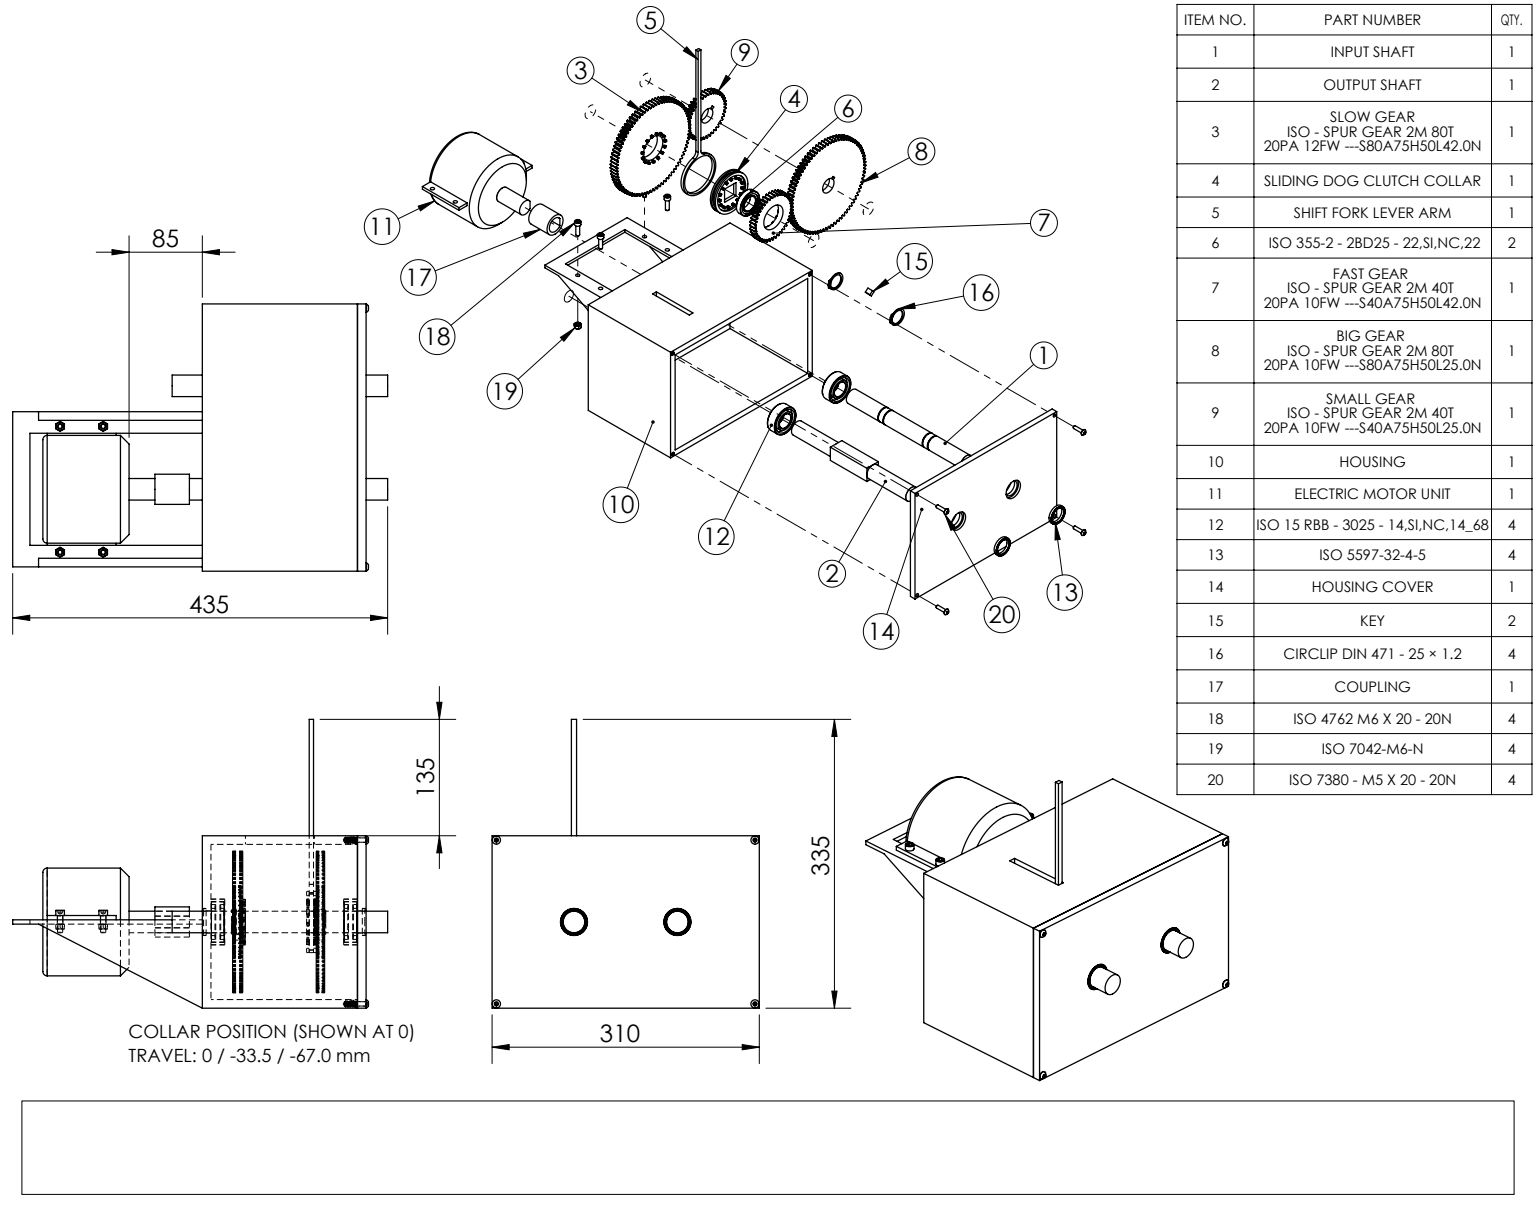
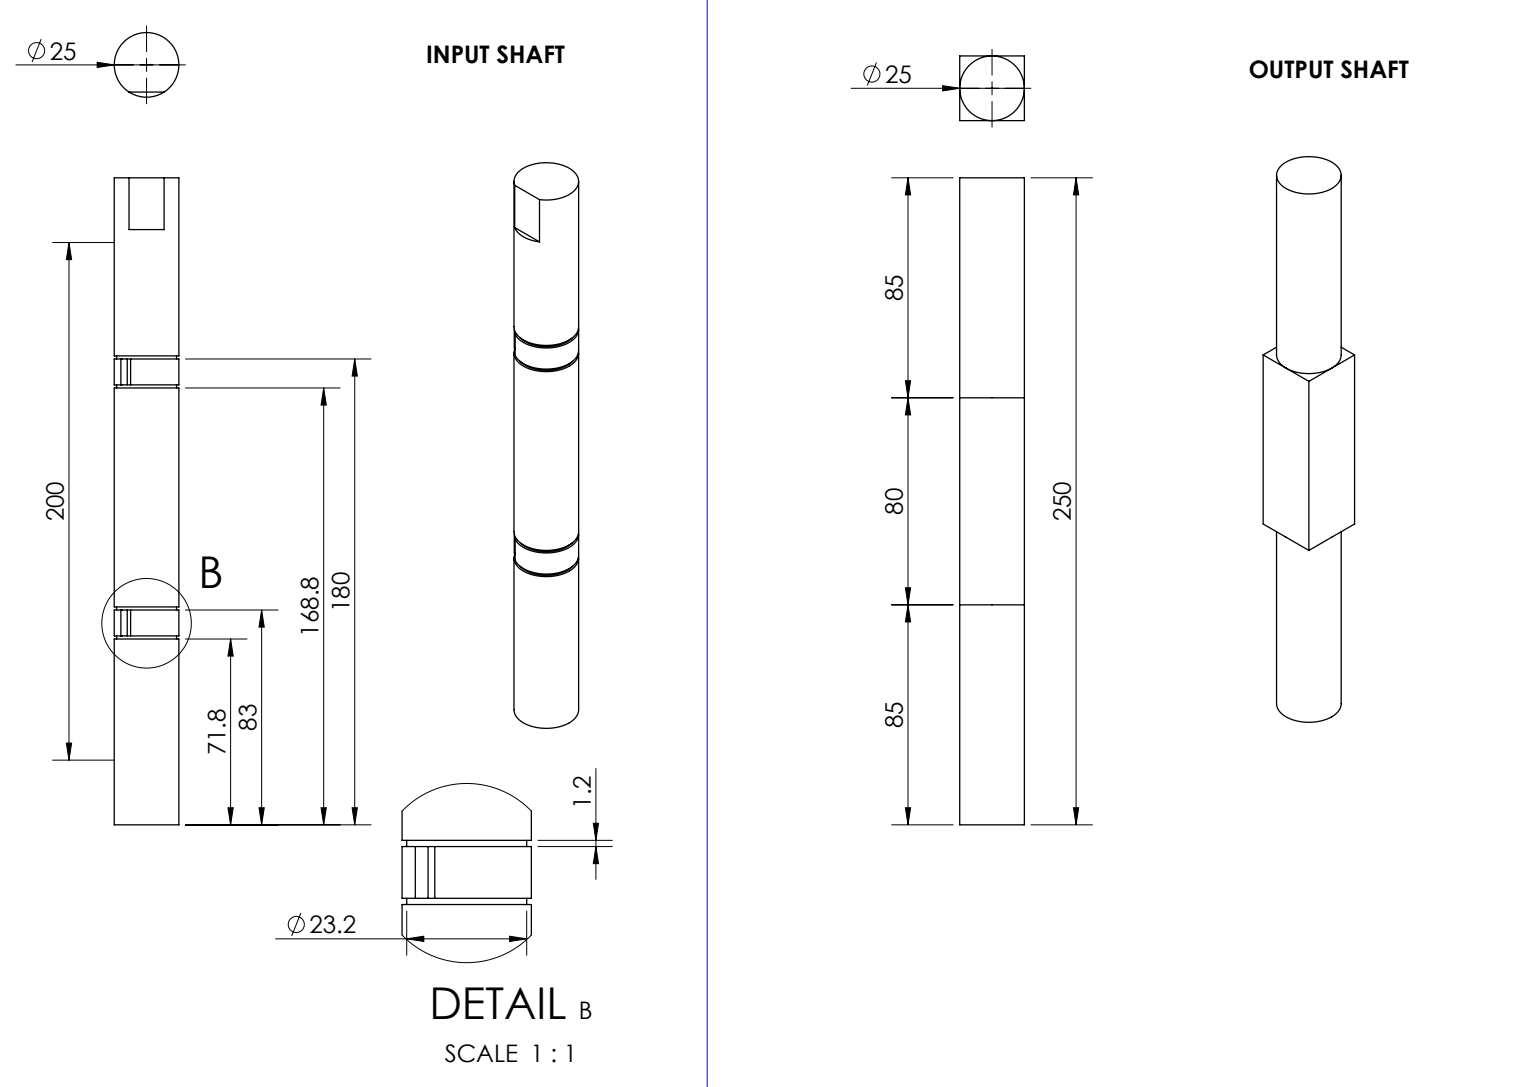
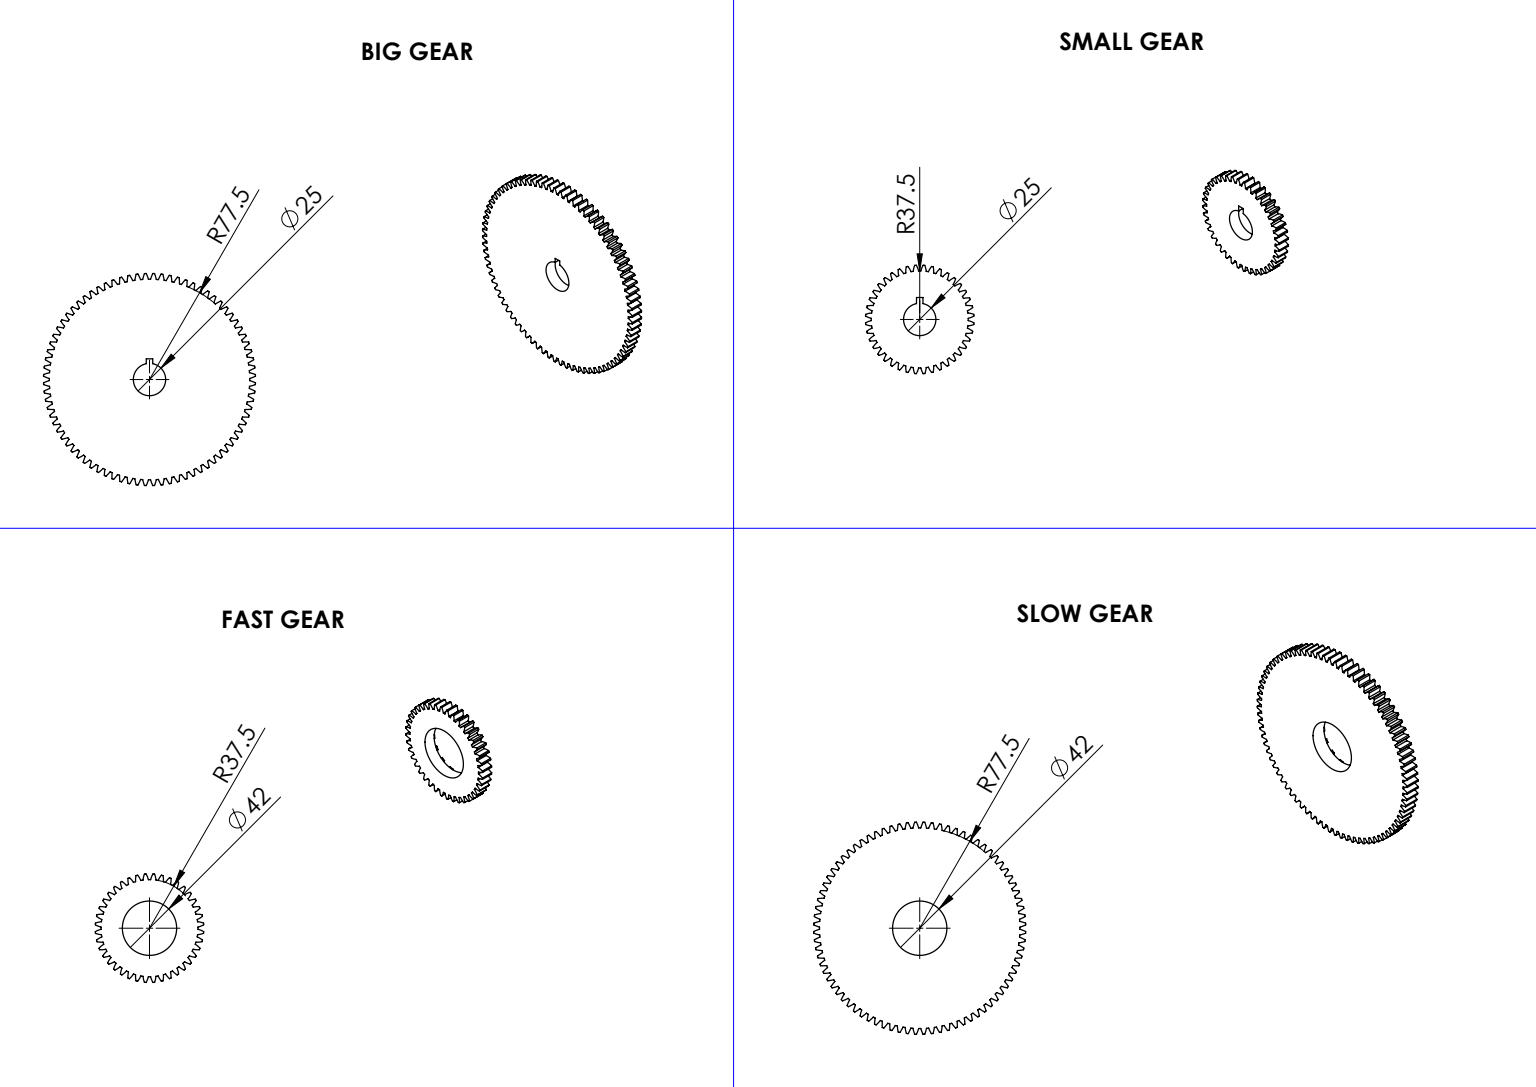
ISO-10303-21;
HEADER;
FILE_DESCRIPTION (('STEP AP214'),
    '1' );
FILE_NAME ('BR-542',
    '2026-10-08T09:53:37',
    ( '' ),
    ( '' ),
    'SwSTEP 2.0',
    'SolidWorks 2026',
    '' );
FILE_SCHEMA (( 'AUTOMOTIVE_DESIGN' ));
ENDSEC;

DATA;
#1 = ORIENTED_EDGE ( 'NONE', *, *, #51679, .F. ) ;
#2 = CARTESIAN_POINT ( 'NONE',  ( -96.15314808468745866, -211.9973110713294489, 75.77864583420047495 ) ) ;
#3 = EDGE_LOOP ( 'NONE', ( #16003, #47116, #6301, #7133 ) ) ;
#4 = DIRECTION ( 'NONE',  ( -1.000000000000000000, -0.000000000000000000, -0.000000000000000000 ) ) ;
#5 = CARTESIAN_POINT ( 'NONE',  ( 10.00000000000000000, 21.53537804866126137, -30.80686688396986028 ) ) ;
#6 = DIRECTION ( 'NONE',  ( -0.000000000000000000, -0.000000000000000000, 1.000000000000000000 ) ) ;
#7 = DIRECTION ( 'NONE',  ( 0.000000000000000000, 0.7071067811865487940, -0.7071067811865462405 ) ) ;
#8 = DIRECTION ( 'NONE',  ( -1.000000000000000000, 0.000000000000000000, 0.000000000000000000 ) ) ;
#9 = CARTESIAN_POINT ( 'NONE',  ( -92.34999999999999432, -209.9999999999999716, 90.00000000000000000 ) ) ;
#10 = CARTESIAN_POINT ( 'NONE',  ( 96.15314808468748708, 91.99731107132950569, 84.98614583420047097 ) ) ;
#11 = CYLINDRICAL_SURFACE ( 'NONE', #11189, 82.00000000000000000 ) ;
#12 = CARTESIAN_POINT ( 'NONE',  ( 20.85212586905262100, -130.9402397935870965, 2.500000000000000000 ) ) ;
#13 = DIRECTION ( 'NONE',  ( 0.000000000000000000, 0.8660254037844421493, 0.4999999999999938938 ) ) ;
#14 = CARTESIAN_POINT ( 'NONE',  ( -5.000000000000000000, 2.488344183252603870, -1.689918788536291405 ) ) ;
#15 = DIRECTION ( 'NONE',  ( 9.814797785686868941E-17, -1.000000000000000000, 0.000000000000000000 ) ) ;
#16 = CARTESIAN_POINT ( 'NONE',  ( 2.255011273957053586, 4.471571325851512846, -0.5083873451168745561 ) ) ;
#17 = DIRECTION ( 'NONE',  ( 0.000000000000000000, 0.8910065241883656784, 0.4539904997395510788 ) ) ;
#18 = CARTESIAN_POINT ( 'NONE',  ( 99.99999999999998579, 90.00000000000000000, -90.00000000000000000 ) ) ;
#19 = AXIS2_PLACEMENT_3D ( 'NONE', #55225, #15366, #9737 ) ;
#20 = CYLINDRICAL_SURFACE ( 'NONE', #64875, 31.99999999999998579 ) ;
#21 = AXIS2_PLACEMENT_3D ( 'NONE', #73803, #50119, #22316 ) ;
#22 = FACE_OUTER_BOUND ( 'NONE', #9056, .T. ) ;
#23 = CARTESIAN_POINT ( 'NONE',  ( -92.69370383062505425, 91.33154071421968467, 89.37822916753378877 ) ) ;
#24 = CARTESIAN_POINT ( 'NONE',  ( 0.000000000000000000, -37.22597642581153821, 10.79786254984320415 ) ) ;
#25 = AXIS2_PLACEMENT_3D ( 'NONE', #2057, #18922, #40477 ) ;
#26 = ADVANCED_FACE ( 'NONE', ( #50299 ), #9718, .T. ) ;
#27 = CARTESIAN_POINT ( 'NONE',  ( -93.07557990970633455, 88.17815826261617929, 75.00000000000001421 ) ) ;
#28 = ORIENTED_EDGE ( 'NONE', *, *, #17747, .T. ) ;
#29 = CARTESIAN_POINT ( 'NONE',  ( -92.35000000000005116, 91.52997821335253548, 77.03541666666666288 ) ) ;
#30 = DIRECTION ( 'NONE',  ( 0.000000000000000000, 0.3090169943749410675, 0.9510565162951556406 ) ) ;
#31 = CARTESIAN_POINT ( 'NONE',  ( 10.00000000000000000, 69.42325613327439271, 34.44570377933623462 ) ) ;
#32 = DIRECTION ( 'NONE',  ( 0.4565542962317865050, 0.000000000000000000, 0.8896955516311735312 ) ) ;
#33 = CIRCLE ( 'NONE', #8406, 42.00000000000000000 ) ;
#34 = DIRECTION ( 'NONE',  ( -8.783410004945701396E-16, -1.065814103640131188E-14, -1.000000000000000000 ) ) ;
#35 = VECTOR ( 'NONE', #29817, 1000.000000000000000 ) ;
#36 = CONICAL_SURFACE ( 'NONE', #30016, 3.000000000000000000, 0.9599310885968762586 ) ;
#37 = CARTESIAN_POINT ( 'NONE',  ( 97.30629616937498838, -208.6684592857803011, 84.45697916753383083 ) ) ;
#38 = ORIENTED_EDGE ( 'NONE', *, *, #69676, .T. ) ;
#39 = EDGE_CURVE ( 'NONE', #49169, #37092, #23562, .T. ) ;
#40 = VECTOR ( 'NONE', #42271, 1000.000000000000000 ) ;
#41 = ORIENTED_EDGE ( 'NONE', *, *, #37857, .F. ) ;
#42 = AXIS2_PLACEMENT_3D ( 'NONE', #21315, #43177, #8581 ) ;
#43 = ADVANCED_FACE ( 'NONE', ( #33760 ), #72489, .F. ) ;
#44 = DIRECTION ( 'NONE',  ( 0.000000000000000000, 0.000000000000000000, -1.000000000000000000 ) ) ;
#45 = VERTEX_POINT ( 'NONE', #4470 ) ;
#46 = DIRECTION ( 'NONE',  ( -1.000000000000000000, 0.000000000000000000, 0.000000000000000000 ) ) ;
#47 = CARTESIAN_POINT ( 'NONE',  ( 96.15314808468750130, -211.9973110713294489, 77.78947916753381264 ) ) ;
#48 = ORIENTED_EDGE ( 'NONE', *, *, #42717, .F. ) ;
#49 = CARTESIAN_POINT ( 'NONE',  ( 95.00000000000000000, -212.6630814284392557, 84.24531250086715772 ) ) ;
#50 = EDGE_CURVE ( 'NONE', #4438, #10838, #58395, .T. ) ;
#51 = EDGE_CURVE ( 'NONE', #68933, #53084, #10085, .T. ) ;
#52 = ORIENTED_EDGE ( 'NONE', *, *, #54649, .T. ) ;
#53 = CARTESIAN_POINT ( 'NONE',  ( -92.35000000000005116, -211.5299782133524786, 88.35958333333334735 ) ) ;
#54 = ORIENTED_EDGE ( 'NONE', *, *, #5365, .T. ) ;
#55 = ORIENTED_EDGE ( 'NONE', *, *, #2305, .T. ) ;
#56 = CARTESIAN_POINT ( 'NONE',  ( -97.30629616937501680, 88.66845928578038638, 75.24947916753383481 ) ) ;
#57 = DIRECTION ( 'NONE',  ( -0.9966891607226785466, -0.08130631524009969413, 0.000000000000000000 ) ) ;
#58 = ORIENTED_EDGE ( 'NONE', *, *, #67325, .F. ) ;
#59 = DIRECTION ( 'NONE',  ( -0.3311129884571295534, -0.9435911131814398445, 0.000000000000000000 ) ) ;
#60 = CARTESIAN_POINT ( 'NONE',  ( 97.64999999999997726, -211.5299782133524502, 87.16895833506762870 ) ) ;
#61 = EDGE_LOOP ( 'NONE', ( #56429, #49717, #59358, #37465 ) ) ;
#62 = DIRECTION ( 'NONE',  ( -1.000000000000000000, 0.000000000000000000, 0.000000000000000000 ) ) ;
#63 = EDGE_LOOP ( 'NONE', ( #58419, #58729, #9713, #39288 ) ) ;
#64 = CARTESIAN_POINT ( 'NONE',  ( -26.29030328629083968, -123.6496510949466341, -5.500000000000000000 ) ) ;
#65 = CIRCLE ( 'NONE', #33475, 42.00000000000000000 ) ;
#66 = EDGE_CURVE ( 'NONE', #32419, #45509, #49931, .T. ) ;
#67 = EDGE_LOOP ( 'NONE', ( #2457, #71707, #71945, #64726 ) ) ;
#68 = CIRCLE ( 'NONE', #60030, 16.00000000000000000 ) ;
#69 = ORIENTED_EDGE ( 'NONE', *, *, #12987, .T. ) ;
#70 = VERTEX_POINT ( 'NONE', #39037 ) ;
#71 = FACE_OUTER_BOUND ( 'NONE', #8361, .T. ) ;
#72 = ITEM_DEFINED_TRANSFORMATION ( 'NONE', 'NONE', #20767,  #43395 ) ;
#73 = CARTESIAN_POINT ( 'NONE',  ( -5.000000000000000000, -2.886751345948134428, -2.080000000000000071 ) ) ;
#74 = ORIENTED_EDGE ( 'NONE', *, *, #31039, .F. ) ;
#75 = VERTEX_POINT ( 'NONE', #9336 ) ;
#76 = AXIS2_PLACEMENT_3D ( 'NONE', #48493, #31191, #42490 ) ;
#77 = ORIENTED_EDGE ( 'NONE', *, *, #22870, .F. ) ;
#78 = CARTESIAN_POINT ( 'NONE',  ( 95.00000000000000000, -213.0599564267049857, 76.18874999999999886 ) ) ;
#79 = CARTESIAN_POINT ( 'NONE',  ( -97.64999999960622290, -209.9999706925929672, 76.74344264316562203 ) ) ;
#80 = CARTESIAN_POINT ( 'NONE',  ( -97.65000000000001990, 90.00000000000004263, 86.82500000000000284 ) ) ;
#81 = EDGE_CURVE ( 'NONE', #13281, #10925, #26630, .T. ) ;
#82 = ORIENTED_EDGE ( 'NONE', *, *, #60544, .T. ) ;
#83 = DIRECTION ( 'NONE',  ( -1.000000000000000000, 0.000000000000000000, 0.000000000000000000 ) ) ;
#84 = ORIENTED_EDGE ( 'NONE', *, *, #17370, .T. ) ;
#85 = LINE ( 'NONE', #57553, #61145 ) ;
#86 = CARTESIAN_POINT ( 'NONE',  ( -92.69370383062498320, -209.9999999999999716, 84.88031250086713442 ) ) ;
#87 = ORIENTED_EDGE ( 'NONE', *, *, #45061, .F. ) ;
#88 = EDGE_CURVE ( 'NONE', #20645, #66879, #14982, .T. ) ;
#89 = CARTESIAN_POINT ( 'NONE',  ( -3.000000000000000000, 0.000000000000000000, 0.000000000000000000 ) ) ;
#90 = CARTESIAN_POINT ( 'NONE',  ( 93.89144186338218390, -212.3693961632864955, 74.97612907457772735 ) ) ;
#91 = CARTESIAN_POINT ( 'NONE',  ( -2.499999999999970690, 73.00000000000001421, -201.6999999999999602 ) ) ;
#92 = CARTESIAN_POINT ( 'NONE',  ( -97.30629616937497417, -208.6684592857803295, 76.25489583420049655 ) ) ;
#93 = AXIS2_PLACEMENT_3D ( 'NONE', #19631, #69384, #17880 ) ;
#94 = CARTESIAN_POINT ( 'NONE',  ( 11.99999999999999822, 66.50666863322000211, 39.78640506895628448 ) ) ;
#95 = CARTESIAN_POINT ( 'NONE',  ( 94.99999999999998579, 90.00000000000002842, 90.00000000000000000 ) ) ;
#96 = VECTOR ( 'NONE', #69294, 1000.000000000000000 ) ;
#97 = VECTOR ( 'NONE', #25254, 1000.000000000000114 ) ;
#98 = TOROIDAL_SURFACE ( 'NONE', #51668, 20.69999999999999929, 0.2999999999999981570 ) ;
#99 = CARTESIAN_POINT ( 'NONE',  ( 0.000000000000000000, -0.9646360437375307573, 23.52805723605590060 ) ) ;
#100 = DIRECTION ( 'NONE',  ( 0.000000000000000000, 0.000000000000000000, 1.000000000000000000 ) ) ;
#101 = CARTESIAN_POINT ( 'NONE',  ( -96.15314808468752972, 91.99731107132950569, 78.74197916753381321 ) ) ;
#102 = CARTESIAN_POINT ( 'NONE',  ( 26.00000000000000355, 0.000000000000000000, 0.000000000000000000 ) ) ;
#103 = DIRECTION ( 'NONE',  ( 1.000000000000000000, 0.000000000000000000, 0.000000000000000000 ) ) ;
#104 =( BOUNDED_CURVE ( )  B_SPLINE_CURVE ( 2, ( #36888, #19593, #59840, #8323, #31250, #71460, #19961 ),
 .UNSPECIFIED., .F., .F. ) 
 B_SPLINE_CURVE_WITH_KNOTS ( ( 3, 2, 2, 3 ),
 ( 0.2291666666666663521, 0.2361111111111107719, 0.2430555555555551639, 0.2499999999999995837 ),
 .UNSPECIFIED. ) 
 CURVE ( )  GEOMETRIC_REPRESENTATION_ITEM ( )  RATIONAL_B_SPLINE_CURVE ( ( 1.000000000000005995, 0.8660254037844328234, 1.000000000000000000, 0.8660254037844387076, 1.000000000000000000, 0.8660254037844467012, 0.9999999999999920064 ) ) 
 REPRESENTATION_ITEM ( '' )  );
#105 = VERTEX_POINT ( 'NONE', #27751 ) ;
#106 = DIRECTION ( 'NONE',  ( -1.000000000000000000, 0.000000000000000000, -0.000000000000000000 ) ) ;
#107 = DIRECTION ( 'NONE',  ( 9.814797785686868941E-17, 1.000000000000000000, -0.000000000000000000 ) ) ;
#108 = CARTESIAN_POINT ( 'NONE',  ( 97.64999999999999147, 90.00000015433757028, 79.60187500750917877 ) ) ;
#109 = PLANE ( 'NONE',  #37048 ) ;
#110 = DIRECTION ( 'NONE',  ( 1.000000000000000000, -0.000000000000000000, -0.000000000000000000 ) ) ;
#111 = DIRECTION ( 'NONE',  ( 1.000000000000000000, 0.000000000000000000, 0.000000000000000000 ) ) ;
#112 = CARTESIAN_POINT ( 'NONE',  ( -93.84685191531248449, -208.0026889286704943, 80.06489583420048461 ) ) ;
#113 = LINE ( 'NONE', #11332, #2116 ) ;
#114 = ORIENTED_EDGE ( 'NONE', *, *, #19664, .T. ) ;
#115 = DIRECTION ( 'NONE',  ( 0.000000000000000000, 0.000000000000000000, 1.000000000000000000 ) ) ;
#116 = DIRECTION ( 'NONE',  ( 1.000000000000000000, -0.000000000000000000, -0.000000000000000000 ) ) ;
#117 = DIRECTION ( 'NONE',  ( 1.000000000000000000, -0.000000000000000000, 0.000000000000000000 ) ) ;
#118 = LINE ( 'NONE', #6814, #70143 ) ;
#119 = CIRCLE ( 'NONE', #8452, 82.00000000000000000 ) ;
#120 = CIRCLE ( 'NONE', #42098, 12.49999999999999645 ) ;
#121 = AXIS2_PLACEMENT_3D ( 'NONE', #14908, #31452, #37108 ) ;
#122 = ADVANCED_FACE ( 'NONE', ( #44690 ), #3363, .T. ) ;
#123 = DIRECTION ( 'NONE',  ( 0.000000000000000000, 0.000000000000000000, -1.000000000000000000 ) ) ;
#124 = EDGE_LOOP ( 'NONE', ( #72657, #17646, #60225, #7667 ) ) ;
#126 = EDGE_CURVE ( 'NONE', #13140, #57222, #72120, .T. ) ;
#125 = CARTESIAN_POINT ( 'NONE',  ( 5.000000000000000000, 27.74655509720779634, -77.16300072079631889 ) ) ;
#127 = CARTESIAN_POINT ( 'NONE',  ( -10.00000000000000000, 0.000000000000000000, 0.000000000000000000 ) ) ;
#128 = EDGE_LOOP ( 'NONE', ( #64642, #36236, #46742, #60430 ) ) ;
#129 = CARTESIAN_POINT ( 'NONE',  ( 92.69370383062501162, -208.6684592857803295, 89.58989583420047609 ) ) ;
#130 = DIRECTION ( 'NONE',  ( 0.000000000000000000, -0.7071067811865389130, -0.7071067811865563435 ) ) ;
#131 = EDGE_LOOP ( 'NONE', ( #13994, #39252, #24769, #61767 ) ) ;
#132 = CARTESIAN_POINT ( 'NONE',  ( 11.99999999999999822, 41.76106447765580043, -62.50884508063379741 ) ) ;
#133 = AXIS2_PLACEMENT_3D ( 'NONE', #60527, #9005, #21768 ) ;
#134 = EDGE_CURVE ( 'NONE', #23470, #67171, #321, .T. ) ;
#135 = ORIENTED_EDGE ( 'NONE', *, *, #35787, .T. ) ;
#136 = DIRECTION ( 'NONE',  ( -0.000000000000000000, -0.000000000000000000, -1.000000000000000000 ) ) ;
#137 = ORIENTED_EDGE ( 'NONE', *, *, #39556, .T. ) ;
#138 = AXIS2_PLACEMENT_3D ( 'NONE', #23331, #68076, #16566 ) ;
#139 = LINE ( 'NONE', #40307, #28824 ) ;
#140 = AXIS2_PLACEMENT_3D ( 'NONE', #41358, #52630, #1547 ) ;
#141 = ORIENTED_EDGE ( 'NONE', *, *, #29114, .F. ) ;
#142 = CARTESIAN_POINT ( 'NONE',  ( 10.00000000000000000, 22.74946021919175720, -29.81001611430984255 ) ) ;
#143 = VERTEX_POINT ( 'NONE', #61975 ) ;
#144 = AXIS2_PLACEMENT_3D ( 'NONE', #36569, #42969, #48233 ) ;
#145 = ORIENTED_EDGE ( 'NONE', *, *, #39730, .F. ) ;
#146 = CYLINDRICAL_SURFACE ( 'NONE', #33227, 26.50000000000000355 ) ;
#147 = ORIENTED_EDGE ( 'NONE', *, *, #29982, .T. ) ;
#148 = ADVANCED_FACE ( 'NONE', ( #73604 ), #38668, .T. ) ;
#149 = ORIENTED_EDGE ( 'NONE', *, *, #29009, .F. ) ;
#150 = CYLINDRICAL_SURFACE ( 'NONE', #8414, 77.49899999999999523 ) ;
#151 = ADVANCED_FACE ( 'NONE', ( #45053 ), #32637, .T. ) ;
#152 = CARTESIAN_POINT ( 'NONE',  ( -18.24502636017238899, -100.7225776329765665, 5.500000000000000000 ) ) ;
#153 = EDGE_CURVE ( 'NONE', #68796, #47180, #52421, .T. ) ;
#154 = ORIENTED_EDGE ( 'NONE', *, *, #63199, .F. ) ;
#155 = ORIENTED_EDGE ( 'NONE', *, *, #25637, .T. ) ;
#156 = CARTESIAN_POINT ( 'NONE',  ( 97.30629616937498838, 91.33154071421968467, 85.56822916753380071 ) ) ;
#158 = ORIENTED_EDGE ( 'NONE', *, *, #43110, .F. ) ;
#157 = EDGE_CURVE ( 'NONE', #60576, #23470, #28588, .T. ) ;
#159 = CARTESIAN_POINT ( 'NONE',  ( 96.15314808468750130, -211.9973110713294489, 82.23447916753380582 ) ) ;
#160 = APPLICATION_PROTOCOL_DEFINITION ( 'draft international standard', 'automotive_design', 1998, #26332 ) ;
#161 = DIRECTION ( 'NONE',  ( 0.000000000000000000, 0.000000000000000000, 1.000000000000000000 ) ) ;
#162 = CARTESIAN_POINT ( 'NONE',  ( 12.00000000000000355, 0.000000000000000000, 21.00000000000000000 ) ) ;
#163 = CARTESIAN_POINT ( 'NONE',  ( -2.500000000000015543, -73.00000000000001421, -255.0000000000000000 ) ) ;
#164 = CARTESIAN_POINT ( 'NONE',  ( -94.99999999999997158, -206.9400435732949575, 89.20624999999999716 ) ) ;
#165 = CARTESIAN_POINT ( 'NONE',  ( -97.65000000000001990, 90.00000000000004263, 79.20499999999999829 ) ) ;
#166 = CARTESIAN_POINT ( 'NONE',  ( 97.65000000000000568, 88.47002178664752137, 85.26395833506762756 ) ) ;
#167 = CARTESIAN_POINT ( 'NONE',  ( -93.84685191531248449, -208.0026889286704943, 84.98614583420047097 ) ) ;
#168 = CARTESIAN_POINT ( 'NONE',  ( -92.69370383062502583, 91.33154071421968467, 85.72697916753381264 ) ) ;
#169 = EDGE_CURVE ( 'NONE', #3345, #5520, #11254, .T. ) ;
#170 = ORIENTED_EDGE ( 'NONE', *, *, #48054, .T. ) ;
#172 = CARTESIAN_POINT ( 'NONE',  ( -95.00000000000002842, 92.66308142843932671, 85.03906250086714635 ) ) ;
#171 = CARTESIAN_POINT ( 'NONE',  ( 96.15314808468748708, 91.99731107132950569, 84.98614583420047097 ) ) ;
#173 = ORIENTED_EDGE ( 'NONE', *, *, #55746, .F. ) ;
#174 = CARTESIAN_POINT ( 'NONE',  ( -7.543218489614351263, -11.91259227951415056, -1.199999999999999956 ) ) ;
#175 = CARTESIAN_POINT ( 'NONE',  ( 96.32499999999998863, -212.2949673200287179, 76.32104166840096582 ) ) ;
#176 = CARTESIAN_POINT ( 'NONE',  ( 12.00000000000000000, -3.948201729842355068, -23.21447184625292692 ) ) ;
#177 = CYLINDRICAL_SURFACE ( 'NONE', #69251, 20.20000000000036522 ) ;
#178 = CARTESIAN_POINT ( 'NONE',  ( -96.15314808468745866, -211.9973110713294489, 86.57364583420047666 ) ) ;
#179 = FACE_OUTER_BOUND ( 'NONE', #56512, .T. ) ;
#180 = AXIS2_PLACEMENT_3D ( 'NONE', #34076, #10405, #33316 ) ;
#181 = AXIS2_PLACEMENT_3D ( 'NONE', #994, #13333, #11843 ) ;
#182 = CARTESIAN_POINT ( 'NONE',  ( 0.000000000000000000, 0.000000000000000000, 0.000000000000000000 ) ) ;
#183 = CARTESIAN_POINT ( 'NONE',  ( 0.000000000000000000, 0.000000000000000000, 0.000000000000000000 ) ) ;
#184 = CARTESIAN_POINT ( 'NONE',  ( 5.000000000000000000, -38.55633173626998911, -16.65560815589452304 ) ) ;
#185 = VERTEX_POINT ( 'NONE', #57079 ) ;
#186 = EDGE_LOOP ( 'NONE', ( #8690, #64007, #52251, #61322 ) ) ;
#187 = CARTESIAN_POINT ( 'NONE',  ( -97.65000000000001990, 90.00000000000004263, 77.29999999999999716 ) ) ;
#188 = LINE ( 'NONE', #23080, #53533 ) ;
#189 = DIRECTION ( 'NONE',  ( -1.000000000000000000, -0.000000000000000000, 0.000000000000000000 ) ) ;
#190 = LINE ( 'NONE', #46749, #7538 ) ;
#191 = CARTESIAN_POINT ( 'NONE',  ( -92.35000000000000853, -208.4700217866474929, 89.73541666666663730 ) ) ;
#192 = CARTESIAN_POINT ( 'NONE',  ( 11.99999999999999822, -69.42325613327415113, -34.44570377933671779 ) ) ;
#193 = ORIENTED_EDGE ( 'NONE', *, *, #19096, .F. ) ;
#194 = CARTESIAN_POINT ( 'NONE',  ( -97.30629616937501680, 88.66845928578038638, 76.99572916753380980 ) ) ;
#195 = DIRECTION ( 'NONE',  ( -0.000000000000000000, -0.000000000000000000, 1.000000000000000000 ) ) ;
#196 = VECTOR ( 'NONE', #2843, 1000.000000000000000 ) ;
#197 = DIRECTION ( 'NONE',  ( 0.000000000000000000, -6.938893903907228378E-15, 1.000000000000000000 ) ) ;
#198 = AXIS2_PLACEMENT_3D ( 'NONE', #15360, #39055, #27767 ) ;
#199 = CARTESIAN_POINT ( 'NONE',  ( 10.00000000000000000, 0.000000000000000000, 0.000000000000000000 ) ) ;
#200 = CARTESIAN_POINT ( 'NONE',  ( 10.00000000000000000, -27.13269053701114331, 25.88420570971391754 ) ) ;
#201 = DIRECTION ( 'NONE',  ( 0.000000000000000000, -0.7071067811865537900, 0.7071067811865413555 ) ) ;
#202 = CARTESIAN_POINT ( 'NONE',  ( 0.000000000000000000, -5.256550761633411284, 77.32052557432838569 ) ) ;
#203 = PRESENTATION_STYLE_ASSIGNMENT (( #57300 ) ) ;
#204 = VECTOR ( 'NONE', #39459, 1000.000000000000000 ) ;
#205 = CARTESIAN_POINT ( 'NONE',  ( 97.30629616937498838, 90.00000000000002842, 78.68906250086715204 ) ) ;
#206 = ADVANCED_FACE ( 'NONE', ( #58175 ), #28481, .T. ) ;
#207 = CARTESIAN_POINT ( 'NONE',  ( -97.30629616937497417, -211.3315407142195852, 79.05947916753382287 ) ) ;
#208 = CARTESIAN_POINT ( 'NONE',  ( -0.7800914985199643992, -121.2811936832255100, 2.500000000000000000 ) ) ;
#209 = EDGE_LOOP ( 'NONE', ( #50770, #39177, #69553, #21845 ) ) ;
#210 = CARTESIAN_POINT ( 'NONE',  ( 11.41210121379328335, -99.40233154247455616, 5.500000000000000000 ) ) ;
#211 = CARTESIAN_POINT ( 'NONE',  ( -93.09170270117411405, -211.8387227684710012, 74.99909419456534465 ) ) ;
#212 = CARTESIAN_POINT ( 'NONE',  ( 11.99999999999999822, -65.64334221924937651, 41.19522573413711797 ) ) ;
#213 = EDGE_CURVE ( 'NONE', #29240, #35405, #33215, .T. ) ;
#214 = EDGE_CURVE ( 'NONE', #50169, #71079, #46057, .T. ) ;
#215 = EDGE_CURVE ( 'NONE', #47891, #8216, #22873, .T. ) ;
#216 = CARTESIAN_POINT ( 'NONE',  ( -92.69370383062505425, 91.33154071421968467, 76.20197916753382117 ) ) ;
#217 = CARTESIAN_POINT ( 'NONE',  ( 97.30629616937498838, -208.6684592857803011, 81.75822916753381264 ) ) ;
#218 = EDGE_LOOP ( 'NONE', ( #22969, #71308, #32265, #23683 ) ) ;
#219 = CARTESIAN_POINT ( 'NONE',  ( -93.67500000000003979, 92.29496732002878900, 75.18333333333332291 ) ) ;
#220 = ORIENTED_EDGE ( 'NONE', *, *, #37863, .T. ) ;
#221 = ADVANCED_FACE ( 'NONE', ( #63104 ), #33867, .F. ) ;
#222 = CYLINDRICAL_SURFACE ( 'NONE', #63992, 2.649999999999999467 ) ;
#223 = ORIENTED_EDGE ( 'NONE', *, *, #32015, .F. ) ;
#224 = ADVANCED_FACE ( 'NONE', ( #20004 ), #64049, .F. ) ;
#225 = AXIS2_PLACEMENT_3D ( 'NONE', #13248, #59124, #26003 ) ;
#226 = DIRECTION ( 'NONE',  ( 0.000000000000000000, 0.9238795325112877377, -0.3826834323650873948 ) ) ;
#227 = AXIS2_PLACEMENT_3D ( 'NONE', #25295, #66623, #48591 ) ;
#228 = ORIENTED_EDGE ( 'NONE', *, *, #5227, .F. ) ;
#229 = ORIENTED_EDGE ( 'NONE', *, *, #36188, .T. ) ;
#230 = EDGE_LOOP ( 'NONE', ( #33493, #51216, #41523, #73402, #35685 ) ) ;
#231 = CARTESIAN_POINT ( 'NONE',  ( 0.000000000000000000, 0.000000000000000000, -6.000000000000000000 ) ) ;
#232 = VERTEX_POINT ( 'NONE', #36200 ) ;
#233 = ORIENTED_EDGE ( 'NONE', *, *, #65058, .T. ) ;
#234 = CARTESIAN_POINT ( 'NONE',  ( 94.99999999999998579, 92.66308142843935514, 83.92781250086716227 ) ) ;
#235 = EDGE_CURVE ( 'NONE', #35660, #27140, #36937, .T. ) ;
#236 = DIRECTION ( 'NONE',  ( 0.000000000000000000, 0.000000000000000000, -1.000000000000000000 ) ) ;
#237 = VERTEX_POINT ( 'NONE', #8375 ) ;
#238 = ORIENTED_EDGE ( 'NONE', *, *, #67114, .T. ) ;
#239 = ORIENTED_EDGE ( 'NONE', *, *, #34376, .F. ) ;
#240 = ORIENTED_EDGE ( 'NONE', *, *, #37205, .F. ) ;
#241 =( NAMED_UNIT ( * ) PLANE_ANGLE_UNIT ( ) SI_UNIT ( $, .RADIAN. ) );
#242 = VECTOR ( 'NONE', #15932, 1000.000000000000000 ) ;
#243 = EDGE_CURVE ( 'NONE', #20441, #46588, #25658, .T. ) ;
#244 = ADVANCED_FACE ( 'NONE', ( #1303 ), #7269, .T. ) ;
#245 = VECTOR ( 'NONE', #9252, 1000.000000000000000 ) ;
#246 = CARTESIAN_POINT ( 'NONE',  ( 0.000000000000000000, 0.000000000000000000, 0.000000000000000000 ) ) ;
#247 = DIRECTION ( 'NONE',  ( -1.000000000000000000, -0.000000000000000000, 0.000000000000000000 ) ) ;
#248 = CARTESIAN_POINT ( 'NONE',  ( -16.06301359042743115, -102.7814171781257357, 2.500000000000000000 ) ) ;
#249 = DIRECTION ( 'NONE',  ( -1.000000000000000000, 0.000000000000000000, -0.000000000000000000 ) ) ;
#250 = VECTOR ( 'NONE', #46862, 1000.000000000000000 ) ;
#251 = FACE_OUTER_BOUND ( 'NONE', #1348, .T. ) ;
#252 = CARTESIAN_POINT ( 'NONE',  ( 0.000000000000000000, 5.835314593368772229, -22.81335362449846826 ) ) ;
#253 = DIRECTION ( 'NONE',  ( 0.000000000000000000, -6.938893903907231533E-15, 1.000000000000000000 ) ) ;
#254 = ORIENTED_EDGE ( 'NONE', *, *, #39026, .T. ) ;
#255 = CARTESIAN_POINT ( 'NONE',  ( -96.32499999999996021, -212.2949673200287179, 82.56520833506762358 ) ) ;
#256 = ORIENTED_EDGE ( 'NONE', *, *, #21571, .T. ) ;
#257 = DIRECTION ( 'NONE',  ( 0.000000000000000000, 0.000000000000000000, 1.000000000000000000 ) ) ;
#258 = ADVANCED_FACE ( 'NONE', ( #18534 ), #30184, .T. ) ;
#259 = ORIENTED_EDGE ( 'NONE', *, *, #14783, .T. ) ;
#261 = CARTESIAN_POINT ( 'NONE',  ( -97.65000000000001990, 90.00000000000004263, 81.18937500173430521 ) ) ;
#260 = CARTESIAN_POINT ( 'NONE',  ( 93.67499999999998295, 92.29496732002878900, 80.44854166840097776 ) ) ;
#262 = ORIENTED_EDGE ( 'NONE', *, *, #9019, .T. ) ;
#263 = CARTESIAN_POINT ( 'NONE',  ( 92.69370383062498320, 90.00000000000002842, 81.54656250086715374 ) ) ;
#264 = PLANE ( 'NONE',  #181 ) ;
#265 = PLANE ( 'NONE',  #60728 ) ;
#266 = CARTESIAN_POINT ( 'NONE',  ( -8.826826895187510402, -94.96827758698185562, 5.500000000000000000 ) ) ;
#267 = CARTESIAN_POINT ( 'NONE',  ( 11.99999999999999822, -2.946379043146863719, 75.11764819372146462 ) ) ;
#268 = ORIENTED_EDGE ( 'NONE', *, *, #56458, .T. ) ;
#269 = CARTESIAN_POINT ( 'NONE',  ( -97.65000000000001990, 90.00000000000004263, 80.47499999999999432 ) ) ;
#270 = DIRECTION ( 'NONE',  ( 0.000000000000000000, 1.000000000000000000, -0.000000000000000000 ) ) ;
#271 = DIRECTION ( 'NONE',  ( -1.000000000000000000, -0.000000000000000000, 0.000000000000000000 ) ) ;
#272 = ORIENTED_EDGE ( 'NONE', *, *, #49233, .T. ) ;
#273 = ORIENTED_EDGE ( 'NONE', *, *, #31155, .T. ) ;
#274 = FACE_OUTER_BOUND ( 'NONE', #69340, .T. ) ;
#275 = CARTESIAN_POINT ( 'NONE',  ( -3.000000000000000000, 0.000000000000000000, 0.000000000000000000 ) ) ;
#276 = FACE_OUTER_BOUND ( 'NONE', #73498, .T. ) ;
#277 = CARTESIAN_POINT ( 'NONE',  ( -92.69370383062498320, -208.6684592857803011, 80.01197916753380923 ) ) ;
#278 = VERTEX_POINT ( 'NONE', #26397 ) ;
#279 = MECHANICAL_DESIGN_GEOMETRIC_PRESENTATION_REPRESENTATION (  '', ( #31450 ), #13423 ) ;
#280 = CYLINDRICAL_SURFACE ( 'NONE', #16286, 42.00000000000000000 ) ;
#281 = CARTESIAN_POINT ( 'NONE',  ( 0.000000000000000000, -22.67460108101774807, -6.353146135318215038 ) ) ;
#282 = VECTOR ( 'NONE', #8652, 999.9999999999998863 ) ;
#283 = CARTESIAN_POINT ( 'NONE',  ( 11.99999999999999822, -76.66974797899830207, -11.30684508768420571 ) ) ;
#284 = CARTESIAN_POINT ( 'NONE',  ( 93.84685191531248449, 91.99731107132950569, 74.93197916753379673 ) ) ;
#285 = FACE_OUTER_BOUND ( 'NONE', #21532, .T. ) ;
#286 = DIRECTION ( 'NONE',  ( -1.000000000000000000, 0.000000000000000000, 0.000000000000000000 ) ) ;
#287 = CARTESIAN_POINT ( 'NONE',  ( -3.759344165985237129, 2.343521743652961183E-15, 19.05560546998412974 ) ) ;
#288 = DIRECTION ( 'NONE',  ( -0.000000000000000000, -0.000000000000000000, 1.000000000000000000 ) ) ;
#289 = DIRECTION ( 'NONE',  ( -1.000000000000000000, 0.000000000000000000, 0.000000000000000000 ) ) ;
#290 = CARTESIAN_POINT ( 'NONE',  ( 11.99999999999999822, 10.30890764327501863, -81.34940948281324324 ) ) ;
#291 = AXIS2_PLACEMENT_3D ( 'NONE', #10658, #61809, #43781 ) ;
#292 = CIRCLE ( 'NONE', #31463, 31.99999999999998934 ) ;
#293 = CARTESIAN_POINT ( 'NONE',  ( 97.30629616937498838, 88.66845928578035796, 88.79614583420048746 ) ) ;
#294 = LINE ( 'NONE', #17534, #41829 ) ;
#295 = CARTESIAN_POINT ( 'NONE',  ( 94.99999999999998579, 86.94004357329502852, 82.53874999999999318 ) ) ;
#296 = ORIENTED_EDGE ( 'NONE', *, *, #49460, .F. ) ;
#297 = CARTESIAN_POINT ( 'NONE',  ( -10.00000000000000000, 0.000000000000000000, 0.000000000000000000 ) ) ;
#298 = CARTESIAN_POINT ( 'NONE',  ( -95.00000000000002842, 92.66308142843932671, 81.22906250086714408 ) ) ;
#299 = VECTOR ( 'NONE', #69573, 1000.000000000000000 ) ;
#300 = VECTOR ( 'NONE', #69732, 1000.000000000000000 ) ;
#301 = EDGE_CURVE ( 'NONE', #16264, #8951, #60626, .T. ) ;
#302 = ADVANCED_FACE ( 'NONE', ( #26021 ), #48946, .F. ) ;
#303 = EDGE_CURVE ( 'NONE', #64095, #48732, #3130, .T. ) ;
#304 = DIRECTION ( 'NONE',  ( 0.000000000000000000, -0.8090169943749531134, 0.5877852522924654766 ) ) ;
#305 = VERTEX_POINT ( 'NONE', #60978 ) ;
#306 =( BOUNDED_CURVE ( )  B_SPLINE_CURVE ( 2, ( #42487, #60161, #54139, #60884, #2672, #20658, #32290, #43244, #36830 ),
 .UNSPECIFIED., .F., .F. ) 
 B_SPLINE_CURVE_WITH_KNOTS ( ( 3, 2, 2, 2, 3 ),
 ( 0.3810111478265176821, 0.3810113392076479033, 0.3880671047485306224, 0.3951228702894133971, 0.4021785743327781493 ),
 .UNSPECIFIED. ) 
 CURVE ( )  GEOMETRIC_REPRESENTATION_ITEM ( )  RATIONAL_B_SPLINE_CURVE ( ( 0.9999927323225166198, 0.9999963660626911555, 1.000000000000000000, 0.8660254037844387076, 1.000000000000000000, 0.8660254037844387076, 1.000000000000000000, 0.8660265714968713446, 0.9999976645954902210 ) ) 
 REPRESENTATION_ITEM ( '' )  );
#307 = CARTESIAN_POINT ( 'NONE',  ( 92.34999999999999432, 90.00000000000002842, 90.00000000000000000 ) ) ;
#308 = FACE_OUTER_BOUND ( 'NONE', #16262, .T. ) ;
#309 = CARTESIAN_POINT ( 'NONE',  ( -100.0000000000260485, 95.00000000000001421, -75.00000000000000000 ) ) ;
#310 = CARTESIAN_POINT ( 'NONE',  ( 10.00000000000000000, -46.21855187248583974, -62.20884554314070414 ) ) ;
#311 = DIRECTION ( 'NONE',  ( -1.000000000000000000, 0.000000000000000000, 0.000000000000000000 ) ) ;
#312 = DIRECTION ( 'NONE',  ( 1.000000000000000000, 0.000000000000000000, -0.000000000000000000 ) ) ;
#313 = ORIENTED_EDGE ( 'NONE', *, *, #65007, .T. ) ;
#314 = ORIENTED_EDGE ( 'NONE', *, *, #27692, .F. ) ;
#315 = EDGE_CURVE ( 'NONE', #4428, #26458, #9223, .T. ) ;
#316 = CARTESIAN_POINT ( 'NONE',  ( 97.30629616937498838, -208.6684592857803295, 81.28197916753381946 ) ) ;
#317 = ADVANCED_FACE ( 'NONE', ( #65897 ), #60865, .T. ) ;
#318 = CYLINDRICAL_SURFACE ( 'NONE', #22478, 37.49900000000000233 ) ;
#319 = DIRECTION ( 'NONE',  ( -1.000000000000000000, 0.000000000000000000, 0.000000000000000000 ) ) ;
#320 = CARTESIAN_POINT ( 'NONE',  ( 5.000000000000000000, 2.691270400161075216, -1.881368198414912429 ) ) ;
#321 =( BOUNDED_CURVE ( )  B_SPLINE_CURVE ( 2, ( #16099, #50676, #20629, #43944, #66860, #72847, #67236, #38290, #61237 ),
 .UNSPECIFIED., .F., .F. ) 
 B_SPLINE_CURVE_WITH_KNOTS ( ( 3, 2, 2, 2, 3 ),
 ( 0.3386766260338263668, 0.3386767459623536980, 0.3457325115032360840, 0.3527882770441184701, 0.3598440426530882807 ),
 .UNSPECIFIED. ) 
 CURVE ( )  GEOMETRIC_REPRESENTATION_ITEM ( )  RATIONAL_B_SPLINE_CURVE ( ( 0.9999954456811732673, 0.9999977228018805953, 1.000000000000000000, 0.8660254037844387076, 1.000000000000000000, 0.8660254037844387076, 1.000000000000000000, 0.8660254037844387076, 1.000000000000000000 ) ) 
 REPRESENTATION_ITEM ( '' )  );
#322 = CARTESIAN_POINT ( 'NONE',  ( 92.35000000049315361, 89.99996796133687837, 83.73041644179049570 ) ) ;
#323 = CYLINDRICAL_SURFACE ( 'NONE', #57366, 37.49900000000000233 ) ;
#324 = CARTESIAN_POINT ( 'NONE',  ( 97.64999999999999147, -209.9999999999999716, 87.77749999999998920 ) ) ;
#325 = ORIENTED_EDGE ( 'NONE', *, *, #34194, .F. ) ;
#326 = MECHANICAL_DESIGN_GEOMETRIC_PRESENTATION_REPRESENTATION (  '', ( #21897 ), #73467 ) ;
#327 = ORIENTED_EDGE ( 'NONE', *, *, #16062, .T. ) ;
#328 = ORIENTED_EDGE ( 'NONE', *, *, #66153, .T. ) ;
#329 = ORIENTED_EDGE ( 'NONE', *, *, #65370, .T. ) ;
#330 = EDGE_CURVE ( 'NONE', #45876, #49292, #56024, .T. ) ;
#331 = EDGE_CURVE ( 'NONE', #62654, #68271, #27501, .T. ) ;
#332 = VECTOR ( 'NONE', #36378, 1000.000000000000000 ) ;
#333 = CARTESIAN_POINT ( 'NONE',  ( -96.15314808468752972, 91.99731107132950569, 89.06072916753382174 ) ) ;
#334 = DIRECTION ( 'NONE',  ( 0.000000000000000000, 0.000000000000000000, 1.000000000000000000 ) ) ;
#335 = DIRECTION ( 'NONE',  ( 0.000000000000000000, -0.8090169943749403458, -0.5877852522924830181 ) ) ;
#336 = CARTESIAN_POINT ( 'NONE',  ( 92.35000000000000853, -209.9999999999999716, 75.47437500173430180 ) ) ;
#337 = CARTESIAN_POINT ( 'NONE',  ( 92.34999999999999432, 90.00000000000002842, 79.83999999999998920 ) ) ;
#338 = EDGE_LOOP ( 'NONE', ( #19478, #31271, #53427, #16608 ) ) ;
#339 = DIRECTION ( 'NONE',  ( -1.000000000000000000, 7.571537405616606460E-15, 2.598394312951952234E-14 ) ) ;
#340 = CIRCLE ( 'NONE', #62732, 82.00000000000000000 ) ;
#341 = ORIENTED_EDGE ( 'NONE', *, *, #54773, .T. ) ;
#342 = CARTESIAN_POINT ( 'NONE',  ( 10.00000000000000000, 2.946379043147425492, -75.11764819372145041 ) ) ;
#343 = ORIENTED_EDGE ( 'NONE', *, *, #47596, .F. ) ;
#344 = CARTESIAN_POINT ( 'NONE',  ( -97.65000000000001990, 91.52997821335253548, 89.39145833506763950 ) ) ;
#345 = AXIS2_PLACEMENT_3D ( 'NONE', #23518, #51340, #45354 ) ;
#346 = CARTESIAN_POINT ( 'NONE',  ( -97.30629616937501680, 91.33154071421968467, 82.76364583420048859 ) ) ;
#347 = CARTESIAN_POINT ( 'NONE',  ( 94.99999999999998579, 92.66308142843935514, 89.64281250086715147 ) ) ;
#348 = ORIENTED_EDGE ( 'NONE', *, *, #27313, .T. ) ;
#349 = CARTESIAN_POINT ( 'NONE',  ( 10.00000000000000000, -55.19960302592104284, 51.03279382321070301 ) ) ;
#350 = DIRECTION ( 'NONE',  ( -1.000000000000000000, 0.000000000000000000, 0.000000000000000000 ) ) ;
#351 = CARTESIAN_POINT ( 'NONE',  ( 96.32499999999998863, -212.2949673200287179, 85.76666666666665151 ) ) ;
#352 = DIRECTION ( 'NONE',  ( -1.000000000000000000, 0.000000000000000000, -0.000000000000000000 ) ) ;
#353 = ORIENTED_EDGE ( 'NONE', *, *, #72482, .T. ) ;
#354 = CARTESIAN_POINT ( 'NONE',  ( -5.000000000000000000, -0.4878135028931876449, -6.000000000000001776 ) ) ;
#355 = AXIS2_PLACEMENT_3D ( 'NONE', #45789, #68711, #63083 ) ;
#356 = AXIS2_PLACEMENT_3D ( 'NONE', #18436, #58663, #43973 ) ;
#357 = CARTESIAN_POINT ( 'NONE',  ( -92.69370383062498320, -209.9999999999999716, 77.89531250086714920 ) ) ;
#358 = ORIENTED_EDGE ( 'NONE', *, *, #28754, .T. ) ;
#359 = VERTEX_POINT ( 'NONE', #37325 ) ;
#360 = DIRECTION ( 'NONE',  ( -0.000000000000000000, -0.000000000000000000, 1.000000000000000000 ) ) ;
#361 = ORIENTED_EDGE ( 'NONE', *, *, #62756, .T. ) ;
#362 = CARTESIAN_POINT ( 'NONE',  ( 92.34999999999990905, 88.47002178664757821, 77.98791666666667766 ) ) ;
#363 = CARTESIAN_POINT ( 'NONE',  ( -96.32499999999996021, -212.2949673200287179, 78.04083333333333883 ) ) ;
#364 = ORIENTED_EDGE ( 'NONE', *, *, #34297, .F. ) ;
#365 = CARTESIAN_POINT ( 'NONE',  ( -96.15314808468745866, -211.9973110713294489, 75.14364583420046984 ) ) ;
#366 = VERTEX_POINT ( 'NONE', #72607 ) ;
#367 = DIRECTION ( 'NONE',  ( 0.000000000000000000, 0.000000000000000000, 1.000000000000000000 ) ) ;
#368 = CARTESIAN_POINT ( 'NONE',  ( -10.00000000000000000, 0.000000000000000000, 0.000000000000000000 ) ) ;
#369 = DIRECTION ( 'NONE',  ( -1.000000000000000000, 0.000000000000000000, 0.000000000000000000 ) ) ;
#370 = VERTEX_POINT ( 'NONE', #32762 ) ;
#371 = DIRECTION ( 'NONE',  ( 0.000000000000000000, 0.000000000000000000, 1.000000000000000000 ) ) ;
#372 =( NAMED_UNIT ( * ) SI_UNIT ( $, .STERADIAN. ) SOLID_ANGLE_UNIT ( ) );
#373 = CARTESIAN_POINT ( 'NONE',  ( 92.69370383062498320, 91.33154071421968467, 83.23989583420048177 ) ) ;
#374 = CYLINDRICAL_SURFACE ( 'NONE', #42423, 31.99999999999999289 ) ;
#375 = LINE ( 'NONE', #57852, #26573 ) ;
#376 = DIRECTION ( 'NONE',  ( 0.000000000000000000, -0.9238795325112906243, 0.3826834323650805114 ) ) ;
#377 = CARTESIAN_POINT ( 'NONE',  ( -5.000000000000000000, 1.352381405509855972, -0.8629530094790016648 ) ) ;
#378 = LINE ( 'NONE', #63140, #40444 ) ;
#379 = CARTESIAN_POINT ( 'NONE',  ( 3.447886558751866115, 3.782864459065575780, -0.7348938709837807837 ) ) ;
#380 = CARTESIAN_POINT ( 'NONE',  ( 5.000000000000002665, -22.90783923731575911, -78.73519480814978522 ) ) ;
#381 = PRODUCT_RELATED_PRODUCT_CATEGORY ( 'part', '', ( #3780 ) ) ;
#382 = EDGE_CURVE ( 'NONE', #38466, #29678, #65248, .T. ) ;
#383 =( GEOMETRIC_REPRESENTATION_CONTEXT ( 3 ) GLOBAL_UNCERTAINTY_ASSIGNED_CONTEXT ( ( #16132 ) ) GLOBAL_UNIT_ASSIGNED_CONTEXT ( ( #58527, #47619, #18304 ) ) REPRESENTATION_CONTEXT ( 'NONE', 'WORKASPACE' ) );
#384 = CARTESIAN_POINT ( 'NONE',  ( 3.429551818649054340, -146.3199197248623875, 5.500000000000000000 ) ) ;
#385 = CARTESIAN_POINT ( 'NONE',  ( -10.00000000000000000, 0.000000000000000000, 0.000000000000000000 ) ) ;
#386 = LINE ( 'NONE', #68776, #73091 ) ;
#387 = AXIS2_PLACEMENT_3D ( 'NONE', #42617, #2061, #64816 ) ;
#388 = EDGE_CURVE ( 'NONE', #19251, #12587, #32396, .T. ) ;
#389 = EDGE_CURVE ( 'NONE', #21226, #47439, #64170, .T. ) ;
#390 = LINE ( 'NONE', #68413, #20038 ) ;
#391 = CIRCLE ( 'NONE', #51961, 16.00000000000000000 ) ;
#392 = ADVANCED_FACE ( 'NONE', ( #21114 ), #31659, .T. ) ;
#393 = DIRECTION ( 'NONE',  ( 0.000000000000000000, 0.000000000000000000, 1.000000000000000000 ) ) ;
#394 = CARTESIAN_POINT ( 'NONE',  ( 0.000000000000000000, -35.95386929396264009, 10.96151621346475658 ) ) ;
#395 = CARTESIAN_POINT ( 'NONE',  ( 22.63442173698368620, -133.7816164738524378, -2.500000000000000000 ) ) ;
#396 = DIRECTION ( 'NONE',  ( -0.000000000000000000, -0.000000000000000000, 1.000000000000000000 ) ) ;
#397 = DIRECTION ( 'NONE',  ( -0.000000000000000000, -0.000000000000000000, 1.000000000000000000 ) ) ;
#398 = AXIS2_PLACEMENT_3D ( 'NONE', #46012, #71039, #28703 ) ;
#399 = AXIS2_PLACEMENT_3D ( 'NONE', #19459, #47664, #13453 ) ;
#400 = CARTESIAN_POINT ( 'NONE',  ( 95.00000000000000000, -207.3369185715606307, 85.83281250086714920 ) ) ;
#401 = ORIENTED_EDGE ( 'NONE', *, *, #30678, .T. ) ;
#402 = ORIENTED_EDGE ( 'NONE', *, *, #38350, .F. ) ;
#403 = EDGE_CURVE ( 'NONE', #28480, #14622, #20753, .T. ) ;
#404 = EDGE_CURVE ( 'NONE', #15647, #17733, #32964, .T. ) ;
#405 = CARTESIAN_POINT ( 'NONE',  ( -97.64999999999996305, -209.9999999999999716, 86.18999999999999773 ) ) ;
#406 = EDGE_LOOP ( 'NONE', ( #60664, #29067, #49767, #42385 ) ) ;
#407 = DIRECTION ( 'NONE',  ( 0.000000000000000000, 0.6691306063588661202, 0.7431448254773871387 ) ) ;
#408 = CARTESIAN_POINT ( 'NONE',  ( 95.00000000000000000, -212.6630814284392557, 76.46656250086712703 ) ) ;
#409 = ORIENTED_EDGE ( 'NONE', *, *, #48240, .T. ) ;
#410 = CARTESIAN_POINT ( 'NONE',  ( 93.84685191531249870, -208.0026889286704943, 83.98072916753382344 ) ) ;
#411 = EDGE_LOOP ( 'NONE', ( #54319, #60311, #25964, #66217 ) ) ;
#412 = LINE ( 'NONE', #28552, #45572 ) ;
#413 = ORIENTED_EDGE ( 'NONE', *, *, #7216, .F. ) ;
#414 = EDGE_LOOP ( 'NONE', ( #16035, #20964, #13795, #59926 ) ) ;
#415 = CARTESIAN_POINT ( 'NONE',  ( 11.99999999999999822, 66.50666863322000211, 39.78640506895628448 ) ) ;
#416 = CARTESIAN_POINT ( 'NONE',  ( 10.00000000000000000, -10.30890764327324227, -81.34940948281347062 ) ) ;
#417 = ORIENTED_EDGE ( 'NONE', *, *, #65115, .F. ) ;
#418 = DIRECTION ( 'NONE',  ( 1.000000000000000000, 0.000000000000000000, 0.000000000000000000 ) ) ;
#419 = CARTESIAN_POINT ( 'NONE',  ( 97.64999999999997726, -211.5299782133524502, 86.53395833506763779 ) ) ;
#420 = VERTEX_POINT ( 'NONE', #38424 ) ;
#421 = CYLINDRICAL_SURFACE ( 'NONE', #34708, 82.00000000000000000 ) ;
#422 = VECTOR ( 'NONE', #39738, 1000.000000000000000 ) ;
#423 = VERTEX_POINT ( 'NONE', #26756 ) ;
#424 = DIRECTION ( 'NONE',  ( 0.000000000000000000, 0.7071067811865436870, 0.7071067811865513475 ) ) ;
#425 = ORIENTED_EDGE ( 'NONE', *, *, #23338, .F. ) ;
#426 = AXIS2_PLACEMENT_3D ( 'NONE', #33565, #39224, #50861 ) ;
#427 = ORIENTED_EDGE ( 'NONE', *, *, #61045, .F. ) ;
#428 = VERTEX_POINT ( 'NONE', #4227 ) ;
#429 = CARTESIAN_POINT ( 'NONE',  ( -92.35001786638896704, -211.5299885285169523, 78.27895762153575276 ) ) ;
#430 = ITEM_DEFINED_TRANSFORMATION ( 'NONE', 'NONE', #43607,  #43395 ) ;
#431 = CYLINDRICAL_SURFACE ( 'NONE', #39041, 82.00000000000000000 ) ;
#432 = ORIENTED_EDGE ( 'NONE', *, *, #15187, .T. ) ;
#433 = AXIS2_PLACEMENT_3D ( 'NONE', #66115, #14212, #26606 ) ;
#434 = ORIENTED_EDGE ( 'NONE', *, *, #33411, .T. ) ;
#435 = ORIENTED_EDGE ( 'NONE', *, *, #50527, .T. ) ;
#436 = DIRECTION ( 'NONE',  ( 0.000000000000000000, 0.000000000000000000, 1.000000000000000000 ) ) ;
#437 = CARTESIAN_POINT ( 'NONE',  ( 94.99999999999998579, 93.05995642670504253, 81.58624999999999261 ) ) ;
#438 = CARTESIAN_POINT ( 'NONE',  ( -93.67500000000003979, 92.29496732002878900, 85.97833333333332462 ) ) ;
#439 = ORIENTED_EDGE ( 'NONE', *, *, #48970, .F. ) ;
#440 = LINE ( 'NONE', #70277, #63595 ) ;
#441 = AXIS2_PLACEMENT_3D ( 'NONE', #21998, #44945, #63995 ) ;
#442 = ORIENTED_EDGE ( 'NONE', *, *, #24306, .T. ) ;
#443 = DIRECTION ( 'NONE',  ( -1.000000000000000000, 0.000000000000000000, 0.000000000000000000 ) ) ;
#444 = CARTESIAN_POINT ( 'NONE',  ( -96.15314808468745866, -211.9973110713294489, 86.57364583420047666 ) ) ;
#445 = ORIENTED_EDGE ( 'NONE', *, *, #4200, .T. ) ;
#446 = AXIS2_PLACEMENT_3D ( 'NONE', #16807, #39746, #40855 ) ;
#447 = CARTESIAN_POINT ( 'NONE',  ( 0.000000000000000000, 41.19522573413731692, 65.64334221924924861 ) ) ;
#448 = CARTESIAN_POINT ( 'NONE',  ( 94.70433044324006744, -212.6272429001183752, 74.99300273738302280 ) ) ;
#449 = CARTESIAN_POINT ( 'NONE',  ( 97.64999999999999147, -209.9999999999999716, 87.77749999999998920 ) ) ;
#450 = CARTESIAN_POINT ( 'NONE',  ( -94.99999999999997158, -212.6630814284392557, 77.10156250086711793 ) ) ;
#451 = EDGE_CURVE ( 'NONE', #39502, #20436, #22152, .T. ) ;
#452 = CYLINDRICAL_SURFACE ( 'NONE', #60264, 2.650000000000540812 ) ;
#453 = CARTESIAN_POINT ( 'NONE',  ( -3.000000000000000000, -4.261787119644969479, -26.19803753235780519 ) ) ;
#454 = VECTOR ( 'NONE', #33806, 1000.000000000000000 ) ;
#455 = CIRCLE ( 'NONE', #66471, 31.99999999999999289 ) ;
#456 = DIRECTION ( 'NONE',  ( -1.000000000000000000, 0.000000000000000000, -0.000000000000000000 ) ) ;
#457 = EDGE_CURVE ( 'NONE', #24962, #18771, #8940, .T. ) ;
#458 = DIRECTION ( 'NONE',  ( 0.000000000000000000, 0.3090169943749410120, 0.9510565162951557516 ) ) ;
#459 = ADVANCED_FACE ( 'NONE', ( #27119 ), #44445, .F. ) ;
#460 = CARTESIAN_POINT ( 'NONE',  ( 94.99999999999998579, 86.94004357329502852, 88.25374999999999659 ) ) ;
#461 = CARTESIAN_POINT ( 'NONE',  ( -96.15314808468751551, 88.00268892867056536, 78.31864583420048120 ) ) ;
#462 = DIRECTION ( 'NONE',  ( -1.000000000000000000, -0.000000000000000000, -0.000000000000000000 ) ) ;
#463 = CARTESIAN_POINT ( 'NONE',  ( 0.000000000000000000, -16.23288003029521320, 33.80338159004277543 ) ) ;
#464 = VERTEX_POINT ( 'NONE', #40275 ) ;
#465 = CARTESIAN_POINT ( 'NONE',  ( -97.64998201403183486, -208.4700114024439301, 80.50145761676010636 ) ) ;
#466 = ADVANCED_FACE ( 'NONE', ( #10577, #5342 ), #11324, .T. ) ;
#467 = DIRECTION ( 'NONE',  ( -1.000000000000000000, 0.000000000000000000, 0.000000000000000000 ) ) ;
#468 = DIRECTION ( 'NONE',  ( -1.000000000000000000, 0.000000000000000000, -0.000000000000000000 ) ) ;
#469 = LINE ( 'NONE', #45568, #28611 ) ;
#470 = CARTESIAN_POINT ( 'NONE',  ( 11.99999999999999822, -59.75363087400035056, -56.15606465355020305 ) ) ;
#471 = FACE_OUTER_BOUND ( 'NONE', #38259, .T. ) ;
#472 = CARTESIAN_POINT ( 'NONE',  ( -97.30629616937497417, -211.3315407142195852, 77.15447916753382174 ) ) ;
#473 = CARTESIAN_POINT ( 'NONE',  ( 0.000000000000000000, -26.02418014898260878, -70.52718814184285634 ) ) ;
#474 = AXIS2_PLACEMENT_3D ( 'NONE', #29907, #2130, #12619 ) ;
#475 = ORIENTED_EDGE ( 'NONE', *, *, #13669, .T. ) ;
#476 = EDGE_CURVE ( 'NONE', #51153, #68962, #28239, .T. ) ;
#477 = CARTESIAN_POINT ( 'NONE',  ( 0.000000000000000000, -73.95703589263958122, -23.16143007188505010 ) ) ;
#478 = DIRECTION ( 'NONE',  ( -0.8191520442889917986, 1.003171929053524747E-16, 0.5735764363510460484 ) ) ;
#479 = DIRECTION ( 'NONE',  ( 0.000000000000000000, 0.000000000000000000, 1.000000000000000000 ) ) ;
#480 = AXIS2_PLACEMENT_3D ( 'NONE', #12899, #47498, #41481 ) ;
#481 = FACE_OUTER_BOUND ( 'NONE', #34293, .T. ) ;
#482 = CARTESIAN_POINT ( 'NONE',  ( 10.00000000000000000, 22.64427369931169309, 30.00120703465213623 ) ) ;
#483 = DIRECTION ( 'NONE',  ( -1.000000000000000000, 0.000000000000000000, 0.000000000000000000 ) ) ;
#484 = ORIENTED_EDGE ( 'NONE', *, *, #61147, .T. ) ;
#485 = EDGE_CURVE ( 'NONE', #55045, #70907, #20950, .T. ) ;
#486 = DIRECTION ( 'NONE',  ( 0.000000000000000000, 0.000000000000000000, 1.000000000000000000 ) ) ;
#487 = ADVANCED_FACE ( 'NONE', ( #68858 ), #74107, .T. ) ;
#488 = FACE_OUTER_BOUND ( 'NONE', #49842, .T. ) ;
#489 = ORIENTED_EDGE ( 'NONE', *, *, #30011, .F. ) ;
#490 = AXIS2_PLACEMENT_3D ( 'NONE', #21064, #31973, #50001 ) ;
#491 = CARTESIAN_POINT ( 'NONE',  ( 92.69370383062501162, -209.9999999999999716, 87.73781250086713612 ) ) ;
#492 = CARTESIAN_POINT ( 'NONE',  ( -96.32499999999996021, -207.7050326799711968, 83.62354166840097491 ) ) ;
#493 = EDGE_CURVE ( 'NONE', #50397, #40961, #31739, .T. ) ;
#494 = CIRCLE ( 'NONE', #59269, 31.99999999999999289 ) ;
#495 = ORIENTED_EDGE ( 'NONE', *, *, #68774, .T. ) ;
#496 = CARTESIAN_POINT ( 'NONE',  ( 92.35000000000000853, -209.9999999999999716, 89.36499999999999488 ) ) ;
#497 = ORIENTED_EDGE ( 'NONE', *, *, #18676, .T. ) ;
#498 = AXIS2_PLACEMENT_3D ( 'NONE', #29163, #40843, #63777 ) ;
#499 = DIRECTION ( 'NONE',  ( -1.000000000000000000, -0.000000000000000000, -0.000000000000000000 ) ) ;
#500 = ORIENTED_EDGE ( 'NONE', *, *, #22914, .F. ) ;
#501 = AXIS2_PLACEMENT_3D ( 'NONE', #68859, #24108, #18089 ) ;
#502 = CARTESIAN_POINT ( 'NONE',  ( -96.15314808468752972, 91.99731107132950569, 80.80572916753382628 ) ) ;
#503 = VERTEX_POINT ( 'NONE', #39168 ) ;
#504 = LINE ( 'NONE', #32888, #943 ) ;
#505 = ORIENTED_EDGE ( 'NONE', *, *, #50, .F. ) ;
#506 = EDGE_LOOP ( 'NONE', ( #47657, #21524 ) ) ;
#507 = CARTESIAN_POINT ( 'NONE',  ( 11.99999999999999822, 75.54627589209970040, -17.28742895386005785 ) ) ;
#508 = ORIENTED_EDGE ( 'NONE', *, *, #49231, .F. ) ;
#509 = ORIENTED_EDGE ( 'NONE', *, *, #24768, .F. ) ;
#510 = B_SPLINE_CURVE_WITH_KNOTS ( 'NONE', 3,
 ( #3394, #26294, #49227, #66535, #39824, #742 ),
 .UNSPECIFIED., .F., .F.,
 ( 4, 2, 4 ),
 ( 0.7528176110416364697, 0.8153862273022683960, 0.8779548435629003222 ),
 .UNSPECIFIED. ) ;
#511 = CARTESIAN_POINT ( 'NONE',  ( 10.00000000000000000, -0.8828120875903202602, 37.48860685352291000 ) ) ;
#512 = ORIENTED_EDGE ( 'NONE', *, *, #65758, .T. ) ;
#513 = VECTOR ( 'NONE', #18864, 1000.000000000000000 ) ;
#514 = ORIENTED_EDGE ( 'NONE', *, *, #11366, .F. ) ;
#515 = CARTESIAN_POINT ( 'NONE',  ( 97.30629616937498838, 88.66845928578037217, 84.19239583420046813 ) ) ;
#516 = ORIENTED_EDGE ( 'NONE', *, *, #53833, .T. ) ;
#517 = CARTESIAN_POINT ( 'NONE',  ( 92.69370383062501162, -208.6684592857803011, 82.60489583420047666 ) ) ;
#518 = APPLICATION_PROTOCOL_DEFINITION ( 'draft international standard', 'automotive_design', 1998, #56557 ) ;
#519 = CARTESIAN_POINT ( 'NONE',  ( -94.99999999999997158, -213.0599564267049857, 81.34812500173430294 ) ) ;
#520 = CARTESIAN_POINT ( 'NONE',  ( -93.33265519076724104, -212.0887925413172184, 75.00000000000000000 ) ) ;
#521 = FACE_OUTER_BOUND ( 'NONE', #2721, .T. ) ;
#522 = PLANE ( 'NONE',  #4394 ) ;
#523 = LINE ( 'NONE', #34687, #51605 ) ;
#524 = DIRECTION ( 'NONE',  ( 0.000000000000000000, 0.000000000000000000, 1.000000000000000000 ) ) ;
#525 = CARTESIAN_POINT ( 'NONE',  ( -96.15314808468747287, -208.0026889286704943, 83.82197916753381151 ) ) ;
#526 = CARTESIAN_POINT ( 'NONE',  ( -92.69370383062502583, 88.66845928578038638, 81.17614583420048291 ) ) ;
#527 = ORIENTED_EDGE ( 'NONE', *, *, #36261, .T. ) ;
#528 = CARTESIAN_POINT ( 'NONE',  ( 94.99999999999998579, 92.66308142843935514, 83.76906250086713612 ) ) ;
#529 =( BOUNDED_CURVE ( )  B_SPLINE_CURVE ( 2, ( #47805, #72207, #66588, #9060, #20711, #13586, #71832, #43301, #43665 ),
 .UNSPECIFIED., .F., .F. ) 
 B_SPLINE_CURVE_WITH_KNOTS ( ( 3, 2, 2, 2, 3 ),
 ( 0.5291824299508934848, 0.5362381811070600079, 0.5432939466479423940, 0.5503497121888247801, 0.5503499107226622611 ),
 .UNSPECIFIED. ) 
 CURVE ( )  GEOMETRIC_REPRESENTATION_ITEM ( )  RATIONAL_B_SPLINE_CURVE ( ( 1.000000000000000000, 0.8660254037844387076, 1.000000000000000000, 0.8660254037844387076, 1.000000000000000000, 0.8660254037844387076, 1.000000000000000000, 0.9999962302473691667, 0.9999924607068835236 ) ) 
 REPRESENTATION_ITEM ( '' )  );
#530 = ORIENTED_EDGE ( 'NONE', *, *, #3696, .T. ) ;
#531 = LINE ( 'NONE', #23425, #23947 ) ;
#532 = CARTESIAN_POINT ( 'NONE',  ( 97.64999999999602665, -210.0000045800691737, 76.42687486206342840 ) ) ;
#533 = FACE_OUTER_BOUND ( 'NONE', #53175, .T. ) ;
#534 = LINE ( 'NONE', #6511, #45287 ) ;
#535 = CARTESIAN_POINT ( 'NONE',  ( -97.30629616937495996, -209.9999999999999716, 86.46781250086714010 ) ) ;
#536 = CARTESIAN_POINT ( 'NONE',  ( 10.00000000000000000, 29.81001611431041098, -22.74946021919100403 ) ) ;
#537 = EDGE_CURVE ( 'NONE', #47446, #69197, #73750, .T. ) ;
#538 = DIRECTION ( 'NONE',  ( 1.000000000000000000, -0.000000000000000000, -0.000000000000000000 ) ) ;
#539 = CARTESIAN_POINT ( 'NONE',  ( 10.00000000000000000, 70.53064760720316428, -26.01480285779861035 ) ) ;
#540 = LINE ( 'NONE', #23438, #24033 ) ;
#541 = ORIENTED_EDGE ( 'NONE', *, *, #46124, .F. ) ;
#542 = AXIS2_PLACEMENT_3D ( 'NONE', #63998, #53079, #24500 ) ;
#543 = ORIENTED_EDGE ( 'NONE', *, *, #58749, .F. ) ;
#544 = EDGE_CURVE ( 'NONE', #21721, #68051, #41359, .T. ) ;
#545 = CARTESIAN_POINT ( 'NONE',  ( -97.65000000000001990, 91.52997821335253548, 77.24708333333332178 ) ) ;
#546 = EDGE_CURVE ( 'NONE', #43524, #52685, #44810, .T. ) ;
#547 = DIRECTION ( 'NONE',  ( -1.000000000000000000, -0.000000000000000000, -0.000000000000000000 ) ) ;
#548 = CARTESIAN_POINT ( 'NONE',  ( 5.000000000000000000, 15.48615015657637706, -39.04073710021327770 ) ) ;
#549 = DIRECTION ( 'NONE',  ( -0.3853207896976547642, 0.9227826878668540234, 0.000000000000000000 ) ) ;
#550 = CARTESIAN_POINT ( 'NONE',  ( -10.00000000000000000, 0.000000000000000000, 0.000000000000000000 ) ) ;
#551 = AXIS2_PLACEMENT_3D ( 'NONE', #66850, #8604, #71359 ) ;
#552 = CARTESIAN_POINT ( 'NONE',  ( 0.000000000000000000, -1.732050807568877859, -1.752539433813135784E-17 ) ) ;
#553 = AXIS2_PLACEMENT_3D ( 'NONE', #47964, #19379, #37052 ) ;
#554 = EDGE_LOOP ( 'NONE', ( #59546, #61872, #69236, #1698 ) ) ;
#555 = CARTESIAN_POINT ( 'NONE',  ( -92.69370383062504004, 90.00000000000004263, 79.80031250086713612 ) ) ;
#556 = ADVANCED_FACE ( 'NONE', ( #33503 ), #45931, .F. ) ;
#557 = DIRECTION ( 'NONE',  ( 0.000000000000000000, 0.000000000000000000, 1.000000000000000000 ) ) ;
#558 = AXIS2_PLACEMENT_3D ( 'NONE', #43819, #60369, #66736 ) ;
#559 = CARTESIAN_POINT ( 'NONE',  ( 10.00000000000000000, 50.23322058963440639, -64.81221759200288091 ) ) ;
#560 = LINE ( 'NONE', #2036, #46654 ) ;
#561 = CARTESIAN_POINT ( 'NONE',  ( 92.35000000039373447, 90.00002930740642171, 76.74344264317738862 ) ) ;
#562 = CARTESIAN_POINT ( 'NONE',  ( 0.000000000000000000, -75.16055320797043748, 18.89407956138231270 ) ) ;
#563 = CARTESIAN_POINT ( 'NONE',  ( -96.15314808468745866, -211.9973110713294489, 87.36739583420049371 ) ) ;
#564 = AXIS2_PLACEMENT_3D ( 'NONE', #54816, #60474, #3712 ) ;
#565 = EDGE_CURVE ( 'NONE', #23559, #52552, #27876, .T. ) ;
#566 = CARTESIAN_POINT ( 'NONE',  ( 97.30629616937498838, 88.66845928578035796, 76.73114583420048973 ) ) ;
#567 = VECTOR ( 'NONE', #11381, 1000.000000000000000 ) ;
#568 = CARTESIAN_POINT ( 'NONE',  ( -96.15314808468747287, -208.0026889286704943, 78.90072916753382515 ) ) ;
#569 = DIRECTION ( 'NONE',  ( 0.000000000000000000, 0.5877852522924708056, -0.8090169943749491166 ) ) ;
#570 = ORIENTED_EDGE ( 'NONE', *, *, #37192, .T. ) ;
#571 = FACE_OUTER_BOUND ( 'NONE', #48022, .T. ) ;
#572 = DIRECTION ( 'NONE',  ( -0.000000000000000000, -0.000000000000000000, 1.000000000000000000 ) ) ;
#573 = CYLINDRICAL_SURFACE ( 'NONE', #58202, 2.649999999999985700 ) ;
#574 = DIRECTION ( 'NONE',  ( -1.000000000000000000, -0.000000000000000000, 0.000000000000000000 ) ) ;
#575 = CARTESIAN_POINT ( 'NONE',  ( 97.30629616937498838, -208.6684592857803011, 78.58322916753381548 ) ) ;
#576 = ORIENTED_EDGE ( 'NONE', *, *, #2147, .F. ) ;
#577 = EDGE_CURVE ( 'NONE', #43302, #35704, #70298, .T. ) ;
#578 = EDGE_CURVE ( 'NONE', #23298, #25333, #62669, .T. ) ;
#579 = VECTOR ( 'NONE', #18980, 1000.000000000000000 ) ;
#580 = FACE_OUTER_BOUND ( 'NONE', #12043, .T. ) ;
#581 = ORIENTED_EDGE ( 'NONE', *, *, #28091, .T. ) ;
#582 = CARTESIAN_POINT ( 'NONE',  ( 1.250000000000000444, -16.78109714094927085, 0.000000000000000000 ) ) ;
#583 = EDGE_LOOP ( 'NONE', ( #10070, #55687, #11544, #43388 ) ) ;
#584 = CYLINDRICAL_SURFACE ( 'NONE', #16618, 16.00000000000000000 ) ;
#585 = CIRCLE ( 'NONE', #53347, 42.00000000000000000 ) ;
#586 = EDGE_LOOP ( 'NONE', ( #41362, #43184, #19887, #37146 ) ) ;
#587 = ORIENTED_EDGE ( 'NONE', *, *, #27135, .F. ) ;
#588 = VERTEX_POINT ( 'NONE', #34626 ) ;
#589 = CARTESIAN_POINT ( 'NONE',  ( 96.92442009029420547, -211.8218417373832096, 75.00000000000001421 ) ) ;
#590 = VERTEX_POINT ( 'NONE', #56835 ) ;
#591 = CIRCLE ( 'NONE', #53356, 35.50000000000000711 ) ;
#592 = ORIENTED_EDGE ( 'NONE', *, *, #52648, .T. ) ;
#593 = CARTESIAN_POINT ( 'NONE',  ( 97.30629616937498838, 90.00000000000002842, 83.76906250086716454 ) ) ;
#594 = AXIS2_PLACEMENT_3D ( 'NONE', #11700, #37618, #37250 ) ;
#596 = CARTESIAN_POINT ( 'NONE',  ( 96.32499999999998863, -212.2949673200287179, 76.24166666666666003 ) ) ;
#595 = AXIS2_PLACEMENT_3D ( 'NONE', #68160, #67039, #38481 ) ;
#597 = ORIENTED_EDGE ( 'NONE', *, *, #35391, .T. ) ;
#598 = ORIENTED_EDGE ( 'NONE', *, *, #41493, .T. ) ;
#599 = ORIENTED_EDGE ( 'NONE', *, *, #44383, .T. ) ;
#600 = ORIENTED_EDGE ( 'NONE', *, *, #27391, .T. ) ;
#601 = FACE_BOUND ( 'NONE', #61690, .T. ) ;
#602 =( NAMED_UNIT ( * ) PLANE_ANGLE_UNIT ( ) SI_UNIT ( $, .RADIAN. ) );
#603 = CARTESIAN_POINT ( 'NONE',  ( -92.34999999999999432, -209.9999999999999716, 85.23749999999999716 ) ) ;
#604 = CARTESIAN_POINT ( 'NONE',  ( 10.00000000000000000, 26.08949754953024325, 27.05870788708241648 ) ) ;
#605 = CYLINDRICAL_SURFACE ( 'NONE', #65079, 2.649999999999985700 ) ;
#606 = CYLINDRICAL_SURFACE ( 'NONE', #23467, 16.00000000000000000 ) ;
#607 = AXIS2_PLACEMENT_3D ( 'NONE', #43704, #71876, #9106 ) ;
#608 = CARTESIAN_POINT ( 'NONE',  ( 10.00000000000000000, 17.80606268964540462, 33.00180498840053644 ) ) ;
#609 = DIRECTION ( 'NONE',  ( -1.000000000000000000, -0.000000000000000000, -0.000000000000000000 ) ) ;
#610 = ORIENTED_EDGE ( 'NONE', *, *, #1325, .T. ) ;
#611 = CARTESIAN_POINT ( 'NONE',  ( -93.67499999999998295, -212.2949673200287179, 79.49604166840096298 ) ) ;
#612 = EDGE_LOOP ( 'NONE', ( #17860, #45967, #2763, #45895 ) ) ;
#613 = DIRECTION ( 'NONE',  ( 0.000000000000000000, -0.4539904997395540764, 0.8910065241883642351 ) ) ;
#614 = AXIS2_PLACEMENT_3D ( 'NONE', #15545, #73036, #49383 ) ;
#615 = ORIENTED_EDGE ( 'NONE', *, *, #59441, .T. ) ;
#616 = EDGE_CURVE ( 'NONE', #5747, #25646, #18544, .T. ) ;
#618 = CARTESIAN_POINT ( 'NONE',  ( -95.00000000000002842, 93.05995642670501411, 81.03062500173430749 ) ) ;
#617 = CARTESIAN_POINT ( 'NONE',  ( 94.99999999999998579, 86.94004357329500010, 80.71312500173431204 ) ) ;
#619 = ORIENTED_EDGE ( 'NONE', *, *, #26416, .F. ) ;
#620 = CARTESIAN_POINT ( 'NONE',  ( 97.30629616937498838, 91.33154071421968467, 79.37697916753381833 ) ) ;
#621 = CARTESIAN_POINT ( 'NONE',  ( -93.67499999999998295, -207.7050326799711968, 82.16833333333332234 ) ) ;
#622 = CARTESIAN_POINT ( 'NONE',  ( 0.000000000000000000, 27.74655509720780344, -77.16300072079631889 ) ) ;
#623 = CIRCLE ( 'NONE', #39007, 77.49899999999999523 ) ;
#624 = ADVANCED_FACE ( 'NONE', ( #40645, #51552 ), #36846, .T. ) ;
#625 = CYLINDRICAL_SURFACE ( 'NONE', #23007, 2.649999999999999467 ) ;
#626 = CARTESIAN_POINT ( 'NONE',  ( 92.35000000000000853, -209.9999999999999716, 84.28499999999999659 ) ) ;
#627 = EDGE_LOOP ( 'NONE', ( #39309, #43860, #42175, #54202, #70134, #50291 ) ) ;
#628 = CARTESIAN_POINT ( 'NONE',  ( -92.35000000000003695, 90.00000000000004263, 80.15749999999999886 ) ) ;
#629 = DIRECTION ( 'NONE',  ( -1.000000000000000000, 0.000000000000000000, -0.000000000000000000 ) ) ;
#630 = CARTESIAN_POINT ( 'NONE',  ( 0.000000000000000000, -37.48860685352290290, -0.8828120875904512665 ) ) ;
#631 = EDGE_LOOP ( 'NONE', ( #18780, #16378, #8241, #67951 ) ) ;
#632 = EDGE_CURVE ( 'NONE', #62228, #65777, #28151, .T. ) ;
#633 = VERTEX_POINT ( 'NONE', #13543 ) ;
#634 = EDGE_CURVE ( 'NONE', #41342, #12738, #7756, .T. ) ;
#635 = CARTESIAN_POINT ( 'NONE',  ( 10.00000000000000000, -16.23288003029473359, -33.80338159004301701 ) ) ;
#636 = FACE_OUTER_BOUND ( 'NONE', #73794, .T. ) ;
#637 = LINE ( 'NONE', #52844, #42561 ) ;
#638 = CARTESIAN_POINT ( 'NONE',  ( -92.69370383062498320, -208.6684592857803011, 76.20197916753382117 ) ) ;
#639 = ORIENTED_EDGE ( 'NONE', *, *, #74332, .F. ) ;
#640 = ADVANCED_FACE ( 'NONE', ( #6800 ), #18087, .T. ) ;
#641 = DIRECTION ( 'NONE',  ( 0.000000000000000000, 0.000000000000000000, 1.000000000000000000 ) ) ;
#642 = AXIS2_PLACEMENT_3D ( 'NONE', #45335, #55858, #4749 ) ;
#643 = LINE ( 'NONE', #23906, #4726 ) ;
#644 = FACE_BOUND ( 'NONE', #53061, .T. ) ;
#645 = CARTESIAN_POINT ( 'NONE',  ( 94.99999999999998579, 87.33691857156068750, 75.83156250086715033 ) ) ;
#646 = DIRECTION ( 'NONE',  ( -1.000000000000000000, 0.000000000000000000, 0.000000000000000000 ) ) ;
#647 = LINE ( 'NONE', #69041, #51696 ) ;
#648 = FACE_OUTER_BOUND ( 'NONE', #4489, .T. ) ;
#649 = LINE ( 'NONE', #40460, #53242 ) ;
#650 = CARTESIAN_POINT ( 'NONE',  ( 15.00000000000000000, 14.60985201121703980, -18.46759930825707841 ) ) ;
#651 = EDGE_CURVE ( 'NONE', #53386, #50810, #36469, .T. ) ;
#652 = CIRCLE ( 'NONE', #28184, 11.59999999999999787 ) ;
#653 = EDGE_CURVE ( 'NONE', #39661, #53810, #37773, .T. ) ;
#654 = AXIS2_PLACEMENT_3D ( 'NONE', #45899, #28211, #35347 ) ;
#655 = CARTESIAN_POINT ( 'NONE',  ( 97.30629616937498838, 88.66845928578035796, 85.62114583420047609 ) ) ;
#656 = EDGE_CURVE ( 'NONE', #45592, #59758, #43789, .T. ) ;
#657 = DIRECTION ( 'NONE',  ( 0.000000000000000000, 0.4539904997395477482, -0.8910065241883673437 ) ) ;
#658 = DIRECTION ( 'NONE',  ( 1.000000000000000000, 0.000000000000000000, 0.000000000000000000 ) ) ;
#659 = ORIENTED_EDGE ( 'NONE', *, *, #57378, .T. ) ;
#660 = DIRECTION ( 'NONE',  ( -1.000000000000000000, 0.000000000000000000, 0.000000000000000000 ) ) ;
#661 = CARTESIAN_POINT ( 'NONE',  ( -92.69370383062505425, 88.66845928578038638, 81.01739583420048518 ) ) ;
#662 = EDGE_CURVE ( 'NONE', #8349, #73763, #13173, .T. ) ;
#664 = EDGE_CURVE ( 'NONE', #39348, #15750, #53376, .T. ) ;
#663 = AXIS2_PLACEMENT_3D ( 'NONE', #26223, #37524, #31862 ) ;
#665 = VECTOR ( 'NONE', #62386, 1000.000000000000000 ) ;
#666 = CARTESIAN_POINT ( 'NONE',  ( 97.30629616937498838, -209.9999999999999716, 86.78531250086714977 ) ) ;
#667 = EDGE_CURVE ( 'NONE', #38085, #21754, #59390, .T. ) ;
#668 = ORIENTED_EDGE ( 'NONE', *, *, #18506, .T. ) ;
#669 = CARTESIAN_POINT ( 'NONE',  ( -92.35000000000003695, 89.99999996655868983, 87.85687500050293863 ) ) ;
#670 = PLANE ( 'NONE',  #22865 ) ;
#671 = CIRCLE ( 'NONE', #61866, 19.05560546998412974 ) ;
#672 = ORIENTED_EDGE ( 'NONE', *, *, #52995, .F. ) ;
#673 = EDGE_CURVE ( 'NONE', #53082, #50612, #29711, .T. ) ;
#674 = CARTESIAN_POINT ( 'NONE',  ( 7.103376864691351012E-17, -120.0000000000000000, -64.00000000000000000 ) ) ;
#675 = DIRECTION ( 'NONE',  ( 0.000000000000000000, 0.07845909572783797692, 0.9969173337331285190 ) ) ;
#676 = AXIS2_PLACEMENT_3D ( 'NONE', #2122, #58480, #24642 ) ;
#677 = ORIENTED_EDGE ( 'NONE', *, *, #18568, .T. ) ;
#678 = ORIENTED_EDGE ( 'NONE', *, *, #36155, .F. ) ;
#679 = CARTESIAN_POINT ( 'NONE',  ( 97.30629616937498838, -209.9999999999999716, 81.86406250086714920 ) ) ;
#680 = CYLINDRICAL_SURFACE ( 'NONE', #59674, 2.649999999999985700 ) ;
#681 = DIRECTION ( 'NONE',  ( -0.000000000000000000, -0.000000000000000000, 1.000000000000000000 ) ) ;
#682 = CARTESIAN_POINT ( 'NONE',  ( 0.000000000000000000, 39.47590169984945163, -71.87247863392373404 ) ) ;
#683 = CARTESIAN_POINT ( 'NONE',  ( 97.64999999989933599, 90.00002309722570715, 83.41187580057898288 ) ) ;
#684 = CARTESIAN_POINT ( 'NONE',  ( 5.000000000000000000, -50.23322058963393744, 64.81221759200325039 ) ) ;
#685 = CARTESIAN_POINT ( 'NONE',  ( 95.00000000000000000, -206.9400435732949575, 84.12625000000001307 ) ) ;
#686 = ORIENTED_EDGE ( 'NONE', *, *, #12634, .T. ) ;
#687 = ORIENTED_EDGE ( 'NONE', *, *, #21533, .F. ) ;
#688 = VERTEX_POINT ( 'NONE', #70670 ) ;
#689 = ORIENTED_EDGE ( 'NONE', *, *, #8488, .T. ) ;
#690 = CARTESIAN_POINT ( 'NONE',  ( 23.50000000000218847, -119.9999999999999716, -48.99999999999936051 ) ) ;
#691 = VECTOR ( 'NONE', #33949, 1000.000000000000000 ) ;
#692 = SURFACE_SIDE_STYLE ('',( #30321 ) ) ;
#693 = CARTESIAN_POINT ( 'NONE',  ( -93.84685191531252713, 88.00268892867056536, 88.74322916753382628 ) ) ;
#694 = CARTESIAN_POINT ( 'NONE',  ( 0.000000000000000000, 0.000000000000000000, 0.000000000000000000 ) ) ;
#695 = PLANE ( 'NONE',  #20980 ) ;
#696 = CARTESIAN_POINT ( 'NONE',  ( 92.35000000000000853, -209.9999999999999716, 76.74437500173429783 ) ) ;
#697 = CARTESIAN_POINT ( 'NONE',  ( 97.64999999999997726, 91.52997821335252127, 78.30541666666668732 ) ) ;
#698 = ORIENTED_EDGE ( 'NONE', *, *, #67370, .F. ) ;
#699 = CARTESIAN_POINT ( 'NONE',  ( -93.67499999999998295, -207.7050326799711968, 89.23270833506762756 ) ) ;
#700 = ORIENTED_EDGE ( 'NONE', *, *, #70526, .F. ) ;
#701 = DIRECTION ( 'NONE',  ( -0.000000000000000000, -1.000000000000000000, -0.000000000000000000 ) ) ;
#702 = ORIENTED_EDGE ( 'NONE', *, *, #35715, .T. ) ;
#703 = CARTESIAN_POINT ( 'NONE',  ( -97.65000000000001990, 90.00000000000004263, 88.17437500173430465 ) ) ;
#704 = CARTESIAN_POINT ( 'NONE',  ( -92.69370383062505425, 88.66845928578038638, 82.44614583420049314 ) ) ;
#705 = CARTESIAN_POINT ( 'NONE',  ( 97.30629616937498838, 91.33154071421968467, 76.04322916753380923 ) ) ;
#706 = CIRCLE ( 'NONE', #10260, 31.99999999999998579 ) ;
#707 = ORIENTED_EDGE ( 'NONE', *, *, #65946, .T. ) ;
#708 = CARTESIAN_POINT ( 'NONE',  ( 10.00000000000000000, -10.74501242461258244, -35.92658777277521409 ) ) ;
#709 = DIRECTION ( 'NONE',  ( 0.000000000000000000, 0.000000000000000000, -1.000000000000000000 ) ) ;
#710 = CARTESIAN_POINT ( 'NONE',  ( 95.00000000000000000, -213.0599564267049857, 85.71374999999999034 ) ) ;
#711 = ADVANCED_FACE ( 'NONE', ( #59052 ), #836, .T. ) ;
#712 = CARTESIAN_POINT ( 'NONE',  ( 15.00000000000000000, 6.762365576493310826, -25.66652317338401090 ) ) ;
#713 = ORIENTED_EDGE ( 'NONE', *, *, #55662, .F. ) ;
#714 = CARTESIAN_POINT ( 'NONE',  ( 15.00000000000000000, -18.13022148937263012, -15.02647892043543898 ) ) ;
#715 = AXIS2_PLACEMENT_3D ( 'NONE', #66827, #15314, #46127 ) ;
#716 = CARTESIAN_POINT ( 'NONE',  ( -97.30629616937497417, -208.6684592857803011, 76.88989583420047325 ) ) ;
#717 = ORIENTED_EDGE ( 'NONE', *, *, #11315, .T. ) ;
#718 = EDGE_CURVE ( 'NONE', #14320, #31534, #29205, .T. ) ;
#719 = VERTEX_POINT ( 'NONE', #2311 ) ;
#721 = CARTESIAN_POINT ( 'NONE',  ( 97.64999999946594755, 90.00005320149050192, 78.96687695417308817 ) ) ;
#720 = VECTOR ( 'NONE', #25751, 1000.000000000000000 ) ;
#722 = EDGE_CURVE ( 'NONE', #29955, #52790, #71225, .T. ) ;
#723 = EDGE_CURVE ( 'NONE', #44034, #16018, #25617, .T. ) ;
#724 = ORIENTED_EDGE ( 'NONE', *, *, #39012, .T. ) ;
#725 = CARTESIAN_POINT ( 'NONE',  ( 0.000000000000000000, -62.50884508063395373, -41.76106447765554464 ) ) ;
#726 = CARTESIAN_POINT ( 'NONE',  ( 9.984461079971730157, -95.40710393340120277, 5.500000000000000000 ) ) ;
#727 = ORIENTED_EDGE ( 'NONE', *, *, #31301, .F. ) ;
#728 = CARTESIAN_POINT ( 'NONE',  ( -97.30629616937497417, -211.3315407142195852, 87.94947916753382344 ) ) ;
#729 = VERTEX_POINT ( 'NONE', #41025 ) ;
#730 = CARTESIAN_POINT ( 'NONE',  ( 97.64999999994533653, 89.99998298270493535, 88.49187441316099978 ) ) ;
#731 = CARTESIAN_POINT ( 'NONE',  ( 0.000000000000000000, -74.74816331893453025, 33.71516098798714722 ) ) ;
#732 = ORIENTED_EDGE ( 'NONE', *, *, #49373, .F. ) ;
#733 = VECTOR ( 'NONE', #407, 1000.000000000000000 ) ;
#734 = ORIENTED_EDGE ( 'NONE', *, *, #67580, .F. ) ;
#735 = CARTESIAN_POINT ( 'NONE',  ( -97.65000000000001990, 90.00000000000004263, 83.72937500173429726 ) ) ;
#736 = CIRCLE ( 'NONE', #30667, 16.00000000000000355 ) ;
#737 = EDGE_CURVE ( 'NONE', #34884, #37666, #67655, .T. ) ;
#738 = CARTESIAN_POINT ( 'NONE',  ( 94.99999999999998579, 87.33691857156068750, 85.99156250086714692 ) ) ;
#739 = CARTESIAN_POINT ( 'NONE',  ( -23.54415474984308787, -120.4156646670583086, 5.500000000000000000 ) ) ;
#740 = FACE_OUTER_BOUND ( 'NONE', #186, .T. ) ;
#741 = CARTESIAN_POINT ( 'NONE',  ( 0.000000000000000000, -36.73666225445845157, -65.58780272294114866 ) ) ;
#742 = CARTESIAN_POINT ( 'NONE',  ( 96.90829729882862864, -211.8387227684681591, 74.99954709728268654 ) ) ;
#743 = EDGE_CURVE ( 'NONE', #60856, #66942, #69583, .T. ) ;
#744 = DIRECTION ( 'NONE',  ( -1.000000000000000000, -0.000000000000000000, -0.000000000000000000 ) ) ;
#745 = CARTESIAN_POINT ( 'NONE',  ( 95.00000000000000000, -213.0599564267049857, 87.69812500173429726 ) ) ;
#746 = CARTESIAN_POINT ( 'NONE',  ( 10.00000000000000000, 17.67226234102874116, -33.17418723428288274 ) ) ;
#747 =( BOUNDED_CURVE ( )  B_SPLINE_CURVE ( 2, ( #24289, #12255, #25012, #14741, #18627, #40847, #41566, #47953, #70870 ),
 .UNSPECIFIED., .F., .F. ) 
 B_SPLINE_CURVE_WITH_KNOTS ( ( 3, 2, 2, 2, 3 ),
 ( 0.2751748541917909407, 0.2822306216366805010, 0.2892863871775971929, 0.2963421527185139959, 0.2963422021995995026 ),
 .UNSPECIFIED. ) 
 CURVE ( )  GEOMETRIC_REPRESENTATION_ITEM ( )  RATIONAL_B_SPLINE_CURVE ( ( 1.000000000000000000, 0.8660254037844387076, 1.000000000000000000, 0.8660254037844387076, 1.000000000000000000, 0.8660254037844387076, 1.000000000000000000, 0.9999990604551106665, 0.9999981209233991253 ) ) 
 REPRESENTATION_ITEM ( '' )  );
#748 = DIRECTION ( 'NONE',  ( -2.628368902995175337E-16, -1.000000000000000000, 0.000000000000000000 ) ) ;
#749 = DIRECTION ( 'NONE',  ( -0.000000000000000000, 0.5000000000000038858, 0.8660254037844363761 ) ) ;
#750 = DIRECTION ( 'NONE',  ( 0.000000000000000000, 0.5877852522924780221, 0.8090169943749438985 ) ) ;
#751 = EDGE_CURVE ( 'NONE', #28286, #68468, #38828, .T. ) ;
#752 = EDGE_CURVE ( 'NONE', #15096, #60587, #35726, .T. ) ;
#753 = CARTESIAN_POINT ( 'NONE',  ( 26.47460221209471598, -121.8961639463267090, 5.500000000000000000 ) ) ;
#754 = DIRECTION ( 'NONE',  ( -1.000000000000000000, -0.000000000000000000, 0.000000000000000000 ) ) ;
#755 = ORIENTED_EDGE ( 'NONE', *, *, #11773, .T. ) ;
#756 =( BOUNDED_CURVE ( )  B_SPLINE_CURVE ( 2, ( #59486, #48574, #47465, #64762, #25279, #41816, #36176, #7978, #48203 ),
 .UNSPECIFIED., .F., .F. ) 
 B_SPLINE_CURVE_WITH_KNOTS ( ( 3, 2, 2, 2, 3 ),
 ( 0.4021785743347534581, 0.4021786358322713695, 0.4092344013731880059, 0.4162901669141046423, 0.4233457466706606609 ),
 .UNSPECIFIED. ) 
 CURVE ( )  GEOMETRIC_REPRESENTATION_ITEM ( )  RATIONAL_B_SPLINE_CURVE ( ( 0.9999976645954944399, 0.9999988322875694724, 1.000000000000000000, 0.8660254037844387076, 1.000000000000000000, 0.8660254037844387076, 1.000000000000000000, 0.8660289314505091873, 0.9999929448536319931 ) ) 
 REPRESENTATION_ITEM ( '' )  );
#757 = DIRECTION ( 'NONE',  ( 0.000000000000000000, 0.000000000000000000, 1.000000000000000000 ) ) ;
#758 = AXIS2_PLACEMENT_3D ( 'NONE', #12505, #70010, #6510 ) ;
#759 = DIRECTION ( 'NONE',  ( 0.000000000000000000, -0.7604059656000227152, -0.6494480483301934282 ) ) ;
#760 = DIRECTION ( 'NONE',  ( 0.000000000000000000, 0.000000000000000000, 1.000000000000000000 ) ) ;
#761 = CARTESIAN_POINT ( 'NONE',  ( -93.67500000000003979, 87.70503267997129626, 77.59104166840097605 ) ) ;
#762 = CYLINDRICAL_SURFACE ( 'NONE', #9243, 16.00000000000000000 ) ;
#763 = AXIS2_PLACEMENT_3D ( 'NONE', #36619, #70444, #32081 ) ;
#764 = CARTESIAN_POINT ( 'NONE',  ( 96.15314808468748708, -208.0026889286704943, 83.87489583420048689 ) ) ;
#765 = VECTOR ( 'NONE', #15129, 1000.000000000000000 ) ;
#766 = VERTEX_POINT ( 'NONE', #25933 ) ;
#767 = AXIS2_PLACEMENT_3D ( 'NONE', #73077, #44536, #67455 ) ;
#768 = EDGE_LOOP ( 'NONE', ( #52256, #54474, #28723, #42542 ) ) ;
#769 = VERTEX_POINT ( 'NONE', #31569 ) ;
#770 = AXIS2_PLACEMENT_3D ( 'NONE', #9925, #56553, #16690 ) ;
#771 = CARTESIAN_POINT ( 'NONE',  ( 0.000000000000000000, 0.000000000000000000, 42.00000000000001421 ) ) ;
#772 = VECTOR ( 'NONE', #57930, 1000.000000000000000 ) ;
#773 = CARTESIAN_POINT ( 'NONE',  ( 96.15314808468748708, -208.0026889286704943, 75.46114583420047950 ) ) ;
#774 = ORIENTED_EDGE ( 'NONE', *, *, #54561, .F. ) ;
#775 = CARTESIAN_POINT ( 'NONE',  ( 92.69370383062501162, -208.6684592857803011, 80.85864583420048746 ) ) ;
#776 = EDGE_LOOP ( 'NONE', ( #60937, #39384, #65729, #18843 ) ) ;
#777 = LINE ( 'NONE', #12011, #7121 ) ;
#778 = ORIENTED_EDGE ( 'NONE', *, *, #49916, .F. ) ;
#779 = VERTEX_POINT ( 'NONE', #26670 ) ;
#780 = LINE ( 'NONE', #58251, #57390 ) ;
#781 = AXIS2_PLACEMENT_3D ( 'NONE', #6819, #24847, #19567 ) ;
#782 = DIRECTION ( 'NONE',  ( 0.000000000000000000, 0.000000000000000000, 1.000000000000000000 ) ) ;
#783 = ORIENTED_EDGE ( 'NONE', *, *, #47685, .F. ) ;
#784 = DIRECTION ( 'NONE',  ( 0.000000000000000000, 0.000000000000000000, 1.000000000000000000 ) ) ;
#785 = CARTESIAN_POINT ( 'NONE',  ( 96.32499999999998863, -207.7050326799711968, 87.96270833506763154 ) ) ;
#786 = ORIENTED_EDGE ( 'NONE', *, *, #5639, .T. ) ;
#787 = DIRECTION ( 'NONE',  ( -1.000000000000000000, -0.000000000000000000, -0.000000000000000000 ) ) ;
#788 = ORIENTED_EDGE ( 'NONE', *, *, #22355, .T. ) ;
#789 = DIRECTION ( 'NONE',  ( -1.000000000000000000, -0.000000000000000000, 0.000000000000000000 ) ) ;
#790 = ORIENTED_EDGE ( 'NONE', *, *, #1567, .F. ) ;
#791 = EDGE_CURVE ( 'NONE', #29550, #48269, #72525, .T. ) ;
#792 = CARTESIAN_POINT ( 'NONE',  ( 97.64999999999997726, 91.52997821335252127, 87.27479166840096525 ) ) ;
#793 = EDGE_CURVE ( 'NONE', #67190, #11833, #21029, .T. ) ;
#794 = ORIENTED_EDGE ( 'NONE', *, *, #4900, .T. ) ;
#795 =( LENGTH_UNIT ( ) NAMED_UNIT ( * ) SI_UNIT ( .MILLI., .METRE. ) );
#796 = ORIENTED_EDGE ( 'NONE', *, *, #32317, .T. ) ;
#797 = DIRECTION ( 'NONE',  ( 0.000000000000000000, 0.1564344650402244019, 0.9876883405951387696 ) ) ;
#798 = DIRECTION ( 'NONE',  ( 0.000000000000000000, 0.000000000000000000, 1.000000000000000000 ) ) ;
#799 = ORIENTED_EDGE ( 'NONE', *, *, #19594, .F. ) ;
#800 = AXIS2_PLACEMENT_3D ( 'NONE', #26996, #3729, #16474 ) ;
#801 = ORIENTED_EDGE ( 'NONE', *, *, #36762, .T. ) ;
#802 = EDGE_CURVE ( 'NONE', #24152, #23304, #61645, .T. ) ;
#803 = ORIENTED_EDGE ( 'NONE', *, *, #14680, .F. ) ;
#804 = DIRECTION ( 'NONE',  ( -1.000000000000000000, 0.000000000000000000, 0.000000000000000000 ) ) ;
#805 = FACE_OUTER_BOUND ( 'NONE', #65981, .T. ) ;
#806 = ADVANCED_FACE ( 'NONE', ( #54514 ), #43981, .F. ) ;
#807 = CARTESIAN_POINT ( 'NONE',  ( -95.00000000000002842, 86.94004357329504273, 86.98374999999998636 ) ) ;
#808 = VERTEX_POINT ( 'NONE', #66179 ) ;
#809 = CARTESIAN_POINT ( 'NONE',  ( -0.8815729230226008184, -93.47222532549339746, -5.500000000000000000 ) ) ;
#810 = EDGE_LOOP ( 'NONE', ( #25878, #42076, #22977, #8689 ) ) ;
#811 = LINE ( 'NONE', #46635, #58781 ) ;
#812 = CARTESIAN_POINT ( 'NONE',  ( -96.15314808468747287, -208.0026889286704943, 85.72697916753379843 ) ) ;
#814 = ORIENTED_EDGE ( 'NONE', *, *, #38959, .F. ) ;
#813 = EDGE_CURVE ( 'NONE', #67853, #69733, #42870, .T. ) ;
#815 = CARTESIAN_POINT ( 'NONE',  ( -97.64999999992174651, -209.9999869687493685, 79.28395951166956479 ) ) ;
#816 = CIRCLE ( 'NONE', #59598, 16.00000000000000000 ) ;
#817 = DIRECTION ( 'NONE',  ( 1.000000000000000000, 0.000000000000000000, 0.000000000000000000 ) ) ;
#818 = CARTESIAN_POINT ( 'NONE',  ( 0.000000000000000000, -81.96053171279903893, 2.543863470248101333 ) ) ;
#819 = CARTESIAN_POINT ( 'NONE',  ( -93.84685191531248449, -208.0026889286704943, 74.82614583420047438 ) ) ;
#820 = DIRECTION ( 'NONE',  ( -2.603472992746261562E-14, -2.546204323184492723E-14, 1.000000000000000000 ) ) ;
#821 = CARTESIAN_POINT ( 'NONE',  ( 0.000000000000000000, 55.20638768913760686, 51.02545421589343988 ) ) ;
#822 = VECTOR ( 'NONE', #46720, 1000.000000000000000 ) ;
#823 = LINE ( 'NONE', #22987, #58907 ) ;
#824 = FACE_OUTER_BOUND ( 'NONE', #34255, .T. ) ;
#825 = AXIS2_PLACEMENT_3D ( 'NONE', #17122, #51706, #44594 ) ;
#826 = DIRECTION ( 'NONE',  ( -0.000000000000000000, -0.000000000000000000, 1.000000000000000000 ) ) ;
#827 = ADVANCED_FACE ( 'NONE', ( #55624 ), #60537, .F. ) ;
#828 = CARTESIAN_POINT ( 'NONE',  ( 10.00000000000000000, -56.15606465355001120, 59.75363087400054951 ) ) ;
#829 = EDGE_CURVE ( 'NONE', #43747, #51185, #3600, .T. ) ;
#830 = CARTESIAN_POINT ( 'NONE',  ( -96.15314808468752972, 91.99731107132950569, 77.47197916753380298 ) ) ;
#831 = DIRECTION ( 'NONE',  ( 0.000000000000000000, 0.8090169943749487835, -0.5877852522924713607 ) ) ;
#832 = DIRECTION ( 'NONE',  ( -1.000000000000000000, 0.000000000000000000, 0.000000000000000000 ) ) ;
#833 = CIRCLE ( 'NONE', #22361, 1.000000000000000888 ) ;
#834 = CIRCLE ( 'NONE', #65457, 16.00000000000000000 ) ;
#835 = ORIENTED_EDGE ( 'NONE', *, *, #23203, .F. ) ;
#836 = CYLINDRICAL_SURFACE ( 'NONE', #58045, 31.99999999999999289 ) ;
#837 = PLANE ( 'NONE',  #5857 ) ;
#838 = EDGE_CURVE ( 'NONE', #24699, #32014, #49262, .T. ) ;
#839 = EDGE_CURVE ( 'NONE', #45762, #32475, #26300, .T. ) ;
#840 = CARTESIAN_POINT ( 'NONE',  ( -0.0004442498512760095037, 0.001194404164628348752, -49.00000000000000000 ) ) ;
#841 = CARTESIAN_POINT ( 'NONE',  ( 10.00000000000000000, -37.58145647212455032, 0.6853352020789044152 ) ) ;
#842 = AXIS2_PLACEMENT_3D ( 'NONE', #18020, #1510, #46224 ) ;
#843 = DIRECTION ( 'NONE',  ( 1.000000000000000000, 1.427937372958405461E-15, 7.962523111839130290E-16 ) ) ;
#844 = CARTESIAN_POINT ( 'NONE',  ( -96.15314808468747287, -208.0026889286704943, 76.99572916753382401 ) ) ;
#845 = FACE_OUTER_BOUND ( 'NONE', #61404, .T. ) ;
#846 = ORIENTED_EDGE ( 'NONE', *, *, #38350, .T. ) ;
#847 = CARTESIAN_POINT ( 'NONE',  ( 0.000000000000000000, -31.52238457039579345, -27.75498641678775158 ) ) ;
#848 = CARTESIAN_POINT ( 'NONE',  ( 0.000000000000000000, 33.71516098798740302, 74.74816331893443078 ) ) ;
#849 = DIRECTION ( 'NONE',  ( 0.000000000000000000, 0.000000000000000000, -1.000000000000000000 ) ) ;
#850 = LINE ( 'NONE', #68873, #20942 ) ;
#851 = DIRECTION ( 'NONE',  ( 0.000000000000000000, 0.000000000000000000, -1.000000000000000000 ) ) ;
#852 = VERTEX_POINT ( 'NONE', #15772 ) ;
#853 = CARTESIAN_POINT ( 'NONE',  ( 12.00000000000000000, 20.85821328998741109, -10.92862929874522671 ) ) ;
#854 =( NAMED_UNIT ( * ) SI_UNIT ( $, .STERADIAN. ) SOLID_ANGLE_UNIT ( ) );
#855 = VERTEX_POINT ( 'NONE', #65800 ) ;
#856 = CARTESIAN_POINT ( 'NONE',  ( 97.30629616937498838, -208.6684592857803295, 83.66322916753381378 ) ) ;
#857 = CARTESIAN_POINT ( 'NONE',  ( -3.000000000000000000, -13.04903810567647682, -19.60159698893442481 ) ) ;
#858 = AXIS2_PLACEMENT_3D ( 'NONE', #17609, #45833, #68755 ) ;
#859 = ORIENTED_EDGE ( 'NONE', *, *, #57057, .T. ) ;
#860 = DIRECTION ( 'NONE',  ( -0.000000000000000000, -0.000000000000000000, -1.000000000000000000 ) ) ;
#861 = AXIS2_PLACEMENT_3D ( 'NONE', #12106, #35045, #12475 ) ;
#862 = ORIENTED_EDGE ( 'NONE', *, *, #52454, .F. ) ;
#863 = DIRECTION ( 'NONE',  ( -1.000000000000000000, -0.000000000000000000, 0.000000000000000000 ) ) ;
#864 = ORIENTED_EDGE ( 'NONE', *, *, #47800, .T. ) ;
#865 = CARTESIAN_POINT ( 'NONE',  ( -92.69370383062502583, 91.33154071421968467, 80.01197916753380923 ) ) ;
#866 = ORIENTED_EDGE ( 'NONE', *, *, #10496, .F. ) ;
#867 = CIRCLE ( 'NONE', #42855, 42.00000000000000000 ) ;
#868 = EDGE_LOOP ( 'NONE', ( #22669, #43084, #16669, #61333 ) ) ;
#869 = EDGE_CURVE ( 'NONE', #18817, #10724, #10128, .T. ) ;
#870 = VECTOR ( 'NONE', #36288, 1000.000000000000000 ) ;
#871 =( BOUNDED_CURVE ( )  B_SPLINE_CURVE ( 2, ( #24028, #46957, #18006, #63886, #69869, #12357, #35300 ),
 .UNSPECIFIED., .F., .F. ) 
 B_SPLINE_CURVE_WITH_KNOTS ( ( 3, 2, 2, 3 ),
 ( 0.8333333333333334814, 0.8402777777777779011, 0.8472222222222222099, 0.8541666666666666297 ),
 .UNSPECIFIED. ) 
 CURVE ( )  GEOMETRIC_REPRESENTATION_ITEM ( )  RATIONAL_B_SPLINE_CURVE ( ( 0.9999999999999978906, 0.8660254037844408170, 1.000000000000000000, 0.8660254037844387076, 1.000000000000000000, 0.8660254037844387076, 1.000000000000000000 ) ) 
 REPRESENTATION_ITEM ( '' )  );
#872 = ORIENTED_EDGE ( 'NONE', *, *, #54865, .T. ) ;
#873 = LINE ( 'NONE', #58714, #8919 ) ;
#874 = FACE_OUTER_BOUND ( 'NONE', #50101, .T. ) ;
#875 = EDGE_CURVE ( 'NONE', #39002, #36881, #2684, .T. ) ;
#876 = ORIENTED_EDGE ( 'NONE', *, *, #60456, .T. ) ;
#877 = PRODUCT_DEFINITION_SHAPE ( 'NONE', 'NONE',  #74371 ) ;
#878 = AXIS2_PLACEMENT_3D ( 'NONE', #26295, #49228, #31195 ) ;
#879 = EDGE_CURVE ( 'NONE', #38728, #27488, #14836, .T. ) ;
#880 = ORIENTED_EDGE ( 'NONE', *, *, #55750, .F. ) ;
#881 = CARTESIAN_POINT ( 'NONE',  ( 96.32499999999998863, -212.2949673200287179, 80.76604166840097321 ) ) ;
#882 = ORIENTED_EDGE ( 'NONE', *, *, #12481, .F. ) ;
#883 = EDGE_CURVE ( 'NONE', #14710, #67113, #37603, .T. ) ;
#884 = ORIENTED_EDGE ( 'NONE', *, *, #13756, .T. ) ;
#885 = ORIENTED_EDGE ( 'NONE', *, *, #19699, .F. ) ;
#886 = CARTESIAN_POINT ( 'NONE',  ( 96.15314808468750130, -211.9973110713294489, 81.59947916753381492 ) ) ;
#887 = PRODUCT_CONTEXT ( 'NONE', #64237, 'mechanical' ) ;
#888 = CARTESIAN_POINT ( 'NONE',  ( 15.00000000000000000, -26.23277895567251505, -4.042438405569750870 ) ) ;
#889 = VECTOR ( 'NONE', #37456, 1000.000000000000000 ) ;
#890 = FACE_OUTER_BOUND ( 'NONE', #46338, .T. ) ;
#891 = CARTESIAN_POINT ( 'NONE',  ( 97.64999999999999147, 89.99999999755287661, 75.15687493081163950 ) ) ;
#892 = EDGE_CURVE ( 'NONE', #32115, #57513, #43257, .T. ) ;
#893 = CARTESIAN_POINT ( 'NONE',  ( -97.65000000000003411, -208.4700217866475214, 89.31208333333333371 ) ) ;
#894 = CARTESIAN_POINT ( 'NONE',  ( 0.000000000000000000, 0.000000000000000000, 21.00000000000000000 ) ) ;
#895 = CARTESIAN_POINT ( 'NONE',  ( 96.32499999999998863, -207.7050326799711968, 76.45333333333333314 ) ) ;
#896 = CARTESIAN_POINT ( 'NONE',  ( -97.30629616937497417, -211.3315407142195852, 85.88572916753382458 ) ) ;
#897 = VECTOR ( 'NONE', #23392, 1000.000000000000000 ) ;
#898 = CARTESIAN_POINT ( 'NONE',  ( -96.15314808468751551, 88.00268892867056536, 82.28739583420048120 ) ) ;
#899 = ORIENTED_EDGE ( 'NONE', *, *, #27993, .F. ) ;
#900 = CARTESIAN_POINT ( 'NONE',  ( 97.30629616937498838, 88.66845928578037217, 85.46239583420047836 ) ) ;
#901 = ORIENTED_EDGE ( 'NONE', *, *, #23587, .F. ) ;
#902 = CARTESIAN_POINT ( 'NONE',  ( 0.000000000000000000, -36.73666225445845157, -65.58780272294114866 ) ) ;
#903 = EDGE_CURVE ( 'NONE', #33655, #1337, #14284, .T. ) ;
#904 = DIRECTION ( 'NONE',  ( -1.000000000000000000, 0.000000000000000000, 0.000000000000000000 ) ) ;
#905 = CARTESIAN_POINT ( 'NONE',  ( 10.00000000000000000, 36.72794159290334903, -65.59268652807170952 ) ) ;
#906 = LINE ( 'NONE', #57272, #26039 ) ;
#907 = CARTESIAN_POINT ( 'NONE',  ( -94.99999999999997158, -212.6630814284392557, 85.35656250086714181 ) ) ;
#908 = CARTESIAN_POINT ( 'NONE',  ( 10.00000000000000000, -73.44644590900043113, -24.73286445877782924 ) ) ;
#909 = DIRECTION ( 'NONE',  ( -1.000000000000000000, 0.000000000000000000, -0.000000000000000000 ) ) ;
#910 = CARTESIAN_POINT ( 'NONE',  ( 10.00000000000000000, 0.000000000000000000, 0.000000000000000000 ) ) ;
#911 = CARTESIAN_POINT ( 'NONE',  ( 92.35000000000005116, 91.52997821335254969, 80.42208333333330472 ) ) ;
#912 = ORIENTED_EDGE ( 'NONE', *, *, #73582, .T. ) ;
#913 = VERTEX_POINT ( 'NONE', #15021 ) ;
#914 = CARTESIAN_POINT ( 'NONE',  ( -93.67500000000003979, 87.70503267997129626, 78.78166666666666629 ) ) ;
#915 = EDGE_CURVE ( 'NONE', #15157, #3606, #40196, .T. ) ;
#916 = CARTESIAN_POINT ( 'NONE',  ( 0.000000000000000000, -120.0000000000000000, -40.00000000000000711 ) ) ;
#917 = EDGE_CURVE ( 'NONE', #41826, #143, #63505, .T. ) ;
#918 = CARTESIAN_POINT ( 'NONE',  ( -97.30629616937501680, 91.33154071421968467, 87.68489583420047495 ) ) ;
#919 = CARTESIAN_POINT ( 'NONE',  ( 97.64999999999999147, -209.9999999999999716, 80.79249999999998977 ) ) ;
#920 = FACE_OUTER_BOUND ( 'NONE', #19157, .T. ) ;
#921 = APPLICATION_CONTEXT ( 'automotive_design' ) ;
#922 = CARTESIAN_POINT ( 'NONE',  ( 97.65000000000000568, -208.4700217866474645, 77.74979166840097378 ) ) ;
#923 = LINE ( 'NONE', #34721, #21582 ) ;
#924 = ORIENTED_EDGE ( 'NONE', *, *, #26109, .T. ) ;
#925 = CARTESIAN_POINT ( 'NONE',  ( -97.30629616937501680, 91.33154071421968467, 76.88989583420047325 ) ) ;
#926 = AXIS2_PLACEMENT_3D ( 'NONE', #39119, #66582, #26705 ) ;
#927 = CYLINDRICAL_SURFACE ( 'NONE', #15144, 12.49999999999999645 ) ;
#928 = FACE_OUTER_BOUND ( 'NONE', #18946, .T. ) ;
#929 = DIRECTION ( 'NONE',  ( 0.000000000000000000, 0.000000000000000000, 1.000000000000000000 ) ) ;
#930 = VECTOR ( 'NONE', #45166, 1000.000000000000000 ) ;
#931 = CARTESIAN_POINT ( 'NONE',  ( 10.00000000000000000, -51.02545421589363883, 55.20638768913742922 ) ) ;
#932 = DIRECTION ( 'NONE',  ( 0.000000000000000000, -0.07845909572785234043, 0.9969173337331274087 ) ) ;
#933 = CARTESIAN_POINT ( 'NONE',  ( -94.99999999999997158, -212.6630814284392557, 84.88031250086714863 ) ) ;
#934 = AXIS2_PLACEMENT_3D ( 'NONE', #72701, #48316, #9575 ) ;
#935 = CARTESIAN_POINT ( 'NONE',  ( 97.64999999946594755, -209.9999467985095976, 78.96687695417307395 ) ) ;
#936 = CARTESIAN_POINT ( 'NONE',  ( 92.69370383062498320, 90.00000000000002842, 76.46656250086715545 ) ) ;
#937 = CARTESIAN_POINT ( 'NONE',  ( -97.30629616937497417, -211.3315407142195852, 75.24947916753383481 ) ) ;
#938 = DIRECTION ( 'NONE',  ( -1.000000000000000000, 0.000000000000000000, -0.000000000000000000 ) ) ;
#939 = ORIENTED_EDGE ( 'NONE', *, *, #65612, .F. ) ;
#940 = DIRECTION ( 'NONE',  ( 0.000000000000000000, 0.9510565162951536422, 0.3090169943749471182 ) ) ;
#941 = CARTESIAN_POINT ( 'NONE',  ( 0.000000000000000000, -32.34446384429951138, -26.79245525562750530 ) ) ;
#942 = DIRECTION ( 'NONE',  ( -1.000000000000000000, -0.000000000000000000, 0.000000000000000000 ) ) ;
#943 = VECTOR ( 'NONE', #9608, 1000.000000000000000 ) ;
#944 = PLANE ( 'NONE',  #67284 ) ;
#945 = CARTESIAN_POINT ( 'NONE',  ( 97.30629616937498838, -211.3315407142195852, 77.20739583420046870 ) ) ;
#946 = ORIENTED_EDGE ( 'NONE', *, *, #71700, .T. ) ;
#947 = AXIS2_PLACEMENT_3D ( 'NONE', #33555, #73025, #5390 ) ;
#948 = EDGE_CURVE ( 'NONE', #66194, #44844, #36716, .T. ) ;
#949 = PLANE ( 'NONE',  #67943 ) ;
#950 = ORIENTED_EDGE ( 'NONE', *, *, #54751, .F. ) ;
#951 = DIRECTION ( 'NONE',  ( 1.000000000000000000, 0.000000000000000000, 0.000000000000000000 ) ) ;
#952 = ORIENTED_EDGE ( 'NONE', *, *, #36133, .T. ) ;
#953 = CARTESIAN_POINT ( 'NONE',  ( -92.35000000053409508, 90.00005320149026034, 78.96687695417308817 ) ) ;
#954 = EDGE_LOOP ( 'NONE', ( #39042, #25241, #27298, #50210 ) ) ;
#955 = ORIENTED_EDGE ( 'NONE', *, *, #71022, .T. ) ;
#956 = EDGE_CURVE ( 'NONE', #64091, #36317, #28160, .T. ) ;
#957 = ORIENTED_EDGE ( 'NONE', *, *, #41163, .T. ) ;
#958 = DIRECTION ( 'NONE',  ( -1.000000000000000000, -0.000000000000000000, 0.000000000000000000 ) ) ;
#959 = EDGE_CURVE ( 'NONE', #14859, #14793, #52027, .T. ) ;
#960 = ORIENTED_EDGE ( 'NONE', *, *, #66954, .T. ) ;
#961 = VERTEX_POINT ( 'NONE', #4894 ) ;
#962 =( BOUNDED_CURVE ( )  B_SPLINE_CURVE ( 2, ( #1157, #42080, #42445, #59365, #65383, #65016, #54102 ),
 .UNSPECIFIED., .F., .F. ) 
 B_SPLINE_CURVE_WITH_KNOTS ( ( 3, 2, 2, 3 ),
 ( 0.4583333333333335924, 0.4652777777777780122, 0.4722222222222224319, 0.4791666666666668517 ),
 .UNSPECIFIED. ) 
 CURVE ( )  GEOMETRIC_REPRESENTATION_ITEM ( )  RATIONAL_B_SPLINE_CURVE ( ( 0.9999999999999946709, 0.8660254037844440367, 1.000000000000000000, 0.8660254037844387076, 1.000000000000000000, 0.8660254037844354880, 1.000000000000003109 ) ) 
 REPRESENTATION_ITEM ( '' )  );
#963 = CARTESIAN_POINT ( 'NONE',  ( 94.99999999999998579, 92.66308142843935514, 83.29281250086717137 ) ) ;
#964 = DIRECTION ( 'NONE',  ( -1.000000000000000000, -0.000000000000000000, 0.000000000000000000 ) ) ;
#965 = CIRCLE ( 'NONE', #50170, 0.2999999999999981570 ) ;
#966 = CARTESIAN_POINT ( 'NONE',  ( 6.938893903907228378E-15, 0.000000000000000000, 0.000000000000000000 ) ) ;
#967 = AXIS2_PLACEMENT_3D ( 'NONE', #58203, #18343, #42767 ) ;
#968 = VERTEX_POINT ( 'NONE', #27411 ) ;
#969 = ADVANCED_FACE ( 'NONE', ( #55990 ), #68023, .T. ) ;
#970 = EDGE_LOOP ( 'NONE', ( #40059, #29578, #18197, #54354 ) ) ;
#971 = EDGE_CURVE ( 'NONE', #30219, #19199, #14467, .T. ) ;
#972 = ORIENTED_EDGE ( 'NONE', *, *, #22497, .F. ) ;
#973 = VERTEX_POINT ( 'NONE', #6001 ) ;
#974 = LINE ( 'NONE', #40408, #37100 ) ;
#975 = VERTEX_POINT ( 'NONE', #17260 ) ;
#976 = CARTESIAN_POINT ( 'NONE',  ( 0.000000000000000000, 0.000000000000000000, 0.000000000000000000 ) ) ;
#977 = CARTESIAN_POINT ( 'NONE',  ( -92.34999999999999432, -208.4700217866474645, 75.20979166840096752 ) ) ;
#978 = CIRCLE ( 'NONE', #22565, 82.00000000000000000 ) ;
#979 = CARTESIAN_POINT ( 'NONE',  ( 10.00000000000000000, -16.45098606841102651, -33.79645857604531045 ) ) ;
#980 = DIRECTION ( 'NONE',  ( 0.000000000000000000, 0.1045284632676570791, -0.9945218953682730678 ) ) ;
#981 = CARTESIAN_POINT ( 'NONE',  ( 92.35000000039364920, -209.9999706968037287, 82.45844277051352833 ) ) ;
#982 = CARTESIAN_POINT ( 'NONE',  ( -24.50849501662245800, -109.8101191361138831, -2.500000000000000444 ) ) ;
#983 = FACE_OUTER_BOUND ( 'NONE', #73941, .T. ) ;
#984 = ORIENTED_EDGE ( 'NONE', *, *, #20979, .T. ) ;
#985 = CARTESIAN_POINT ( 'NONE',  ( -93.67499999999998295, -207.7050326799711968, 77.80270833506763495 ) ) ;
#986 = VERTEX_POINT ( 'NONE', #10495 ) ;
#987 = CARTESIAN_POINT ( 'NONE',  ( 0.000000000000000000, -64.81221759200379040, 50.23322058963324110 ) ) ;
#988 = ORIENTED_EDGE ( 'NONE', *, *, #17612, .T. ) ;
#990 = CARTESIAN_POINT ( 'NONE',  ( -97.65000000000001990, 88.47002178664754979, 78.70229166840096013 ) ) ;
#989 = CARTESIAN_POINT ( 'NONE',  ( 92.34999999999999432, 91.52997821335252127, 79.86645833506761960 ) ) ;
#991 = VERTEX_POINT ( 'NONE', #21780 ) ;
#992 = CARTESIAN_POINT ( 'NONE',  ( 92.69370383062498320, 90.00000000000002842, 78.37156250086715659 ) ) ;
#993 = EDGE_CURVE ( 'NONE', #12738, #35320, #23278, .T. ) ;
#994 = CARTESIAN_POINT ( 'NONE',  ( 15.00000000000000000, -19.89357724625003598, -12.59942793731059041 ) ) ;
#995 = CARTESIAN_POINT ( 'NONE',  ( -92.35000000000003695, 89.99999997928479445, 80.87187500099602744 ) ) ;
#996 = CARTESIAN_POINT ( 'NONE',  ( 0.000000000000000000, 37.22597642581150268, 5.202137450157037435 ) ) ;
#997 = DIRECTION ( 'NONE',  ( 0.000000000000000000, 0.000000000000000000, 1.000000000000000000 ) ) ;
#998 = ORIENTED_EDGE ( 'NONE', *, *, #42050, .F. ) ;
#999 = CARTESIAN_POINT ( 'NONE',  ( 92.35000000000003695, -208.4700217866474929, 77.24708333333332178 ) ) ;
#1000 = CARTESIAN_POINT ( 'NONE',  ( 0.000000000000000000, 16.95692799528845640, -1.176623242955009039E-14 ) ) ;
#1001 = ORIENTED_EDGE ( 'NONE', *, *, #65099, .T. ) ;
#1002 = CIRCLE ( 'NONE', #15377, 32.00000000000000000 ) ;
#1003 = ORIENTED_EDGE ( 'NONE', *, *, #34297, .T. ) ;
#1004 = CIRCLE ( 'NONE', #67001, 42.00000000000000000 ) ;
#1005 = AXIS2_PLACEMENT_3D ( 'NONE', #19392, #42340, #53993 ) ;
#1006 = CIRCLE ( 'NONE', #63389, 31.99999999999999289 ) ;
#1007 = ADVANCED_FACE ( 'NONE', ( #69142 ), #17626, .T. ) ;
#1008 = DIRECTION ( 'NONE',  ( -0.000000000000000000, -0.000000000000000000, 1.000000000000000000 ) ) ;
#1009 = CARTESIAN_POINT ( 'NONE',  ( 5.000000000000002665, -2.543863470248944214, 81.96053171279901051 ) ) ;
#1010 = CARTESIAN_POINT ( 'NONE',  ( -93.84685191531247028, -211.9973110713294489, 77.94822916753382458 ) ) ;
#1011 = VECTOR ( 'NONE', #2786, 1000.000000000000000 ) ;
#1012 = ADVANCED_FACE ( 'NONE', ( #22160 ), #34862, .T. ) ;
#1013 = ORIENTED_EDGE ( 'NONE', *, *, #51838, .T. ) ;
#1014 = DIRECTION ( 'NONE',  ( -1.000000000000000000, 0.000000000000000000, -0.000000000000000000 ) ) ;
#1015 = DIRECTION ( 'NONE',  ( -1.000000000000000000, 0.000000000000000000, -0.000000000000000000 ) ) ;
#1016 = DIRECTION ( 'NONE',  ( 1.000000000000000000, 0.000000000000000000, 0.000000000000000000 ) ) ;
#1017 = CARTESIAN_POINT ( 'NONE',  ( 5.000000000000000000, -40.65526001592664329, 71.21200624218782593 ) ) ;
#1018 = DIRECTION ( 'NONE',  ( -0.000000000000000000, -0.000000000000000000, 1.000000000000000000 ) ) ;
#1019 = CARTESIAN_POINT ( 'NONE',  ( 10.00000000000000000, -8.830959090342926032, 74.65491531819115778 ) ) ;
#1020 = DIRECTION ( 'NONE',  ( -1.000000000000000000, 0.000000000000000000, 0.000000000000000000 ) ) ;
#1021 = CARTESIAN_POINT ( 'NONE',  ( 92.34999999999999432, 90.00000000000002842, 86.26937500173430351 ) ) ;
#1022 = CARTESIAN_POINT ( 'NONE',  ( 11.99999999999999822, -73.95703589263958122, -23.16143007188505010 ) ) ;
#1023 = DIRECTION ( 'NONE',  ( 0.000000000000000000, -1.000000000000000000, 0.000000000000000000 ) ) ;
#1024 = AXIS2_PLACEMENT_3D ( 'NONE', #8514, #65658, #64924 ) ;
#1025 = CARTESIAN_POINT ( 'NONE',  ( 92.69370383062498320, 88.66845928578035796, 87.94947916753382344 ) ) ;
#1026 = AXIS2_PLACEMENT_3D ( 'NONE', #3591, #2859, #37037 ) ;
#1027 = VECTOR ( 'NONE', #57764, 1000.000000000000000 ) ;
#1028 = CARTESIAN_POINT ( 'NONE',  ( -96.15314808468745866, -211.9973110713294489, 86.09739583420049769 ) ) ;
#1029 = CARTESIAN_POINT ( 'NONE',  ( 0.000000000000000000, 51.03279382321088065, 55.19960302592086521 ) ) ;
#1030 = ORIENTED_EDGE ( 'NONE', *, *, #64700, .F. ) ;
#1031 = CARTESIAN_POINT ( 'NONE',  ( -97.65000000000006253, 91.52997821335252127, 81.69208333333332916 ) ) ;
#1032 = CARTESIAN_POINT ( 'NONE',  ( -92.34999999999999432, -208.4700217866474645, 80.21041666666666003 ) ) ;
#1033 = CARTESIAN_POINT ( 'NONE',  ( -93.26027265873601380, 91.51405112163766375, 74.79348190356853365 ) ) ;
#1034 = AXIS2_PLACEMENT_3D ( 'NONE', #51639, #52754, #57661 ) ;
#1035 = AXIS2_PLACEMENT_3D ( 'NONE', #72622, #66281, #14754 ) ;
#1036 = CARTESIAN_POINT ( 'NONE',  ( 92.69370383062501162, -209.9999999999999716, 86.46781250086714010 ) ) ;
#1037 = EDGE_CURVE ( 'NONE', #26528, #55462, #37286, .T. ) ;
#1038 = VERTEX_POINT ( 'NONE', #45100 ) ;
#1039 = DIRECTION ( 'NONE',  ( -1.000000000000000000, 0.000000000000000000, -0.000000000000000000 ) ) ;
#1040 = ORIENTED_EDGE ( 'NONE', *, *, #39297, .F. ) ;
#1041 = DIRECTION ( 'NONE',  ( -0.000000000000000000, -0.000000000000000000, -1.000000000000000000 ) ) ;
#1042 = EDGE_CURVE ( 'NONE', #26594, #50602, #50718, .T. ) ;
#1043 = DIRECTION ( 'NONE',  ( -0.000000000000000000, -0.000000000000000000, 1.000000000000000000 ) ) ;
#1044 = CIRCLE ( 'NONE', #32217, 82.00000000000000000 ) ;
#1045 = AXIS2_PLACEMENT_3D ( 'NONE', #37846, #37482, #72037 ) ;
#1046 = ORIENTED_EDGE ( 'NONE', *, *, #53499, .F. ) ;
#1047 = EDGE_CURVE ( 'NONE', #70648, #50470, #62474, .T. ) ;
#1048 = ORIENTED_EDGE ( 'NONE', *, *, #56690, .T. ) ;
#1049 = VECTOR ( 'NONE', #6917, 1000.000000000000000 ) ;
#1050 = CIRCLE ( 'NONE', #17802, 42.00000000000000000 ) ;
#1051 = CARTESIAN_POINT ( 'NONE',  ( 97.30629616937498838, -208.6684592857803295, 80.64697916753382856 ) ) ;
#1052 = CARTESIAN_POINT ( 'NONE',  ( 0.000000000000000000, -11.30684508768395524, 76.66974797899831628 ) ) ;
#1053 = CYLINDRICAL_SURFACE ( 'NONE', #39955, 2.649999999999985700 ) ;
#1054 = COLOUR_RGB ( '', 0.66274510, 0.83137255, 0.94901961) ;
#1055 = CYLINDRICAL_SURFACE ( 'NONE', #60505, 31.99999999999998579 ) ;
#1056 = CARTESIAN_POINT ( 'NONE',  ( 0.000000000000000000, -59.03342792756297541, 46.54456581323783126 ) ) ;
#1057 = DIRECTION ( 'NONE',  ( 1.000000000000000000, 0.000000000000000000, 0.000000000000000000 ) ) ;
#1058 = CARTESIAN_POINT ( 'NONE',  ( 95.00000000000000000, -206.9400435732949575, 86.03125000000000000 ) ) ;
#1059 = ORIENTED_EDGE ( 'NONE', *, *, #39337, .F. ) ;
#1060 = EDGE_CURVE ( 'NONE', #59771, #48642, #39457, .T. ) ;
#1061 = VERTEX_POINT ( 'NONE', #5626 ) ;
#1062 = VERTEX_POINT ( 'NONE', #51465 ) ;
#1063 = ORIENTED_EDGE ( 'NONE', *, *, #64797, .T. ) ;
#1064 = CARTESIAN_POINT ( 'NONE',  ( -3.000000000000000000, -26.23277895567245821, -4.042438405570103477 ) ) ;
#1065 = FILL_AREA_STYLE_COLOUR ( '', #49528 ) ;
#1066 = CARTESIAN_POINT ( 'NONE',  ( -95.00000000000002842, 92.66308142843932671, 87.73781250086715033 ) ) ;
#1067 = CARTESIAN_POINT ( 'NONE',  ( 3.000000000000000000, 0.000000000000000000, 0.000000000000000000 ) ) ;
#1068 = DIRECTION ( 'NONE',  ( 0.000000000000000000, 0.000000000000000000, 1.000000000000000000 ) ) ;
#1069 = CARTESIAN_POINT ( 'NONE',  ( 93.67500000000001137, -207.7050326799711968, 74.73354166840096013 ) ) ;
#1070 = CARTESIAN_POINT ( 'NONE',  ( 96.32499999999998863, 87.70503267997126784, 77.51166666666665606 ) ) ;
#1071 = ORIENTED_EDGE ( 'NONE', *, *, #70363, .T. ) ;
#1072 = CARTESIAN_POINT ( 'NONE',  ( -97.64999999999994884, -211.5299782133524502, 88.22729166840096582 ) ) ;
#1073 = EDGE_LOOP ( 'NONE', ( #38003, #2560, #56508, #46336 ) ) ;
#1074 = CARTESIAN_POINT ( 'NONE',  ( -97.64999999999999147, -211.5299782133525071, 84.97291666666667709 ) ) ;
#1075 = ADVANCED_FACE ( 'NONE', ( #57486 ), #20, .T. ) ;
#1076 = VERTEX_POINT ( 'NONE', #53317 ) ;
#1077 = CARTESIAN_POINT ( 'NONE',  ( -95.00000000000002842, 86.94004357329504273, 88.33312500173428816 ) ) ;
#1078 = CARTESIAN_POINT ( 'NONE',  ( -93.84685191531254134, 91.99731107132950569, 82.60489583420049087 ) ) ;
#1079 = VECTOR ( 'NONE', #34029, 1000.000000000000000 ) ;
#1080 = CARTESIAN_POINT ( 'NONE',  ( 97.30629616937498838, 90.00000000000002842, 74.72031250086713783 ) ) ;
#1081 = EDGE_CURVE ( 'NONE', #58897, #8861, #49235, .T. ) ;
#1082 = EDGE_LOOP ( 'NONE', ( #30138, #24808, #4651, #72575 ) ) ;
#1083 = DIRECTION ( 'NONE',  ( -1.000000000000000000, -0.000000000000000000, 0.000000000000000000 ) ) ;
#1084 = AXIS2_PLACEMENT_3D ( 'NONE', #26024, #31296, #60267 ) ;
#1085 = CIRCLE ( 'NONE', #9393, 31.99999999999999289 ) ;
#1086 = DIRECTION ( 'NONE',  ( 0.000000000000000000, -0.000000000000000000, -1.000000000000000000 ) ) ;
#1087 = CARTESIAN_POINT ( 'NONE',  ( 22.08297821871651934, -111.8242998470044540, 5.500000000000000000 ) ) ;
#1088 = CARTESIAN_POINT ( 'NONE',  ( -97.64999999999996305, -209.9999999999999716, 86.26937500173430351 ) ) ;
#1089 = ORIENTED_EDGE ( 'NONE', *, *, #58225, .F. ) ;
#1090 = CARTESIAN_POINT ( 'NONE',  ( 6.719258119307965238, -15.35072898742050107, 0.000000000000000000 ) ) ;
#1091 = EDGE_CURVE ( 'NONE', #44704, #27953, #35640, .T. ) ;
#1092 = LINE ( 'NONE', #24349, #38349 ) ;
#1093 = VERTEX_POINT ( 'NONE', #17993 ) ;
#1094 = VERTEX_POINT ( 'NONE', #69858 ) ;
#1095 = VECTOR ( 'NONE', #67288, 1000.000000000000000 ) ;
#1096 = DIRECTION ( 'NONE',  ( 0.000000000000000000, 0.9723699203976756689, 0.2334453638559093047 ) ) ;
#1097 = VERTEX_POINT ( 'NONE', #7455 ) ;
#1098 = ADVANCED_FACE ( 'NONE', ( #64980 ), #24013, .T. ) ;
#1099 = CARTESIAN_POINT ( 'NONE',  ( -92.34999999999999432, -209.9999999999999716, 89.04749999999999943 ) ) ;
#1100 = DIRECTION ( 'NONE',  ( -1.000000000000000000, 0.000000000000000000, 0.000000000000000000 ) ) ;
#1101 = ORIENTED_EDGE ( 'NONE', *, *, #21972, .F. ) ;
#1102 = CARTESIAN_POINT ( 'NONE',  ( -93.84685191531248449, -208.0026889286704943, 87.04989583420048405 ) ) ;
#1103 = ORIENTED_EDGE ( 'NONE', *, *, #70883, .T. ) ;
#1104 = DIRECTION ( 'NONE',  ( 0.000000000000000000, 0.000000000000000000, 1.000000000000000000 ) ) ;
#1105 = CYLINDRICAL_SURFACE ( 'NONE', #41654, 37.49900000000000233 ) ;
#1106 = ORIENTED_EDGE ( 'NONE', *, *, #17167, .T. ) ;
#1107 = AXIS2_PLACEMENT_3D ( 'NONE', #20105, #19733, #37790 ) ;
#1108 = ORIENTED_EDGE ( 'NONE', *, *, #8076, .F. ) ;
#1109 = DIRECTION ( 'NONE',  ( -0.000000000000000000, -0.000000000000000000, -1.000000000000000000 ) ) ;
#1110 = CIRCLE ( 'NONE', #14248, 15.50000000000000000 ) ;
#1111 = PRESENTATION_STYLE_ASSIGNMENT (( #54051 ) ) ;
#1112 = CARTESIAN_POINT ( 'NONE',  ( 92.69370383062498320, 88.66845928578035796, 81.44072916753380298 ) ) ;
#1113 = LINE ( 'NONE', #11970, #36398 ) ;
#1114 = CARTESIAN_POINT ( 'NONE',  ( 8.000000000000007105, 1.142349898368116708E-14, 6.370018489481387452E-15 ) ) ;
#1115 = CARTESIAN_POINT ( 'NONE',  ( -96.32500000000001705, 92.29496732002878900, 85.44916666666665606 ) ) ;
#1116 = DIRECTION ( 'NONE',  ( 1.000000000000000000, -0.000000000000000000, -0.000000000000000000 ) ) ;
#1117 = DIRECTION ( 'NONE',  ( -1.000000000000000000, -0.000000000000000000, -0.000000000000000000 ) ) ;
#1118 = CARTESIAN_POINT ( 'NONE',  ( 4.999999999999999112, -2.663952781846440576, 41.91543099594817789 ) ) ;
#1119 = DIRECTION ( 'NONE',  ( 0.000000000000000000, 0.000000000000000000, 1.000000000000000000 ) ) ;
#1120 = CARTESIAN_POINT ( 'NONE',  ( 94.99999999999998579, 90.00000000000002842, 90.00000000000000000 ) ) ;
#1121 = DIRECTION ( 'NONE',  ( 0.000000000000000000, 0.000000000000000000, 1.000000000000000000 ) ) ;
#1122 = CARTESIAN_POINT ( 'NONE',  ( -92.69370383062505425, 91.33154071421968467, 88.10822916753380696 ) ) ;
#1123 = LINE ( 'NONE', #17998, #61089 ) ;
#1124 = AXIS2_PLACEMENT_3D ( 'NONE', #51978, #64384, #59114 ) ;
#1125 = CARTESIAN_POINT ( 'NONE',  ( 0.000000000000000000, -31.47745569255092235, -68.26794271651296242 ) ) ;
#1126 = VERTEX_POINT ( 'NONE', #23638 ) ;
#1128 = CARTESIAN_POINT ( 'NONE',  ( 0.000000000000000000, 37.16516213103277266, 4.992566952385114831 ) ) ;
#1127 = AXIS2_PLACEMENT_3D ( 'NONE', #39142, #38401, #33110 ) ;
#1129 = DIRECTION ( 'NONE',  ( 0.000000000000000000, 0.9238795325112851842, 0.3826834323650937786 ) ) ;
#1130 = CARTESIAN_POINT ( 'NONE',  ( 92.35000000046503033, 89.99996900126896548, 83.09538598081184091 ) ) ;
#1131 = AXIS2_PLACEMENT_3D ( 'NONE', #52664, #1217, #24110 ) ;
#1132 = ADVANCED_FACE ( 'NONE', ( #70214 ), #70959, .T. ) ;
#1133 = EDGE_CURVE ( 'NONE', #26842, #70819, #32431, .T. ) ;
#1134 = DIRECTION ( 'NONE',  ( 0.000000000000000000, 0.000000000000000000, 1.000000000000000000 ) ) ;
#1135 = CARTESIAN_POINT ( 'NONE',  ( 96.15314808468750130, -211.9973110713294489, 81.12322916753382174 ) ) ;
#1136 = AXIS2_PLACEMENT_3D ( 'NONE', #65708, #35636, #14189 ) ;
#1137 = EDGE_CURVE ( 'NONE', #25853, #74080, #3155, .T. ) ;
#1138 = ORIENTED_EDGE ( 'NONE', *, *, #48438, .T. ) ;
#1139 = ADVANCED_FACE ( 'NONE', ( #34923 ), #47315, .T. ) ;
#1140 = ORIENTED_EDGE ( 'NONE', *, *, #2156, .F. ) ;
#1141 = DIRECTION ( 'NONE',  ( -1.000000000000000000, 0.000000000000000000, 0.000000000000000000 ) ) ;
#1142 = VERTEX_POINT ( 'NONE', #18355 ) ;
#1143 = CARTESIAN_POINT ( 'NONE',  ( 95.00000000000000000, -206.9400435732949575, 88.57124999999999204 ) ) ;
#1144 = EDGE_CURVE ( 'NONE', #34884, #21495, #31203, .T. ) ;
#1145 = LINE ( 'NONE', #24398, #36387 ) ;
#1146 = ORIENTED_EDGE ( 'NONE', *, *, #73833, .F. ) ;
#1147 = CARTESIAN_POINT ( 'NONE',  ( 95.00000000000000000, -207.3369185715606307, 80.75281250086715090 ) ) ;
#1148 = AXIS2_PLACEMENT_3D ( 'NONE', #69760, #16793, #69391 ) ;
#1149 = CIRCLE ( 'NONE', #29913, 16.00000000000000000 ) ;
#1150 = ORIENTED_EDGE ( 'NONE', *, *, #57635, .F. ) ;
#1151 = CARTESIAN_POINT ( 'NONE',  ( 97.64999999999999147, 89.99999990163419739, 80.23687499810812085 ) ) ;
#1152 = ORIENTED_EDGE ( 'NONE', *, *, #27406, .T. ) ;
#1153 = ORIENTED_EDGE ( 'NONE', *, *, #63592, .T. ) ;
#1154 = CARTESIAN_POINT ( 'NONE',  ( 0.000000000000000000, 37.58145647212455032, -0.6853352020786441789 ) ) ;
#1155 = AXIS2_PLACEMENT_3D ( 'NONE', #13195, #24128, #69961 ) ;
#1156 = VECTOR ( 'NONE', #16470, 1000.000000000000000 ) ;
#1157 = CARTESIAN_POINT ( 'NONE',  ( -97.65000000000001990, 90.00000000000004263, 83.01499999999998636 ) ) ;
#1158 = AXIS2_PLACEMENT_3D ( 'NONE', #11271, #69884, #51869 ) ;
#1159 = VERTEX_POINT ( 'NONE', #63877 ) ;
#1160 = FACE_OUTER_BOUND ( 'NONE', #45975, .T. ) ;
#1161 = CARTESIAN_POINT ( 'NONE',  ( 92.35000000000000853, -209.9999999999999716, 86.26937500173430351 ) ) ;
#1163 = CIRCLE ( 'NONE', #17913, 42.00000000000000000 ) ;
#1162 = CARTESIAN_POINT ( 'NONE',  ( 94.99999999999998579, 86.94004357329500010, 87.61875000000000568 ) ) ;
#1164 = EDGE_LOOP ( 'NONE', ( #66927, #73159, #62142, #19064 ) ) ;
#1165 = CARTESIAN_POINT ( 'NONE',  ( 92.35001072950491618, 91.52998440803509084, 84.94645790656223028 ) ) ;
#1166 = VERTEX_POINT ( 'NONE', #7082 ) ;
#1167 = VECTOR ( 'NONE', #67110, 1000.000000000000000 ) ;
#1168 = ORIENTED_EDGE ( 'NONE', *, *, #43119, .T. ) ;
#1169 = CARTESIAN_POINT ( 'NONE',  ( -97.30629616937501680, 90.00000000000004263, 89.80156250086714920 ) ) ;
#1170 = VERTEX_POINT ( 'NONE', #30001 ) ;
#1171 = CARTESIAN_POINT ( 'NONE',  ( 97.64999999999997726, 88.47002178664753558, 86.53395833506763779 ) ) ;
#1172 = ORIENTED_EDGE ( 'NONE', *, *, #5947, .F. ) ;
#1173 = VERTEX_POINT ( 'NONE', #12346 ) ;
#1174 = CARTESIAN_POINT ( 'NONE',  ( 15.00000000000000000, 0.000000000000000000, 0.000000000000000000 ) ) ;
#1175 = EDGE_CURVE ( 'NONE', #61985, #23343, #58965, .T. ) ;
#1176 = EDGE_CURVE ( 'NONE', #54538, #68921, #7226, .T. ) ;
#1177 = DIRECTION ( 'NONE',  ( -1.000000000000000000, 0.000000000000000000, -0.000000000000000000 ) ) ;
#1178 = ORIENTED_EDGE ( 'NONE', *, *, #31971, .T. ) ;
#1179 = ORIENTED_EDGE ( 'NONE', *, *, #14136, .T. ) ;
#1180 = EDGE_LOOP ( 'NONE', ( #3896, #18215, #17497, #47321 ) ) ;
#1181 = DIRECTION ( 'NONE',  ( -1.000000000000000000, 0.000000000000000000, -0.000000000000000000 ) ) ;
#1182 = DIRECTION ( 'NONE',  ( -1.000000000000000000, -0.000000000000000000, -0.000000000000000000 ) ) ;
#1183 = CARTESIAN_POINT ( 'NONE',  ( -92.35000000000005116, 88.47002178664754979, 88.35958333333333314 ) ) ;
#1184 = EDGE_LOOP ( 'NONE', ( #11101, #10539, #73075, #4642 ) ) ;
#1185 = ADVANCED_FACE ( 'NONE', ( #52568 ), #1489, .F. ) ;
#1186 = CARTESIAN_POINT ( 'NONE',  ( -10.00000000000000000, 0.000000000000000000, 0.000000000000000000 ) ) ;
#1187 =( BOUNDED_CURVE ( )  B_SPLINE_CURVE ( 2, ( #53628, #31794, #37083, #54740, #54373, #2170, #25056 ),
 .UNSPECIFIED., .F., .F. ) 
 B_SPLINE_CURVE_WITH_KNOTS ( ( 3, 2, 2, 3 ),
 ( 0.1905056698846566698, 0.1975614351456765616, 0.2046172006865936144, 0.2116728463017078510 ),
 .UNSPECIFIED. ) 
 CURVE ( )  GEOMETRIC_REPRESENTATION_ITEM ( )  RATIONAL_B_SPLINE_CURVE ( ( 1.000000000000000000, 0.8660254037844387076, 1.000000000000000000, 0.8660254037844387076, 1.000000000000000000, 0.8660276809308252721, 0.9999954457846356171 ) ) 
 REPRESENTATION_ITEM ( '' )  );
#1188 = DIRECTION ( 'NONE',  ( 0.000000000000000000, 0.000000000000000000, 1.000000000000000000 ) ) ;
#1189 = ORIENTED_EDGE ( 'NONE', *, *, #14589, .F. ) ;
#1190 = CARTESIAN_POINT ( 'NONE',  ( 10.00000000000000000, 63.18004540533029001, 44.88180994100400767 ) ) ;
#1191 = CARTESIAN_POINT ( 'NONE',  ( -97.30629616937497417, -208.6684592857803011, 82.60489583420047666 ) ) ;
#1192 = VERTEX_POINT ( 'NONE', #59329 ) ;
#1193 = AXIS2_PLACEMENT_3D ( 'NONE', #174, #70007, #57649 ) ;
#1194 = CARTESIAN_POINT ( 'NONE',  ( 11.99999999999999822, 72.35432306680485226, -20.40083707022909110 ) ) ;
#1195 = CARTESIAN_POINT ( 'NONE',  ( 93.74200686866063847, -212.2877248121147034, 74.97309184317512631 ) ) ;
#1196 = CARTESIAN_POINT ( 'NONE',  ( 10.00000000000000000, -36.13751322684434797, 21.40280677340358295 ) ) ;
#1197 = CARTESIAN_POINT ( 'NONE',  ( -92.69370383062498320, -211.3315407142195852, 77.84239583420047381 ) ) ;
#1198 = AXIS2_PLACEMENT_3D ( 'NONE', #56876, #45224, #10253 ) ;
#1199 = VECTOR ( 'NONE', #23641, 1000.000000000000000 ) ;
#1200 = VECTOR ( 'NONE', #13246, 1000.000000000000000 ) ;
#1201 = DIRECTION ( 'NONE',  ( 0.000000000000000000, 0.000000000000000000, 1.000000000000000000 ) ) ;
#1202 = DIRECTION ( 'NONE',  ( -1.000000000000000000, 0.000000000000000000, 0.000000000000000000 ) ) ;
#1204 = CIRCLE ( 'NONE', #3594, 16.00000000000000000 ) ;
#1203 = DIRECTION ( 'NONE',  ( -1.000000000000000000, -0.000000000000000000, -0.000000000000000000 ) ) ;
#1205 = CARTESIAN_POINT ( 'NONE',  ( 11.99999999999999822, 0.000000000000000000, 0.000000000000000000 ) ) ;
#1206 = CARTESIAN_POINT ( 'NONE',  ( -9.937067298023309903, 7.583184918921312523, 52.00000000000002132 ) ) ;
#1207 = CARTESIAN_POINT ( 'NONE',  ( -95.00000000000002842, 87.33691857156074434, 77.10156250086711793 ) ) ;
#1208 = DIRECTION ( 'NONE',  ( 0.000000000000000000, 0.000000000000000000, 1.000000000000000000 ) ) ;
#1209 = PLANE ( 'NONE',  #42259 ) ;
#1210 = ORIENTED_EDGE ( 'NONE', *, *, #37944, .T. ) ;
#1211 = DIRECTION ( 'NONE',  ( -1.000000000000000000, 0.000000000000000000, -0.000000000000000000 ) ) ;
#1212 = VECTOR ( 'NONE', #3746, 1000.000000000000000 ) ;
#1213 = CARTESIAN_POINT ( 'NONE',  ( 97.65000000000000568, -208.4700217866474645, 89.17979166840096639 ) ) ;
#1215 = FACE_OUTER_BOUND ( 'NONE', #8701, .T. ) ;
#1214 = AXIS2_PLACEMENT_3D ( 'NONE', #42287, #30244, #59569 ) ;
#1216 = CIRCLE ( 'NONE', #54036, 82.00000000000000000 ) ;
#1217 = DIRECTION ( 'NONE',  ( -0.000000000000000000, -0.000000000000000000, 1.000000000000000000 ) ) ;
#1218 = CARTESIAN_POINT ( 'NONE',  ( 12.83284365640956182, 1.604257322819167057E-15, 0.000000000000000000 ) ) ;
#1219 = CARTESIAN_POINT ( 'NONE',  ( 13.83832728059186046, -142.6495187161941089, 5.500000000000000000 ) ) ;
#1220 = CARTESIAN_POINT ( 'NONE',  ( -97.30629616937495996, -209.9999999999999716, 77.10156250086714635 ) ) ;
#1221 = AXIS2_PLACEMENT_3D ( 'NONE', #72653, #50483, #50850 ) ;
#1222 = CIRCLE ( 'NONE', #10785, 77.49899999999999523 ) ;
#1223 = DIRECTION ( 'NONE',  ( 1.000000000000000000, 0.000000000000000000, -0.000000000000000000 ) ) ;
#1224 = ORIENTED_EDGE ( 'NONE', *, *, #42313, .F. ) ;
#1225 = DIRECTION ( 'NONE',  ( 0.000000000000000000, 0.000000000000000000, 1.000000000000000000 ) ) ;
#1226 = LINE ( 'NONE', #70684, #62292 ) ;
#1227 = CARTESIAN_POINT ( 'NONE',  ( -97.65000000000001990, 90.00000000000004263, 90.00000000000000000 ) ) ;
#1228 = FACE_OUTER_BOUND ( 'NONE', #28220, .T. ) ;
#1229 = ADVANCED_FACE ( 'NONE', ( #7820 ), #30737, .T. ) ;
#1230 = DIRECTION ( 'NONE',  ( 0.000000000000000000, 0.000000000000000000, 1.000000000000000000 ) ) ;
#1231 = ORIENTED_EDGE ( 'NONE', *, *, #64365, .F. ) ;
#1232 = ADVANCED_FACE ( 'NONE', ( #2956 ), #31484, .T. ) ;
#1233 = DIRECTION ( 'NONE',  ( 0.000000000000000000, -0.8090169943749401238, -0.5877852522924831291 ) ) ;
#1234 = EDGE_LOOP ( 'NONE', ( #47291, #63723 ) ) ;
#1235 = EDGE_CURVE ( 'NONE', #19038, #52874, #22855, .T. ) ;
#1236 = AXIS2_PLACEMENT_3D ( 'NONE', #49211, #20650, #30670 ) ;
#1237 = CARTESIAN_POINT ( 'NONE',  ( 93.84685191531249870, -208.0026889286704943, 86.36197916753381776 ) ) ;
#1238 = CARTESIAN_POINT ( 'NONE',  ( -92.35000000010064980, -209.9999769027738239, 83.41187580057901130 ) ) ;
#1239 = ORIENTED_EDGE ( 'NONE', *, *, #62083, .F. ) ;
#1240 = CARTESIAN_POINT ( 'NONE',  ( -92.35000000000005116, 91.52997821335253548, 79.57541666666666913 ) ) ;
#1241 = AXIS2_PLACEMENT_3D ( 'NONE', #63682, #1665, #13266 ) ;
#1242 = ORIENTED_EDGE ( 'NONE', *, *, #57164, .F. ) ;
#1243 = DIRECTION ( 'NONE',  ( 0.000000000000000000, 0.000000000000000000, 1.000000000000000000 ) ) ;
#1244 = VERTEX_POINT ( 'NONE', #49151 ) ;
#1245 = CARTESIAN_POINT ( 'NONE',  ( -97.30629616937501680, 88.66845928578038638, 80.96447916753382401 ) ) ;
#1246 = VERTEX_POINT ( 'NONE', #31110 ) ;
#1247 = ORIENTED_EDGE ( 'NONE', *, *, #5534, .T. ) ;
#1248 = CIRCLE ( 'NONE', #19220, 31.99999999999999645 ) ;
#1249 = DIRECTION ( 'NONE',  ( 0.000000000000000000, -0.07845909572783058006, -0.9969173337331290741 ) ) ;
#1250 = ORIENTED_EDGE ( 'NONE', *, *, #69986, .F. ) ;
#1251 = DIRECTION ( 'NONE',  ( -1.000000000000000000, -0.000000000000000000, -0.000000000000000000 ) ) ;
#1252 = DIRECTION ( 'NONE',  ( -0.000000000000000000, -0.000000000000000000, 1.000000000000000000 ) ) ;
#1253 = EDGE_CURVE ( 'NONE', #62521, #29721, #66451, .T. ) ;
#1254 = EDGE_CURVE ( 'NONE', #32004, #20003, #26430, .T. ) ;
#1255 = VERTEX_POINT ( 'NONE', #66093 ) ;
#1256 = DIRECTION ( 'NONE',  ( 0.000000000000000000, 0.3090169943749412895, 0.9510565162951556406 ) ) ;
#1257 = VERTEX_POINT ( 'NONE', #14939 ) ;
#1258 = DIRECTION ( 'NONE',  ( -1.000000000000000000, -0.000000000000000000, 0.000000000000000000 ) ) ;
#1259 = ORIENTED_EDGE ( 'NONE', *, *, #39645, .F. ) ;
#1260 = CIRCLE ( 'NONE', #20423, 31.99999999999998579 ) ;
#1261 = EDGE_LOOP ( 'NONE', ( #9691, #58194, #22600, #52420 ) ) ;
#1262 = VERTEX_POINT ( 'NONE', #37880 ) ;
#1263 = CARTESIAN_POINT ( 'NONE',  ( 93.84685191531251292, -211.9973110713294489, 82.76364583420047438 ) ) ;
#1264 = AXIS2_PLACEMENT_3D ( 'NONE', #61042, #50496, #16287 ) ;
#1265 = ADVANCED_FACE ( 'NONE', ( #71698 ), #68476, .F. ) ;
#1266 = EDGE_CURVE ( 'NONE', #63423, #62521, #21300, .T. ) ;
#1267 = AXIS2_PLACEMENT_3D ( 'NONE', #4310, #67439, #33213 ) ;
#1268 = SHAPE_DEFINITION_REPRESENTATION ( #56642, #36835 ) ;
#1269 = DIRECTION ( 'NONE',  ( -0.000000000000000000, -0.000000000000000000, 1.000000000000000000 ) ) ;
#1270 = CARTESIAN_POINT ( 'NONE',  ( -10.00000000000000000, 0.000000000000000000, 0.000000000000000000 ) ) ;
#1271 = CARTESIAN_POINT ( 'NONE',  ( 92.35000000000000853, -209.9999999999999716, 79.20499999999999829 ) ) ;
#1272 = CARTESIAN_POINT ( 'NONE',  ( -97.64999999999996305, -209.9999999999999716, 89.36499999999999488 ) ) ;
#1273 = LINE ( 'NONE', #62545, #61221 ) ;
#1274 = VECTOR ( 'NONE', #31612, 1000.000000000000000 ) ;
#1275 = CARTESIAN_POINT ( 'NONE',  ( -16.07206065793331007, -141.0698568150738197, -2.500000000000000000 ) ) ;
#1276 = CONICAL_SURFACE ( 'NONE', #8416, 15.39727592608509177, 1.361356816555577609 ) ;
#1277 = CARTESIAN_POINT ( 'NONE',  ( -97.30629616937495996, -209.9999999999999716, 85.83281250086714920 ) ) ;
#1278 = CARTESIAN_POINT ( 'NONE',  ( -92.69370383062504004, 90.00000000000004263, 81.22906250086715829 ) ) ;
#1279 = ORIENTED_EDGE ( 'NONE', *, *, #2361, .T. ) ;
#1280 = CARTESIAN_POINT ( 'NONE',  ( 93.84685191531248449, 91.99731107132950569, 82.55197916753380127 ) ) ;
#1281 = VERTEX_POINT ( 'NONE', #37144 ) ;
#1282 = CARTESIAN_POINT ( 'NONE',  ( -95.00000000000002842, 86.94004357329504273, 78.80812500173429669 ) ) ;
#1283 = CARTESIAN_POINT ( 'NONE',  ( 15.00000000000000000, -13.04903810567675393, -19.60159698893424718 ) ) ;
#1284 = CARTESIAN_POINT ( 'NONE',  ( 0.000000000000000000, 22.90783923731629912, 78.73519480814962890 ) ) ;
#1285 = DIRECTION ( 'NONE',  ( 0.000000000000000000, -0.9238795325112821866, -0.3826834323651008285 ) ) ;
#1286 = CARTESIAN_POINT ( 'NONE',  ( -5.000000000000000000, 2.419979747126332903, -5.688163366729713566 ) ) ;
#1287 = CARTESIAN_POINT ( 'NONE',  ( -92.69370383062498320, -211.3315407142195852, 88.00239583420047040 ) ) ;
#1288 = CARTESIAN_POINT ( 'NONE',  ( 5.000000000000000000, -64.81221759200379040, 50.23322058963324110 ) ) ;
#1289 = DIRECTION ( 'NONE',  ( -1.000000000000000000, -0.000000000000000000, -0.000000000000000000 ) ) ;
#1290 = CYLINDRICAL_SURFACE ( 'NONE', #1954, 12.49999999999999645 ) ;
#1291 = VECTOR ( 'NONE', #65356, 1000.000000000000000 ) ;
#1292 = DIRECTION ( 'NONE',  ( 0.000000000000000000, 0.5224985647159500202, -0.8526401643540915121 ) ) ;
#1293 = ORIENTED_EDGE ( 'NONE', *, *, #14537, .T. ) ;
#1294 = ORIENTED_EDGE ( 'NONE', *, *, #18339, .T. ) ;
#1295 = CARTESIAN_POINT ( 'NONE',  ( -97.65000000000001990, 88.47002178664754979, 78.62291666666668277 ) ) ;
#1296 = DIRECTION ( 'NONE',  ( -0.4279312458753000703, -0.9038112904824842087, 0.000000000000000000 ) ) ;
#1297 = CARTESIAN_POINT ( 'NONE',  ( -97.30629616937501680, 90.00000000000004263, 89.00781250086714635 ) ) ;
#1298 = CARTESIAN_POINT ( 'NONE',  ( 0.000000000000000000, 33.71516098798849015, -74.74816331893393340 ) ) ;
#1299 = CARTESIAN_POINT ( 'NONE',  ( 92.34999999999999432, 90.00000000000002842, 76.66499999999999204 ) ) ;
#1300 = CARTESIAN_POINT ( 'NONE',  ( 0.000000000000000000, -71.27951684758046724, 30.41916302227088309 ) ) ;
#1301 = CARTESIAN_POINT ( 'NONE',  ( 11.99999999999999822, 51.03279382321166224, -55.19960302592011914 ) ) ;
#1302 = ORIENTED_EDGE ( 'NONE', *, *, #61731, .T. ) ;
#1303 = FACE_OUTER_BOUND ( 'NONE', #33672, .T. ) ;
#1304 = DIRECTION ( 'NONE',  ( 0.000000000000000000, 0.000000000000000000, 1.000000000000000000 ) ) ;
#1305 = CYLINDRICAL_SURFACE ( 'NONE', #51389, 31.99999999999998579 ) ;
#1306 = DIRECTION ( 'NONE',  ( -1.000000000000000000, 0.000000000000000000, -0.000000000000000000 ) ) ;
#1307 = CARTESIAN_POINT ( 'NONE',  ( -97.64999999999996305, -209.9999999999999716, 90.00000000000000000 ) ) ;
#1308 = CIRCLE ( 'NONE', #26476, 31.99999999999998934 ) ;
#1309 = CARTESIAN_POINT ( 'NONE',  ( 11.99999999999999822, -40.65526001592564853, -71.21200624218839437 ) ) ;
#1310 = CARTESIAN_POINT ( 'NONE',  ( -94.99999999999997158, -212.6630814284392557, 87.42031250086715488 ) ) ;
#1311 =( LENGTH_UNIT ( ) NAMED_UNIT ( * ) SI_UNIT ( .MILLI., .METRE. ) );
#1312 = EDGE_CURVE ( 'NONE', #51311, #11086, #32593, .T. ) ;
#1313 = CYLINDRICAL_SURFACE ( 'NONE', #10823, 31.99999999999998579 ) ;
#1314 = ADVANCED_FACE ( 'NONE', ( #54791 ), #3687, .T. ) ;
#1315 = DIRECTION ( 'NONE',  ( -1.000000000000000000, -0.000000000000000000, -0.000000000000000000 ) ) ;
#1316 = EDGE_CURVE ( 'NONE', #57811, #52268, #8931, .T. ) ;
#1317 = CARTESIAN_POINT ( 'NONE',  ( -96.15314808468745866, -211.9973110713294489, 75.30239583420048177 ) ) ;
#1318 = DIRECTION ( 'NONE',  ( 0.000000000000000000, 0.000000000000000000, 1.000000000000000000 ) ) ;
#1319 = AXIS2_PLACEMENT_3D ( 'NONE', #14732, #21472, #56073 ) ;
#1320 = EDGE_LOOP ( 'NONE', ( #66595, #15736, #2918, #49929 ) ) ;
#1321 = CARTESIAN_POINT ( 'NONE',  ( 0.000000000000000000, -27.13269053701114331, 25.88420570971391754 ) ) ;
#1322 = DIRECTION ( 'NONE',  ( -1.000000000000000000, 0.000000000000000000, 0.000000000000000000 ) ) ;
#1323 = CARTESIAN_POINT ( 'NONE',  ( 0.000000000000000000, 30.00120703465205452, 22.64427369931179967 ) ) ;
#1324 = CIRCLE ( 'NONE', #39714, 15.99999999999999822 ) ;
#1325 = EDGE_CURVE ( 'NONE', #15992, #50254, #26586, .T. ) ;
#1326 = AXIS2_PLACEMENT_3D ( 'NONE', #48969, #48614, #71528 ) ;
#1327 = CARTESIAN_POINT ( 'NONE',  ( -92.69370383062504004, 90.00000000000004263, 75.51406250086715488 ) ) ;
#1328 = CARTESIAN_POINT ( 'NONE',  ( 95.00000000000000000, -212.6630814284392557, 76.46656250086712703 ) ) ;
#1329 = ORIENTED_EDGE ( 'NONE', *, *, #18478, .F. ) ;
#1330 = EDGE_CURVE ( 'NONE', #9413, #14702, #54034, .T. ) ;
#1331 = DIRECTION ( 'NONE',  ( -1.000000000000000000, 0.000000000000000000, -0.000000000000000000 ) ) ;
#1332 = ORIENTED_EDGE ( 'NONE', *, *, #14740, .T. ) ;
#1333 = EDGE_CURVE ( 'NONE', #6700, #65764, #21417, .T. ) ;
#1334 = CARTESIAN_POINT ( 'NONE',  ( 0.000000000000000000, 26.02418014898310261, 70.52718814184268581 ) ) ;
#1335 = ORIENTED_EDGE ( 'NONE', *, *, #11023, .T. ) ;
#1336 = CARTESIAN_POINT ( 'NONE',  ( 0.000000000000000000, -72.35432306680498016, 20.40083707022857951 ) ) ;
#1337 = VERTEX_POINT ( 'NONE', #25480 ) ;
#1338 = ORIENTED_EDGE ( 'NONE', *, *, #32822, .T. ) ;
#1339 = EDGE_LOOP ( 'NONE', ( #20708, #25966, #12886, #8431 ) ) ;
#1340 = LINE ( 'NONE', #12563, #61150 ) ;
#1341 = EDGE_CURVE ( 'NONE', #59461, #44099, #3318, .T. ) ;
#1342 = EDGE_CURVE ( 'NONE', #44951, #8568, #15304, .T. ) ;
#1343 = EDGE_LOOP ( 'NONE', ( #50298, #67195, #1354, #42780 ) ) ;
#1344 = ORIENTED_EDGE ( 'NONE', *, *, #2745, .F. ) ;
#1345 = CARTESIAN_POINT ( 'NONE',  ( 92.69370383062498320, 91.33154071421968467, 84.66864583420047552 ) ) ;
#1346 = DIRECTION ( 'NONE',  ( -1.000000000000000000, -0.000000000000000000, -0.000000000000000000 ) ) ;
#1347 = CARTESIAN_POINT ( 'NONE',  ( 97.64999999999997726, -211.5299782133524502, 76.29458333333333542 ) ) ;
#1348 = EDGE_LOOP ( 'NONE', ( #12482, #25821, #42433, #73861 ) ) ;
#1349 = ORIENTED_EDGE ( 'NONE', *, *, #68241, .T. ) ;
#1350 = CIRCLE ( 'NONE', #16923, 3.299999999999997158 ) ;
#1351 = VERTEX_POINT ( 'NONE', #8565 ) ;
#1352 = CYLINDRICAL_SURFACE ( 'NONE', #10629, 16.00000000000000000 ) ;
#1353 = CIRCLE ( 'NONE', #7319, 82.00000000000000000 ) ;
#1354 = ORIENTED_EDGE ( 'NONE', *, *, #44246, .T. ) ;
#1355 = CARTESIAN_POINT ( 'NONE',  ( -8.944667923005411581E-16, -120.0000000000000142, -55.00000000000000711 ) ) ;
#1356 = CARTESIAN_POINT ( 'NONE',  ( -97.64999999999996305, -210.0000123297513142, 75.47437542817786493 ) ) ;
#1357 = DIRECTION ( 'NONE',  ( -1.000000000000000000, 0.000000000000000000, 0.000000000000000000 ) ) ;
#1358 = CARTESIAN_POINT ( 'NONE',  ( -10.90473778262209414, 0.000000000000000000, 0.000000000000000000 ) ) ;
#1359 = DIRECTION ( 'NONE',  ( 0.000000000000000000, 0.000000000000000000, -1.000000000000000000 ) ) ;
#1360 = CYLINDRICAL_SURFACE ( 'NONE', #49182, 2.649999999999985700 ) ;
#1361 = DIRECTION ( 'NONE',  ( 0.000000000000000000, -0.9876883405951361050, -0.1564344650402419989 ) ) ;
#1362 = CARTESIAN_POINT ( 'NONE',  ( -92.34999999999999432, -208.4700217866474645, 80.28979166840098003 ) ) ;
#1363 = ORIENTED_EDGE ( 'NONE', *, *, #47890, .T. ) ;
#1364 = PLANE ( 'NONE',  #1524 ) ;
#1365 = VERTEX_POINT ( 'NONE', #26209 ) ;
#1367 = CARTESIAN_POINT ( 'NONE',  ( -97.65000000000001990, 88.47002178664754979, 75.52729166840099140 ) ) ;
#1366 = CARTESIAN_POINT ( 'NONE',  ( 96.32499999999998863, 87.70503267997126784, 80.13104166840095388 ) ) ;
#1368 = ORIENTED_EDGE ( 'NONE', *, *, #26702, .T. ) ;
#1369 = CARTESIAN_POINT ( 'NONE',  ( 92.69370383062498320, 90.00000000000002842, 80.27656250086714351 ) ) ;
#1370 = CARTESIAN_POINT ( 'NONE',  ( 10.00000000000000000, 0.000000000000000000, 0.000000000000000000 ) ) ;
#1371 = CARTESIAN_POINT ( 'NONE',  ( 0.000000000000000000, -120.0000000000000000, 2.500000000000000000 ) ) ;
#1372 = CARTESIAN_POINT ( 'NONE',  ( -7.572224309238338336, -145.4393675041377492, -2.500000000000000444 ) ) ;
#1373 = AXIS2_PLACEMENT_3D ( 'NONE', #24818, #13162, #19174 ) ;
#1374 = FACE_OUTER_BOUND ( 'NONE', #64661, .T. ) ;
#1375 = VERTEX_POINT ( 'NONE', #43538 ) ;
#1376 = DIRECTION ( 'NONE',  ( 0.000000000000000000, 0.000000000000000000, 1.000000000000000000 ) ) ;
#1377 = VECTOR ( 'NONE', #14068, 1000.000000000000000 ) ;
#1378 = DIRECTION ( 'NONE',  ( 1.000000000000000000, -0.000000000000000000, 0.000000000000000000 ) ) ;
#1379 = ORIENTED_EDGE ( 'NONE', *, *, #46496, .F. ) ;
#1380 = VECTOR ( 'NONE', #34980, 1000.000000000000000 ) ;
#1381 = ORIENTED_EDGE ( 'NONE', *, *, #5276, .T. ) ;
#1382 = AXIS2_PLACEMENT_3D ( 'NONE', #31665, #27412, #42591 ) ;
#1383 = CYLINDRICAL_SURFACE ( 'NONE', #67856, 2.649999999999999467 ) ;
#1384 = CARTESIAN_POINT ( 'NONE',  ( -6.170112525937322623, 10.87104923258428180, 125.0000000000000000 ) ) ;
#1385 = CARTESIAN_POINT ( 'NONE',  ( -97.30629616937495996, -209.9999999999999716, 78.37156250086715659 ) ) ;
#1386 = VERTEX_POINT ( 'NONE', #54421 ) ;
#1387 = EDGE_CURVE ( 'NONE', #52407, #28756, #61183, .T. ) ;
#1388 = DIRECTION ( 'NONE',  ( -1.000000000000000000, 7.955419762439749020E-15, 2.563413034563919251E-14 ) ) ;
#1389 = CARTESIAN_POINT ( 'NONE',  ( -94.99999999999997158, -209.9999999999999716, 90.00000000000000000 ) ) ;
#1390 = CARTESIAN_POINT ( 'NONE',  ( -92.34999999999999432, -209.9999999999999716, 90.00000000000000000 ) ) ;
#1391 = CARTESIAN_POINT ( 'NONE',  ( 10.00000000000000000, 37.01155633439068282, -6.555932627142014191 ) ) ;
#1392 = CARTESIAN_POINT ( 'NONE',  ( 10.00000000000000000, 0.000000000000000000, 0.000000000000000000 ) ) ;
#1393 = CARTESIAN_POINT ( 'NONE',  ( 12.00000000000000000, 5.835314593368777558, 22.81335362449846471 ) ) ;
#1394 = ADVANCED_FACE ( 'NONE', ( #38992 ), #12165, .F. ) ;
#1395 = DIRECTION ( 'NONE',  ( 0.000000000000000000, -0.07845909572785234043, 0.9969173337331274087 ) ) ;
#1396 = CARTESIAN_POINT ( 'NONE',  ( 10.00000000000000000, -59.46389618801999433, 49.70050353004867816 ) ) ;
#1397 = DIRECTION ( 'NONE',  ( 0.000000000000000000, 0.000000000000000000, -1.000000000000000000 ) ) ;
#1398 = EDGE_CURVE ( 'NONE', #55375, #766, #45384, .T. ) ;
#1399 = DIRECTION ( 'NONE',  ( -0.000000000000000000, -0.000000000000000000, 1.000000000000000000 ) ) ;
#1400 = CARTESIAN_POINT ( 'NONE',  ( 93.84685191531248449, 88.00268892867053694, 86.09739583420049769 ) ) ;
#1401 = EDGE_CURVE ( 'NONE', #32707, #28632, #35106, .T. ) ;
#1402 = CARTESIAN_POINT ( 'NONE',  ( -92.69370383062498320, -211.3315407142195852, 86.25614583420048120 ) ) ;
#1403 = ORIENTED_EDGE ( 'NONE', *, *, #50554, .F. ) ;
#1404 = VECTOR ( 'NONE', #49786, 1000.000000000000000 ) ;
#1405 = CARTESIAN_POINT ( 'NONE',  ( 96.32499999999998863, -212.2949673200287179, 83.30604166840096525 ) ) ;
#1406 = AXIS2_PLACEMENT_3D ( 'NONE', #47553, #28778, #47185 ) ;
#1407 = CARTESIAN_POINT ( 'NONE',  ( -92.34999999999999432, -208.4700217866474645, 82.75041666666665208 ) ) ;
#1408 = CARTESIAN_POINT ( 'NONE',  ( -92.69370383062505425, 88.66845928578038638, 77.20739583420046870 ) ) ;
#1409 = AXIS2_PLACEMENT_3D ( 'NONE', #53674, #19086, #35631 ) ;
#1410 = AXIS2_PLACEMENT_3D ( 'NONE', #22614, #38047, #49679 ) ;
#1411 = CARTESIAN_POINT ( 'NONE',  ( 95.00000000000000000, -207.3369185715606307, 85.67406250086715147 ) ) ;
#1412 = ORIENTED_EDGE ( 'NONE', *, *, #5219, .F. ) ;
#1413 = VECTOR ( 'NONE', #13421, 1000.000000000000000 ) ;
#1414 = ORIENTED_EDGE ( 'NONE', *, *, #22167, .T. ) ;
#1415 =( BOUNDED_CURVE ( )  B_SPLINE_CURVE ( 2, ( #55247, #62014, #10879, #21026, #50342, #61269, #73272 ),
 .UNSPECIFIED., .F., .F. ) 
 B_SPLINE_CURVE_WITH_KNOTS ( ( 3, 2, 2, 3 ),
 ( 0.8125000000000002220, 0.8194444444444446418, 0.8263888888888889506, 0.8333333333333334814 ),
 .UNSPECIFIED. ) 
 CURVE ( )  GEOMETRIC_REPRESENTATION_ITEM ( )  RATIONAL_B_SPLINE_CURVE ( ( 0.9999999999999956701, 0.8660254037844430375, 1.000000000000000000, 0.8660254037844387076, 1.000000000000000000, 0.8660254037844365982, 1.000000000000002220 ) ) 
 REPRESENTATION_ITEM ( '' )  );
#1416 = ADVANCED_FACE ( 'NONE', ( #10037 ), #32956, .F. ) ;
#1417 = EDGE_LOOP ( 'NONE', ( #24724, #55404, #20548, #16275 ) ) ;
#1418 = VECTOR ( 'NONE', #74185, 1000.000000000000000 ) ;
#1419 = DIRECTION ( 'NONE',  ( 1.000000000000000000, 0.000000000000000000, 0.000000000000000000 ) ) ;
#1421 = CARTESIAN_POINT ( 'NONE',  ( 97.64999999999999147, 90.00000000000002842, 90.00000000000000000 ) ) ;
#1420 = AXIS2_PLACEMENT_3D ( 'NONE', #24353, #57095, #29979 ) ;
#1422 = EDGE_LOOP ( 'NONE', ( #60315, #40508, #7746, #707 ) ) ;
#1423 = AXIS2_PLACEMENT_3D ( 'NONE', #13367, #36300, #7735 ) ;
#1424 = ORIENTED_EDGE ( 'NONE', *, *, #33606, .T. ) ;
#1425 = CARTESIAN_POINT ( 'NONE',  ( 95.00000000000000000, -207.3369185715606307, 83.29281250086715715 ) ) ;
#1426 = EDGE_CURVE ( 'NONE', #17494, #34012, #52386, .T. ) ;
#1427 = DIRECTION ( 'NONE',  ( 0.000000000000000000, 0.000000000000000000, 1.000000000000000000 ) ) ;
#1428 = EDGE_CURVE ( 'NONE', #19508, #17352, #18011, .T. ) ;
#1429 = CARTESIAN_POINT ( 'NONE',  ( 1.560000000000000053, -0.8660254037844384856, -1.500000000000000000 ) ) ;
#1430 = AXIS2_PLACEMENT_3D ( 'NONE', #4521, #4148, #32316 ) ;
#1431 = CYLINDRICAL_SURFACE ( 'NONE', #22074, 77.49899999999999523 ) ;
#1432 = DIRECTION ( 'NONE',  ( 1.000000000000000000, 0.000000000000000000, 0.000000000000000000 ) ) ;
#1433 = EDGE_CURVE ( 'NONE', #64991, #31095, #60059, .T. ) ;
#1434 = DIRECTION ( 'NONE',  ( 0.000000000000000000, -0.7071067811865535679, 0.7071067811865413555 ) ) ;
#1435 = CARTESIAN_POINT ( 'NONE',  ( 93.67500000000001137, -212.2949673200287179, 85.02583333333332405 ) ) ;
#1436 = EDGE_LOOP ( 'NONE', ( #22950, #70821, #30835 ) ) ;
#1437 = ORIENTED_EDGE ( 'NONE', *, *, #10127, .T. ) ;
#1438 = ORIENTED_EDGE ( 'NONE', *, *, #18270, .F. ) ;
#1439 = VERTEX_POINT ( 'NONE', #45008 ) ;
#1440 = CARTESIAN_POINT ( 'NONE',  ( 0.000000000000000000, 59.46389618801963195, 49.70050353004911159 ) ) ;
#1441 = CARTESIAN_POINT ( 'NONE',  ( -97.30629616937501680, 90.00000000000004263, 88.53156250086716739 ) ) ;
#1442 = CARTESIAN_POINT ( 'NONE',  ( -0.0004442498525516064278, 0.001194404164626844313, -80.00000000000000000 ) ) ;
#1443 = CARTESIAN_POINT ( 'NONE',  ( 97.65000000000000568, -210.0000154727341055, 78.33187446658581621 ) ) ;
#1444 = CARTESIAN_POINT ( 'NONE',  ( 93.84685191531249870, -208.0026889286704943, 88.90197916753380980 ) ) ;
#1445 = CARTESIAN_POINT ( 'NONE',  ( 97.64999999999997726, 88.47002178664753558, 79.46958333333333258 ) ) ;
#1446 = ORIENTED_EDGE ( 'NONE', *, *, #4810, .F. ) ;
#1447 = CARTESIAN_POINT ( 'NONE',  ( -97.64999999999996305, -209.9999999999999716, 89.44437500173430067 ) ) ;
#1448 = ORIENTED_EDGE ( 'NONE', *, *, #18311, .T. ) ;
#1449 = CARTESIAN_POINT ( 'NONE',  ( -57.50000000000000000, 0.000000000000000000, -270.0000000000000000 ) ) ;
#1450 = VERTEX_POINT ( 'NONE', #33321 ) ;
#1451 = CARTESIAN_POINT ( 'NONE',  ( -92.35000000000005116, 91.52997821335253548, 87.27479166840096525 ) ) ;
#1452 = CARTESIAN_POINT ( 'NONE',  ( 94.99999999999998579, 87.33691857156068750, 75.19656250086714522 ) ) ;
#1453 = ORIENTED_EDGE ( 'NONE', *, *, #6036, .T. ) ;
#1454 = CARTESIAN_POINT ( 'NONE',  ( 10.00000000000000000, 37.58145647212453611, 16.68533520207917675 ) ) ;
#1455 = DIRECTION ( 'NONE',  ( 1.000000000000000000, 0.000000000000000000, 0.000000000000000000 ) ) ;
#1456 = DIRECTION ( 'NONE',  ( 0.000000000000000000, 0.000000000000000000, 1.000000000000000000 ) ) ;
#1457 = AXIS2_PLACEMENT_3D ( 'NONE', #5326, #47014, #69566 ) ;
#1458 = FACE_OUTER_BOUND ( 'NONE', #20264, .T. ) ;
#1459 = EDGE_LOOP ( 'NONE', ( #69912, #42166 ) ) ;
#1460 = CARTESIAN_POINT ( 'NONE',  ( 10.00000000000000000, 54.21277698773675979, 55.38113227695801299 ) ) ;
#1461 = CARTESIAN_POINT ( 'NONE',  ( -94.99999999999997158, -207.3369185715606307, 75.51406250086714067 ) ) ;
#1462 = ORIENTED_EDGE ( 'NONE', *, *, #50315, .F. ) ;
#1463 = VERTEX_POINT ( 'NONE', #51007 ) ;
#1464 = CARTESIAN_POINT ( 'NONE',  ( 11.99999999999999822, 51.02545421589402252, -55.20638768913705263 ) ) ;
#1465 = AXIS2_PLACEMENT_3D ( 'NONE', #47742, #70655, #59776 ) ;
#1466 = CARTESIAN_POINT ( 'NONE',  ( 10.00000000000000000, 27.13269053701096922, 25.88420570971410228 ) ) ;
#1467 = CARTESIAN_POINT ( 'NONE',  ( 8.452893869119503023, -12.51233732111638375, -1.199999999999999956 ) ) ;
#1468 = ORIENTED_EDGE ( 'NONE', *, *, #34535, .F. ) ;
#1469 = CARTESIAN_POINT ( 'NONE',  ( -97.30629616937497417, -208.6684592857803011, 86.57364583420047666 ) ) ;
#1470 = ORIENTED_EDGE ( 'NONE', *, *, #28367, .T. ) ;
#1471 = ORIENTED_EDGE ( 'NONE', *, *, #12870, .F. ) ;
#1472 = ADVANCED_FACE ( 'NONE', ( #38621 ), #1313, .T. ) ;
#1473 = ORIENTED_EDGE ( 'NONE', *, *, #45783, .F. ) ;
#1474 = CARTESIAN_POINT ( 'NONE',  ( 11.99999999999999822, 80.55351364060588537, 15.33399622253511829 ) ) ;
#1475 = CIRCLE ( 'NONE', #43468, 37.49900000000000944 ) ;
#1476 = AXIS2_PLACEMENT_3D ( 'NONE', #15646, #9993, #43498 ) ;
#1477 = FILL_AREA_STYLE ('',( #48034 ) ) ;
#1478 = CARTESIAN_POINT ( 'NONE',  ( 94.99999999999998579, 92.66308142843932671, 81.86406250086713499 ) ) ;
#1479 = FACE_OUTER_BOUND ( 'NONE', #30990, .T. ) ;
#1480 = AXIS2_PLACEMENT_3D ( 'NONE', #65172, #58785, #7282 ) ;
#1481 = CARTESIAN_POINT ( 'NONE',  ( 10.00000000000000000, -29.81001611430991360, -22.74946021919165418 ) ) ;
#1482 = ADVANCED_FACE ( 'NONE', ( #68307 ), #67559, .T. ) ;
#1483 = CYLINDRICAL_SURFACE ( 'NONE', #12026, 2.649999999999999467 ) ;
#1484 = CARTESIAN_POINT ( 'NONE',  ( 10.00000000000000000, 73.72996012237460661, -14.67089635893632504 ) ) ;
#1485 = LINE ( 'NONE', #36753, #73620 ) ;
#1486 = EDGE_CURVE ( 'NONE', #13338, #50169, #7947, .T. ) ;
#1487 = LINE ( 'NONE', #13080, #23907 ) ;
#1488 = LINE ( 'NONE', #13456, #332 ) ;
#1489 = CYLINDRICAL_SURFACE ( 'NONE', #8409, 2.649999999999999467 ) ;
#1490 = EDGE_CURVE ( 'NONE', #73251, #73292, #52095, .T. ) ;
#1491 = DIRECTION ( 'NONE',  ( 0.000000000000000000, 0.000000000000000000, 1.000000000000000000 ) ) ;
#1492 = CARTESIAN_POINT ( 'NONE',  ( -93.84685191531252713, 88.00268892867056536, 87.94947916753380923 ) ) ;
#1493 = DIRECTION ( 'NONE',  ( 0.000000000000000000, 0.000000000000000000, 1.000000000000000000 ) ) ;
#1494 = CARTESIAN_POINT ( 'NONE',  ( 10.00000000000000000, 0.8828120875905820508, -37.48860685352290290 ) ) ;
#1495 = EDGE_CURVE ( 'NONE', #24191, #40982, #61218, .T. ) ;
#1496 = VERTEX_POINT ( 'NONE', #33711 ) ;
#1497 = CARTESIAN_POINT ( 'NONE',  ( 97.64999999999987779, -208.4700217866473793, 83.38541666666667140 ) ) ;
#1498 = DIRECTION ( 'NONE',  ( 0.000000000000000000, 0.8910065241883688980, -0.4539904997395445840 ) ) ;
#1499 = EDGE_CURVE ( 'NONE', #11081, #22472, #23824, .T. ) ;
#1500 = CARTESIAN_POINT ( 'NONE',  ( 0.000000000000000000, 0.000000000000000000, 53.20000000000001705 ) ) ;
#1501 = STYLED_ITEM ( 'NONE', ( #59364 ), #59777 ) ;
#1502 = VECTOR ( 'NONE', #20654, 1000.000000000000000 ) ;
#1503 = DIRECTION ( 'NONE',  ( -1.000000000000000000, 0.000000000000000000, 0.000000000000000000 ) ) ;
#1504 = CARTESIAN_POINT ( 'NONE',  ( 97.30629616937498838, -208.6684592857803011, 83.18697916753382060 ) ) ;
#1505 = AXIS2_PLACEMENT_3D ( 'NONE', #21389, #15770, #33046 ) ;
#1506 = ORIENTED_EDGE ( 'NONE', *, *, #55790, .T. ) ;
#1507 = ORIENTED_EDGE ( 'NONE', *, *, #8990, .T. ) ;
#1508 = VECTOR ( 'NONE', #39066, 1000.000000000000000 ) ;
#1509 = ADVANCED_FACE ( 'NONE', ( #64059 ), #36208, .T. ) ;
#1510 = DIRECTION ( 'NONE',  ( -1.000000000000000000, -0.000000000000000000, 0.000000000000000000 ) ) ;
#1511 = ORIENTED_EDGE ( 'NONE', *, *, #34886, .F. ) ;
#1512 = EDGE_CURVE ( 'NONE', #7988, #58803, #65910, .T. ) ;
#1513 = LINE ( 'NONE', #12735, #60580 ) ;
#1514 = AXIS2_PLACEMENT_3D ( 'NONE', #60420, #67529, #38211 ) ;
#1515 = CARTESIAN_POINT ( 'NONE',  ( 11.99999999999999822, -35.91791733033428358, -68.67312586195033930 ) ) ;
#1516 = VERTEX_POINT ( 'NONE', #48238 ) ;
#1517 = CARTESIAN_POINT ( 'NONE',  ( 96.15314808468750130, -211.9973110713294489, 80.48822916753381662 ) ) ;
#1518 = ORIENTED_EDGE ( 'NONE', *, *, #22646, .F. ) ;
#1519 = DIRECTION ( 'NONE',  ( -1.000000000000000000, -0.000000000000000000, 0.000000000000000000 ) ) ;
#1520 = ORIENTED_EDGE ( 'NONE', *, *, #9260, .T. ) ;
#1521 = AXIS2_PLACEMENT_3D ( 'NONE', #26148, #53617, #71638 ) ;
#1522 = VERTEX_POINT ( 'NONE', #24563 ) ;
#1523 = CARTESIAN_POINT ( 'NONE',  ( 0.000000000000000000, 0.000000000000000000, 0.000000000000000000 ) ) ;
#1524 = AXIS2_PLACEMENT_3D ( 'NONE', #17861, #63742, #12218 ) ;
#1525 = FILL_AREA_STYLE ('',( #52986 ) ) ;
#1526 = DIRECTION ( 'NONE',  ( -1.000000000000000000, 0.000000000000000000, 0.000000000000000000 ) ) ;
#1527 = ORIENTED_EDGE ( 'NONE', *, *, #52461, .F. ) ;
#1528 = CARTESIAN_POINT ( 'NONE',  ( 11.99999999999999822, 79.10210256391367523, 21.60688246758614284 ) ) ;
#1529 = CARTESIAN_POINT ( 'NONE',  ( 97.64999999999997726, -211.5299782133524502, 83.35895833506762642 ) ) ;
#1530 = CARTESIAN_POINT ( 'NONE',  ( 92.34999999999999432, 90.00000000000002842, 90.00000000000000000 ) ) ;
#1531 = ORIENTED_EDGE ( 'NONE', *, *, #3412, .F. ) ;
#1532 = DIRECTION ( 'NONE',  ( 0.000000000000000000, 0.000000000000000000, 1.000000000000000000 ) ) ;
#1533 = CARTESIAN_POINT ( 'NONE',  ( -92.35000000000003695, 90.00000000000004263, 78.88750000000000284 ) ) ;
#1534 = ORIENTED_EDGE ( 'NONE', *, *, #56706, .T. ) ;
#1535 = VERTEX_POINT ( 'NONE', #2781 ) ;
#1536 = CARTESIAN_POINT ( 'NONE',  ( 4.999999999999999112, -0.2835658343809315252, -0.5205273423269578537 ) ) ;
#1537 = ORIENTED_EDGE ( 'NONE', *, *, #72023, .T. ) ;
#1538 = CARTESIAN_POINT ( 'NONE',  ( 92.34999999999999432, 88.47002178664753558, 87.59229166840096070 ) ) ;
#1539 = EDGE_LOOP ( 'NONE', ( #2290, #72966 ) ) ;
#1540 = ORIENTED_EDGE ( 'NONE', *, *, #59533, .T. ) ;
#1541 = LINE ( 'NONE', #45898, #64524 ) ;
#1542 = CARTESIAN_POINT ( 'NONE',  ( 0.000000000000000000, -4.261787119644969479, -26.19803753235780519 ) ) ;
#1543 = VERTEX_POINT ( 'NONE', #30193 ) ;
#1544 = ORIENTED_EDGE ( 'NONE', *, *, #14957, .F. ) ;
#1545 = ORIENTED_EDGE ( 'NONE', *, *, #47043, .F. ) ;
#1546 = DIRECTION ( 'NONE',  ( 0.000000000000000000, 0.7431448254773862505, 0.6691306063588672304 ) ) ;
#1547 = DIRECTION ( 'NONE',  ( -7.945298363252408085E-16, -1.065814103640131188E-14, -1.000000000000000000 ) ) ;
#1548 = CARTESIAN_POINT ( 'NONE',  ( -97.65000000000001990, 90.00000000000004263, 86.18999999999999773 ) ) ;
#1549 = ORIENTED_EDGE ( 'NONE', *, *, #875, .F. ) ;
#1550 = CARTESIAN_POINT ( 'NONE',  ( 0.000000000000000000, -59.46389618801999433, 49.70050353004867816 ) ) ;
#1551 = CARTESIAN_POINT ( 'NONE',  ( 10.00000000000000000, 26.79245525562761188, -32.34446384429941901 ) ) ;
#1552 = ORIENTED_EDGE ( 'NONE', *, *, #14097, .T. ) ;
#1553 = CARTESIAN_POINT ( 'NONE',  ( -26.53422223201112828, -120.6595836127786043, 5.500000000000000000 ) ) ;
#1554 = CARTESIAN_POINT ( 'NONE',  ( -92.69370383062498320, -208.6684592857803011, 82.39322916753381776 ) ) ;
#1555 = ORIENTED_EDGE ( 'NONE', *, *, #26109, .F. ) ;
#1556 = CARTESIAN_POINT ( 'NONE',  ( 6.078523336270777024E-16, 5.773502691896261751, -6.000000000000000000 ) ) ;
#1557 = CARTESIAN_POINT ( 'NONE',  ( 0.000000000000000000, -46.54456581323847786, 59.03342792756247093 ) ) ;
#1558 = CARTESIAN_POINT ( 'NONE',  ( 93.67499999999998295, 92.29496732002878900, 89.33854166840096411 ) ) ;
#1559 = PLANE ( 'NONE',  #50671 ) ;
#1560 = EDGE_CURVE ( 'NONE', #10604, #44963, #42510, .T. ) ;
#1561 = STYLED_ITEM ( 'NONE', ( #5849 ), #37264 ) ;
#1562 = FACE_OUTER_BOUND ( 'NONE', #21689, .T. ) ;
#1563 = EDGE_CURVE ( 'NONE', #57100, #11579, #47135, .T. ) ;
#1564 = CIRCLE ( 'NONE', #68777, 37.49900000000000233 ) ;
#1565 = FACE_OUTER_BOUND ( 'NONE', #2977, .T. ) ;
#1566 = CARTESIAN_POINT ( 'NONE',  ( 96.85456758451090309, -211.3788240028427765, 74.79348190356850523 ) ) ;
#1567 = EDGE_CURVE ( 'NONE', #47714, #31828, #41285, .T. ) ;
#1568 = DIRECTION ( 'NONE',  ( 0.000000000000000000, 0.9969173337331276308, 0.07845909572784874608 ) ) ;
#1569 = CARTESIAN_POINT ( 'NONE',  ( 15.00000000000000000, -22.32062822937469093, 14.36278369418830181 ) ) ;
#1570 = CIRCLE ( 'NONE', #60360, 3.299999999999997158 ) ;
#1571 = CARTESIAN_POINT ( 'NONE',  ( -96.15314808468752972, 91.99731107132950569, 79.37697916753380412 ) ) ;
#1572 = CARTESIAN_POINT ( 'NONE',  ( -10.00000000000000000, 0.000000000000000000, 0.000000000000000000 ) ) ;
#1573 = DIRECTION ( 'NONE',  ( -0.000000000000000000, 1.625241993126352200E-15, 1.000000000000000000 ) ) ;
#1574 = CIRCLE ( 'NONE', #2798, 82.00000000000000000 ) ;
#1575 = DIRECTION ( 'NONE',  ( 0.000000000000000000, -0.000000000000000000, -1.000000000000000000 ) ) ;
#1576 = EDGE_CURVE ( 'NONE', #33089, #21642, #34083, .T. ) ;
#1577 = CARTESIAN_POINT ( 'NONE',  ( 11.99999999999999822, 68.26794271651307611, -31.47745569255064169 ) ) ;
#1578 = LINE ( 'NONE', #69587, #65841 ) ;
#1579 = AXIS2_PLACEMENT_3D ( 'NONE', #26390, #49313, #35370 ) ;
#1580 = DIRECTION ( 'NONE',  ( -0.7071067811865474617, 0.000000000000000000, 0.7071067811865474617 ) ) ;
#1581 = CARTESIAN_POINT ( 'NONE',  ( 10.00000000000000000, -6.736453364083292428, -36.88895765772640800 ) ) ;
#1582 = CARTESIAN_POINT ( 'NONE',  ( 95.00000000000000000, -209.9999999999999716, 90.00000000000000000 ) ) ;
#1583 = CARTESIAN_POINT ( 'NONE',  ( -92.69370383062498320, -210.9303121318040155, 74.84209103131394158 ) ) ;
#1584 = CARTESIAN_POINT ( 'NONE',  ( 10.00000000000000000, 33.80338159004283938, 16.23288003029508886 ) ) ;
#1585 = EDGE_CURVE ( 'NONE', #57628, #18829, #8754, .T. ) ;
#1586 = ORIENTED_EDGE ( 'NONE', *, *, #57493, .F. ) ;
#1587 = CARTESIAN_POINT ( 'NONE',  ( 10.00000000000000000, -35.47612816024506088, -22.48208911017539435 ) ) ;
#1588 = EDGE_CURVE ( 'NONE', #7308, #26594, #25659, .T. ) ;
#1589 = DIRECTION ( 'NONE',  ( 0.000000000000000000, -0.9876883405951394357, 0.1564344650402205716 ) ) ;
#1590 = CARTESIAN_POINT ( 'NONE',  ( 3.000000000000000000, 0.000000000000000000, -6.000000000000001776 ) ) ;
#1591 = CARTESIAN_POINT ( 'NONE',  ( 0.000000000000000000, -19.89357724624987256, -12.59942793731086041 ) ) ;
#1592 = ADVANCED_FACE ( 'NONE', ( #19648 ), #13277, .T. ) ;
#1593 = EDGE_CURVE ( 'NONE', #24805, #16594, #19640, .T. ) ;
#1594 = CARTESIAN_POINT ( 'NONE',  ( 97.64999999999999147, 90.00001154861291752, 83.41187540116095533 ) ) ;
#1595 = EDGE_LOOP ( 'NONE', ( #4910, #24656 ) ) ;
#1596 = DIRECTION ( 'NONE',  ( -0.000000000000000000, -0.000000000000000000, 1.000000000000000000 ) ) ;
#1597 = EDGE_CURVE ( 'NONE', #29219, #39517, #2881, .T. ) ;
#1598 = SURFACE_STYLE_USAGE ( .BOTH. , #12090 ) ;
#1599 = ORIENTED_EDGE ( 'NONE', *, *, #38387, .F. ) ;
#1600 = CARTESIAN_POINT ( 'NONE',  ( 93.84685191531251292, -211.9973110713294489, 85.93864583420048575 ) ) ;
#1601 = CARTESIAN_POINT ( 'NONE',  ( 92.69370383062501162, -209.9999999999999716, 87.89656250086714806 ) ) ;
#1602 = ORIENTED_EDGE ( 'NONE', *, *, #6612, .T. ) ;
#1603 = CARTESIAN_POINT ( 'NONE',  ( 11.99999999999999822, -24.73286445877757345, 73.44644590900053061 ) ) ;
#1604 = EDGE_CURVE ( 'NONE', #60490, #17740, #70780, .T. ) ;
#1605 = AXIS2_PLACEMENT_3D ( 'NONE', #24970, #53924, #59563 ) ;
#1606 = VERTEX_POINT ( 'NONE', #36951 ) ;
#1607 = DIRECTION ( 'NONE',  ( 0.000000000000000000, 0.000000000000000000, -1.000000000000000000 ) ) ;
#1608 = ORIENTED_EDGE ( 'NONE', *, *, #37255, .T. ) ;
#1609 = CARTESIAN_POINT ( 'NONE',  ( -93.84685191531254134, 91.99731107132950569, 81.33489583420049485 ) ) ;
#1610 = AXIS2_PLACEMENT_3D ( 'NONE', #59355, #54817, #8590 ) ;
#1611 = VERTEX_POINT ( 'NONE', #59524 ) ;
#1612 = ORIENTED_EDGE ( 'NONE', *, *, #35372, .F. ) ;
#1613 = CYLINDRICAL_SURFACE ( 'NONE', #24485, 3.299999999999969624 ) ;
#1614 = VERTEX_POINT ( 'NONE', #42238 ) ;
#1615 = DIRECTION ( 'NONE',  ( 0.000000000000000000, 0.000000000000000000, 1.000000000000000000 ) ) ;
#1616 =( NAMED_UNIT ( * ) PLANE_ANGLE_UNIT ( ) SI_UNIT ( $, .RADIAN. ) );
#1617 = ORIENTED_EDGE ( 'NONE', *, *, #51959, .T. ) ;
#1618 = DIRECTION ( 'NONE',  ( -1.000000000000000000, 0.000000000000000000, 0.000000000000000000 ) ) ;
#1619 = AXIS2_PLACEMENT_3D ( 'NONE', #13758, #25425, #3623 ) ;
#1620 = ORIENTED_EDGE ( 'NONE', *, *, #10264, .F. ) ;
#1621 =( BOUNDED_CURVE ( )  B_SPLINE_CURVE ( 2, ( #67884, #27269, #44959, #20901, #21253, #16375, #39317 ),
 .UNSPECIFIED., .F., .F. ) 
 B_SPLINE_CURVE_WITH_KNOTS ( ( 3, 2, 2, 3 ),
 ( 0.06350193517771154927, 0.07055765540916983380, 0.07761342095008726127, 0.08466915177933910519 ),
 .UNSPECIFIED. ) 
 CURVE ( )  GEOMETRIC_REPRESENTATION_ITEM ( )  RATIONAL_B_SPLINE_CURVE ( ( 0.9999982793426236416, 0.8660262641186515786, 1.000000000000000000, 0.8660254037844387076, 1.000000000000000000, 0.8660260628881676359, 0.9999986817990271781 ) ) 
 REPRESENTATION_ITEM ( '' )  );
#1622 = CARTESIAN_POINT ( 'NONE',  ( 94.70433044323989691, 87.37275709988163896, 74.99300273738302280 ) ) ;
#1623 = AXIS2_PLACEMENT_3D ( 'NONE', #10219, #44069, #38428 ) ;
#1624 = VERTEX_POINT ( 'NONE', #42596 ) ;
#1625 = ORIENTED_EDGE ( 'NONE', *, *, #25023, .F. ) ;
#1626 = CIRCLE ( 'NONE', #21979, 13.71399988598171049 ) ;
#1627 = EDGE_LOOP ( 'NONE', ( #50321, #61394, #9092, #16789 ) ) ;
#1628 = CARTESIAN_POINT ( 'NONE',  ( 95.00000000000000000, -212.6630814284392557, 82.18156250086714465 ) ) ;
#1629 = CARTESIAN_POINT ( 'NONE',  ( 0.000000000000000000, -81.96053171279903893, 2.543863470248094227 ) ) ;
#1630 = AXIS2_PLACEMENT_3D ( 'NONE', #62392, #51090, #33800 ) ;
#1631 = CONTEXT_DEPENDENT_SHAPE_REPRESENTATION ( #71439, #33177 ) ;
#1632 = LINE ( 'NONE', #2734, #4166 ) ;
#1633 = CARTESIAN_POINT ( 'NONE',  ( 0.000000000000000000, -76.69515212745996280, -29.01471420065643869 ) ) ;
#1634 = CARTESIAN_POINT ( 'NONE',  ( 10.00000000000000000, 55.16347631943041563, 60.67117009219156643 ) ) ;
#1635 = CARTESIAN_POINT ( 'NONE',  ( 10.00000000000000000, -75.11764819372145041, -2.946379043147127064 ) ) ;
#1636 = DIRECTION ( 'NONE',  ( 0.4565542962317865050, 0.000000000000000000, 0.8896955516311735312 ) ) ;
#1637 = CARTESIAN_POINT ( 'NONE',  ( -96.15314808468745866, -211.9973110713294489, 85.93864583420048575 ) ) ;
#1638 = CARTESIAN_POINT ( 'NONE',  ( -95.00000000000002842, 92.66308142843932671, 83.29281250086717137 ) ) ;
#1639 = EDGE_LOOP ( 'NONE', ( #49549, #69239, #69076, #41140, #52089 ) ) ;
#1640 = CARTESIAN_POINT ( 'NONE',  ( 92.69370383062498320, 88.66845928578037217, 79.53572916753380184 ) ) ;
#1641 = ORIENTED_EDGE ( 'NONE', *, *, #28400, .F. ) ;
#1642 = CARTESIAN_POINT ( 'NONE',  ( 11.99999999999999822, 76.69515212746016175, 29.01471420065590578 ) ) ;
#1643 = PLANE ( 'NONE',  #55177 ) ;
#1644 = CARTESIAN_POINT ( 'NONE',  ( 0.000000000000000000, -20.40083707022935400, 72.35432306680478121 ) ) ;
#1645 = CARTESIAN_POINT ( 'NONE',  ( -20.63750000000001705, -1.978676859095576340E-13, -15.80000000000029914 ) ) ;
#1646 = LINE ( 'NONE', #7251, #29630 ) ;
#1647 = CARTESIAN_POINT ( 'NONE',  ( -97.30629616937495996, -209.9999999999999716, 84.56281250086713897 ) ) ;
#1648 = CARTESIAN_POINT ( 'NONE',  ( 10.00000000000000000, 35.38097989696528600, -12.42422080174602605 ) ) ;
#1649 = EDGE_CURVE ( 'NONE', #6687, #39397, #29244, .T. ) ;
#1650 = CARTESIAN_POINT ( 'NONE',  ( 92.35000000003287823, 90.00000839536618003, 84.99910573348789455 ) ) ;
#1651 = DIRECTION ( 'NONE',  ( -1.000000000000000000, -0.000000000000000000, 0.000000000000000000 ) ) ;
#1652 = DIRECTION ( 'NONE',  ( -1.000000000000000000, 0.000000000000000000, 0.000000000000000000 ) ) ;
#1653 = ORIENTED_EDGE ( 'NONE', *, *, #66798, .T. ) ;
#1654 = EDGE_CURVE ( 'NONE', #23480, #37858, #64796, .T. ) ;
#1655 = VERTEX_POINT ( 'NONE', #42974 ) ;
#1656 = ADVANCED_FACE ( 'NONE', ( #14386 ), #37334, .F. ) ;
#1657 = ADVANCED_FACE ( 'NONE', ( #53506 ), #65168, .T. ) ;
#1658 = CARTESIAN_POINT ( 'NONE',  ( -97.65000000000001990, 91.52997821335253548, 75.97708333333333997 ) ) ;
#1659 = DIRECTION ( 'NONE',  ( -1.000000000000000000, 0.000000000000000000, 0.000000000000000000 ) ) ;
#1660 = CARTESIAN_POINT ( 'NONE',  ( -97.30629616937501680, 90.00000000000004263, 88.37281250086715545 ) ) ;
#1661 = CARTESIAN_POINT ( 'NONE',  ( -11.99999999999999645, 2.553388576222231231E-15, 20.69999999999999929 ) ) ;
#1662 = DIRECTION ( 'NONE',  ( 0.000000000000000000, -0.5000000000000038858, -0.8660254037844363761 ) ) ;
#1663 = AXIS2_PLACEMENT_3D ( 'NONE', #53590, #13727, #36664 ) ;
#1664 = FACE_OUTER_BOUND ( 'NONE', #62733, .T. ) ;
#1665 = DIRECTION ( 'NONE',  ( -1.000000000000000000, -0.000000000000000000, -0.000000000000000000 ) ) ;
#1666 = ORIENTED_EDGE ( 'NONE', *, *, #39550, .T. ) ;
#1667 = CARTESIAN_POINT ( 'NONE',  ( -95.00000000000002842, 87.33691857156074434, 75.83156250086715033 ) ) ;
#1668 = CARTESIAN_POINT ( 'NONE',  ( 10.00000000000000000, -22.64427369931191336, 30.00120703465197280 ) ) ;
#1669 = CARTESIAN_POINT ( 'NONE',  ( 0.000000000000000000, 0.000000000000000000, 0.000000000000000000 ) ) ;
#1670 = CARTESIAN_POINT ( 'NONE',  ( 93.67500000000001137, -207.7050326799711968, 84.25854166840096582 ) ) ;
#1671 = CARTESIAN_POINT ( 'NONE',  ( -15.70000000000000284, -120.0000000000000000, -90.00000000000000000 ) ) ;
#1672 = CARTESIAN_POINT ( 'NONE',  ( -92.69370383062498320, -209.9999999999999716, 85.67406250086715147 ) ) ;
#1673 = SURFACE_STYLE_FILL_AREA ( #63320 ) ;
#1674 = EDGE_CURVE ( 'NONE', #6114, #67241, #3500, .T. ) ;
#1675 = DIRECTION ( 'NONE',  ( -0.000000000000000000, 0.6691306063588672304, 0.7431448254773862505 ) ) ;
#1676 = AXIS2_PLACEMENT_3D ( 'NONE', #49631, #3078, #56026 ) ;
#1677 = AXIS2_PLACEMENT_3D ( 'NONE', #55257, #34087, #27709 ) ;
#1678 = CARTESIAN_POINT ( 'NONE',  ( 2.500000000000029754, 73.00000000000001421, -258.2999999999999545 ) ) ;
#1679 = CARTESIAN_POINT ( 'NONE',  ( -97.30629616937495996, -209.9999999999999716, 77.73656250086715147 ) ) ;
#1680 = CARTESIAN_POINT ( 'NONE',  ( 93.67499999999998295, 92.29496732002878900, 88.62416666666665321 ) ) ;
#1681 = VERTEX_POINT ( 'NONE', #39176 ) ;
#1682 = CARTESIAN_POINT ( 'NONE',  ( 11.99999999999999822, -73.73191006444561424, -14.66109333815538918 ) ) ;
#1683 = CARTESIAN_POINT ( 'NONE',  ( 11.99999999999999822, 54.21277698773675979, 55.38113227695801299 ) ) ;
#1684 = CARTESIAN_POINT ( 'NONE',  ( 96.32499999999997442, 92.29496732002878900, 85.42270833506762528 ) ) ;
#1685 = EDGE_CURVE ( 'NONE', #50776, #855, #28066, .T. ) ;
#1687 = EDGE_CURVE ( 'NONE', #32720, #39781, #6457, .T. ) ;
#1686 = VECTOR ( 'NONE', #33317, 1000.000000000000000 ) ;
#1688 = DIRECTION ( 'NONE',  ( -1.000000000000000000, -0.000000000000000000, -0.000000000000000000 ) ) ;
#1689 = CARTESIAN_POINT ( 'NONE',  ( 92.69370383062501162, -209.9999999999999716, 77.57781250086713953 ) ) ;
#1690 = ORIENTED_EDGE ( 'NONE', *, *, #30848, .T. ) ;
#1691 = LINE ( 'NONE', #47509, #19176 ) ;
#1692 = SURFACE_STYLE_FILL_AREA ( #25327 ) ;
#1693 = ORIENTED_EDGE ( 'NONE', *, *, #12824, .T. ) ;
#1694 = CARTESIAN_POINT ( 'NONE',  ( 11.99999999999999822, 0.000000000000000000, 0.000000000000000000 ) ) ;
#1695 = VERTEX_POINT ( 'NONE', #33516 ) ;
#1696 = CIRCLE ( 'NONE', #5272, 77.49899999999999523 ) ;
#1697 = CARTESIAN_POINT ( 'NONE',  ( -97.64998344411506537, 91.52998777189718282, 79.23145767387349281 ) ) ;
#1698 = ORIENTED_EDGE ( 'NONE', *, *, #43746, .T. ) ;
#1699 = ORIENTED_EDGE ( 'NONE', *, *, #61480, .F. ) ;
#1700 = ORIENTED_EDGE ( 'NONE', *, *, #51808, .T. ) ;
#1701 = CARTESIAN_POINT ( 'NONE',  ( -97.64999999996712177, 90.00000839536629371, 84.99910573348492449 ) ) ;
#1702 = ORIENTED_EDGE ( 'NONE', *, *, #65557, .T. ) ;
#1703 = AXIS2_PLACEMENT_3D ( 'NONE', #54205, #42188, #65489 ) ;
#1704 = VERTEX_POINT ( 'NONE', #49333 ) ;
#1705 = CARTESIAN_POINT ( 'NONE',  ( 92.69370383062498320, 91.33154071421968467, 79.58864583420047722 ) ) ;
#1706 = CARTESIAN_POINT ( 'NONE',  ( 0.000000000000000000, 18.89407956138256139, 75.16055320797038064 ) ) ;
#1707 = CARTESIAN_POINT ( 'NONE',  ( 0.4301293587033142574, -121.4370068666438556, -2.500000000000000000 ) ) ;
#1708 = ORIENTED_EDGE ( 'NONE', *, *, #60623, .F. ) ;
#1709 = ORIENTED_EDGE ( 'NONE', *, *, #54143, .F. ) ;
#1710 = ORIENTED_EDGE ( 'NONE', *, *, #25380, .T. ) ;
#1711 = DIRECTION ( 'NONE',  ( -0.000000000000000000, -0.000000000000000000, 1.000000000000000000 ) ) ;
#1712 = ORIENTED_EDGE ( 'NONE', *, *, #1401, .F. ) ;
#1713 = CIRCLE ( 'NONE', #17289, 31.99999999999999289 ) ;
#1714 = CARTESIAN_POINT ( 'NONE',  ( -5.574404190523511974E-14, 1.019753860068740540E-13, -55.00000000000000711 ) ) ;
#1715 = CARTESIAN_POINT ( 'NONE',  ( 0.000000000000000000, -46.53671651293907274, -59.03961581697448935 ) ) ;
#1716 = LINE ( 'NONE', #13684, #11133 ) ;
#1717 = CARTESIAN_POINT ( 'NONE',  ( 10.00000000000000000, 2.956366410621684260, -75.11725578898465017 ) ) ;
#1718 = CARTESIAN_POINT ( 'NONE',  ( -0.0004442498525516064278, 0.001194404164626844313, -90.00000000000000000 ) ) ;
#1719 = DIRECTION ( 'NONE',  ( 0.000000000000000000, -0.9876883405951361050, -0.1564344650402419989 ) ) ;
#1720 = CARTESIAN_POINT ( 'NONE',  ( 94.99999999999998579, 93.05995642670504253, 77.77624999999999034 ) ) ;
#1721 = CARTESIAN_POINT ( 'NONE',  ( -94.99999999999997158, -206.9400435732949575, 79.76062500173429726 ) ) ;
#1722 = CARTESIAN_POINT ( 'NONE',  ( -22.53294031248081808, -134.0273518838794757, -2.500000000000000000 ) ) ;
#1723 = ORIENTED_EDGE ( 'NONE', *, *, #48136, .T. ) ;
#1725 = CARTESIAN_POINT ( 'NONE',  ( -95.00000000000002842, 86.94004357329504273, 75.63312500173429953 ) ) ;
#1724 = CARTESIAN_POINT ( 'NONE',  ( 92.69370383062498320, 90.00000000000002842, 89.64281250086713726 ) ) ;
#1726 = CIRCLE ( 'NONE', #31724, 31.99999999999998579 ) ;
#1727 = VERTEX_POINT ( 'NONE', #72262 ) ;
#1728 = CARTESIAN_POINT ( 'NONE',  ( 94.99999999999998579, 87.33691857156068750, 79.80031250086715033 ) ) ;
#1729 = VECTOR ( 'NONE', #24933, 1000.000000000000000 ) ;
#1730 = CARTESIAN_POINT ( 'NONE',  ( -97.64999999999996305, -209.9999999999999716, 82.37999999999999545 ) ) ;
#1731 = DIRECTION ( 'NONE',  ( -1.000000000000000000, 0.000000000000000000, -0.000000000000000000 ) ) ;
#1732 = DIRECTION ( 'NONE',  ( 1.000000000000000000, 0.000000000000000000, 0.000000000000000000 ) ) ;
#1733 = ADVANCED_FACE ( 'NONE', ( #21493 ), #72618, .F. ) ;
#1734 = LINE ( 'NONE', #70461, #12258 ) ;
#1735 = DIRECTION ( 'NONE',  ( 1.000000000000000000, 0.000000000000000000, 0.000000000000000000 ) ) ;
#1736 = VERTEX_POINT ( 'NONE', #38800 ) ;
#1737 = EDGE_CURVE ( 'NONE', #62140, #50450, #9856, .T. ) ;
#1738 = DIRECTION ( 'NONE',  ( -1.000000000000000000, 0.000000000000000000, 0.000000000000000000 ) ) ;
#1739 = CIRCLE ( 'NONE', #12468, 16.00000000000000000 ) ;
#1740 = CARTESIAN_POINT ( 'NONE',  ( 1.301042606982605321E-15, 5.773502691896264416, -5.553418012614792509 ) ) ;
#1741 = ORIENTED_EDGE ( 'NONE', *, *, #25450, .T. ) ;
#1742 = EDGE_CURVE ( 'NONE', #2166, #43747, #62203, .T. ) ;
#1743 = ORIENTED_EDGE ( 'NONE', *, *, #72785, .T. ) ;
#1744 = EDGE_CURVE ( 'NONE', #52184, #4841, #67009, .T. ) ;
#1745 = DIRECTION ( 'NONE',  ( -1.000000000000000000, -0.000000000000000000, 0.000000000000000000 ) ) ;
#1746 = DIRECTION ( 'NONE',  ( -1.000000000000000000, -0.000000000000000000, -0.000000000000000000 ) ) ;
#1747 = DIRECTION ( 'NONE',  ( 1.000000000000000000, -0.000000000000000000, -0.000000000000000000 ) ) ;
#1748 = CARTESIAN_POINT ( 'NONE',  ( 10.05638427806949586, -98.76043467366159234, 2.500000000000000000 ) ) ;
#1749 = CARTESIAN_POINT ( 'NONE',  ( -93.84685191531248449, -208.0026889286704943, 77.52489583420047836 ) ) ;
#1750 = EDGE_CURVE ( 'NONE', #21370, #55509, #60500, .T. ) ;
#1751 = ORIENTED_EDGE ( 'NONE', *, *, #16450, .F. ) ;
#1752 = CIRCLE ( 'NONE', #55740, 16.00000000000000000 ) ;
#1753 = DIRECTION ( 'NONE',  ( 0.000000000000000000, 0.1564344650402311743, -0.9876883405951377704 ) ) ;
#1754 = CARTESIAN_POINT ( 'NONE',  ( 4.903647372192503795, -146.0423547792665886, -2.500000000000000000 ) ) ;
#1755 = DIRECTION ( 'NONE',  ( -1.000000000000000000, 0.000000000000000000, 0.000000000000000000 ) ) ;
#1756 = DIRECTION ( 'NONE',  ( 1.000000000000000000, 0.000000000000000000, -0.000000000000000000 ) ) ;
#1757 = DIRECTION ( 'NONE',  ( 0.000000000000000000, 0.000000000000000000, 1.000000000000000000 ) ) ;
#1758 = LINE ( 'NONE', #18263, #66097 ) ;
#1759 = CYLINDRICAL_SURFACE ( 'NONE', #69719, 2.649999999999999467 ) ;
#1760 = CYLINDRICAL_SURFACE ( 'NONE', #50839, 31.99999999999998579 ) ;
#1761 = FACE_OUTER_BOUND ( 'NONE', #45328, .T. ) ;
#1762 = ADVANCED_FACE ( 'NONE', ( #3869 ), #67367, .T. ) ;
#1763 = DIRECTION ( 'NONE',  ( 0.000000000000000000, 0.000000000000000000, 1.000000000000000000 ) ) ;
#1764 = EDGE_CURVE ( 'NONE', #39181, #43104, #22066, .T. ) ;
#1765 = AXIS2_PLACEMENT_3D ( 'NONE', #44988, #68289, #73165 ) ;
#1766 = CARTESIAN_POINT ( 'NONE',  ( 97.30629616937498838, 91.33154071421968467, 85.09197916753380753 ) ) ;
#1767 = CARTESIAN_POINT ( 'NONE',  ( -92.69370383062498320, -208.6684592857803295, 86.99697916753382287 ) ) ;
#1768 = DIRECTION ( 'NONE',  ( 0.000000000000000000, 0.8090169943749486725, -0.5877852522924713607 ) ) ;
#1769 = ORIENTED_EDGE ( 'NONE', *, *, #39831, .T. ) ;
#1770 = CARTESIAN_POINT ( 'NONE',  ( -96.32500000000001705, 92.29496732002878900, 81.63916666666666799 ) ) ;
#1771 = CARTESIAN_POINT ( 'NONE',  ( -97.64999999999996305, -209.9999999999999716, 81.10999999999999943 ) ) ;
#1772 = CARTESIAN_POINT ( 'NONE',  ( -97.30629616937501680, 90.00000000000004263, 76.30781250086714351 ) ) ;
#1773 = ADVANCED_FACE ( 'NONE', ( #15493 ), #56091, .T. ) ;
#1774 = EDGE_CURVE ( 'NONE', #14718, #17127, #24477, .T. ) ;
#1775 = CIRCLE ( 'NONE', #40207, 12.75000000000265565 ) ;
#1776 = CARTESIAN_POINT ( 'NONE',  ( 97.30629616937498838, -211.3315407142195852, 86.73239583420047438 ) ) ;
#1777 = VERTEX_POINT ( 'NONE', #67745 ) ;
#1778 = EDGE_LOOP ( 'NONE', ( #27540, #48936, #26434, #34433 ) ) ;
#1779 = CIRCLE ( 'NONE', #46184, 12.49999999999999645 ) ;
#1780 = AXIS2_PLACEMENT_3D ( 'NONE', #62501, #62116, #27521 ) ;
#1781 = VERTEX_POINT ( 'NONE', #33901 ) ;
#1782 = AXIS2_PLACEMENT_3D ( 'NONE', #18093, #41035, #58311 ) ;
#1783 = FACE_OUTER_BOUND ( 'NONE', #22087, .T. ) ;
#1784 = VECTOR ( 'NONE', #5629, 1000.000000000000000 ) ;
#1785 = CARTESIAN_POINT ( 'NONE',  ( 30.50000000000000000, -120.0000000000000000, 2.500000000000000000 ) ) ;
#1786 = EDGE_LOOP ( 'NONE', ( #59836, #5307, #25692, #57159 ) ) ;
#1787 = VERTEX_POINT ( 'NONE', #50807 ) ;
#1788 = AXIS2_PLACEMENT_3D ( 'NONE', #24828, #48138, #59416 ) ;
#1789 = CARTESIAN_POINT ( 'NONE',  ( 10.00000000000000000, -59.03342792756297541, 46.54456581323783126 ) ) ;
#1790 = CARTESIAN_POINT ( 'NONE',  ( 92.69370383062501162, -208.6684592857803295, 82.12864583420048348 ) ) ;
#1792 = CARTESIAN_POINT ( 'NONE',  ( 92.34999999999999432, 90.00000000000002842, 81.10999999999999943 ) ) ;
#1791 = CIRCLE ( 'NONE', #11346, 15.99999999999999645 ) ;
#1793 = CARTESIAN_POINT ( 'NONE',  ( 5.000000000000000000, -22.48208911017474065, -35.47612816024548721 ) ) ;
#1794 = CARTESIAN_POINT ( 'NONE',  ( 0.000000000000000000, -16.45098606841149902, 33.79645857604508308 ) ) ;
#1795 = CARTESIAN_POINT ( 'NONE',  ( 92.35000000000000853, -209.9999999999999716, 85.55499999999999261 ) ) ;
#1796 = EDGE_CURVE ( 'NONE', #32190, #40071, #39551, .T. ) ;
#1797 = AXIS2_PLACEMENT_3D ( 'NONE', #45062, #34888, #6326 ) ;
#1798 = ORIENTED_EDGE ( 'NONE', *, *, #2824, .T. ) ;
#1799 = ORIENTED_EDGE ( 'NONE', *, *, #67467, .T. ) ;
#1800 = VERTEX_POINT ( 'NONE', #51930 ) ;
#1801 = EDGE_LOOP ( 'NONE', ( #7477, #67129, #5153, #54165 ) ) ;
#1802 = CARTESIAN_POINT ( 'NONE',  ( -93.84685191531252713, 88.00268892867056536, 88.10822916753382117 ) ) ;
#1803 = CARTESIAN_POINT ( 'NONE',  ( 11.99999999999999822, 5.256550761632864166, 77.32052557432842832 ) ) ;
#1804 = EDGE_CURVE ( 'NONE', #48805, #70509, #59712, .T. ) ;
#1805 = DIRECTION ( 'NONE',  ( -1.000000000000000000, -0.000000000000000000, 0.000000000000000000 ) ) ;
#1806 = CARTESIAN_POINT ( 'NONE',  ( 93.84685191531251292, -211.9973110713294489, 87.84364583420047268 ) ) ;
#1807 = CARTESIAN_POINT ( 'NONE',  ( 93.67499999999999716, 87.70503267997126784, 79.31083333333333485 ) ) ;
#1808 = EDGE_CURVE ( 'NONE', #1450, #35339, #6452, .T. ) ;
#1809 = VERTEX_POINT ( 'NONE', #69229 ) ;
#1810 = CARTESIAN_POINT ( 'NONE',  ( -96.32499999999996021, -207.7050326799711968, 88.06854166840095388 ) ) ;
#1811 = ORIENTED_EDGE ( 'NONE', *, *, #51766, .F. ) ;
#1812 = DIRECTION ( 'NONE',  ( -1.000000000000000000, 0.000000000000000000, 0.000000000000000000 ) ) ;
#1813 = ORIENTED_EDGE ( 'NONE', *, *, #40779, .T. ) ;
#1814 = CARTESIAN_POINT ( 'NONE',  ( -97.65000000000001990, 88.47002178664754979, 86.32229166840097889 ) ) ;
#1815 = CARTESIAN_POINT ( 'NONE',  ( 93.84685191531248449, 91.99731107132950569, 89.69572916753382685 ) ) ;
#1816 = VERTEX_POINT ( 'NONE', #35018 ) ;
#1817 = CARTESIAN_POINT ( 'NONE',  ( 0.000000000000000000, 0.000000000000000000, 0.000000000000000000 ) ) ;
#1818 = ADVANCED_FACE ( 'NONE', ( #69598 ), #6092, .F. ) ;
#1819 = LINE ( 'NONE', #64944, #43412 ) ;
#1820 = CARTESIAN_POINT ( 'NONE',  ( 95.00000000000000000, -209.9999999999999716, 90.00000000000000000 ) ) ;
#1821 = LINE ( 'NONE', #57824, #26304 ) ;
#1822 = ORIENTED_EDGE ( 'NONE', *, *, #50920, .T. ) ;
#1823 = CARTESIAN_POINT ( 'NONE',  ( 15.00000000000000000, 0.000000000000000000, 0.000000000000000000 ) ) ;
#1824 = CARTESIAN_POINT ( 'NONE',  ( -97.64999999993855795, 90.00001182123732235, 81.82400613091868991 ) ) ;
#1825 = AXIS2_PLACEMENT_3D ( 'NONE', #50580, #21252, #39316 ) ;
#1826 = ORIENTED_EDGE ( 'NONE', *, *, #3341, .T. ) ;
#1827 = ORIENTED_EDGE ( 'NONE', *, *, #69328, .T. ) ;
#1828 = CYLINDRICAL_SURFACE ( 'NONE', #2605, 31.99999999999998579 ) ;
#1829 = CARTESIAN_POINT ( 'NONE',  ( 5.000000000000000888, 0.9828435001097636237, -5.956909652965543422 ) ) ;
#1830 = DIRECTION ( 'NONE',  ( 0.000000000000000000, 0.000000000000000000, 1.000000000000000000 ) ) ;
#1831 = CARTESIAN_POINT ( 'NONE',  ( -97.30629616937497417, -211.3315407142195852, 88.58447916753382856 ) ) ;
#1832 = ORIENTED_EDGE ( 'NONE', *, *, #65900, .T. ) ;
#1833 = AXIS2_PLACEMENT_3D ( 'NONE', #38345, #39094, #60909 ) ;
#1834 = EDGE_CURVE ( 'NONE', #56117, #3345, #113, .T. ) ;
#1835 = CARTESIAN_POINT ( 'NONE',  ( -26.53422223201112828, -120.6595836127786043, 5.500000000000000000 ) ) ;
#1836 = VECTOR ( 'NONE', #32453, 1000.000000000000000 ) ;
#1837 = ORIENTED_EDGE ( 'NONE', *, *, #48323, .F. ) ;
#1838 = EDGE_LOOP ( 'NONE', ( #45044, #16033, #19530, #9739 ) ) ;
#1839 = DIRECTION ( 'NONE',  ( -0.7585478161175706058, -0.6516173805718078471, 0.000000000000000000 ) ) ;
#1840 = AXIS2_PLACEMENT_3D ( 'NONE', #8394, #31311, #54263 ) ;
#1841 = FACE_OUTER_BOUND ( 'NONE', #23600, .T. ) ;
#1842 = FACE_OUTER_BOUND ( 'NONE', #73904, .T. ) ;
#1843 = CARTESIAN_POINT ( 'NONE',  ( 93.84685191531248449, 91.99731107132950569, 80.01197916753380923 ) ) ;
#1844 = CARTESIAN_POINT ( 'NONE',  ( 0.000000000000000000, 62.20884554314020676, 46.21855187248652896 ) ) ;
#1845 = CARTESIAN_POINT ( 'NONE',  ( 11.99999999999999822, -59.46389618801929089, -49.70050353004953081 ) ) ;
#1846 = CARTESIAN_POINT ( 'NONE',  ( -7.500000000000015099, -73.00000000000001421, -204.9999999999999716 ) ) ;
#1847 = DIRECTION ( 'NONE',  ( 0.5200609990132993854, 0.8541291221503275466, -0.000000000000000000 ) ) ;
#1848 = CARTESIAN_POINT ( 'NONE',  ( 95.00000000002596323, -209.9999999999999147, -64.99999999999349143 ) ) ;
#1849 = EDGE_CURVE ( 'NONE', #15455, #32135, #60896, .T. ) ;
#1850 = DIRECTION ( 'NONE',  ( -1.000000000000000000, 0.000000000000000000, 0.000000000000000000 ) ) ;
#1851 = CARTESIAN_POINT ( 'NONE',  ( -35.37301231164799731, -123.0000000000000142, 2.500000000000000000 ) ) ;
#1852 = EDGE_CURVE ( 'NONE', #588, #49792, #56478, .T. ) ;
#1853 =( BOUNDED_CURVE ( )  B_SPLINE_CURVE ( 2, ( #56734, #57097, #61995, #5234, #68384, #362, #28133 ),
 .UNSPECIFIED., .F., .F. ) 
 B_SPLINE_CURVE_WITH_KNOTS ( ( 3, 2, 2, 3 ),
 ( 0.7708333333333328152, 0.7777777777777775681, 0.7847222222222222099, 0.7916666666666669627 ),
 .UNSPECIFIED. ) 
 CURVE ( )  GEOMETRIC_REPRESENTATION_ITEM ( )  RATIONAL_B_SPLINE_CURVE ( ( 1.000000000000010658, 0.8660254037844280495, 1.000000000000000000, 0.8660254037844387076, 1.000000000000000000, 0.8660254037844322683, 1.000000000000006439 ) ) 
 REPRESENTATION_ITEM ( '' )  );
#1854 = EDGE_CURVE ( 'NONE', #52969, #23763, #14079, .T. ) ;
#1855 = CARTESIAN_POINT ( 'NONE',  ( 10.00000000000000000, -22.64427369931191336, 30.00120703465197280 ) ) ;
#1856 = TOROIDAL_SURFACE ( 'NONE', #35462, 3.250000000000001332, 0.2500000000000000000 ) ;
#1857 = CARTESIAN_POINT ( 'NONE',  ( -1.250000000000000444, -16.78109714094927085, -1.199999999999999956 ) ) ;
#1858 = VERTEX_POINT ( 'NONE', #51184 ) ;
#1859 = CARTESIAN_POINT ( 'NONE',  ( -96.15314808468751551, 88.00268892867056536, 87.20864583420046756 ) ) ;
#1860 = CARTESIAN_POINT ( 'NONE',  ( 10.00000000000000000, 72.35160999960817207, 20.41045688087850607 ) ) ;
#1861 = AXIS2_PLACEMENT_3D ( 'NONE', #8469, #42316, #64498 ) ;
#1862 = DIRECTION ( 'NONE',  ( 0.000000000000000000, 0.000000000000000000, 1.000000000000000000 ) ) ;
#1863 = VERTEX_POINT ( 'NONE', #4982 ) ;
#1864 = CARTESIAN_POINT ( 'NONE',  ( 0.000000000000000000, -16.65560815589383381, -38.55633173627028754 ) ) ;
#1865 = DIRECTION ( 'NONE',  ( -1.000000000000000000, 0.000000000000000000, 0.000000000000000000 ) ) ;
#1866 = CARTESIAN_POINT ( 'NONE',  ( 2.369999999999999662, 4.749999999999999112, 0.000000000000000000 ) ) ;
#1867 = DIRECTION ( 'NONE',  ( -1.000000000000000000, 0.000000000000000000, -0.000000000000000000 ) ) ;
#1868 = CIRCLE ( 'NONE', #11433, 77.49899999999998101 ) ;
#1869 = CARTESIAN_POINT ( 'NONE',  ( 96.15314808468748708, -208.0026889286704943, 81.96989583420048575 ) ) ;
#1870 = VERTEX_POINT ( 'NONE', #51564 ) ;
#1871 = ORIENTED_EDGE ( 'NONE', *, *, #11857, .F. ) ;
#1872 = ADVANCED_FACE ( 'NONE', ( #62495 ), #10974, .T. ) ;
#1873 = DIRECTION ( 'NONE',  ( -0.000000000000000000, -0.000000000000000000, -1.000000000000000000 ) ) ;
#1874 = ORIENTED_EDGE ( 'NONE', *, *, #17594, .F. ) ;
#1875 = CARTESIAN_POINT ( 'NONE',  ( 92.35000000000000853, -209.9999999999999716, 88.73000000000000398 ) ) ;
#1876 = CARTESIAN_POINT ( 'NONE',  ( 92.69370383062501162, -208.6684592857803295, 76.25489583420049655 ) ) ;
#1877 = AXIS2_PLACEMENT_3D ( 'NONE', #45743, #47200, #70113 ) ;
#1878 = ORIENTED_EDGE ( 'NONE', *, *, #4867, .T. ) ;
#1879 = CIRCLE ( 'NONE', #16226, 26.50000000000552092 ) ;
#1880 = CARTESIAN_POINT ( 'NONE',  ( 95.00000000000000000, -212.6630814284392557, 79.80031250086715033 ) ) ;
#1881 = ORIENTED_EDGE ( 'NONE', *, *, #2771, .F. ) ;
#1882 = LINE ( 'NONE', #8596, #69536 ) ;
#1883 = ORIENTED_EDGE ( 'NONE', *, *, #40336, .T. ) ;
#1884 = CIRCLE ( 'NONE', #53482, 31.99999999999999289 ) ;
#1885 = EDGE_LOOP ( 'NONE', ( #9049, #54453, #6920, #47224 ) ) ;
#1886 = CARTESIAN_POINT ( 'NONE',  ( 97.65000000000000568, -208.4700217866474645, 86.63979166840096013 ) ) ;
#1887 = DIRECTION ( 'NONE',  ( 0.000000000000000000, -0.1564344650402381687, 0.9876883405951365491 ) ) ;
#1888 = ADVANCED_FACE ( 'NONE', ( #34637 ), #56842, .F. ) ;
#1889 = ORIENTED_EDGE ( 'NONE', *, *, #3175, .T. ) ;
#1890 = LINE ( 'NONE', #47346, #22174 ) ;
#1891 = CARTESIAN_POINT ( 'NONE',  ( 93.67500000000001137, -207.7050326799711968, 83.62354166840097491 ) ) ;
#1892 = CARTESIAN_POINT ( 'NONE',  ( 94.99999999999998579, 93.05995642670504253, 89.20624999999999716 ) ) ;
#1893 = EDGE_CURVE ( 'NONE', #8568, #25521, #46500, .T. ) ;
#1894 = ORIENTED_EDGE ( 'NONE', *, *, #44039, .F. ) ;
#1895 = FACE_OUTER_BOUND ( 'NONE', #3899, .T. ) ;
#1896 = CARTESIAN_POINT ( 'NONE',  ( 11.99999999999999822, 77.16300072079698680, -27.74655509720590629 ) ) ;
#1897 = APPLICATION_CONTEXT ( 'automotive_design' ) ;
#1898 = ORIENTED_EDGE ( 'NONE', *, *, #35296, .F. ) ;
#1899 = ORIENTED_EDGE ( 'NONE', *, *, #7386, .T. ) ;
#1900 = CARTESIAN_POINT ( 'NONE',  ( -92.69370383062505425, 88.66845928578038638, 89.43114583420049257 ) ) ;
#1901 = CARTESIAN_POINT ( 'NONE',  ( 94.99999999999998579, 87.33691857156068750, 84.08656250086713158 ) ) ;
#1902 = ORIENTED_EDGE ( 'NONE', *, *, #53163, .T. ) ;
#1903 = CIRCLE ( 'NONE', #18644, 15.39727592589476579 ) ;
#1904 = CARTESIAN_POINT ( 'NONE',  ( 96.32499999999998863, 87.70503267997126784, 87.11604166840096752 ) ) ;
#1905 = EDGE_CURVE ( 'NONE', #70889, #60073, #66898, .T. ) ;
#1906 = EDGE_CURVE ( 'NONE', #31995, #22414, #45941, .T. ) ;
#1907 = ORIENTED_EDGE ( 'NONE', *, *, #16647, .T. ) ;
#1908 = FACE_BOUND ( 'NONE', #36354, .T. ) ;
#1909 = DIRECTION ( 'NONE',  ( -0.6862798483830533369, -0.7273375899149812085, 0.000000000000000000 ) ) ;
#1910 = EDGE_LOOP ( 'NONE', ( #3819, #45720, #14057, #17027 ) ) ;
#1911 = ORIENTED_EDGE ( 'NONE', *, *, #47294, .F. ) ;
#1912 = CIRCLE ( 'NONE', #61934, 31.99999999999998934 ) ;
#1913 = ORIENTED_EDGE ( 'NONE', *, *, #2534, .F. ) ;
#1914 = DIRECTION ( 'NONE',  ( 0.000000000000000000, -1.000000000000000000, 0.000000000000000000 ) ) ;
#1915 = CARTESIAN_POINT ( 'NONE',  ( 92.34999999999999432, 91.52997821335252127, 75.42145833506764063 ) ) ;
#1916 = CARTESIAN_POINT ( 'NONE',  ( -97.65000000000001990, 88.47002178664754979, 84.97291666666666288 ) ) ;
#1917 = EDGE_LOOP ( 'NONE', ( #19140, #20873 ) ) ;
#1918 = CARTESIAN_POINT ( 'NONE',  ( 11.99999999999999822, 74.65374052328648702, 8.840884882375350529 ) ) ;
#1919 = DIRECTION ( 'NONE',  ( 1.000000000000000000, 0.000000000000000000, 0.000000000000000000 ) ) ;
#1920 = ORIENTED_EDGE ( 'NONE', *, *, #51945, .T. ) ;
#1921 = FACE_OUTER_BOUND ( 'NONE', #49565, .T. ) ;
#1922 = CARTESIAN_POINT ( 'NONE',  ( -96.15314808468747287, -208.0026889286704943, 83.82197916753381151 ) ) ;
#1923 = ORIENTED_EDGE ( 'NONE', *, *, #36567, .F. ) ;
#1925 = EDGE_CURVE ( 'NONE', #38652, #27167, #17350, .T. ) ;
#1924 = DIRECTION ( 'NONE',  ( -1.000000000000000000, -0.000000000000000000, 0.000000000000000000 ) ) ;
#1926 = DIRECTION ( 'NONE',  ( -1.000000000000000000, -0.000000000000000000, 0.000000000000000000 ) ) ;
#1927 = CARTESIAN_POINT ( 'NONE',  ( -92.35000000000003695, 90.00000000000004263, 90.00000000000000000 ) ) ;
#1928 = DIRECTION ( 'NONE',  ( -1.000000000000000000, 0.000000000000000000, 0.000000000000000000 ) ) ;
#1929 = CARTESIAN_POINT ( 'NONE',  ( 97.64999999999447766, 89.99999459739470353, 81.50687481489491404 ) ) ;
#1930 = DIRECTION ( 'NONE',  ( 0.000000000000000000, 0.4539904997395414754, 0.8910065241883706744 ) ) ;
#1931 = CARTESIAN_POINT ( 'NONE',  ( -0.8815729230226008184, -93.47222532549339746, 5.500000000000000000 ) ) ;
#1932 = LINE ( 'NONE', #66533, #72366 ) ;
#1933 = CARTESIAN_POINT ( 'NONE',  ( 0.000000000000000000, -70.52718814184277107, 26.02418014898285037 ) ) ;
#1934 = DIRECTION ( 'NONE',  ( -1.000000000000000000, 0.000000000000000000, 0.000000000000000000 ) ) ;
#1935 = EDGE_CURVE ( 'NONE', #54478, #45, #11693, .T. ) ;
#1936 = EDGE_CURVE ( 'NONE', #52599, #67382, #12842, .T. ) ;
#1937 = CARTESIAN_POINT ( 'NONE',  ( -92.69370383062504004, 90.00000000000004263, 89.48406250086715374 ) ) ;
#1938 = FACE_OUTER_BOUND ( 'NONE', #41703, .T. ) ;
#1939 = CARTESIAN_POINT ( 'NONE',  ( -18.12185313557660038, -104.9634299478706794, 5.500000000000000000 ) ) ;
#1940 = ADVANCED_FACE ( 'NONE', ( #845 ), #22253, .F. ) ;
#1941 = TOROIDAL_SURFACE ( 'NONE', #16270, 57.50000000000000000, 5.000000000000000000 ) ;
#1942 = DIRECTION ( 'NONE',  ( 0.000000000000000000, 0.000000000000000000, 1.000000000000000000 ) ) ;
#1944 = DIRECTION ( 'NONE',  ( -7.685483754327489091E-16, -1.065814103640131188E-14, -1.000000000000000000 ) ) ;
#1943 = VECTOR ( 'NONE', #31711, 1000.000000000000000 ) ;
#1945 = CARTESIAN_POINT ( 'NONE',  ( 0.000000000000000000, 0.000000000000000000, 0.000000000000000000 ) ) ;
#1946 = DIRECTION ( 'NONE',  ( 1.000000000000000000, 0.000000000000000000, 0.000000000000000000 ) ) ;
#1947 = DIRECTION ( 'NONE',  ( -1.000000000000000000, -0.000000000000000000, -0.000000000000000000 ) ) ;
#1948 = AXIS2_PLACEMENT_3D ( 'NONE', #24843, #15317, #26966 ) ;
#1949 = DIRECTION ( 'NONE',  ( -1.000000000000000000, 0.000000000000000000, 0.000000000000000000 ) ) ;
#1950 = CARTESIAN_POINT ( 'NONE',  ( -96.15314808468747287, -208.0026889286704943, 76.36072916753381890 ) ) ;
#1951 = AXIS2_PLACEMENT_3D ( 'NONE', #58393, #74203, #557 ) ;
#1952 = CARTESIAN_POINT ( 'NONE',  ( -31.74999999999995737, 0.000000000000000000, 5.000000000000000000 ) ) ;
#1953 = CIRCLE ( 'NONE', #48702, 13.36666666666666536 ) ;
#1954 = AXIS2_PLACEMENT_3D ( 'NONE', #53481, #47472, #13254 ) ;
#1955 = ORIENTED_EDGE ( 'NONE', *, *, #41345, .F. ) ;
#1956 = CARTESIAN_POINT ( 'NONE',  ( -22.67106064244953245, -113.6342314410295842, 2.500000000000000000 ) ) ;
#1957 = LINE ( 'NONE', #24475, #11872 ) ;
#1958 = CARTESIAN_POINT ( 'NONE',  ( 0.000000000000000000, -10.45096189432344147, 21.10159698893425784 ) ) ;
#1959 = EDGE_LOOP ( 'NONE', ( #56725, #22128, #74154, #73797 ) ) ;
#1960 = CARTESIAN_POINT ( 'NONE',  ( -3.000000000000000000, 23.50000000000000000, 1.499999999999997780 ) ) ;
#1961 = CARTESIAN_POINT ( 'NONE',  ( 0.000000000000000000, 74.74816331893477184, -33.71516098798660011 ) ) ;
#1962 = ORIENTED_EDGE ( 'NONE', *, *, #51424, .T. ) ;
#1963 = EDGE_CURVE ( 'NONE', #16556, #59396, #47406, .T. ) ;
#1964 = CARTESIAN_POINT ( 'NONE',  ( 93.84685191531251292, -211.9973110713294489, 86.57364583420047666 ) ) ;
#1965 = CARTESIAN_POINT ( 'NONE',  ( 92.69370383062501162, -208.6684592857803295, 89.74864583420048803 ) ) ;
#1966 = VERTEX_POINT ( 'NONE', #2696 ) ;
#1967 = ADVANCED_FACE ( 'NONE', ( #36117 ), #41392, .F. ) ;
#1968 = DIRECTION ( 'NONE',  ( -1.000000000000000000, -0.000000000000000000, -0.000000000000000000 ) ) ;
#1969 = ORIENTED_EDGE ( 'NONE', *, *, #5881, .F. ) ;
#1970 = CARTESIAN_POINT ( 'NONE',  ( -92.34999999999999432, -209.9999999999999716, 80.79249999999998977 ) ) ;
#1971 = ORIENTED_EDGE ( 'NONE', *, *, #69410, .T. ) ;
#1972 = CARTESIAN_POINT ( 'NONE',  ( -92.69370383062504004, 90.00000000000004263, 81.22906250086715829 ) ) ;
#1973 = EDGE_CURVE ( 'NONE', #17553, #64952, #13551, .T. ) ;
#1974 = VERTEX_POINT ( 'NONE', #19559 ) ;
#1975 = ORIENTED_EDGE ( 'NONE', *, *, #24507, .T. ) ;
#1976 = DIRECTION ( 'NONE',  ( -1.000000000000000000, -0.000000000000000000, -0.000000000000000000 ) ) ;
#1977 = ADVANCED_FACE ( 'NONE', ( #41753 ), #7186, .T. ) ;
#1978 = ORIENTED_EDGE ( 'NONE', *, *, #60682, .T. ) ;
#1979 = CARTESIAN_POINT ( 'NONE',  ( 0.000000000000000000, -21.40280677340398086, 36.13751322684410638 ) ) ;
#1980 = ORIENTED_EDGE ( 'NONE', *, *, #50845, .F. ) ;
#1981 = DIRECTION ( 'NONE',  ( 0.000000000000000000, 0.000000000000000000, -1.000000000000000000 ) ) ;
#1982 = ORIENTED_EDGE ( 'NONE', *, *, #9744, .F. ) ;
#1983 = CARTESIAN_POINT ( 'NONE',  ( 12.49999999999999645, 1.530808498934191127E-15, -125.0000000000000000 ) ) ;
#1984 = AXIS2_PLACEMENT_3D ( 'NONE', #62555, #51246, #68559 ) ;
#1985 = ORIENTED_EDGE ( 'NONE', *, *, #55925, .F. ) ;
#1986 = ADVANCED_FACE ( 'NONE', ( #71421 ), #24117, .F. ) ;
#1987 = ORIENTED_EDGE ( 'NONE', *, *, #10454, .T. ) ;
#1988 = VERTEX_POINT ( 'NONE', #47042 ) ;
#1989 = CARTESIAN_POINT ( 'NONE',  ( 95.00000000000000000, -207.3369185715606307, 79.95906250086713385 ) ) ;
#1990 = DIRECTION ( 'NONE',  ( 0.000000000000000000, 0.9876883405951383255, -0.1564344650402277048 ) ) ;
#1991 = CONTEXT_DEPENDENT_SHAPE_REPRESENTATION ( #4736, #65566 ) ;
#1992 = DIRECTION ( 'NONE',  ( 1.000000000000000000, 1.427937372958405461E-15, 7.962523111839130290E-16 ) ) ;
#1993 = LINE ( 'NONE', #8337, #11259 ) ;
#1994 = VECTOR ( 'NONE', #52722, 1000.000000000000000 ) ;
#1995 = CARTESIAN_POINT ( 'NONE',  ( 11.99999999999999822, 0.000000000000000000, 0.000000000000000000 ) ) ;
#1996 = DIRECTION ( 'NONE',  ( -1.000000000000000000, 0.000000000000000000, 0.000000000000000000 ) ) ;
#1997 = VECTOR ( 'NONE', #73274, 1000.000000000000000 ) ;
#1998 = CARTESIAN_POINT ( 'NONE',  ( 11.99999999999999822, 0.000000000000000000, 0.000000000000000000 ) ) ;
#1999 = DIRECTION ( 'NONE',  ( 0.000000000000000000, -0.000000000000000000, 1.000000000000000000 ) ) ;
#2000 = CARTESIAN_POINT ( 'NONE',  ( -94.99999999999997158, -212.6630814284392557, 80.27656250086714351 ) ) ;
#2001 = CARTESIAN_POINT ( 'NONE',  ( -95.00000000000002842, 87.33691857156074434, 80.43531250086715545 ) ) ;
#2002 = ORIENTED_EDGE ( 'NONE', *, *, #69178, .T. ) ;
#2003 = AXIS2_PLACEMENT_3D ( 'NONE', #29705, #11677, #35720 ) ;
#2004 = EDGE_CURVE ( 'NONE', #59025, #67396, #36886, .T. ) ;
#2005 = CARTESIAN_POINT ( 'NONE',  ( 97.30629616937498838, 90.00000000000002842, 82.34031250086714238 ) ) ;
#2006 = AXIS2_PLACEMENT_3D ( 'NONE', #58291, #57566, #19172 ) ;
#2007 = ORIENTED_EDGE ( 'NONE', *, *, #24640, .F. ) ;
#2008 = CARTESIAN_POINT ( 'NONE',  ( 15.00000000000000000, 26.49999999999999645, 1.499999999999995781 ) ) ;
#2009 = DIRECTION ( 'NONE',  ( -1.000000000000000000, 0.000000000000000000, 0.000000000000000000 ) ) ;
#2011 = EDGE_CURVE ( 'NONE', #44097, #4558, #30834, .T. ) ;
#2010 = CYLINDRICAL_SURFACE ( 'NONE', #31399, 77.49899999999999523 ) ;
#2012 = FACE_OUTER_BOUND ( 'NONE', #10594, .T. ) ;
#2013 = CARTESIAN_POINT ( 'NONE',  ( 11.99999999999999822, 8.840884882376133902, -74.65374052328640175 ) ) ;
#2014 = CARTESIAN_POINT ( 'NONE',  ( -94.99999999999997158, -207.3369185715606307, 82.49906250086715431 ) ) ;
#2015 = DIRECTION ( 'NONE',  ( -0.7585478161175716050, -0.6516173805718067369, 0.000000000000000000 ) ) ;
#2016 = LINE ( 'NONE', #24903, #46301 ) ;
#2017 = EDGE_CURVE ( 'NONE', #24699, #18969, #8786, .T. ) ;
#2018 = DIRECTION ( 'NONE',  ( -1.000000000000000000, 0.000000000000000000, 0.000000000000000000 ) ) ;
#2019 = ORIENTED_EDGE ( 'NONE', *, *, #57120, .F. ) ;
#2020 = AXIS2_PLACEMENT_3D ( 'NONE', #21412, #62039, #10146 ) ;
#2021 = EDGE_LOOP ( 'NONE', ( #17016, #33841, #35931, #24776 ) ) ;
#2022 = CYLINDRICAL_SURFACE ( 'NONE', #15656, 16.00000000000000000 ) ;
#2023 = CARTESIAN_POINT ( 'NONE',  ( 0.000000000000000000, 3.925862922256769583, -41.81611651403857621 ) ) ;
#2024 = CARTESIAN_POINT ( 'NONE',  ( 0.000000000000000000, 0.000000000000000000, -4.400000000000001243 ) ) ;
#2025 = EDGE_CURVE ( 'NONE', #36317, #26097, #34984, .T. ) ;
#2026 = CARTESIAN_POINT ( 'NONE',  ( -95.00000000000002842, 87.33691857156074434, 85.99156250086714692 ) ) ;
#2027 = CARTESIAN_POINT ( 'NONE',  ( 0.000000000000000000, 35.95386929396256903, -10.96151621346501237 ) ) ;
#2028 = CARTESIAN_POINT ( 'NONE',  ( 11.99999999999999822, 0.000000000000000000, 0.000000000000000000 ) ) ;
#2029 = CARTESIAN_POINT ( 'NONE',  ( -23.30023580412278505, -123.4057321492263384, 5.500000000000000000 ) ) ;
#2030 = DIRECTION ( 'NONE',  ( -1.000000000000000000, 0.000000000000000000, 0.000000000000000000 ) ) ;
#2031 = ORIENTED_EDGE ( 'NONE', *, *, #62393, .T. ) ;
#2032 = CARTESIAN_POINT ( 'NONE',  ( -97.30629616937501680, 90.00000000000004263, 75.67281250086713840 ) ) ;
#2033 = EDGE_CURVE ( 'NONE', #48200, #185, #64699, .T. ) ;
#2034 = CARTESIAN_POINT ( 'NONE',  ( 10.00000000000000000, -40.98264845739755913, 9.188173127307164734 ) ) ;
#2035 = CLOSED_SHELL ( 'NONE', ( #30843, #53299, #302, #25026, #60112, #57640, #40573, #22486, #44929, #51198, #42095, #58290, #61829, #7482, #45373, #47263, #49888, #8489, #25397, #17549, #53469, #11560, #6297, #37604, #32650, #6641, #53402, #33495, #63872, #73659, #3012 ) ) ;
#2036 = CARTESIAN_POINT ( 'NONE',  ( 5.999999999999999112, 27.74655509720669500, 77.16300072079670258 ) ) ;
#2037 = DIRECTION ( 'NONE',  ( 0.000000000000000000, -0.5877852522924802425, 0.8090169943749422332 ) ) ;
#2038 = DIRECTION ( 'NONE',  ( 0.000000000000000000, -0.4539904997395542430, 0.8910065241883641241 ) ) ;
#2039 = CARTESIAN_POINT ( 'NONE',  ( -93.84685191531248449, -208.0026889286704943, 86.41489583420049314 ) ) ;
#2040 = FILL_AREA_STYLE_COLOUR ( '', #49372 ) ;
#2041 = DIRECTION ( 'NONE',  ( 0.000000000000000000, 0.000000000000000000, 1.000000000000000000 ) ) ;
#2042 = AXIS2_PLACEMENT_3D ( 'NONE', #16207, #62085, #56819 ) ;
#2043 = CARTESIAN_POINT ( 'NONE',  ( -11.59517495878806947, -96.12423995607481686, 5.500000000000000000 ) ) ;
#2044 = CARTESIAN_POINT ( 'NONE',  ( -96.15314808468747287, -208.0026889286704943, 76.36072916753381890 ) ) ;
#2045 = FACE_OUTER_BOUND ( 'NONE', #57394, .T. ) ;
#2046 = CIRCLE ( 'NONE', #15204, 15.99999999999999822 ) ;
#2047 = ORIENTED_EDGE ( 'NONE', *, *, #70798, .F. ) ;
#2048 = CARTESIAN_POINT ( 'NONE',  ( -97.64999999999996305, -209.9999999999999716, 81.82437500173429612 ) ) ;
#2049 = CARTESIAN_POINT ( 'NONE',  ( 92.34999999999990905, 91.52997821335249284, 75.97708333333333997 ) ) ;
#2050 = CARTESIAN_POINT ( 'NONE',  ( 97.64999999999990621, 90.00000071509185773, 85.31687502647973531 ) ) ;
#2051 = AXIS2_PLACEMENT_3D ( 'NONE', #54225, #53109, #30897 ) ;
#2052 = AXIS2_PLACEMENT_3D ( 'NONE', #46814, #30245, #13325 ) ;
#2053 = DIRECTION ( 'NONE',  ( -1.000000000000000000, 0.000000000000000000, -0.000000000000000000 ) ) ;
#2054 = CARTESIAN_POINT ( 'NONE',  ( 96.15314808468750130, -211.9973110713294489, 76.51947916753380241 ) ) ;
#2055 = VERTEX_POINT ( 'NONE', #19197 ) ;
#2056 = AXIS2_PLACEMENT_3D ( 'NONE', #16139, #55245, #56751 ) ;
#2057 = CARTESIAN_POINT ( 'NONE',  ( 10.00000000000000000, 0.000000000000000000, 0.000000000000000000 ) ) ;
#2058 = LINE ( 'NONE', #46780, #39113 ) ;
#2059 = VERTEX_POINT ( 'NONE', #1584 ) ;
#2060 =( BOUNDED_CURVE ( )  B_SPLINE_CURVE ( 2, ( #61830, #44538, #55436, #21584, #72349, #38141, #38891 ),
 .UNSPECIFIED., .F., .F. ) 
 B_SPLINE_CURVE_WITH_KNOTS ( ( 3, 2, 2, 3 ),
 ( 0.2708333333333337034, 0.2777777777777781232, 0.2847222222222224874, 0.2916666666666669072 ),
 .UNSPECIFIED. ) 
 CURVE ( )  GEOMETRIC_REPRESENTATION_ITEM ( )  RATIONAL_B_SPLINE_CURVE ( ( 0.9999999999999924505, 0.8660254037844462571, 1.000000000000000000, 0.8660254037844387076, 1.000000000000000000, 0.8660254037844343777, 1.000000000000004219 ) ) 
 REPRESENTATION_ITEM ( '' )  );
#2061 = DIRECTION ( 'NONE',  ( -1.000000000000000000, -0.000000000000000000, 0.000000000000000000 ) ) ;
#2062 = VERTEX_POINT ( 'NONE', #7916 ) ;
#2063 = ADVANCED_FACE ( 'NONE', ( #53774 ), #58313, .T. ) ;
#2064 = DIRECTION ( 'NONE',  ( -0.000000000000000000, 0.000000000000000000, 1.000000000000000000 ) ) ;
#2065 = EDGE_CURVE ( 'NONE', #35604, #57809, #19361, .T. ) ;
#2066 = AXIS2_PLACEMENT_3D ( 'NONE', #35214, #70515, #46880 ) ;
#2067 = ORIENTED_EDGE ( 'NONE', *, *, #74116, .F. ) ;
#2068 = ORIENTED_EDGE ( 'NONE', *, *, #40560, .T. ) ;
#2070 = ORIENTED_EDGE ( 'NONE', *, *, #1144, .T. ) ;
#2069 = ADVANCED_FACE ( 'NONE', ( #30464 ), #53413, .F. ) ;
#2071 = FACE_OUTER_BOUND ( 'NONE', #69092, .T. ) ;
#2072 = AXIS2_PLACEMENT_3D ( 'NONE', #41054, #53068, #59448 ) ;
#2073 = ORIENTED_EDGE ( 'NONE', *, *, #17898, .F. ) ;
#2074 = ORIENTED_EDGE ( 'NONE', *, *, #59970, .F. ) ;
#2075 = CARTESIAN_POINT ( 'NONE',  ( 93.84685191531248449, 91.99731107132950569, 80.17072916753382117 ) ) ;
#2076 = CARTESIAN_POINT ( 'NONE',  ( 97.64999999964365429, -210.0000434577794408, 89.12687334326047051 ) ) ;
#2077 = FACE_OUTER_BOUND ( 'NONE', #32273, .T. ) ;
#2078 = EDGE_LOOP ( 'NONE', ( #30248, #40135, #17651, #51121 ) ) ;
#2079 = EDGE_LOOP ( 'NONE', ( #37265, #53284, #7770, #56109, #46056, #15253, #7415, #10741, #69066, #67673, #71670, #46050, #43374, #4538, #44452, #24396, #18336, #73012, #54371, #51399, #946, #46681, #68084, #73961, #4087, #66512, #46789, #442, #49864, #6338, #14821, #27894, #59131, #432, #15444, #38036, #48524, #49811, #63474, #26894, #25539, #17845, #43872, #29144, #71066, #17562, #35576, #67128, #57657, #23744, #3378, #27674, #18021, #12442, #12234, #3800, #9150, #54194, #59427, #56072, #40987, #68664, #2358, #43484, #43759, #58285, #28502, #45416, #50992, #35661, #60771, #19743, #55794, #65399, #27890, #56212, #61400, #4556, #50837, #70109, #44689, #37173, #24917, #59550, #37282, #28651, #19231, #47601, #15000, #38098, #58513, #68055, #25251, #28373, #46599, #22576, #42531, #434, #61779, #54813, #15266, #65561, #60486, #57251, #47705, #38090, #29757, #57667, #11073, #58859, #13621, #69004, #12022, #36213, #43798, #4217, #12655, #12756, #59190, #66801, #57240, #69, #27134, #14994, #59249, #53333, #3893, #36726, #49288, #60840, #8035, #55465, #28404, #46044, #41631, #56160, #41586, #19582, #40971, #48923, #50114, #19983, #52635, #21752, #26907, #42618, #14236, #4628, #70848, #19527, #53743, #31439, #27462, #58998, #45908, #13024, #39879, #44558, #5199, #64715, #12833, #59645, #6645, #69283, #61104, #19061, #67994, #58092, #69652, #17365, #23244, #7017, #61219, #40804, #20997, #6960, #50190, #27147, #26043, #9876, #40576, #55946, #5829, #3628, #8856, #69190, #49898, #46136, #4193, #38210, #27379, #33074, #3069, #20694, #12572, #33160, #54472, #52174, #18776, #60471, #17004, #61129, #37492, #40499, #10851, #35171, #24709, #55275, #67502, #31918, #47791, #60656, #31793, #64921, #33681, #51892, #69801, #52506, #45648, #23160, #56813, #44086, #55599, #28465, #13559, #66348, #10591, #7570, #23479, #1693, #53517, #72106, #53887, #68456, #13610, #70420, #51126, #30172, #67862, #55827, #28964, #62255, #66294, #58609, #14227, #22808, #12046, #11367, #36690, #13984, #23449, #34423, #73489, #34949, #71550, #1710, #36056, #38083, #59841, #2854, #12904, #35959, #3430, #23148, #39877, #2451, #28847, #30330, #43656, #71342, #22655, #64837, #19482, #9119, #48455, #72782, #74066, #42116, #1955, #61141, #14073, #63269, #69262, #14424, #38840, #40585, #68237, #59308, #43235, #30506, #55448, #24906, #15408, #2463, #57876, #68064, #39870, #34815, #47962, #73863, #7779, #15569, #46416, #788, #21760, #71920, #44402, #27819, #48821, #33205, #18682, #52998, #68888, #47792, #40908, #40238, #7749, #45807, #59379, #46984, #24077, #67036, #74172, #16112, #5862 ) ) ;
#2080 = VERTEX_POINT ( 'NONE', #31216 ) ;
#2081 = DIRECTION ( 'NONE',  ( 0.000000000000000000, -1.000000000000000000, -1.040834085586084257E-14 ) ) ;
#2082 = ORIENTED_EDGE ( 'NONE', *, *, #60638, .T. ) ;
#2083 = DIRECTION ( 'NONE',  ( 1.000000000000000000, 0.000000000000000000, 0.000000000000000000 ) ) ;
#2084 = CARTESIAN_POINT ( 'NONE',  ( 0.6180191030787338669, -93.50720753887522108, -2.500000000000000000 ) ) ;
#2085 = CARTESIAN_POINT ( 'NONE',  ( 11.99999999999999822, 30.41916302227216562, -71.27951684757994144 ) ) ;
#2086 = CARTESIAN_POINT ( 'NONE',  ( 10.00000000000000000, -54.21277698773715059, 55.38113227695762930 ) ) ;
#2087 = FACE_OUTER_BOUND ( 'NONE', #66940, .T. ) ;
#2088 = DIRECTION ( 'NONE',  ( 1.000000000000000000, 0.000000000000000000, 0.000000000000000000 ) ) ;
#2089 = EDGE_CURVE ( 'NONE', #65194, #3728, #37418, .T. ) ;
#2090 = CARTESIAN_POINT ( 'NONE',  ( -3.000000000000000000, 8.688484142254221609, -21.88630264137359660 ) ) ;
#2091 = CARTESIAN_POINT ( 'NONE',  ( -97.64999999999996305, -209.9999999999999716, 80.55437500173430010 ) ) ;
#2092 = CARTESIAN_POINT ( 'NONE',  ( 0.000000000000000000, -25.60904388321925396, 6.976881207771170601 ) ) ;
#2094 = CARTESIAN_POINT ( 'NONE',  ( -93.67500000000003979, 92.29496732002878900, 74.62770833506762358 ) ) ;
#2093 = CARTESIAN_POINT ( 'NONE',  ( 94.99999999999998579, 93.05995642670504253, 75.95062500173428077 ) ) ;
#2095 = ORIENTED_EDGE ( 'NONE', *, *, #69495, .F. ) ;
#2096 = CARTESIAN_POINT ( 'NONE',  ( 92.69370383062498320, 91.33154071421968467, 75.14364583420049826 ) ) ;
#2097 = CIRCLE ( 'NONE', #858, 16.00000000000000000 ) ;
#2098 = FACE_OUTER_BOUND ( 'NONE', #23322, .T. ) ;
#2099 = CARTESIAN_POINT ( 'NONE',  ( 10.00000000000000000, 0.8828120875900632436, 37.48860685352291000 ) ) ;
#2100 = CARTESIAN_POINT ( 'NONE',  ( 10.00000000000000000, 21.32104025579158701, -30.84782396557194772 ) ) ;
#2101 = CARTESIAN_POINT ( 'NONE',  ( -24.94940289813038703, -237.3777120880567963, 5.500000000000000000 ) ) ;
#2102 = VECTOR ( 'NONE', #50687, 1000.000000000000000 ) ;
#2103 = CYLINDRICAL_SURFACE ( 'NONE', #73824, 2.500000000000000000 ) ;
#2104 = VERTEX_POINT ( 'NONE', #71791 ) ;
#2105 = FACE_OUTER_BOUND ( 'NONE', #23044, .T. ) ;
#2106 = ADVANCED_FACE ( 'NONE', ( #27417 ), #21785, .T. ) ;
#2107 = EDGE_CURVE ( 'NONE', #22856, #34880, #48875, .T. ) ;
#2108 = LINE ( 'NONE', #47928, #14368 ) ;
#2109 = ORIENTED_EDGE ( 'NONE', *, *, #41746, .F. ) ;
#2110 = AXIS2_PLACEMENT_3D ( 'NONE', #38774, #4210, #10194 ) ;
#2111 = ORIENTED_EDGE ( 'NONE', *, *, #67660, .T. ) ;
#2112 = CIRCLE ( 'NONE', #74075, 15.99999999999999822 ) ;
#2113 = EDGE_CURVE ( 'NONE', #8769, #59758, #72169, .T. ) ;
#2114 = DIRECTION ( 'NONE',  ( 0.000000000000000000, 0.000000000000000000, 1.000000000000000000 ) ) ;
#2115 = PLANE ( 'NONE',  #73532 ) ;
#2116 = VECTOR ( 'NONE', #18095, 1000.000000000000000 ) ;
#2117 = DIRECTION ( 'NONE',  ( 1.000000000000000000, 1.427937372958405461E-15, 7.962523111839130290E-16 ) ) ;
#2118 = CARTESIAN_POINT ( 'NONE',  ( -93.67499999999998295, -207.7050326799711968, 75.81833333333332803 ) ) ;
#2119 = CARTESIAN_POINT ( 'NONE',  ( -92.69370383062498320, -209.9999999999999716, 76.78406250086715090 ) ) ;
#2120 = VERTEX_POINT ( 'NONE', #32682 ) ;
#2121 = DIRECTION ( 'NONE',  ( -1.000000000000000000, 0.000000000000000000, 0.000000000000000000 ) ) ;
#2122 = CARTESIAN_POINT ( 'NONE',  ( 0.000000000000000000, -62.50884508063395373, -41.76106447765554464 ) ) ;
#2123 = VECTOR ( 'NONE', #44670, 1000.000000000000000 ) ;
#2124 = PRESENTATION_STYLE_ASSIGNMENT (( #17159 ) ) ;
#2125 = LINE ( 'NONE', #31011, #56050 ) ;
#2126 = DIRECTION ( 'NONE',  ( -1.000000000000000000, 0.000000000000000000, 0.000000000000000000 ) ) ;
#2127 = DIRECTION ( 'NONE',  ( -1.000000000000000000, 0.000000000000000000, -0.000000000000000000 ) ) ;
#2128 = LINE ( 'NONE', #12254, #7315 ) ;
#2129 = CARTESIAN_POINT ( 'NONE',  ( -10.00000000000000000, 0.000000000000000000, 0.000000000000000000 ) ) ;
#2130 = DIRECTION ( 'NONE',  ( -1.000000000000000000, 0.000000000000000000, -0.000000000000000000 ) ) ;
#2131 = AXIS2_PLACEMENT_3D ( 'NONE', #4098, #37188, #72118 ) ;
#2132 = DIRECTION ( 'NONE',  ( 0.000000000000000000, 0.7604059656000322631, -0.6494480483301821039 ) ) ;
#2133 = CARTESIAN_POINT ( 'NONE',  ( 93.84685191531248449, 91.99731107132950569, 85.25072916753381946 ) ) ;
#2134 = CARTESIAN_POINT ( 'NONE',  ( -97.30629616937495996, -209.9999999999999716, 87.26156250086715715 ) ) ;
#2135 = CARTESIAN_POINT ( 'NONE',  ( 10.00000000000000000, 25.88420570971400991, 27.13269053701105449 ) ) ;
#2136 = VERTEX_POINT ( 'NONE', #73283 ) ;
#2137 = DIRECTION ( 'NONE',  ( -1.000000000000000000, 0.000000000000000000, 0.000000000000000000 ) ) ;
#2138 = CARTESIAN_POINT ( 'NONE',  ( -92.34999999999999432, -209.9999999999999716, 82.06250000000000000 ) ) ;
#2139 = CARTESIAN_POINT ( 'NONE',  ( -96.15314808468752972, 91.99731107132950569, 75.56697916753381605 ) ) ;
#2140 = CARTESIAN_POINT ( 'NONE',  ( 92.69370383062501162, -208.6684592857803011, 85.77989583420048803 ) ) ;
#2141 = ORIENTED_EDGE ( 'NONE', *, *, #2607, .T. ) ;
#2142 = DIRECTION ( 'NONE',  ( -1.000000000000000000, 0.000000000000000000, 0.000000000000000000 ) ) ;
#2143 = ORIENTED_EDGE ( 'NONE', *, *, #26142, .T. ) ;
#2144 = AXIS2_PLACEMENT_3D ( 'NONE', #19810, #54046, #58562 ) ;
#2145 = ORIENTED_EDGE ( 'NONE', *, *, #64889, .T. ) ;
#2146 = CIRCLE ( 'NONE', #66983, 37.49900000000000944 ) ;
#2147 = EDGE_CURVE ( 'NONE', #16094, #45782, #53018, .T. ) ;
#2148 = CARTESIAN_POINT ( 'NONE',  ( -3.000000000000000000, 5.835314593368772229, -22.81335362449846826 ) ) ;
#2149 = DIRECTION ( 'NONE',  ( 0.000000000000000000, -0.3090169943749349057, -0.9510565162951577500 ) ) ;
#2150 = AXIS2_PLACEMENT_3D ( 'NONE', #12967, #16878, #39811 ) ;
#2151 = EDGE_CURVE ( 'NONE', #37629, #51617, #36609, .T. ) ;
#2152 = ORIENTED_EDGE ( 'NONE', *, *, #9221, .F. ) ;
#2153 = CIRCLE ( 'NONE', #54916, 77.49899999999999523 ) ;
#2154 = VERTEX_POINT ( 'NONE', #43630 ) ;
#2155 = DIRECTION ( 'NONE',  ( 0.000000000000000000, 1.000000000000000000, -9.787530781167598712E-16 ) ) ;
#2156 = EDGE_CURVE ( 'NONE', #36701, #53249, #14294, .T. ) ;
#2157 = CARTESIAN_POINT ( 'NONE',  ( 96.15314808468750130, -211.9973110713294489, 77.31322916753381946 ) ) ;
#2158 = CYLINDRICAL_SURFACE ( 'NONE', #46467, 37.49900000000000233 ) ;
#2159 = CYLINDRICAL_SURFACE ( 'NONE', #33991, 32.00000000000000000 ) ;
#2160 = CARTESIAN_POINT ( 'NONE',  ( -26.29030328629083968, -123.6496510949466341, 2.500000000000000000 ) ) ;
#2161 = CYLINDRICAL_SURFACE ( 'NONE', #44701, 77.49899999999999523 ) ;
#2162 = EDGE_CURVE ( 'NONE', #51113, #46234, #14576, .T. ) ;
#2163 = DIRECTION ( 'NONE',  ( -1.000000000000000000, 0.000000000000000000, 0.000000000000000000 ) ) ;
#2164 = CARTESIAN_POINT ( 'NONE',  ( 95.00000000000000000, -213.0599564267049857, 83.17374999999999829 ) ) ;
#2165 = ORIENTED_EDGE ( 'NONE', *, *, #6174, .T. ) ;
#2166 = VERTEX_POINT ( 'NONE', #31947 ) ;
#2167 = EDGE_CURVE ( 'NONE', #37724, #39945, #55632, .T. ) ;
#2168 = EDGE_LOOP ( 'NONE', ( #30262, #12321, #9359, #63638 ) ) ;
#2169 = VERTEX_POINT ( 'NONE', #37245 ) ;
#2170 = CARTESIAN_POINT ( 'NONE',  ( -97.64997399525502431, -211.5299932271988723, 86.32229270695523837 ) ) ;
#2171 = AXIS2_PLACEMENT_3D ( 'NONE', #11912, #52889, #7400 ) ;
#2172 = CARTESIAN_POINT ( 'NONE',  ( -96.15314808468752972, 91.99731107132950569, 84.61572916753381435 ) ) ;
#2173 = CARTESIAN_POINT ( 'NONE',  ( 23.41451323550360186, -132.5004227906269989, -5.500000000000000000 ) ) ;
#2174 = CARTESIAN_POINT ( 'NONE',  ( 10.00000000000000000, 76.69515212746057387, -29.01471420065480089 ) ) ;
#2175 = CARTESIAN_POINT ( 'NONE',  ( -1.384174031800281979, -120.5779811845464735, -2.500000000000000000 ) ) ;
#2176 = EDGE_CURVE ( 'NONE', #41055, #54186, #54523, .T. ) ;
#2177 = VECTOR ( 'NONE', #62193, 1000.000000000000000 ) ;
#2178 = ORIENTED_EDGE ( 'NONE', *, *, #14660, .T. ) ;
#2179 = DIRECTION ( 'NONE',  ( -1.000000000000000000, -0.000000000000000000, -0.000000000000000000 ) ) ;
#2180 = ORIENTED_EDGE ( 'NONE', *, *, #58720, .T. ) ;
#2181 = EDGE_CURVE ( 'NONE', #37253, #52969, #24207, .T. ) ;
#2182 = CARTESIAN_POINT ( 'NONE',  ( 0.000000000000000000, -10.30890764327441822, 81.34940948281332851 ) ) ;
#2183 = ORIENTED_EDGE ( 'NONE', *, *, #4249, .F. ) ;
#2184 = CARTESIAN_POINT ( 'NONE',  ( -96.32500000000001705, 92.29496732002878900, 86.79854166840097207 ) ) ;
#2185 = AXIS2_PLACEMENT_3D ( 'NONE', #10980, #22631, #73372 ) ;
#2186 = CARTESIAN_POINT ( 'NONE',  ( 96.15314808468748708, 91.99731107132950569, 86.41489583420049314 ) ) ;
#2187 = PLANE ( 'NONE',  #44209 ) ;
#2188 = DIRECTION ( 'NONE',  ( 0.000000000000000000, 0.9876883405951372152, 0.1564344650402346160 ) ) ;
#2189 = DIRECTION ( 'NONE',  ( -0.9918136447140100120, 0.1276937514489704939, 0.000000000000000000 ) ) ;
#2190 = CARTESIAN_POINT ( 'NONE',  ( -11.59999999999999964, -0.8299999999999986278, 0.000000000000000000 ) ) ;
#2191 = ORIENTED_EDGE ( 'NONE', *, *, #47228, .T. ) ;
#2192 = DIRECTION ( 'NONE',  ( 0.000000000000000000, 0.9510565162951521989, 0.3090169943749517256 ) ) ;
#2193 = ADVANCED_FACE ( 'NONE', ( #15396 ), #3050, .T. ) ;
#2194 = EDGE_CURVE ( 'NONE', #58172, #67479, #30195, .T. ) ;
#2195 = LINE ( 'NONE', #6685, #73174 ) ;
#2196 = ORIENTED_EDGE ( 'NONE', *, *, #1428, .T. ) ;
#2197 = ORIENTED_EDGE ( 'NONE', *, *, #69129, .F. ) ;
#2198 = CARTESIAN_POINT ( 'NONE',  ( 11.99999999999999822, 0.000000000000000000, 0.000000000000000000 ) ) ;
#2199 = CYLINDRICAL_SURFACE ( 'NONE', #34816, 2.650000000000540812 ) ;
#2200 = CARTESIAN_POINT ( 'NONE',  ( -97.65000000000001990, 90.00000000000004263, 75.47437500173430180 ) ) ;
#2201 = CARTESIAN_POINT ( 'NONE',  ( -92.69370383062498320, -208.6684592857803011, 88.26697916753381890 ) ) ;
#2202 = ORIENTED_EDGE ( 'NONE', *, *, #62936, .T. ) ;
#2203 = AXIS2_PLACEMENT_3D ( 'NONE', #1523, #6392, #12744 ) ;
#2204 = DIRECTION ( 'NONE',  ( -1.000000000000000000, -0.000000000000000000, -0.000000000000000000 ) ) ;
#2205 = ORIENTED_EDGE ( 'NONE', *, *, #16288, .T. ) ;
#2206 = VECTOR ( 'NONE', #31382, 999.9999999999998863 ) ;
#2207 = VECTOR ( 'NONE', #33319, 1000.000000000000000 ) ;
#2208 = EDGE_LOOP ( 'NONE', ( #5662, #48384, #16356, #23020 ) ) ;
#2209 = CARTESIAN_POINT ( 'NONE',  ( 0.000000000000000000, 18.84667830672605859, -18.68964196561243796 ) ) ;
#2210 = CARTESIAN_POINT ( 'NONE',  ( 94.99999999999998579, 93.05995642670504253, 86.66624999999999091 ) ) ;
#2211 = AXIS2_PLACEMENT_3D ( 'NONE', #12517, #45652, #69669 ) ;
#2212 = CYLINDRICAL_SURFACE ( 'NONE', #9342, 42.00000000000000000 ) ;
#2213 = CARTESIAN_POINT ( 'NONE',  ( 97.30629616937498838, 90.00000000000002842, 82.97531250086714749 ) ) ;
#2214 = DIRECTION ( 'NONE',  ( 1.000000000000000000, 0.000000000000000000, 0.000000000000000000 ) ) ;
#2215 = DIRECTION ( 'NONE',  ( -1.000000000000000000, -0.000000000000000000, 0.000000000000000000 ) ) ;
#2216 = DIRECTION ( 'NONE',  ( -0.000000000000000000, -0.000000000000000000, 1.000000000000000000 ) ) ;
#2217 = FACE_OUTER_BOUND ( 'NONE', #70885, .T. ) ;
#2218 = CARTESIAN_POINT ( 'NONE',  ( -92.35000000000005116, 88.47002178664754979, 77.00895833506763211 ) ) ;
#2219 = CARTESIAN_POINT ( 'NONE',  ( 10.00000000000000000, 40.65526001592612459, 71.21200624218811015 ) ) ;
#2220 = DIRECTION ( 'NONE',  ( 1.000000000000000000, 0.000000000000000000, 0.000000000000000000 ) ) ;
#2221 = CARTESIAN_POINT ( 'NONE',  ( 92.35000000000000853, -208.4700217866474645, 85.58145833506763722 ) ) ;
#2222 = CARTESIAN_POINT ( 'NONE',  ( 0.000000000000000000, 75.16055320797057959, -18.89407956138176914 ) ) ;
#2223 = ORIENTED_EDGE ( 'NONE', *, *, #63704, .T. ) ;
#2224 = CARTESIAN_POINT ( 'NONE',  ( -93.84685191531254134, 91.99731107132950569, 86.89114583420047211 ) ) ;
#2225 = DIRECTION ( 'NONE',  ( -1.000000000000000000, -0.000000000000000000, -0.000000000000000000 ) ) ;
#2226 = ADVANCED_FACE ( 'NONE', ( #72533 ), #60186, .F. ) ;
#2227 = VECTOR ( 'NONE', #22749, 1000.000000000000000 ) ;
#2229 = EDGE_CURVE ( 'NONE', #46998, #14970, #33054, .T. ) ;
#2228 = VECTOR ( 'NONE', #24928, 1000.000000000000000 ) ;
#2230 = CARTESIAN_POINT ( 'NONE',  ( 0.000000000000000000, 76.41127070299290835, -12.93880638057234123 ) ) ;
#2231 = EDGE_CURVE ( 'NONE', #25802, #52184, #66907, .T. ) ;
#2232 = ORIENTED_EDGE ( 'NONE', *, *, #11483, .T. ) ;
#2233 =( GEOMETRIC_REPRESENTATION_CONTEXT ( 3 ) GLOBAL_UNCERTAINTY_ASSIGNED_CONTEXT ( ( #8273 ) ) GLOBAL_UNIT_ASSIGNED_CONTEXT ( ( #17270, #61286, #16524 ) ) REPRESENTATION_CONTEXT ( 'NONE', 'WORKASPACE' ) );
#2234 = CARTESIAN_POINT ( 'NONE',  ( 0.000000000000000000, 0.000000000000000000, 0.000000000000000000 ) ) ;
#2235 = LINE ( 'NONE', #48059, #42023 ) ;
#2236 = CARTESIAN_POINT ( 'NONE',  ( 10.00000000000000000, -55.20638768913797634, 51.02545421589302777 ) ) ;
#2237 = EDGE_CURVE ( 'NONE', #44790, #71356, #42871, .T. ) ;
#2238 = CARTESIAN_POINT ( 'NONE',  ( 93.84685191531251292, -211.9973110713294489, 83.55739583420049144 ) ) ;
#2239 = EDGE_CURVE ( 'NONE', #60337, #68796, #23644, .T. ) ;
#2240 = EDGE_LOOP ( 'NONE', ( #3243, #38073, #43114, #12626 ) ) ;
#2241 = ORIENTED_EDGE ( 'NONE', *, *, #11525, .T. ) ;
#2242 = CYLINDRICAL_SURFACE ( 'NONE', #47591, 2.649999999999985700 ) ;
#2243 = ORIENTED_EDGE ( 'NONE', *, *, #9495, .F. ) ;
#2244 = DIRECTION ( 'NONE',  ( 1.000000000000000000, 0.000000000000000000, -0.000000000000000000 ) ) ;
#2245 = DIRECTION ( 'NONE',  ( -0.000000000000000000, -0.000000000000000000, 1.000000000000000000 ) ) ;
#2246 = EDGE_CURVE ( 'NONE', #62834, #3072, #22923, .T. ) ;
#2247 = AXIS2_PLACEMENT_3D ( 'NONE', #1064, #40500, #13026 ) ;
#2248 = EDGE_LOOP ( 'NONE', ( #12656, #52522, #7149, #49721 ) ) ;
#2249 = CARTESIAN_POINT ( 'NONE',  ( 92.69370383062501162, -209.9999999999999716, 79.64156250086715261 ) ) ;
#2250 = VECTOR ( 'NONE', #24283, 1000.000000000000000 ) ;
#2251 = AXIS2_PLACEMENT_3D ( 'NONE', #31758, #14848, #42685 ) ;
#2252 = ORIENTED_EDGE ( 'NONE', *, *, #13400, .F. ) ;
#2253 = CARTESIAN_POINT ( 'NONE',  ( 96.32499999999998863, 87.70503267997126784, 79.41666666666665719 ) ) ;
#2254 = ORIENTED_EDGE ( 'NONE', *, *, #54247, .F. ) ;
#2255 = ORIENTED_EDGE ( 'NONE', *, *, #9692, .F. ) ;
#2256 = DIRECTION ( 'NONE',  ( -1.000000000000000000, 0.000000000000000000, 0.000000000000000000 ) ) ;
#2257 = CIRCLE ( 'NONE', #29837, 37.49900000000000233 ) ;
#2258 = CARTESIAN_POINT ( 'NONE',  ( 96.32499999999998863, -207.7050326799711968, 80.26333333333332121 ) ) ;
#2259 = ORIENTED_EDGE ( 'NONE', *, *, #58765, .T. ) ;
#2260 = CARTESIAN_POINT ( 'NONE',  ( -96.32500000000001705, 92.29496732002878900, 84.17916666666666003 ) ) ;
#2261 = CARTESIAN_POINT ( 'NONE',  ( 97.64999999999997726, -208.4700217866474645, 82.82979166840095786 ) ) ;
#2262 = CARTESIAN_POINT ( 'NONE',  ( 94.99999999999998579, 93.05995642670504253, 84.12625000000001307 ) ) ;
#2263 = ADVANCED_FACE ( 'NONE', ( #10505 ), #63510, .T. ) ;
#2264 = EDGE_LOOP ( 'NONE', ( #67169, #30583, #61452, #35054 ) ) ;
#2265 = DIRECTION ( 'NONE',  ( 0.000000000000000000, 0.000000000000000000, 1.000000000000000000 ) ) ;
#2266 = EDGE_CURVE ( 'NONE', #45880, #26872, #58477, .T. ) ;
#2267 = DIRECTION ( 'NONE',  ( 0.000000000000000000, -0.8090169943749402348, -0.5877852522924830181 ) ) ;
#2268 = VERTEX_POINT ( 'NONE', #11986 ) ;
#2269 = VERTEX_POINT ( 'NONE', #23284 ) ;
#2270 = CARTESIAN_POINT ( 'NONE',  ( -97.30629616937501680, 91.33154071421968467, 89.11364583420049712 ) ) ;
#2271 = CARTESIAN_POINT ( 'NONE',  ( 92.69370383062498320, 88.66845928578037217, 81.44072916753381719 ) ) ;
#2272 = ORIENTED_EDGE ( 'NONE', *, *, #68865, .F. ) ;
#2273 = CARTESIAN_POINT ( 'NONE',  ( 97.64999999999997726, 88.47002178664753558, 85.89895833506764689 ) ) ;
#2274 = CIRCLE ( 'NONE', #39440, 31.99999999999999289 ) ;
#2275 = VERTEX_POINT ( 'NONE', #16151 ) ;
#2276 = DIRECTION ( 'NONE',  ( 1.000000000000000000, 0.000000000000000000, 0.000000000000000000 ) ) ;
#2277 = ORIENTED_EDGE ( 'NONE', *, *, #3250, .T. ) ;
#2278 = AXIS2_PLACEMENT_3D ( 'NONE', #66936, #15819, #38749 ) ;
#2279 = ORIENTED_EDGE ( 'NONE', *, *, #8294, .F. ) ;
#2280 = ORIENTED_EDGE ( 'NONE', *, *, #62245, .F. ) ;
#2281 = DIRECTION ( 'NONE',  ( -1.000000000000000000, 0.000000000000000000, -0.000000000000000000 ) ) ;
#2282 = CARTESIAN_POINT ( 'NONE',  ( 96.32499999999997442, 92.29496732002878900, 75.26270833506764291 ) ) ;
#2283 = VECTOR ( 'NONE', #21810, 1000.000000000000000 ) ;
#2284 = AXIS2_PLACEMENT_3D ( 'NONE', #18097, #62498, #69231 ) ;
#2285 = CARTESIAN_POINT ( 'NONE',  ( -95.00000000000002842, 93.05995642670501411, 83.49125000000000796 ) ) ;
#2286 = ORIENTED_EDGE ( 'NONE', *, *, #39127, .F. ) ;
#2287 = CARTESIAN_POINT ( 'NONE',  ( 96.73972734126401463, 91.51405112163766375, 74.79348190356853365 ) ) ;
#2288 = AXIS2_PLACEMENT_3D ( 'NONE', #50925, #56953, #40387 ) ;
#2289 = LINE ( 'NONE', #42111, #27503 ) ;
#2290 = ORIENTED_EDGE ( 'NONE', *, *, #74029, .F. ) ;
#2291 =( BOUNDED_CURVE ( )  B_SPLINE_CURVE ( 2, ( #27012, #72860, #38309, #31916, #49574, #20265, #44324 ),
 .UNSPECIFIED., .F., .F. ) 
 B_SPLINE_CURVE_WITH_KNOTS ( ( 3, 2, 2, 3 ),
 ( 0.5503499107253647660, 0.5574054777324447540, 0.5644612432733617791, 0.5715170088694363493 ),
 .UNSPECIFIED. ) 
 CURVE ( )  GEOMETRIC_REPRESENTATION_ITEM ( )  RATIONAL_B_SPLINE_CURVE ( ( 0.9999924607068964022, 0.8660291735370631017, 1.000000000000000000, 0.8660254037844387076, 1.000000000000000000, 0.8660254037844387076, 1.000000000000000000 ) ) 
 REPRESENTATION_ITEM ( '' )  );
#2292 = DIRECTION ( 'NONE',  ( 0.000000000000000000, 0.9969173337331281859, -0.07845909572784168229 ) ) ;
#2293 = CARTESIAN_POINT ( 'NONE',  ( -92.69370383062498320, -211.3315407142195852, 83.55739583420047722 ) ) ;
#2294 = VERTEX_POINT ( 'NONE', #16906 ) ;
#2295 = DIRECTION ( 'NONE',  ( 0.000000000000000000, 0.000000000000000000, -1.000000000000000000 ) ) ;
#2296 = DIRECTION ( 'NONE',  ( 1.000000000000000000, 0.000000000000000000, 0.000000000000000000 ) ) ;
#2297 = CARTESIAN_POINT ( 'NONE',  ( 0.000000000000000000, 5.773502691896262640, 0.000000000000000000 ) ) ;
#2298 = CARTESIAN_POINT ( 'NONE',  ( 12.00000000000000000, -22.32062822937469093, 14.36278369418830181 ) ) ;
#2299 = DIRECTION ( 'NONE',  ( -1.000000000000000000, 0.000000000000000000, 0.000000000000000000 ) ) ;
#2300 = CYLINDRICAL_SURFACE ( 'NONE', #76, 82.00000000000000000 ) ;
#2301 = CARTESIAN_POINT ( 'NONE',  ( 97.01450244679210755, -211.1324117838501877, 74.79348190356851944 ) ) ;
#2302 = DIRECTION ( 'NONE',  ( -1.000000000000000000, 0.000000000000000000, 0.000000000000000000 ) ) ;
#2303 = CARTESIAN_POINT ( 'NONE',  ( 10.00000000000000000, 65.64334221924909230, 41.19522573413756561 ) ) ;
#2304 = VECTOR ( 'NONE', #20815, 1000.000000000000000 ) ;
#2305 = EDGE_CURVE ( 'NONE', #54905, #49986, #32055, .T. ) ;
#2306 = CARTESIAN_POINT ( 'NONE',  ( -97.30629616937501680, 90.00000000000004263, 76.30781250086714351 ) ) ;
#2307 = DIRECTION ( 'NONE',  ( 0.000000000000000000, 0.5877852522924742473, -0.8090169943749465631 ) ) ;
#2308 = DIRECTION ( 'NONE',  ( 0.000000000000000000, 0.000000000000000000, 1.000000000000000000 ) ) ;
#2309 = UNCERTAINTY_MEASURE_WITH_UNIT (LENGTH_MEASURE( 1.000000000000000082E-05 ), #36000, 'distance_accuracy_value', 'NONE');
#2310 = AXIS2_PLACEMENT_3D ( 'NONE', #38860, #55408, #3931 ) ;
#2311 = CARTESIAN_POINT ( 'NONE',  ( 11.99999999999999822, 39.47590169984846398, 71.87247863392425984 ) ) ;
#2312 = AXIS2_PLACEMENT_3D ( 'NONE', #69309, #7633, #6179 ) ;
#2313 = VECTOR ( 'NONE', #1580, 1000.000000000000114 ) ;
#2314 = DIRECTION ( 'NONE',  ( 0.000000000000000000, 0.000000000000000000, 1.000000000000000000 ) ) ;
#2315 = CARTESIAN_POINT ( 'NONE',  ( -15.44521549751111955, -137.7748507232956001, -2.500000000000000000 ) ) ;
#2316 = CARTESIAN_POINT ( 'NONE',  ( 92.35000000000000853, -209.9999999999999716, 77.29999999999999716 ) ) ;
#2317 = CARTESIAN_POINT ( 'NONE',  ( 0.000000000000000000, 74.65374052328660071, -8.840884882374309583 ) ) ;
#2318 = CARTESIAN_POINT ( 'NONE',  ( 97.64999999999999147, 90.00000000000002842, 90.00000000000000000 ) ) ;
#2319 = CARTESIAN_POINT ( 'NONE',  ( -92.34999999999999432, -211.5299782133524502, 89.62958333333332916 ) ) ;
#2320 = VECTOR ( 'NONE', #60550, 1000.000000000000000 ) ;
#2321 = EDGE_CURVE ( 'NONE', #28941, #7487, #57491, .T. ) ;
#2322 = ADVANCED_FACE ( 'NONE', ( #73654 ), #10891, .F. ) ;
#2323 = DIRECTION ( 'NONE',  ( -0.000000000000000000, -0.000000000000000000, 1.000000000000000000 ) ) ;
#2324 = ORIENTED_EDGE ( 'NONE', *, *, #13247, .F. ) ;
#2325 = CARTESIAN_POINT ( 'NONE',  ( 10.00000000000000000, -26.79245525562691199, -32.34446384430000876 ) ) ;
#2326 = PLANE ( 'NONE',  #26246 ) ;
#2327 = CARTESIAN_POINT ( 'NONE',  ( 97.64999999999999147, -209.9999999999999716, 76.34749999999999659 ) ) ;
#2328 = EDGE_CURVE ( 'NONE', #15222, #73599, #8029, .T. ) ;
#2329 = CARTESIAN_POINT ( 'NONE',  ( -20.30386590532155111, -102.9045904027214959, -2.500000000000000000 ) ) ;
#2330 = VECTOR ( 'NONE', #54980, 1000.000000000000000 ) ;
#2331 = EDGE_CURVE ( 'NONE', #38213, #8802, #40450, .T. ) ;
#2332 = VECTOR ( 'NONE', #7775, 1000.000000000000114 ) ;
#2333 = VECTOR ( 'NONE', #25162, 1000.000000000000000 ) ;
#2334 = AXIS2_PLACEMENT_3D ( 'NONE', #66121, #42441, #70988 ) ;
#2335 = ORIENTED_EDGE ( 'NONE', *, *, #52197, .T. ) ;
#2336 = CIRCLE ( 'NONE', #22757, 0.5999999999999928724 ) ;
#2337 = DIRECTION ( 'NONE',  ( 1.000000000000000000, 0.000000000000000000, -0.000000000000000000 ) ) ;
#2338 = CYLINDRICAL_SURFACE ( 'NONE', #25953, 16.00000000000000000 ) ;
#2339 = EDGE_LOOP ( 'NONE', ( #11916, #20613, #39036, #53494 ) ) ;
#2340 = VECTOR ( 'NONE', #20874, 1000.000000000000000 ) ;
#2341 = CARTESIAN_POINT ( 'NONE',  ( 93.84685191531249870, -208.0026889286704943, 83.18697916753382060 ) ) ;
#2342 = CARTESIAN_POINT ( 'NONE',  ( 97.30629616937498838, -209.9999999999999716, 87.57906250086715261 ) ) ;
#2343 = EDGE_CURVE ( 'NONE', #62638, #43916, #41555, .T. ) ;
#2344 = EDGE_LOOP ( 'NONE', ( #61508, #36126, #11112, #46149 ) ) ;
#2345 = CARTESIAN_POINT ( 'NONE',  ( 7.399999999999994138, 1.489868709406086122E-13, 12.50000000000000533 ) ) ;
#2346 = ORIENTED_EDGE ( 'NONE', *, *, #61272, .T. ) ;
#2347 = VERTEX_POINT ( 'NONE', #51844 ) ;
#2348 = CARTESIAN_POINT ( 'NONE',  ( -95.00000000000002842, 87.33691857156074434, 77.26031250086714408 ) ) ;
#2349 = ORIENTED_EDGE ( 'NONE', *, *, #47198, .F. ) ;
#2350 = ORIENTED_EDGE ( 'NONE', *, *, #71718, .F. ) ;
#2351 = CARTESIAN_POINT ( 'NONE',  ( -20.30386590532152979, -102.9045904027214959, 5.500000000000000000 ) ) ;
#2352 = ORIENTED_EDGE ( 'NONE', *, *, #68826, .T. ) ;
#2353 = CARTESIAN_POINT ( 'NONE',  ( 10.00000000000000000, -30.00120703465189465, -22.64427369931201639 ) ) ;
#2354 = CIRCLE ( 'NONE', #59913, 12.49999999999999645 ) ;
#2355 = EDGE_CURVE ( 'NONE', #16458, #40253, #71665, .T. ) ;
#2356 = VERTEX_POINT ( 'NONE', #5634 ) ;
#2357 = PLANE ( 'NONE',  #10599 ) ;
#2358 = ORIENTED_EDGE ( 'NONE', *, *, #34277, .T. ) ;
#2359 = DIRECTION ( 'NONE',  ( 1.000000000000000000, 0.000000000000000000, 0.000000000000000000 ) ) ;
#2360 = VECTOR ( 'NONE', #38026, 1000.000000000000000 ) ;
#2361 = EDGE_CURVE ( 'NONE', #54121, #6591, #390, .T. ) ;
#2362 = AXIS2_PLACEMENT_3D ( 'NONE', #71172, #19677, #41882 ) ;
#2363 = ORIENTED_EDGE ( 'NONE', *, *, #5707, .F. ) ;
#2364 = AXIS2_PLACEMENT_3D ( 'NONE', #9678, #43903, #15309 ) ;
#2365 = CIRCLE ( 'NONE', #22792, 82.00000000000000000 ) ;
#2366 = ORIENTED_EDGE ( 'NONE', *, *, #47957, .F. ) ;
#2367 = ORIENTED_EDGE ( 'NONE', *, *, #58401, .T. ) ;
#2368 = CARTESIAN_POINT ( 'NONE',  ( 93.84685191531249870, -208.0026889286704943, 76.83697916753381207 ) ) ;
#2369 = FACE_OUTER_BOUND ( 'NONE', #40880, .T. ) ;
#2370 = CONTEXT_DEPENDENT_SHAPE_REPRESENTATION ( #27770, #45858 ) ;
#2371 = CARTESIAN_POINT ( 'NONE',  ( -3.000000000000000000, -19.89357724624987256, -12.59942793731086041 ) ) ;
#2372 = ORIENTED_EDGE ( 'NONE', *, *, #7575, .T. ) ;
#2373 = CARTESIAN_POINT ( 'NONE',  ( 6.719258119307965238, -15.35072898742050107, -1.199999999999999956 ) ) ;
#2374 = FACE_OUTER_BOUND ( 'NONE', #18159, .T. ) ;
#2375 = AXIS2_PLACEMENT_3D ( 'NONE', #49526, #60099, #66104 ) ;
#2376 = CARTESIAN_POINT ( 'NONE',  ( -92.34999999999999432, -209.9999999999999716, 75.71250000000000568 ) ) ;
#2377 = LINE ( 'NONE', #60234, #64876 ) ;
#2378 = DIRECTION ( 'NONE',  ( 0.000000000000000000, 0.000000000000000000, -1.000000000000000000 ) ) ;
#2379 = CARTESIAN_POINT ( 'NONE',  ( -92.69370383062498320, -211.3315407142195852, 80.38239583420049428 ) ) ;
#2380 = CARTESIAN_POINT ( 'NONE',  ( -92.69370383062502583, 91.33154071421968467, 79.37697916753381833 ) ) ;
#2381 = ORIENTED_EDGE ( 'NONE', *, *, #60782, .T. ) ;
#2382 = CARTESIAN_POINT ( 'NONE',  ( 94.99999999999998579, 92.66308142843935514, 80.59406250086715318 ) ) ;
#2383 = EDGE_LOOP ( 'NONE', ( #10793, #2879, #10748, #24982 ) ) ;
#2384 = CARTESIAN_POINT ( 'NONE',  ( 93.67499999999998295, 92.29496732002878900, 78.54354166840096241 ) ) ;
#2385 = DIRECTION ( 'NONE',  ( 0.000000000000000000, 0.000000000000000000, 1.000000000000000000 ) ) ;
#2386 = DIRECTION ( 'NONE',  ( -0.000000000000000000, -0.000000000000000000, -1.000000000000000000 ) ) ;
#2387 = LINE ( 'NONE', #42567, #40371 ) ;
#2388 = DIRECTION ( 'NONE',  ( 0.000000000000000000, 0.000000000000000000, 1.000000000000000000 ) ) ;
#2389 = CARTESIAN_POINT ( 'NONE',  ( -93.84685191531247028, -211.9973110713294489, 83.50447916753381605 ) ) ;
#2390 = CIRCLE ( 'NONE', #53976, 16.00000000000000000 ) ;
#2391 = DIRECTION ( 'NONE',  ( 1.000000000000000000, -0.000000000000000000, 0.000000000000000000 ) ) ;
#2392 = FACE_OUTER_BOUND ( 'NONE', #70808, .T. ) ;
#2393 = CARTESIAN_POINT ( 'NONE',  ( 10.00000000000000000, 0.000000000000000000, 0.000000000000000000 ) ) ;
#2394 = ORIENTED_EDGE ( 'NONE', *, *, #12407, .F. ) ;
#2395 = CIRCLE ( 'NONE', #28739, 16.00000000000000000 ) ;
#2396 = VECTOR ( 'NONE', #30345, 1000.000000000000000 ) ;
#2397 = VERTEX_POINT ( 'NONE', #57127 ) ;
#2398 = CARTESIAN_POINT ( 'NONE',  ( 11.99999999999999822, -74.18225833017913828, 34.94270380257611208 ) ) ;
#2399 = VECTOR ( 'NONE', #8785, 1000.000000000000000 ) ;
#2400 = AXIS2_PLACEMENT_3D ( 'NONE', #34460, #40115, #63068 ) ;
#2401 = CARTESIAN_POINT ( 'NONE',  ( 11.99999999999999822, 0.000000000000000000, 0.000000000000000000 ) ) ;
#2402 = DIRECTION ( 'NONE',  ( 0.000000000000000000, -0.8526401643540860720, -0.5224985647159590130 ) ) ;
#2403 = CARTESIAN_POINT ( 'NONE',  ( -96.15314808468751551, 88.00268892867056536, 86.57364583420047666 ) ) ;
#2404 = CARTESIAN_POINT ( 'NONE',  ( 0.000000000000000000, -3.894527615417333610, -81.90746397400393164 ) ) ;
#2405 = DIRECTION ( 'NONE',  ( -0.6862798483830533369, -0.7273375899149812085, 0.000000000000000000 ) ) ;
#2406 = DIRECTION ( 'NONE',  ( -7.945298363252408085E-16, -1.065814103640131188E-14, -1.000000000000000000 ) ) ;
#2407 = EDGE_LOOP ( 'NONE', ( #7210, #21070, #63186, #27827 ) ) ;
#2408 = CARTESIAN_POINT ( 'NONE',  ( -92.69370383062504004, 90.00000000000004263, 74.72031250086713783 ) ) ;
#2409 = EDGE_CURVE ( 'NONE', #19936, #50232, #5563, .T. ) ;
#2410 = CARTESIAN_POINT ( 'NONE',  ( 11.99999999999999822, 70.52718814184294160, -26.02418014898236720 ) ) ;
#2411 = DIRECTION ( 'NONE',  ( -1.000000000000000000, -0.000000000000000000, -0.000000000000000000 ) ) ;
#2412 = CARTESIAN_POINT ( 'NONE',  ( -3.000000000000000000, 26.50000000000000000, -1.500000000000001332 ) ) ;
#2413 = DIRECTION ( 'NONE',  ( -1.000000000000000000, 0.000000000000000000, 0.000000000000000000 ) ) ;
#2414 = CARTESIAN_POINT ( 'NONE',  ( -97.64999999999996305, -209.9999999999999716, 76.03000000000000114 ) ) ;
#2415 = CARTESIAN_POINT ( 'NONE',  ( -93.84685191531247028, -211.9973110713294489, 82.39322916753381776 ) ) ;
#2416 =( NAMED_UNIT ( * ) PLANE_ANGLE_UNIT ( ) SI_UNIT ( $, .RADIAN. ) );
#2417 = EDGE_CURVE ( 'NONE', #23688, #40782, #10815, .T. ) ;
#2418 = EDGE_CURVE ( 'NONE', #12733, #55763, #59337, .T. ) ;
#2419 = DIRECTION ( 'NONE',  ( 1.000000000000000000, -0.000000000000000000, -0.000000000000000000 ) ) ;
#2420 = AXIS2_PLACEMENT_3D ( 'NONE', #41593, #25422, #42709 ) ;
#2421 = CARTESIAN_POINT ( 'NONE',  ( 94.99999999999998579, 92.66308142843932671, 75.03781250086714749 ) ) ;
#2422 = AXIS2_PLACEMENT_3D ( 'NONE', #44885, #32469, #32835 ) ;
#2423 = CARTESIAN_POINT ( 'NONE',  ( -92.69370383062498320, -208.6684592857803295, 76.20197916753382117 ) ) ;
#2424 = LINE ( 'NONE', #24211, #31417 ) ;
#2425 = ORIENTED_EDGE ( 'NONE', *, *, #21212, .T. ) ;
#2426 = EDGE_CURVE ( 'NONE', #25590, #50309, #17637, .T. ) ;
#2427 = CARTESIAN_POINT ( 'NONE',  ( 24.94940289813197509, -237.3777120880564553, -5.500000000000000000 ) ) ;
#2428 = DIRECTION ( 'NONE',  ( 0.6064928550163524168, 0.7950889364178788110, -0.000000000000000000 ) ) ;
#2429 = AXIS2_PLACEMENT_3D ( 'NONE', #58772, #30182, #64785 ) ;
#2430 = DIRECTION ( 'NONE',  ( 0.000000000000000000, -1.000000000000000000, 0.000000000000000000 ) ) ;
#2431 = VECTOR ( 'NONE', #73815, 1000.000000000000114 ) ;
#2432 = FACE_OUTER_BOUND ( 'NONE', #29237, .T. ) ;
#2433 = CARTESIAN_POINT ( 'NONE',  ( 92.69370383062501162, -209.9999999999999716, 88.53156250086716739 ) ) ;
#2434 = EDGE_LOOP ( 'NONE', ( #65330, #60143, #52415, #7736 ) ) ;
#2435 = CARTESIAN_POINT ( 'NONE',  ( 15.00000000000000000, 5.835314593368470248, -22.81335362449854642 ) ) ;
#2436 = DIRECTION ( 'NONE',  ( 0.000000000000000000, 0.000000000000000000, -1.000000000000000000 ) ) ;
#2437 = CARTESIAN_POINT ( 'NONE',  ( 11.99999999999999822, -77.32052557432845674, 5.256550761632577284 ) ) ;
#2438 = EDGE_CURVE ( 'NONE', #49630, #38085, #24023, .T. ) ;
#2439 = ORIENTED_EDGE ( 'NONE', *, *, #42439, .T. ) ;
#2440 = CYLINDRICAL_SURFACE ( 'NONE', #37531, 31.99999999999998579 ) ;
#2441 = EDGE_CURVE ( 'NONE', #8621, #33107, #31119, .T. ) ;
#2442 = ADVANCED_FACE ( 'NONE', ( #59711 ), #30006, .F. ) ;
#2443 = ORIENTED_EDGE ( 'NONE', *, *, #32516, .F. ) ;
#2444 = CIRCLE ( 'NONE', #39649, 82.00000000000000000 ) ;
#2445 = CARTESIAN_POINT ( 'NONE',  ( 0.000000000000000000, 0.000000000000000000, -90.00000000000000000 ) ) ;
#2446 = EDGE_CURVE ( 'NONE', #52874, #20645, #42077, .T. ) ;
#2447 = AXIS2_PLACEMENT_3D ( 'NONE', #58213, #42406, #6358 ) ;
#2448 = VECTOR ( 'NONE', #71191, 1000.000000000000000 ) ;
#2449 = AXIS2_PLACEMENT_3D ( 'NONE', #19349, #59212, #6604 ) ;
#2450 = EDGE_LOOP ( 'NONE', ( #72929, #48162 ) ) ;
#2451 = ORIENTED_EDGE ( 'NONE', *, *, #40250, .T. ) ;
#2452 = ORIENTED_EDGE ( 'NONE', *, *, #42883, .T. ) ;
#2453 = VECTOR ( 'NONE', #14953, 999.9999999999998863 ) ;
#2454 = LINE ( 'NONE', #24953, #27482 ) ;
#2455 = ADVANCED_FACE ( 'NONE', ( #13821 ), #70220, .F. ) ;
#2456 = VERTEX_POINT ( 'NONE', #70970 ) ;
#2457 = ORIENTED_EDGE ( 'NONE', *, *, #56794, .F. ) ;
#2458 = CARTESIAN_POINT ( 'NONE',  ( 97.30629616937498838, 90.00000000000002842, 80.59406250086715318 ) ) ;
#2459 = DIRECTION ( 'NONE',  ( -1.000000000000000000, 0.000000000000000000, -0.000000000000000000 ) ) ;
#2460 = CYLINDRICAL_SURFACE ( 'NONE', #18814, 31.99999999999998579 ) ;
#2461 = ORIENTED_EDGE ( 'NONE', *, *, #25863, .T. ) ;
#2462 = ORIENTED_EDGE ( 'NONE', *, *, #51771, .F. ) ;
#2463 = ORIENTED_EDGE ( 'NONE', *, *, #9082, .T. ) ;
#2464 = DIRECTION ( 'NONE',  ( -1.000000000000000000, 0.000000000000000000, -0.000000000000000000 ) ) ;
#2465 = VERTEX_POINT ( 'NONE', #18726 ) ;
#2466 = CARTESIAN_POINT ( 'NONE',  ( 3.144186300207962859E-15, -120.0000000000000000, -90.00000000000001421 ) ) ;
#2467 = DIRECTION ( 'NONE',  ( -0.000000000000000000, -0.000000000000000000, -1.000000000000000000 ) ) ;
#2468 = DIRECTION ( 'NONE',  ( 1.000000000000000000, -7.571539615859142926E-15, -2.592266024478009537E-14 ) ) ;
#2469 = CARTESIAN_POINT ( 'NONE',  ( -7.400000000000014566, -1.501883841367401167E-13, -13.10000000000024123 ) ) ;
#2470 = CARTESIAN_POINT ( 'NONE',  ( 10.00000000000000000, 0.000000000000000000, 0.000000000000000000 ) ) ;
#2471 = CYLINDRICAL_SURFACE ( 'NONE', #41864, 2.649999999999985700 ) ;
#2472 = CARTESIAN_POINT ( 'NONE',  ( -96.32499999999996021, -207.7050326799711968, 76.63854166840096127 ) ) ;
#2473 = CARTESIAN_POINT ( 'NONE',  ( -97.30629616937501680, 90.00000000000004263, 89.80156250086714920 ) ) ;
#2475 = CARTESIAN_POINT ( 'NONE',  ( -96.32500000000001705, 87.70503267997129626, 76.21520833506762926 ) ) ;
#2474 = CARTESIAN_POINT ( 'NONE',  ( 92.34999999999999432, 88.47002178664753558, 75.52729166840099140 ) ) ;
#2476 = AXIS2_PLACEMENT_3D ( 'NONE', #9904, #31717, #71941 ) ;
#2477 = ORIENTED_EDGE ( 'NONE', *, *, #33420, .F. ) ;
#2478 = CARTESIAN_POINT ( 'NONE',  ( 97.30629616937498838, 91.33154071421968467, 76.20197916753382117 ) ) ;
#2479 = CARTESIAN_POINT ( 'NONE',  ( 93.67499999999998295, 92.29496732002878900, 82.27416666666665890 ) ) ;
#2480 = DIRECTION ( 'NONE',  ( -1.000000000000000000, -0.000000000000000000, 0.000000000000000000 ) ) ;
#2481 = CARTESIAN_POINT ( 'NONE',  ( 10.00000000000000000, 37.48860685352291000, 0.8828120875901893649 ) ) ;
#2482 = DIRECTION ( 'NONE',  ( 0.000000000000000000, 0.000000000000000000, 1.000000000000000000 ) ) ;
#2483 = DIRECTION ( 'NONE',  ( -0.000000000000000000, 0.1045284632676436315, 0.9945218953682742891 ) ) ;
#2484 = VECTOR ( 'NONE', #12704, 1000.000000000000000 ) ;
#2485 = VERTEX_POINT ( 'NONE', #52957 ) ;
#2486 = CARTESIAN_POINT ( 'NONE',  ( -97.64999999999996305, -209.9999999999999716, 87.45999999999999375 ) ) ;
#2487 = CIRCLE ( 'NONE', #21635, 32.00000000000000711 ) ;
#2488 = CYLINDRICAL_SURFACE ( 'NONE', #61222, 2.649999999999999467 ) ;
#2489 = EDGE_LOOP ( 'NONE', ( #3517, #34755, #4345, #25455 ) ) ;
#2490 = ORIENTED_EDGE ( 'NONE', *, *, #28162, .F. ) ;
#2491 = AXIS2_PLACEMENT_3D ( 'NONE', #56724, #28124, #21353 ) ;
#2492 = FACE_OUTER_BOUND ( 'NONE', #52801, .T. ) ;
#2493 = CARTESIAN_POINT ( 'NONE',  ( 2.750000000000000000, 0.000000000000000000, 0.000000000000000000 ) ) ;
#2494 = DIRECTION ( 'NONE',  ( -0.000000000000000000, -0.000000000000000000, 1.000000000000000000 ) ) ;
#2495 = DIRECTION ( 'NONE',  ( 1.000000000000000000, 0.000000000000000000, -0.000000000000000000 ) ) ;
#2496 = DIRECTION ( 'NONE',  ( -1.000000000000000000, 0.000000000000000000, 0.000000000000000000 ) ) ;
#2497 = CARTESIAN_POINT ( 'NONE',  ( -97.30629616937497417, -208.6684592857803011, 75.77864583420048916 ) ) ;
#2498 = EDGE_LOOP ( 'NONE', ( #10615, #56014, #68071, #49433 ) ) ;
#2499 = EDGE_CURVE ( 'NONE', #22473, #67855, #51677, .T. ) ;
#2500 = VECTOR ( 'NONE', #40079, 1000.000000000000000 ) ;
#2501 = DIRECTION ( 'NONE',  ( 1.000000000000000000, 0.000000000000000000, 0.000000000000000000 ) ) ;
#2502 = DIRECTION ( 'NONE',  ( 0.000000000000000000, 0.3090169943749482839, -0.9510565162951533091 ) ) ;
#2503 = ADVANCED_FACE ( 'NONE', ( #29631 ), #64246, .F. ) ;
#2504 = LINE ( 'NONE', #12977, #33234 ) ;
#2505 = EDGE_CURVE ( 'NONE', #6335, #6594, #41666, .T. ) ;
#2506 = CYLINDRICAL_SURFACE ( 'NONE', #25732, 31.99999999999998579 ) ;
#2507 = FACE_OUTER_BOUND ( 'NONE', #72844, .T. ) ;
#2508 = UNCERTAINTY_MEASURE_WITH_UNIT (LENGTH_MEASURE( 1.000000000000000082E-05 ), #45710, 'distance_accuracy_value', 'NONE');
#2509 = CARTESIAN_POINT ( 'NONE',  ( -3.000000000000000000, -22.32062822937469804, -14.36278369418829826 ) ) ;
#2510 = AXIS2_PLACEMENT_3D ( 'NONE', #6403, #24066, #424 ) ;
#2511 = EDGE_CURVE ( 'NONE', #58816, #26361, #8429, .T. ) ;
#2512 = AXIS2_PLACEMENT_3D ( 'NONE', #8401, #1039, #71159 ) ;
#2513 = FACE_OUTER_BOUND ( 'NONE', #69564, .T. ) ;
#2514 = PLANE ( 'NONE',  #41762 ) ;
#2515 = ADVANCED_FACE ( 'NONE', ( #69504 ), #40946, .T. ) ;
#2516 =( BOUNDED_CURVE ( )  B_SPLINE_CURVE ( 2, ( #11798, #69329, #5825, #17096, #219, #23471, #21985 ),
 .UNSPECIFIED., .F., .F. ) 
 B_SPLINE_CURVE_WITH_KNOTS ( ( 3, 2, 2, 3 ),
 ( 0.9583333333333337034, 0.9652777777777781232, 0.9722222222222225430, 0.9791666666666669627 ),
 .UNSPECIFIED. ) 
 CURVE ( )  GEOMETRIC_REPRESENTATION_ITEM ( )  RATIONAL_B_SPLINE_CURVE ( ( 0.9999999999999935607, 0.8660254037844451469, 1.000000000000000000, 0.8660254037844387076, 1.000000000000000000, 0.8660254037844322683, 1.000000000000006439 ) ) 
 REPRESENTATION_ITEM ( '' )  );
#2517 = CARTESIAN_POINT ( 'NONE',  ( 97.30629616937498838, 91.33154071421968467, 84.45697916753383083 ) ) ;
#2518 = CARTESIAN_POINT ( 'NONE',  ( -94.99999999999997158, -207.3369185715606307, 86.46781250086714010 ) ) ;
#2519 = CARTESIAN_POINT ( 'NONE',  ( 10.00000000000000000, 37.22597642581158084, -5.202137450156524068 ) ) ;
#2520 = ORIENTED_EDGE ( 'NONE', *, *, #39666, .F. ) ;
#2521 = EDGE_CURVE ( 'NONE', #14991, #24836, #69662, .T. ) ;
#2522 = CARTESIAN_POINT ( 'NONE',  ( 5.000000000000000000, -56.15606465354917276, -59.75363087400133111 ) ) ;
#2523 = CARTESIAN_POINT ( 'NONE',  ( -94.99999999999997158, -213.0599564267049857, 81.26874999999999716 ) ) ;
#2524 = CARTESIAN_POINT ( 'NONE',  ( -92.69370383062505425, 88.66845928578038638, 76.57239583420046358 ) ) ;
#2525 = CARTESIAN_POINT ( 'NONE',  ( 92.69370383062501162, -211.3315407142195852, 84.61572916753380014 ) ) ;
#2526 = ORIENTED_EDGE ( 'NONE', *, *, #56990, .F. ) ;
#2527 = FILL_AREA_STYLE ('',( #11610 ) ) ;
#2528 = ORIENTED_EDGE ( 'NONE', *, *, #51579, .T. ) ;
#2529 = EDGE_CURVE ( 'NONE', #54682, #42030, #66082, .T. ) ;
#2530 = ORIENTED_EDGE ( 'NONE', *, *, #43715, .F. ) ;
#2531 = CIRCLE ( 'NONE', #34844, 31.99999999999998934 ) ;
#2533 = CIRCLE ( 'NONE', #38549, 77.49899999999999523 ) ;
#2532 = CARTESIAN_POINT ( 'NONE',  ( 11.99999999999999822, -23.16143007188376757, -73.95703589263997912 ) ) ;
#2534 = EDGE_CURVE ( 'NONE', #31921, #51229, #7462, .T. ) ;
#2535 = EDGE_CURVE ( 'NONE', #57809, #63132, #58221, .T. ) ;
#2536 = VERTEX_POINT ( 'NONE', #2230 ) ;
#2537 = DIRECTION ( 'NONE',  ( 0.000000000000000000, -0.9510565162951510887, 0.3090169943749551673 ) ) ;
#2538 = CARTESIAN_POINT ( 'NONE',  ( 95.00000000000000000, -212.6630814284392557, 78.53031250086715431 ) ) ;
#2539 = CARTESIAN_POINT ( 'NONE',  ( -43.60332556124591008, -133.0000000000000000, 2.500000000000002220 ) ) ;
#2540 = EDGE_CURVE ( 'NONE', #32056, #12963, #19470, .T. ) ;
#2541 = CARTESIAN_POINT ( 'NONE',  ( -0.7800914985199643992, -121.2811936832255100, -2.500000000000000000 ) ) ;
#2542 = CARTESIAN_POINT ( 'NONE',  ( 97.64999999999999147, -209.9999999999999716, 80.79249999999998977 ) ) ;
#2543 = DIRECTION ( 'NONE',  ( 0.000000000000000000, 0.000000000000000000, 1.000000000000000000 ) ) ;
#2544 = CARTESIAN_POINT ( 'NONE',  ( -95.00000000000002842, 86.94004357329504273, 83.25312500173430408 ) ) ;
#2545 = CARTESIAN_POINT ( 'NONE',  ( 97.64999999999999147, -209.9999999999999716, 82.69749999999999091 ) ) ;
#2546 = ORIENTED_EDGE ( 'NONE', *, *, #16968, .T. ) ;
#2547 = ORIENTED_EDGE ( 'NONE', *, *, #55991, .F. ) ;
#2548 = ORIENTED_EDGE ( 'NONE', *, *, #44102, .T. ) ;
#2549 = ORIENTED_EDGE ( 'NONE', *, *, #36224, .F. ) ;
#2550 = CARTESIAN_POINT ( 'NONE',  ( 2.500000000000035083, 90.00000000000000000, -279.9999999999999432 ) ) ;
#2551 = CIRCLE ( 'NONE', #3759, 77.49899999999999523 ) ;
#2552 = AXIS2_PLACEMENT_3D ( 'NONE', #71387, #31913, #19889 ) ;
#2553 = CARTESIAN_POINT ( 'NONE',  ( -93.84685191531252713, 88.00268892867056536, 83.66322916753382799 ) ) ;
#2554 = CARTESIAN_POINT ( 'NONE',  ( -93.67499999999998295, -207.7050326799711968, 77.08833333333332405 ) ) ;
#2555 = AXIS2_PLACEMENT_3D ( 'NONE', #54062, #30372, #42045 ) ;
#2556 = PLANE ( 'NONE',  #34190 ) ;
#2557 = CARTESIAN_POINT ( 'NONE',  ( 96.32499999999998863, 87.70503267997126784, 75.60666666666665492 ) ) ;
#2558 = ORIENTED_EDGE ( 'NONE', *, *, #6028, .T. ) ;
#2559 = CARTESIAN_POINT ( 'NONE',  ( -96.32499999999996021, -207.7050326799711968, 84.89354166840095672 ) ) ;
#2560 = ORIENTED_EDGE ( 'NONE', *, *, #1750, .T. ) ;
#2561 = LINE ( 'NONE', #48369, #245 ) ;
#2562 = EDGE_LOOP ( 'NONE', ( #41987, #28970, #17725, #36974 ) ) ;
#2563 = CARTESIAN_POINT ( 'NONE',  ( -92.35000000000003695, 90.00000000000004263, 87.22187500173430408 ) ) ;
#2564 = CARTESIAN_POINT ( 'NONE',  ( 94.99999999999998579, 87.33691857156068750, 86.15031250086714465 ) ) ;
#2565 = CARTESIAN_POINT ( 'NONE',  ( 10.00000000000000000, 0.000000000000000000, 0.000000000000000000 ) ) ;
#2566 = LINE ( 'NONE', #17135, #41037 ) ;
#2567 = DIRECTION ( 'NONE',  ( 0.000000000000000000, 0.8910065241883690090, -0.4539904997395446395 ) ) ;
#2568 = DIRECTION ( 'NONE',  ( 0.3090169943749448977, 0.9510565162951543083, 0.000000000000000000 ) ) ;
#2569 = ORIENTED_EDGE ( 'NONE', *, *, #52387, .F. ) ;
#2570 = CARTESIAN_POINT ( 'NONE',  ( 94.99999999999998579, 90.00000000000002842, 90.00000000000000000 ) ) ;
#2571 = DIRECTION ( 'NONE',  ( 0.000000000000000000, 0.000000000000000000, 1.000000000000000000 ) ) ;
#2572 = VERTEX_POINT ( 'NONE', #6721 ) ;
#2573 = ORIENTED_EDGE ( 'NONE', *, *, #28192, .T. ) ;
#2574 = CARTESIAN_POINT ( 'NONE',  ( -2.500000000000003997, 4.330127018922192761, -6.000000000000000000 ) ) ;
#2575 = CARTESIAN_POINT ( 'NONE',  ( 0.000000000000000000, 0.000000000000000000, 0.000000000000000000 ) ) ;
#2576 = CARTESIAN_POINT ( 'NONE',  ( -97.65000000000004832, -211.5299782133524218, 83.06791666666666174 ) ) ;
#2577 = CARTESIAN_POINT ( 'NONE',  ( -97.30629616937497417, -208.6684592857803011, 85.30364583420048064 ) ) ;
#2578 = ORIENTED_EDGE ( 'NONE', *, *, #34614, .T. ) ;
#2579 = LINE ( 'NONE', #1835, #53727 ) ;
#2580 = VERTEX_POINT ( 'NONE', #42784 ) ;
#2581 = VERTEX_POINT ( 'NONE', #32601 ) ;
#2582 = AXIS2_PLACEMENT_3D ( 'NONE', #25840, #48403, #66447 ) ;
#2583 = AXIS2_PLACEMENT_3D ( 'NONE', #32833, #55782, #22692 ) ;
#2584 = EDGE_CURVE ( 'NONE', #70598, #34383, #43273, .T. ) ;
#2585 = DIRECTION ( 'NONE',  ( -1.000000000000000000, 0.000000000000000000, -0.000000000000000000 ) ) ;
#2586 = VECTOR ( 'NONE', #71315, 1000.000000000000000 ) ;
#2587 = CARTESIAN_POINT ( 'NONE',  ( 94.99999999999998579, 87.33691857156068750, 88.69031250086716511 ) ) ;
#2588 = EDGE_CURVE ( 'NONE', #49292, #19761, #72634, .T. ) ;
#2589 = CARTESIAN_POINT ( 'NONE',  ( 92.69370383062498320, 91.33154071421968467, 82.60489583420049087 ) ) ;
#2590 = CARTESIAN_POINT ( 'NONE',  ( 1.560000000000000053, -1.732050807568877859, -1.752539433813135784E-17 ) ) ;
#2591 = DIRECTION ( 'NONE',  ( -1.000000000000000000, -0.000000000000000000, 0.000000000000000000 ) ) ;
#2592 = CARTESIAN_POINT ( 'NONE',  ( -6.170112525937308412, 10.87104923258428890, 52.00000000000002132 ) ) ;
#2593 = CARTESIAN_POINT ( 'NONE',  ( 0.000000000000000000, 0.000000000000000000, 0.000000000000000000 ) ) ;
#2594 = ADVANCED_FACE ( 'NONE', ( #67193 ), #3694, .T. ) ;
#2596 = EDGE_CURVE ( 'NONE', #67396, #13415, #20952, .T. ) ;
#2595 = CARTESIAN_POINT ( 'NONE',  ( -97.65000000000001990, 90.00003217427526181, 76.74437388893713319 ) ) ;
#2597 = CARTESIAN_POINT ( 'NONE',  ( -23.54415474984308432, -120.4156646670583086, -2.500000000000000000 ) ) ;
#2598 = DIRECTION ( 'NONE',  ( 0.000000000000000000, 0.000000000000000000, 1.000000000000000000 ) ) ;
#2599 = PRODUCT_DEFINITION_CONTEXT ( 'detailed design', #26332, 'design' ) ;
#2600 = CARTESIAN_POINT ( 'NONE',  ( -97.64999999953592180, 89.99996903277666149, 77.38038495128051864 ) ) ;
#2601 = ORIENTED_EDGE ( 'NONE', *, *, #24062, .F. ) ;
#2602 = CARTESIAN_POINT ( 'NONE',  ( -92.69370383062505425, 88.66845928578038638, 88.00239583420047040 ) ) ;
#2603 = CIRCLE ( 'NONE', #23016, 82.00000000000000000 ) ;
#2604 = FACE_OUTER_BOUND ( 'NONE', #63993, .T. ) ;
#2605 = AXIS2_PLACEMENT_3D ( 'NONE', #24717, #8544, #31459 ) ;
#2606 = VECTOR ( 'NONE', #50629, 1000.000000000000000 ) ;
#2607 = EDGE_CURVE ( 'NONE', #61596, #32352, #4060, .T. ) ;
#2608 = DIRECTION ( 'NONE',  ( 0.000000000000000000, -0.8090169943749531134, 0.5877852522924653655 ) ) ;
#2609 = ORIENTED_EDGE ( 'NONE', *, *, #47878, .F. ) ;
#2610 = AXIS2_PLACEMENT_3D ( 'NONE', #25220, #48146, #13187 ) ;
#2611 = DIRECTION ( 'NONE',  ( 0.6575728627325955200, -0.7533909544171997208, 0.000000000000000000 ) ) ;
#2612 = CARTESIAN_POINT ( 'NONE',  ( -26.50000000000000355, -120.0000000000000000, -80.00000000000000000 ) ) ;
#2613 = FACE_OUTER_BOUND ( 'NONE', #73912, .T. ) ;
#2614 = EDGE_CURVE ( 'NONE', #18110, #44000, #8577, .T. ) ;
#2615 = ADVANCED_FACE ( 'NONE', ( #26957 ), #2964, .F. ) ;
#2616 = CARTESIAN_POINT ( 'NONE',  ( 96.15314808468748708, -208.0026889286704943, 80.69989583420047552 ) ) ;
#2617 = VERTEX_POINT ( 'NONE', #38632 ) ;
#2618 = VERTEX_POINT ( 'NONE', #66100 ) ;
#2619 = CARTESIAN_POINT ( 'NONE',  ( 10.00000000000000000, -74.74816331893453025, 33.71516098798714722 ) ) ;
#2620 = VERTEX_POINT ( 'NONE', #66824 ) ;
#2621 = FACE_OUTER_BOUND ( 'NONE', #36232, .T. ) ;
#2622 = FACE_OUTER_BOUND ( 'NONE', #62454, .T. ) ;
#2623 = ORIENTED_EDGE ( 'NONE', *, *, #8125, .T. ) ;
#2624 = DIRECTION ( 'NONE',  ( -0.2867529058022035837, 0.9580045777625452175, 0.000000000000000000 ) ) ;
#2625 = CARTESIAN_POINT ( 'NONE',  ( 97.30629616937498838, -208.6684592857803011, 77.47197916753381719 ) ) ;
#2626 = CIRCLE ( 'NONE', #15789, 31.99999999999999289 ) ;
#2627 = ORIENTED_EDGE ( 'NONE', *, *, #62325, .T. ) ;
#2628 = CARTESIAN_POINT ( 'NONE',  ( 12.00000000000000000, -25.60904388321925040, -6.976881207771167048 ) ) ;
#2629 = VERTEX_POINT ( 'NONE', #20206 ) ;
#2630 = ORIENTED_EDGE ( 'NONE', *, *, #67247, .T. ) ;
#2631 = CARTESIAN_POINT ( 'NONE',  ( 0.000000000000000000, 0.000000000000000000, 0.000000000000000000 ) ) ;
#2632 = AXIS2_PLACEMENT_3D ( 'NONE', #51171, #15859, #38422 ) ;
#2633 = DIRECTION ( 'NONE',  ( -1.000000000000000000, -0.000000000000000000, -0.000000000000000000 ) ) ;
#2634 = ORIENTED_EDGE ( 'NONE', *, *, #24041, .F. ) ;
#2635 = CARTESIAN_POINT ( 'NONE',  ( 12.13205353604972991, -140.1820037904669789, 5.500000000000000000 ) ) ;
#2636 = CARTESIAN_POINT ( 'NONE',  ( 97.64999999999997726, -211.5299782133524502, 83.99395833506763154 ) ) ;
#2637 = CARTESIAN_POINT ( 'NONE',  ( 97.64999999999999147, 90.00000000000002842, 83.96750000000000114 ) ) ;
#2638 = ORIENTED_EDGE ( 'NONE', *, *, #47490, .F. ) ;
#2639 = CARTESIAN_POINT ( 'NONE',  ( -3.961125083139900749, -143.2122702051246677, 5.500000000000000000 ) ) ;
#2640 = VECTOR ( 'NONE', #25446, 1000.000000000000000 ) ;
#2641 = CARTESIAN_POINT ( 'NONE',  ( 12.13205353604972991, -140.1820037904669789, 5.500000000000000000 ) ) ;
#2642 = ORIENTED_EDGE ( 'NONE', *, *, #42778, .T. ) ;
#2643 = ORIENTED_EDGE ( 'NONE', *, *, #20449, .F. ) ;
#2644 = CARTESIAN_POINT ( 'NONE',  ( -93.84685191531254134, 91.99731107132950569, 88.31989583420048007 ) ) ;
#2645 = CARTESIAN_POINT ( 'NONE',  ( 94.99999999999998579, 87.33691857156068750, 80.27656250086714351 ) ) ;
#2646 = ORIENTED_EDGE ( 'NONE', *, *, #28659, .T. ) ;
#2647 = CARTESIAN_POINT ( 'NONE',  ( 94.99999999999998579, 93.05995642670504253, 82.30062500173428930 ) ) ;
#2648 = DIRECTION ( 'NONE',  ( 0.000000000000000000, 0.000000000000000000, 1.000000000000000000 ) ) ;
#2649 = ORIENTED_EDGE ( 'NONE', *, *, #67729, .T. ) ;
#2650 = CARTESIAN_POINT ( 'NONE',  ( -92.34999999999999432, -209.9999999999999716, 86.50750000000000739 ) ) ;
#2651 = CIRCLE ( 'NONE', #54248, 31.99999999999998579 ) ;
#2652 = ORIENTED_EDGE ( 'NONE', *, *, #47022, .F. ) ;
#2653 = AXIS2_PLACEMENT_3D ( 'NONE', #69449, #19420, #42368 ) ;
#2654 = VERTEX_POINT ( 'NONE', #43173 ) ;
#2655 = ORIENTED_EDGE ( 'NONE', *, *, #22354, .T. ) ;
#2656 = CARTESIAN_POINT ( 'NONE',  ( 11.99999999999999822, 39.78640506895698792, -66.50666863321958999 ) ) ;
#2657 = CIRCLE ( 'NONE', #18226, 16.00000000000000000 ) ;
#2658 = FACE_OUTER_BOUND ( 'NONE', #6933, .T. ) ;
#2659 = CARTESIAN_POINT ( 'NONE',  ( -95.00000000000002842, 86.94004357329504273, 85.07874999999999943 ) ) ;
#2660 = VERTEX_POINT ( 'NONE', #14949 ) ;
#2661 = CARTESIAN_POINT ( 'NONE',  ( 11.99999999999999822, -76.66974797899844418, 11.30684508768314522 ) ) ;
#2662 = CARTESIAN_POINT ( 'NONE',  ( 0.000000000000000000, 0.000000000000000000, 0.000000000000000000 ) ) ;
#2663 = ORIENTED_EDGE ( 'NONE', *, *, #20184, .T. ) ;
#2664 = CARTESIAN_POINT ( 'NONE',  ( 11.99999999999999822, 33.71516098798849015, -74.74816331893393340 ) ) ;
#2665 = CARTESIAN_POINT ( 'NONE',  ( -92.69370383062498320, -208.6684592857803011, 78.58322916753381548 ) ) ;
#2666 = ORIENTED_EDGE ( 'NONE', *, *, #47521, .F. ) ;
#2667 = DIRECTION ( 'NONE',  ( -0.1850432970638682395, 0.9827303690289280746, 0.000000000000000000 ) ) ;
#2668 = DIRECTION ( 'NONE',  ( -1.000000000000000000, 0.000000000000000000, 0.000000000000000000 ) ) ;
#2669 = DIRECTION ( 'NONE',  ( -1.000000000000000000, 0.000000000000000000, 0.000000000000000000 ) ) ;
#2670 = CARTESIAN_POINT ( 'NONE',  ( 10.00000000000000000, 4.992566952384984269, 37.16516213103279398 ) ) ;
#2671 = EDGE_CURVE ( 'NONE', #22209, #16806, #61189, .T. ) ;
#2672 = CARTESIAN_POINT ( 'NONE',  ( 93.67500000000001137, -207.7050326799711968, 83.62354166840097491 ) ) ;
#2673 = ADVANCED_FACE ( 'NONE', ( #21310 ), #9679, .T. ) ;
#2674 = DIRECTION ( 'NONE',  ( -1.000000000000000000, 0.000000000000000000, 0.000000000000000000 ) ) ;
#2675 = PLANE ( 'NONE',  #31570 ) ;
#2676 = CARTESIAN_POINT ( 'NONE',  ( 10.00000000000000000, 77.49459641780886443, -0.8261519478433788644 ) ) ;
#2678 = EDGE_CURVE ( 'NONE', #23574, #16444, #67840, .T. ) ;
#2677 = CYLINDRICAL_SURFACE ( 'NONE', #16447, 16.00000000000000000 ) ;
#2679 = CARTESIAN_POINT ( 'NONE',  ( -95.00000000000002842, 87.33691857156074434, 89.32531250086715602 ) ) ;
#2680 = FACE_OUTER_BOUND ( 'NONE', #5977, .T. ) ;
#2681 = DIRECTION ( 'NONE',  ( -1.000000000000000000, -0.000000000000000000, -0.000000000000000000 ) ) ;
#2682 = DIRECTION ( 'NONE',  ( 0.000000000000000000, 0.000000000000000000, 1.000000000000000000 ) ) ;
#2683 = ADVANCED_FACE ( 'NONE', ( #10046 ), #55913, .T. ) ;
#2684 = LINE ( 'NONE', #60176, #47258 ) ;
#2685 = STYLED_ITEM ( 'NONE', ( #59897 ), #3205 ) ;
#2686 = CIRCLE ( 'NONE', #44672, 77.49899999999998101 ) ;
#2687 = CYLINDRICAL_SURFACE ( 'NONE', #59335, 31.99999999999998579 ) ;
#2688 = CARTESIAN_POINT ( 'NONE',  ( 93.84685191531248449, 91.99731107132950569, 89.06072916753382174 ) ) ;
#2689 = CARTESIAN_POINT ( 'NONE',  ( 32.50000000000000000, -120.0000000000000000, 2.500000000000000000 ) ) ;
#2690 = DIRECTION ( 'NONE',  ( -1.000000000000000000, 0.000000000000000000, 0.000000000000000000 ) ) ;
#2691 = CIRCLE ( 'NONE', #17031, 31.99999999999998579 ) ;
#2692 = DIRECTION ( 'NONE',  ( 0.000000000000000000, 0.000000000000000000, 1.000000000000000000 ) ) ;
#2693 = CARTESIAN_POINT ( 'NONE',  ( -92.34999999999999432, -209.9999999999999716, 88.41249999999999432 ) ) ;
#2694 = ADVANCED_FACE ( 'NONE', ( #32965 ), #8941, .F. ) ;
#2695 = AXIS2_PLACEMENT_3D ( 'NONE', #30078, #3029, #35711 ) ;
#2696 = CARTESIAN_POINT ( 'NONE',  ( 24.95699195200416654, -110.9640411295978595, 2.500000000000000000 ) ) ;
#2697 = ADVANCED_FACE ( 'NONE', ( #60457 ), #31858, .T. ) ;
#2698 = VECTOR ( 'NONE', #10737, 1000.000000000000000 ) ;
#2699 = ORIENTED_EDGE ( 'NONE', *, *, #21892, .F. ) ;
#2700 = DIRECTION ( 'NONE',  ( 0.000000000000000000, 0.000000000000000000, 1.000000000000000000 ) ) ;
#2701 = CARTESIAN_POINT ( 'NONE',  ( 92.35001072685611234, -211.5299844065056902, 78.06729209680055703 ) ) ;
#2702 = EDGE_CURVE ( 'NONE', #73774, #55313, #72084, .T. ) ;
#2703 = EDGE_LOOP ( 'NONE', ( #42664, #9447, #53288, #40165 ) ) ;
#2704 = CARTESIAN_POINT ( 'NONE',  ( 10.00000000000000000, 0.000000000000000000, 0.000000000000000000 ) ) ;
#2705 = DIRECTION ( 'NONE',  ( 0.000000000000000000, -1.000000000000000000, 0.000000000000000000 ) ) ;
#2706 = ORIENTED_EDGE ( 'NONE', *, *, #48892, .T. ) ;
#2707 = CARTESIAN_POINT ( 'NONE',  ( 95.00000000000000000, -207.3369185715606307, 82.49906250086715431 ) ) ;
#2708 = CARTESIAN_POINT ( 'NONE',  ( 92.69370383062501162, -209.9999999999999716, 89.80156250086714920 ) ) ;
#2709 = ORIENTED_EDGE ( 'NONE', *, *, #42608, .T. ) ;
#2710 = CARTESIAN_POINT ( 'NONE',  ( 5.999999999999999112, 64.81221759200415988, -50.23322058963276504 ) ) ;
#2711 = ORIENTED_EDGE ( 'NONE', *, *, #39044, .F. ) ;
#2712 = CARTESIAN_POINT ( 'NONE',  ( -0.1219594728601508804, -118.5049662589159567, -2.500000000000000000 ) ) ;
#2713 = ORIENTED_EDGE ( 'NONE', *, *, #22413, .F. ) ;
#2714 = CARTESIAN_POINT ( 'NONE',  ( -96.15314808468752972, 91.99731107132950569, 78.26572916753382003 ) ) ;
#2715 = ORIENTED_EDGE ( 'NONE', *, *, #48309, .T. ) ;
#2716 = VERTEX_POINT ( 'NONE', #60819 ) ;
#2717 = DIRECTION ( 'NONE',  ( -0.000000000000000000, -0.000000000000000000, -1.000000000000000000 ) ) ;
#2718 = ORIENTED_EDGE ( 'NONE', *, *, #19405, .F. ) ;
#2719 = FACE_OUTER_BOUND ( 'NONE', #6414, .T. ) ;
#2720 = DIRECTION ( 'NONE',  ( 0.000000000000000000, 0.3090169943749410675, 0.9510565162951556406 ) ) ;
#2721 = EDGE_LOOP ( 'NONE', ( #34967, #21826, #70511, #58260 ) ) ;
#2722 = DIRECTION ( 'NONE',  ( -0.000000000000000000, 0.8090169943749503378, 0.5877852522924690293 ) ) ;
#2723 = VERTEX_POINT ( 'NONE', #9301 ) ;
#2724 =( BOUNDED_CURVE ( )  B_SPLINE_CURVE ( 2, ( #35371, #52653, #41380, #460, #58665, #17703, #12062 ),
 .UNSPECIFIED., .F., .F. ) 
 B_SPLINE_CURVE_WITH_KNOTS ( ( 3, 2, 2, 3 ),
 ( 0.1041666666666670182, 0.1111111111111114103, 0.1180555555555558161, 0.1250000000000002220 ),
 .UNSPECIFIED. ) 
 CURVE ( )  GEOMETRIC_REPRESENTATION_ITEM ( )  RATIONAL_B_SPLINE_CURVE ( ( 0.9999999999999933387, 0.8660254037844453689, 1.000000000000000000, 0.8660254037844387076, 1.000000000000000000, 0.8660254037844343777, 1.000000000000004219 ) ) 
 REPRESENTATION_ITEM ( '' )  );
#2725 = CARTESIAN_POINT ( 'NONE',  ( 0.000000000000000000, 66.50666863322055633, -39.78640506895536078 ) ) ;
#2726 = EDGE_LOOP ( 'NONE', ( #54837, #44802, #69623, #30782 ) ) ;
#2727 = EDGE_CURVE ( 'NONE', #57712, #52639, #31859, .T. ) ;
#2728 = COLOUR_RGB ( '', 0.72549020, 0.75294118, 0.79215686) ;
#2729 = ORIENTED_EDGE ( 'NONE', *, *, #17511, .F. ) ;
#2730 = EDGE_LOOP ( 'NONE', ( #43648, #11853, #10232, #41324 ) ) ;
#2731 = CARTESIAN_POINT ( 'NONE',  ( 92.69370383062501162, -209.9999999999999716, 78.21281250086714465 ) ) ;
#2732 = DIRECTION ( 'NONE',  ( 0.000000000000000000, 0.000000000000000000, 1.000000000000000000 ) ) ;
#2733 = CONTEXT_DEPENDENT_SHAPE_REPRESENTATION ( #18642, #19471 ) ;
#2734 = CARTESIAN_POINT ( 'NONE',  ( 97.64999999999999147, 90.00000000000002842, 90.00000000000000000 ) ) ;
#2735 = VERTEX_POINT ( 'NONE', #34839 ) ;
#2737 = CARTESIAN_POINT ( 'NONE',  ( -92.34999999999999432, -211.5299782133524218, 78.91395833506763324 ) ) ;
#2736 = AXIS2_PLACEMENT_3D ( 'NONE', #604, #34398, #11468 ) ;
#2738 = ORIENTED_EDGE ( 'NONE', *, *, #40000, .T. ) ;
#2739 = CARTESIAN_POINT ( 'NONE',  ( 11.99999999999999822, 0.000000000000000000, 0.000000000000000000 ) ) ;
#2740 = CYLINDRICAL_SURFACE ( 'NONE', #69209, 2.649999999999999467 ) ;
#2741 = EDGE_CURVE ( 'NONE', #32448, #64295, #40471, .T. ) ;
#2742 = DIRECTION ( 'NONE',  ( -1.000000000000000000, 0.000000000000000000, 0.000000000000000000 ) ) ;
#2743 = CARTESIAN_POINT ( 'NONE',  ( 10.00000000000000000, 66.50666863322000211, 39.78640506895629869 ) ) ;
#2744 = CARTESIAN_POINT ( 'NONE',  ( -94.99999999999997158, -207.3369185715606307, 80.59406250086715318 ) ) ;
#2745 = EDGE_CURVE ( 'NONE', #32355, #66201, #56675, .T. ) ;
#2746 = CARTESIAN_POINT ( 'NONE',  ( -92.69370383062502583, 88.66845928578038638, 80.54114583420049200 ) ) ;
#2747 = AXIS2_PLACEMENT_3D ( 'NONE', #4317, #55800, #50893 ) ;
#2748 = ORIENTED_EDGE ( 'NONE', *, *, #8772, .F. ) ;
#2749 = CARTESIAN_POINT ( 'NONE',  ( 92.69370383062498320, 91.33154071421968467, 81.33489583420048064 ) ) ;
#2750 = AXIS2_PLACEMENT_3D ( 'NONE', #51429, #69825, #23260 ) ;
#2751 = EDGE_LOOP ( 'NONE', ( #12229, #62623, #61997, #60581 ) ) ;
#2752 = FACE_OUTER_BOUND ( 'NONE', #72336, .T. ) ;
#2753 = DIRECTION ( 'NONE',  ( 1.000000000000000000, -0.000000000000000000, 0.000000000000000000 ) ) ;
#2754 = CARTESIAN_POINT ( 'NONE',  ( -96.32499999999996021, -212.2949673200287179, 76.77083333333332860 ) ) ;
#2755 = DIRECTION ( 'NONE',  ( 0.02332147558787931590, 0.9997280174009348652, -0.000000000000000000 ) ) ;
#2756 = DIRECTION ( 'NONE',  ( 0.000000000000000000, 0.000000000000000000, 1.000000000000000000 ) ) ;
#2757 = CARTESIAN_POINT ( 'NONE',  ( -97.30629616937497417, -211.3315407142195852, 81.44072916753380298 ) ) ;
#2758 = EDGE_CURVE ( 'NONE', #7483, #63916, #28822, .T. ) ;
#2759 = CARTESIAN_POINT ( 'NONE',  ( 0.9774260708577211521, -121.1378217241763622, 2.500000000000000000 ) ) ;
#2760 = CARTESIAN_POINT ( 'NONE',  ( 10.00000000000000000, 17.67226234102826510, 33.17418723428314564 ) ) ;
#2761 = DIRECTION ( 'NONE',  ( 0.000000000000000000, -0.3090169943749349057, -0.9510565162951576390 ) ) ;
#2762 = ORIENTED_EDGE ( 'NONE', *, *, #2758, .T. ) ;
#2763 = ORIENTED_EDGE ( 'NONE', *, *, #29843, .F. ) ;
#2764 = DIRECTION ( 'NONE',  ( 0.000000000000000000, -1.000000000000000000, -1.047444401652940007E-14 ) ) ;
#2765 = CARTESIAN_POINT ( 'NONE',  ( -97.65000000000001990, 88.47002178664754979, 75.44791666666667140 ) ) ;
#2766 = DIRECTION ( 'NONE',  ( -1.000000000000000000, -0.000000000000000000, 0.000000000000000000 ) ) ;
#2767 = CARTESIAN_POINT ( 'NONE',  ( -93.84685191531254134, 91.99731107132950569, 83.71614583420047495 ) ) ;
#2768 = CARTESIAN_POINT ( 'NONE',  ( -97.19210266091309336, -208.8322938842643168, 74.89296886168689582 ) ) ;
#2769 = CARTESIAN_POINT ( 'NONE',  ( 10.00000000000000000, 72.35432306680455383, 20.40083707023012494 ) ) ;
#2770 = DIRECTION ( 'NONE',  ( 0.000000000000000000, 0.9510565162951521989, 0.3090169943749515591 ) ) ;
#2771 = EDGE_CURVE ( 'NONE', #41920, #17282, #12242, .T. ) ;
#2772 = ORIENTED_EDGE ( 'NONE', *, *, #11899, .F. ) ;
#2773 = CARTESIAN_POINT ( 'NONE',  ( -92.69370383062504004, 89.06968361095763953, 74.68334086212732359 ) ) ;
#2774 = DIRECTION ( 'NONE',  ( -0.000000000000000000, 0.1045284632676569680, 0.9945218953682730678 ) ) ;
#2775 = DIRECTION ( 'NONE',  ( 0.000000000000000000, 0.000000000000000000, -1.000000000000000000 ) ) ;
#2776 = CYLINDRICAL_SURFACE ( 'NONE', #58571, 2.649999999999985700 ) ;
#2777 = DIRECTION ( 'NONE',  ( -1.000000000000000000, -0.000000000000000000, 0.000000000000000000 ) ) ;
#2778 = FACE_OUTER_BOUND ( 'NONE', #230, .T. ) ;
#2779 = CARTESIAN_POINT ( 'NONE',  ( -92.69370383062498320, -209.9999999999999716, 81.22906250086715829 ) ) ;
#2780 = EDGE_CURVE ( 'NONE', #26458, #72049, #50651, .T. ) ;
#2781 = CARTESIAN_POINT ( 'NONE',  ( 10.00000000000000000, -35.38097989696503021, -12.42422080174676147 ) ) ;
#2782 = EDGE_CURVE ( 'NONE', #44699, #57645, #37233, .T. ) ;
#2783 = EDGE_CURVE ( 'NONE', #20472, #61501, #4829, .T. ) ;
#2784 = CARTESIAN_POINT ( 'NONE',  ( 21.07894319797337701, -103.8699611390234878, -5.500000000000000000 ) ) ;
#2785 = CARTESIAN_POINT ( 'NONE',  ( -100.0000000000260485, 95.00000000000001421, 75.00000000000001421 ) ) ;
#2786 = DIRECTION ( 'NONE',  ( -1.000000000000000000, -0.000000000000000000, 0.000000000000000000 ) ) ;
#2787 = VERTEX_POINT ( 'NONE', #73194 ) ;
#2788 = CARTESIAN_POINT ( 'NONE',  ( 10.00000000000000000, -77.49459641780886443, 0.8261519478428377417 ) ) ;
#2789 = CARTESIAN_POINT ( 'NONE',  ( 10.00000000000000000, -62.20884554314051940, 46.21855187248608132 ) ) ;
#2790 = CARTESIAN_POINT ( 'NONE',  ( 11.99999999999999822, -77.49459641780886443, -0.8261519478439277586 ) ) ;
#2791 = AXIS2_PLACEMENT_3D ( 'NONE', #23869, #17485, #40412 ) ;
#2792 = LINE ( 'NONE', #42986, #27681 ) ;
#2793 = CARTESIAN_POINT ( 'NONE',  ( 93.84685191531249870, -208.0026889286704943, 87.79072916753381151 ) ) ;
#2794 = VERTEX_POINT ( 'NONE', #45392 ) ;
#2795 = FACE_OUTER_BOUND ( 'NONE', #71475, .T. ) ;
#2796 = DIRECTION ( 'NONE',  ( 1.000000000000000000, -0.000000000000000000, -0.000000000000000000 ) ) ;
#2797 = ORIENTED_EDGE ( 'NONE', *, *, #40085, .T. ) ;
#2798 = AXIS2_PLACEMENT_3D ( 'NONE', #44666, #50650, #28092 ) ;
#2799 = DIRECTION ( 'NONE',  ( 0.000000000000000000, 0.000000000000000000, 1.000000000000000000 ) ) ;
#2800 = VERTEX_POINT ( 'NONE', #21694 ) ;
#2801 = DIRECTION ( 'NONE',  ( 0.000000000000000000, 1.000000000000000000, 0.000000000000000000 ) ) ;
#2802 = AXIS2_PLACEMENT_3D ( 'NONE', #5993, #11237, #68766 ) ;
#2803 = ORIENTED_EDGE ( 'NONE', *, *, #25974, .F. ) ;
#2804 = VERTEX_POINT ( 'NONE', #10414 ) ;
#2805 = ORIENTED_EDGE ( 'NONE', *, *, #18353, .F. ) ;
#2806 = ORIENTED_EDGE ( 'NONE', *, *, #57155, .T. ) ;
#2807 = DIRECTION ( 'NONE',  ( 0.000000000000000000, 0.000000000000000000, 1.000000000000000000 ) ) ;
#2808 = ORIENTED_EDGE ( 'NONE', *, *, #40826, .F. ) ;
#2809 = ORIENTED_EDGE ( 'NONE', *, *, #26416, .T. ) ;
#2810 = CARTESIAN_POINT ( 'NONE',  ( 93.84685191531248449, 88.00268892867053694, 79.74739583420048916 ) ) ;
#2811 = DIRECTION ( 'NONE',  ( 0.000000000000000000, 0.000000000000000000, 1.000000000000000000 ) ) ;
#2812 = FACE_OUTER_BOUND ( 'NONE', #64835, .T. ) ;
#2813 = ORIENTED_EDGE ( 'NONE', *, *, #40858, .F. ) ;
#2814 = ORIENTED_EDGE ( 'NONE', *, *, #59753, .T. ) ;
#2815 = EDGE_CURVE ( 'NONE', #73400, #54114, #21592, .T. ) ;
#2816 = ORIENTED_EDGE ( 'NONE', *, *, #74295, .F. ) ;
#2817 = FACE_OUTER_BOUND ( 'NONE', #24401, .T. ) ;
#2818 = ORIENTED_EDGE ( 'NONE', *, *, #7831, .F. ) ;
#2819 = DIRECTION ( 'NONE',  ( 5.437773009819413426E-16, -6.230136962689586602E-16, 0.9999999999999997780 ) ) ;
#2820 = DIRECTION ( 'NONE',  ( 0.000000000000000000, -0.9969173337331287410, 0.07845909572783489605 ) ) ;
#2821 = LINE ( 'NONE', #26077, #61572 ) ;
#2822 = DIRECTION ( 'NONE',  ( 1.000000000000000000, 0.000000000000000000, -0.000000000000000000 ) ) ;
#2823 = DIRECTION ( 'NONE',  ( -1.000000000000000000, 0.000000000000000000, -0.000000000000000000 ) ) ;
#2824 = EDGE_CURVE ( 'NONE', #9802, #55839, #28443, .T. ) ;
#2825 = CARTESIAN_POINT ( 'NONE',  ( 10.00000000000000000, -10.96151621346461447, -35.95386929396268272 ) ) ;
#2826 = CARTESIAN_POINT ( 'NONE',  ( 10.00000000000000000, -37.01155633439053361, -6.555932627142825986 ) ) ;
#2827 = CARTESIAN_POINT ( 'NONE',  ( -92.34999999999999432, -208.4700217866474645, 76.47979166840096354 ) ) ;
#2828 = EDGE_CURVE ( 'NONE', #28379, #23563, #72941, .T. ) ;
#2829 = DIRECTION ( 'NONE',  ( 0.000000000000000000, 0.07845909572783793529, 0.9969173337331285190 ) ) ;
#2830 = AXIS2_PLACEMENT_3D ( 'NONE', #11877, #46474, #57763 ) ;
#2832 = CARTESIAN_POINT ( 'NONE',  ( -93.67500000000003979, 87.70503267997129626, 77.59104166840097605 ) ) ;
#2831 = CARTESIAN_POINT ( 'NONE',  ( 94.99999999999998579, 93.05995642670504253, 76.58562500173430010 ) ) ;
#2833 = ORIENTED_EDGE ( 'NONE', *, *, #52136, .T. ) ;
#2834 = CARTESIAN_POINT ( 'NONE',  ( 96.15314808468748708, 88.00268892867053694, 76.04322916753382344 ) ) ;
#2835 = LINE ( 'NONE', #8064, #42152 ) ;
#2836 = CARTESIAN_POINT ( 'NONE',  ( 10.00000000000000000, 0.000000000000000000, 0.000000000000000000 ) ) ;
#2837 = CARTESIAN_POINT ( 'NONE',  ( 3.000000000000000000, 2.935248768560057897, -3.252606517456513302E-15 ) ) ;
#2838 = CARTESIAN_POINT ( 'NONE',  ( -96.32500000000001705, 92.29496732002878900, 78.54354166840096241 ) ) ;
#2839 = CARTESIAN_POINT ( 'NONE',  ( 0.000000000000000000, 37.48860685352291000, 0.8828120875901893649 ) ) ;
#2840 = EDGE_CURVE ( 'NONE', #58070, #55829, #4811, .T. ) ;
#2841 = AXIS2_PLACEMENT_3D ( 'NONE', #2466, #71564, #14429 ) ;
#2842 = ORIENTED_EDGE ( 'NONE', *, *, #51935, .T. ) ;
#2843 = DIRECTION ( 'NONE',  ( -1.000000000000000000, 0.000000000000000000, -0.000000000000000000 ) ) ;
#2844 = DIRECTION ( 'NONE',  ( 0.000000000000000000, 0.000000000000000000, -1.000000000000000000 ) ) ;
#2845 = ORIENTED_EDGE ( 'NONE', *, *, #10162, .F. ) ;
#2846 = ORIENTED_EDGE ( 'NONE', *, *, #65954, .F. ) ;
#2847 = DIRECTION ( 'NONE',  ( 0.000000000000000000, 0.9510565162951523099, 0.3090169943749517811 ) ) ;
#2848 = DIRECTION ( 'NONE',  ( 0.000000000000000000, 0.2334453638559058908, -0.9723699203976764460 ) ) ;
#2849 = DIRECTION ( 'NONE',  ( 0.000000000000000000, 0.9781476007338069101, -0.2079116908177532086 ) ) ;
#2850 = FACE_OUTER_BOUND ( 'NONE', #1422, .T. ) ;
#2851 = DIRECTION ( 'NONE',  ( -1.000000000000000000, -0.000000000000000000, 0.000000000000000000 ) ) ;
#2852 = CARTESIAN_POINT ( 'NONE',  ( 11.99999999999999822, -70.52718814184240159, -26.02418014898383802 ) ) ;
#2853 = EDGE_CURVE ( 'NONE', #60113, #31095, #1004, .T. ) ;
#2854 = ORIENTED_EDGE ( 'NONE', *, *, #39839, .T. ) ;
#2855 = LINE ( 'NONE', #8832, #70358 ) ;
#2856 = CIRCLE ( 'NONE', #36460, 31.99999999999998579 ) ;
#2857 = AXIS2_PLACEMENT_3D ( 'NONE', #9383, #49598, #19912 ) ;
#2858 = DIRECTION ( 'NONE',  ( 0.000000000000000000, 0.8910065241883655673, 0.4539904997395510233 ) ) ;
#2859 = DIRECTION ( 'NONE',  ( -1.000000000000000000, 0.000000000000000000, 0.000000000000000000 ) ) ;
#2860 = CARTESIAN_POINT ( 'NONE',  ( 0.000000000000000000, 71.87247863392413194, 39.47590169984871267 ) ) ;
#2861 = CARTESIAN_POINT ( 'NONE',  ( 0.000000000000000000, -2.663952781845850826, -41.91543099594819921 ) ) ;
#2862 = CARTESIAN_POINT ( 'NONE',  ( 97.64999999999999147, -210.0000000983658026, 80.23687499810812085 ) ) ;
#2863 = CARTESIAN_POINT ( 'NONE',  ( -93.67499999999998295, -207.7050326799711968, 77.80270833506763495 ) ) ;
#2864 = DIRECTION ( 'NONE',  ( -1.000000000000000000, 0.000000000000000000, -0.000000000000000000 ) ) ;
#2865 = EDGE_CURVE ( 'NONE', #57786, #15718, #41784, .T. ) ;
#2866 = ADVANCED_FACE ( 'NONE', ( #16432 ), #65068, .F. ) ;
#2867 = CARTESIAN_POINT ( 'NONE',  ( 92.69370383062498320, 90.00000000000002842, 85.35656250086715602 ) ) ;
#2868 = AXIS2_PLACEMENT_3D ( 'NONE', #12120, #35427, #47091 ) ;
#2869 = CARTESIAN_POINT ( 'NONE',  ( -93.84685191531247028, -211.9973110713294489, 83.02822916753380866 ) ) ;
#2870 = DIRECTION ( 'NONE',  ( 0.000000000000000000, -0.9945218953682745111, 0.1045284632676429237 ) ) ;
#2871 = ORIENTED_EDGE ( 'NONE', *, *, #7905, .F. ) ;
#2872 = CARTESIAN_POINT ( 'NONE',  ( 0.000000000000000000, 81.90746397400393164, -3.894527615416979671 ) ) ;
#2873 = CARTESIAN_POINT ( 'NONE',  ( -96.32499999999996021, -212.2949673200287179, 76.77083333333332860 ) ) ;
#2874 = CARTESIAN_POINT ( 'NONE',  ( 0.000000000000000000, 0.000000000000000000, 0.000000000000000000 ) ) ;
#2875 = CARTESIAN_POINT ( 'NONE',  ( 92.69370383062501162, -211.3315407142195852, 82.71072916753379900 ) ) ;
#2876 = ORIENTED_EDGE ( 'NONE', *, *, #65855, .F. ) ;
#2877 = AXIS2_PLACEMENT_3D ( 'NONE', #16872, #21757, #29236 ) ;
#2878 = FACE_OUTER_BOUND ( 'NONE', #21917, .T. ) ;
#2879 = ORIENTED_EDGE ( 'NONE', *, *, #37598, .T. ) ;
#2880 = ORIENTED_EDGE ( 'NONE', *, *, #9602, .T. ) ;
#2881 = CIRCLE ( 'NONE', #62941, 82.00000000000000000 ) ;
#2882 = EDGE_CURVE ( 'NONE', #54619, #42737, #31756, .T. ) ;
#2883 = FACE_BOUND ( 'NONE', #6394, .T. ) ;
#2884 = VECTOR ( 'NONE', #32891, 1000.000000000000000 ) ;
#2885 = VERTEX_POINT ( 'NONE', #22837 ) ;
#2886 = PLANE ( 'NONE',  #28775 ) ;
#2887 = CARTESIAN_POINT ( 'NONE',  ( 92.69370383062501162, -209.9999999999999716, 78.37156250086715659 ) ) ;
#2888 = DIRECTION ( 'NONE',  ( 0.000000000000000000, 0.000000000000000000, 1.000000000000000000 ) ) ;
#2889 = CARTESIAN_POINT ( 'NONE',  ( -96.32500000000001705, 92.29496732002878900, 76.63854166840096127 ) ) ;
#2890 = EDGE_CURVE ( 'NONE', #61621, #67171, #39759, .T. ) ;
#2891 = CIRCLE ( 'NONE', #60511, 32.00000000000000000 ) ;
#2892 = CARTESIAN_POINT ( 'NONE',  ( -3.308722450212110699E-21, 16.95692799528845995, 2.500000000000000000 ) ) ;
#2893 = CARTESIAN_POINT ( 'NONE',  ( 15.00000000000000000, 16.83928648764922542, -16.46020748918050458 ) ) ;
#2894 = VECTOR ( 'NONE', #59999, 1000.000000000000000 ) ;
#2895 = CARTESIAN_POINT ( 'NONE',  ( 97.64999999999999147, 89.99999999755287661, 75.15687493081163950 ) ) ;
#2896 = CARTESIAN_POINT ( 'NONE',  ( 95.00000000000000000, -206.9400435732949575, 82.85625000000000284 ) ) ;
#2897 = EDGE_CURVE ( 'NONE', #13869, #2268, #63387, .T. ) ;
#2898 = ORIENTED_EDGE ( 'NONE', *, *, #29089, .F. ) ;
#2899 = ORIENTED_EDGE ( 'NONE', *, *, #49915, .F. ) ;
#2900 = EDGE_LOOP ( 'NONE', ( #16411, #48435, #30762, #25608 ) ) ;
#2901 = VECTOR ( 'NONE', #19819, 1000.000000000000000 ) ;
#2902 = VERTEX_POINT ( 'NONE', #45779 ) ;
#2903 = DIRECTION ( 'NONE',  ( -0.000000000000000000, -0.000000000000000000, -1.000000000000000000 ) ) ;
#2904 = CIRCLE ( 'NONE', #66529, 77.49900000000000944 ) ;
#2905 = EDGE_CURVE ( 'NONE', #68809, #19857, #17741, .T. ) ;
#2906 = CARTESIAN_POINT ( 'NONE',  ( -92.69370383062502583, 88.66845928578038638, 82.44614583420049314 ) ) ;
#2907 = DIRECTION ( 'NONE',  ( -1.000000000000000000, 0.000000000000000000, 0.000000000000000000 ) ) ;
#2908 = DIRECTION ( 'NONE',  ( -1.000000000000000000, -0.000000000000000000, -0.000000000000000000 ) ) ;
#2909 = ADVANCED_FACE ( 'NONE', ( #9066 ), #16103, .T. ) ;
#2910 = CARTESIAN_POINT ( 'NONE',  ( 96.32499999999997442, 92.29496732002878900, 75.81833333333332803 ) ) ;
#2911 = CARTESIAN_POINT ( 'NONE',  ( 0.000000000000000000, 75.11725578898467859, 2.956366410620910656 ) ) ;
#2912 = ORIENTED_EDGE ( 'NONE', *, *, #47229, .F. ) ;
#2913 = CARTESIAN_POINT ( 'NONE',  ( -97.64999999999994884, -211.5299782133524502, 86.32229166840097889 ) ) ;
#2914 = ORIENTED_EDGE ( 'NONE', *, *, #45284, .F. ) ;
#2915 = DIRECTION ( 'NONE',  ( -0.000000000000000000, -0.000000000000000000, -1.000000000000000000 ) ) ;
#2916 = ORIENTED_EDGE ( 'NONE', *, *, #5879, .T. ) ;
#2917 = CARTESIAN_POINT ( 'NONE',  ( -93.67500000000003979, 87.70503267997129626, 85.21104166840096639 ) ) ;
#2918 = ORIENTED_EDGE ( 'NONE', *, *, #54166, .F. ) ;
#2919 = CARTESIAN_POINT ( 'NONE',  ( 96.15314808468748708, 88.00268892867053694, 86.20322916753382003 ) ) ;
#2920 = LINE ( 'NONE', #26550, #46624 ) ;
#2921 = CARTESIAN_POINT ( 'NONE',  ( 0.000000000000000000, 24.73286445877808148, -73.44644590900034586 ) ) ;
#2922 = DIRECTION ( 'NONE',  ( 0.000000000000000000, 0.000000000000000000, 1.000000000000000000 ) ) ;
#2923 = ADVANCED_FACE ( 'NONE', ( #4474 ), #17220, .T. ) ;
#2924 = CARTESIAN_POINT ( 'NONE',  ( -30.50000000000000000, -120.0000000000000000, 2.500000000000000000 ) ) ;
#2925 = ORIENTED_EDGE ( 'NONE', *, *, #72549, .F. ) ;
#2926 = CARTESIAN_POINT ( 'NONE',  ( 2.500000000000003109, -4.330127018922192761, -6.000000000000000000 ) ) ;
#2927 = CARTESIAN_POINT ( 'NONE',  ( 1.560000000000000053, 0.8660254037844389297, 1.500000000000000000 ) ) ;
#2928 = VERTEX_POINT ( 'NONE', #61981 ) ;
#2929 = VERTEX_POINT ( 'NONE', #5221 ) ;
#2930 = CYLINDRICAL_SURFACE ( 'NONE', #55360, 16.00000000000000000 ) ;
#2931 = CYLINDRICAL_SURFACE ( 'NONE', #60054, 31.99999999999999289 ) ;
#2932 = AXIS2_PLACEMENT_3D ( 'NONE', #48759, #2934, #20926 ) ;
#2933 = EDGE_CURVE ( 'NONE', #58686, #41070, #14135, .T. ) ;
#2934 = DIRECTION ( 'NONE',  ( -1.000000000000000000, 0.000000000000000000, 0.000000000000000000 ) ) ;
#2935 =( BOUNDED_CURVE ( )  B_SPLINE_CURVE ( 2, ( #23444, #41110, #34342, #46748, #18167, #12147, #919 ),
 .UNSPECIFIED., .F., .F. ) 
 B_SPLINE_CURVE_WITH_KNOTS ( ( 3, 2, 2, 3 ),
 ( 0.5833333333333329263, 0.5902777777777776791, 0.5972222222222223209, 0.6041666666666670737 ),
 .UNSPECIFIED. ) 
 CURVE ( )  GEOMETRIC_REPRESENTATION_ITEM ( )  RATIONAL_B_SPLINE_CURVE ( ( 1.000000000000008660, 0.8660254037844301589, 1.000000000000000000, 0.8660254037844387076, 1.000000000000000000, 0.8660254037844301589, 1.000000000000008660 ) ) 
 REPRESENTATION_ITEM ( '' )  );
#2936 = CARTESIAN_POINT ( 'NONE',  ( -97.30629616937497417, -211.3315407142195852, 84.77447916753381207 ) ) ;
#2937 = ORIENTED_EDGE ( 'NONE', *, *, #64890, .F. ) ;
#2938 = DIRECTION ( 'NONE',  ( -0.000000000000000000, -0.000000000000000000, 1.000000000000000000 ) ) ;
#2939 = ADVANCED_FACE ( 'NONE', ( #73608 ), #33377, .T. ) ;
#2940 = ORIENTED_EDGE ( 'NONE', *, *, #44122, .T. ) ;
#2941 = DIRECTION ( 'NONE',  ( 0.000000000000000000, -0.5224985647159379187, -0.8526401643540989506 ) ) ;
#2942 = EDGE_CURVE ( 'NONE', #52264, #37092, #28870, .T. ) ;
#2943 = CIRCLE ( 'NONE', #30475, 77.49899999999999523 ) ;
#2944 = CARTESIAN_POINT ( 'NONE',  ( -20.62008904684763166, -131.2721749321093512, 2.500000000000000000 ) ) ;
#2945 = DIRECTION ( 'NONE',  ( 0.000000000000000000, -0.7071067811865389130, -0.7071067811865563435 ) ) ;
#2946 = CARTESIAN_POINT ( 'NONE',  ( 93.84685191531248449, 91.99731107132950569, 76.83697916753381207 ) ) ;
#2947 = LINE ( 'NONE', #2590, #8833 ) ;
#2948 = CYLINDRICAL_SURFACE ( 'NONE', #18202, 16.00000000000000000 ) ;
#2949 = CARTESIAN_POINT ( 'NONE',  ( -3.000000000000000000, -13.04903810567647682, -19.60159698893442481 ) ) ;
#2950 = CARTESIAN_POINT ( 'NONE',  ( 92.80789733908675032, 91.16770611573555527, 74.89296886168688161 ) ) ;
#2951 = CARTESIAN_POINT ( 'NONE',  ( 10.00000000000000000, 15.48615015657582283, 39.04073710021349797 ) ) ;
#2952 = DIRECTION ( 'NONE',  ( 0.000000000000000000, 0.8660254037844363761, -0.5000000000000039968 ) ) ;
#2953 = ADVANCED_FACE ( 'NONE', ( #68365 ), #22877, .F. ) ;
#2954 = CIRCLE ( 'NONE', #6527, 31.99999999999998934 ) ;
#2955 = CIRCLE ( 'NONE', #65395, 31.99999999999998579 ) ;
#2956 = FACE_OUTER_BOUND ( 'NONE', #24596, .T. ) ;
#2957 = EDGE_CURVE ( 'NONE', #62465, #52552, #27369, .T. ) ;
#2958 = DIRECTION ( 'NONE',  ( 0.000000000000000000, 0.000000000000000000, -1.000000000000000000 ) ) ;
#2959 = VERTEX_POINT ( 'NONE', #11566 ) ;
#2960 = AXIS2_PLACEMENT_3D ( 'NONE', #15954, #56181, #74209 ) ;
#2961 = CARTESIAN_POINT ( 'NONE',  ( -93.84685191531252713, 88.00268892867056536, 82.86947916753379673 ) ) ;
#2962 = AXIS2_PLACEMENT_3D ( 'NONE', #17997, #33808, #63879 ) ;
#2963 = DIRECTION ( 'NONE',  ( -1.000000000000000000, -0.000000000000000000, 0.000000000000000000 ) ) ;
#2964 = PLANE ( 'NONE',  #49843 ) ;
#2965 = CIRCLE ( 'NONE', #28157, 42.00000000000000000 ) ;
#2966 = ORIENTED_EDGE ( 'NONE', *, *, #71220, .T. ) ;
#2967 = DIRECTION ( 'NONE',  ( -0.8191520442889890230, 0.000000000000000000, -0.5735764363510501562 ) ) ;
#2968 = CARTESIAN_POINT ( 'NONE',  ( 10.00000000000000000, 20.41045688087930898, -72.35160999960793049 ) ) ;
#2969 = CYLINDRICAL_SURFACE ( 'NONE', #31130, 31.99999999999999289 ) ;
#2970 = AXIS2_PLACEMENT_3D ( 'NONE', #7042, #29969, #47639 ) ;
#2971 = CARTESIAN_POINT ( 'NONE',  ( 92.69370383062501162, -211.3315407142195852, 79.69447916753381378 ) ) ;
#2972 = ORIENTED_EDGE ( 'NONE', *, *, #41908, .F. ) ;
#2973 = VERTEX_POINT ( 'NONE', #62741 ) ;
#2974 = DIRECTION ( 'NONE',  ( 0.000000000000000000, -0.9510565162951565288, 0.3090169943749382364 ) ) ;
#2975 = CARTESIAN_POINT ( 'NONE',  ( 0.000000000000000000, -6.555932627142676772, 37.01155633439056203 ) ) ;
#2976 = CARTESIAN_POINT ( 'NONE',  ( -43.60332556124591008, -123.0000000000000142, 2.500000000000000000 ) ) ;
#2977 = EDGE_LOOP ( 'NONE', ( #29074, #48341, #59458, #63020 ) ) ;
#2978 = DIRECTION ( 'NONE',  ( 0.9580045777625452175, 0.2867529058022035837, -0.000000000000000000 ) ) ;
#2979 = CARTESIAN_POINT ( 'NONE',  ( 96.15314808468748708, -208.0026889286704943, 75.61989583420049144 ) ) ;
#2980 = ORIENTED_EDGE ( 'NONE', *, *, #14651, .T. ) ;
#2981 = EDGE_CURVE ( 'NONE', #67992, #45327, #28576, .T. ) ;
#2982 = CARTESIAN_POINT ( 'NONE',  ( 10.00000000000000000, 8.830959090343430518, -74.65491531819107252 ) ) ;
#2983 = VERTEX_POINT ( 'NONE', #56337 ) ;
#2984 = ORIENTED_EDGE ( 'NONE', *, *, #55790, .F. ) ;
#2985 = DIRECTION ( 'NONE',  ( 0.000000000000000000, -0.2079116908177671419, 0.9781476007338040235 ) ) ;
#2986 = AXIS2_PLACEMENT_3D ( 'NONE', #72112, #54104, #8222 ) ;
#2987 = ADVANCED_FACE ( 'NONE', ( #60589 ), #28121, .T. ) ;
#2988 = DIRECTION ( 'NONE',  ( 0.000000000000000000, -0.5224985647159380298, -0.8526401643540988395 ) ) ;
#2989 = VERTEX_POINT ( 'NONE', #10461 ) ;
#2990 = DIRECTION ( 'NONE',  ( -0.7950889364178798102, 0.6064928550163511956, 0.000000000000000000 ) ) ;
#2991 = CARTESIAN_POINT ( 'NONE',  ( 96.32499999999998863, -212.2949673200287179, 82.03604166840096923 ) ) ;
#2992 = EDGE_CURVE ( 'NONE', #23616, #17390, #35761, .T. ) ;
#2993 = CARTESIAN_POINT ( 'NONE',  ( 94.99999999999998579, 93.05995642670504253, 86.03125000000000000 ) ) ;
#2994 = ADVANCED_FACE ( 'NONE', ( #23240 ), #21740, .F. ) ;
#2995 = ORIENTED_EDGE ( 'NONE', *, *, #17255, .F. ) ;
#2996 = FACE_OUTER_BOUND ( 'NONE', #32621, .T. ) ;
#2997 = CARTESIAN_POINT ( 'NONE',  ( -93.67499999999998295, -212.2949673200287179, 89.02104166840096866 ) ) ;
#2998 = ORIENTED_EDGE ( 'NONE', *, *, #892, .F. ) ;
#2999 = ORIENTED_EDGE ( 'NONE', *, *, #6438, .F. ) ;
#3000 = CARTESIAN_POINT ( 'NONE',  ( -93.84685191531254134, 91.99731107132950569, 89.58989583420049030 ) ) ;
#3001 = CIRCLE ( 'NONE', #37811, 77.49900000000000944 ) ;
#3002 = CARTESIAN_POINT ( 'NONE',  ( 97.30629616937498838, 90.00000000000002842, 82.97531250086714749 ) ) ;
#3003 = VECTOR ( 'NONE', #38102, 1000.000000000000000 ) ;
#3004 = EDGE_LOOP ( 'NONE', ( #18199, #49944, #33070, #14403 ) ) ;
#3005 = CARTESIAN_POINT ( 'NONE',  ( 92.34999999999999432, 91.52997821335252127, 81.13645833506764404 ) ) ;
#3006 = CARTESIAN_POINT ( 'NONE',  ( 11.99999999999999822, -51.03279382321125723, 55.19960302592048862 ) ) ;
#3007 = EDGE_LOOP ( 'NONE', ( #3845, #52907, #63616, #71587 ) ) ;
#3008 = FACE_OUTER_BOUND ( 'NONE', #28657, .T. ) ;
#3009 = AXIS2_PLACEMENT_3D ( 'NONE', #1323, #69322, #24935 ) ;
#3010 = ORIENTED_EDGE ( 'NONE', *, *, #53161, .F. ) ;
#3011 = ORIENTED_EDGE ( 'NONE', *, *, #64917, .F. ) ;
#3012 = ADVANCED_FACE ( 'NONE', ( #22118 ), #14704, .F. ) ;
#3013 = ORIENTED_EDGE ( 'NONE', *, *, #7066, .F. ) ;
#3014 = CARTESIAN_POINT ( 'NONE',  ( 15.00000000000000000, -4.261787119644963262, 26.19803753235780164 ) ) ;
#3015 = CARTESIAN_POINT ( 'NONE',  ( 12.49999999999999645, 1.530808498934191127E-15, 20.00000000000000000 ) ) ;
#3016 = EDGE_CURVE ( 'NONE', #48031, #70536, #36961, .T. ) ;
#3017 = CARTESIAN_POINT ( 'NONE',  ( -95.00000000000002842, 86.94004357329504273, 85.71374999999997613 ) ) ;
#3018 = VERTEX_POINT ( 'NONE', #39415 ) ;
#3019 = CARTESIAN_POINT ( 'NONE',  ( 6.000000000000000000, 22.90783923731629201, 78.73519480814962890 ) ) ;
#3020 = AXIS2_PLACEMENT_3D ( 'NONE', #39598, #9160, #44501 ) ;
#3021 = DIRECTION ( 'NONE',  ( 0.000000000000000000, 0.000000000000000000, 1.000000000000000000 ) ) ;
#3022 = VERTEX_POINT ( 'NONE', #62360 ) ;
#3023 = CYLINDRICAL_SURFACE ( 'NONE', #67196, 82.00000000000000000 ) ;
#3024 = CARTESIAN_POINT ( 'NONE',  ( -92.69370383062498320, -209.9999999999999716, 78.53031250086714010 ) ) ;
#3025 = VERTEX_POINT ( 'NONE', #51057 ) ;
#3026 = LINE ( 'NONE', #19898, #60294 ) ;
#3027 = DIRECTION ( 'NONE',  ( 0.000000000000000000, -0.1045284632676429099, -0.9945218953682744001 ) ) ;
#3028 = CARTESIAN_POINT ( 'NONE',  ( 11.99999999999999822, -49.70050353004932475, 59.46389618801947563 ) ) ;
#3029 = DIRECTION ( 'NONE',  ( -1.000000000000000000, 0.000000000000000000, -0.000000000000000000 ) ) ;
#3030 = AXIS2_PLACEMENT_3D ( 'NONE', #47815, #37293, #43313 ) ;
#3031 = CARTESIAN_POINT ( 'NONE',  ( 0.000000000000000000, 0.000000000000000000, 0.000000000000000000 ) ) ;
#3032 = EDGE_CURVE ( 'NONE', #61574, #61214, #73981, .T. ) ;
#3033 = ADVANCED_FACE ( 'NONE', ( #24341 ), #2187, .T. ) ;
#3034 = CARTESIAN_POINT ( 'NONE',  ( 26.09152095774781799, -124.8716048804687375, 5.500000000000000000 ) ) ;
#3035 = CARTESIAN_POINT ( 'NONE',  ( 92.69370383062498320, 88.66845928578035796, 89.06072916753382174 ) ) ;
#3036 = LINE ( 'NONE', #9373, #47208 ) ;
#3037 = CARTESIAN_POINT ( 'NONE',  ( 13.83832728059186046, -142.6495187161941089, -5.500000000000000000 ) ) ;
#3038 = CARTESIAN_POINT ( 'NONE',  ( -92.34999999999999432, -208.4700217866474645, 86.63979166840096013 ) ) ;
#3039 = CARTESIAN_POINT ( 'NONE',  ( -92.69370383062502583, 88.66845928578038638, 75.93739583420047268 ) ) ;
#3040 = DIRECTION ( 'NONE',  ( -1.000000000000000000, 0.000000000000000000, 0.000000000000000000 ) ) ;
#3041 = CARTESIAN_POINT ( 'NONE',  ( -2.503857664561936813E-16, -5.773502691896267081, -6.000000000000000000 ) ) ;
#3042 = DIRECTION ( 'NONE',  ( 0.000000000000000000, 0.7604059656000323741, -0.6494480483301819929 ) ) ;
#3043 = DIRECTION ( 'NONE',  ( -1.000000000000000000, 0.000000000000000000, 0.000000000000000000 ) ) ;
#3044 = CARTESIAN_POINT ( 'NONE',  ( -93.67499999999998295, -212.2949673200287179, 84.57604166840096127 ) ) ;
#3045 = FACE_OUTER_BOUND ( 'NONE', #46790, .T. ) ;
#3046 = AXIS2_PLACEMENT_3D ( 'NONE', #8883, #8523, #25436 ) ;
#3047 = CARTESIAN_POINT ( 'NONE',  ( -2.500000000000015543, -73.00000000000001421, -255.0000000000000000 ) ) ;
#3048 = CARTESIAN_POINT ( 'NONE',  ( 97.65000000000000568, 88.47002178664752137, 75.73895833506765030 ) ) ;
#3049 = CARTESIAN_POINT ( 'NONE',  ( -93.67499999999998295, -212.2949673200287179, 88.94166666666666288 ) ) ;
#3050 = CYLINDRICAL_SURFACE ( 'NONE', #62644, 11.59999999999999787 ) ;
#3051 = ORIENTED_EDGE ( 'NONE', *, *, #65354, .T. ) ;
#3052 = CIRCLE ( 'NONE', #27235, 77.49900000000000944 ) ;
#3053 = CARTESIAN_POINT ( 'NONE',  ( 0.000000000000000000, 0.000000000000000000, 0.000000000000000000 ) ) ;
#3054 = AXIS2_PLACEMENT_3D ( 'NONE', #56998, #55872, #38586 ) ;
#3055 = CARTESIAN_POINT ( 'NONE',  ( -42.50000000000000000, 0.000000000000000000, -20.99999999999999645 ) ) ;
#3056 = DIRECTION ( 'NONE',  ( -7.728965982074743403E-16, -1.065814103640131346E-14, -1.000000000000000000 ) ) ;
#3057 = CARTESIAN_POINT ( 'NONE',  ( -3.000000000000000000, -13.04903810567647682, -19.60159698893442481 ) ) ;
#3058 = CIRCLE ( 'NONE', #6632, 31.99999999999998579 ) ;
#3059 = AXIS2_PLACEMENT_3D ( 'NONE', #3031, #25922, #60523 ) ;
#3060 = ORIENTED_EDGE ( 'NONE', *, *, #18565, .T. ) ;
#3061 = CARTESIAN_POINT ( 'NONE',  ( 0.000000000000000000, 0.000000000000000000, 0.000000000000000000 ) ) ;
#3062 = FACE_OUTER_BOUND ( 'NONE', #13368, .T. ) ;
#3063 = ORIENTED_EDGE ( 'NONE', *, *, #48240, .F. ) ;
#3064 = CARTESIAN_POINT ( 'NONE',  ( 93.84685191531251292, -211.9973110713294489, 82.12864583420046927 ) ) ;
#3065 = CARTESIAN_POINT ( 'NONE',  ( 92.69370383062501162, -208.6684592857803295, 89.11364583420049712 ) ) ;
#3066 = ORIENTED_EDGE ( 'NONE', *, *, #4965, .T. ) ;
#3067 = VECTOR ( 'NONE', #17136, 1000.000000000000000 ) ;
#3068 = CARTESIAN_POINT ( 'NONE',  ( 96.15314808468750130, -211.9973110713294489, 86.83822916753382515 ) ) ;
#3069 = ORIENTED_EDGE ( 'NONE', *, *, #73929, .F. ) ;
#3070 = ADVANCED_FACE ( 'NONE', ( #40901 ), #35979, .T. ) ;
#3071 = DIRECTION ( 'NONE',  ( -1.000000000000000000, 0.000000000000000000, -0.000000000000000000 ) ) ;
#3072 = VERTEX_POINT ( 'NONE', #17588 ) ;
#3073 = CARTESIAN_POINT ( 'NONE',  ( -97.30629616937501680, 90.00000000000004263, 77.10156250086714635 ) ) ;
#3074 = EDGE_LOOP ( 'NONE', ( #36887, #53165, #62381, #13225 ) ) ;
#3075 = ADVANCED_FACE ( 'NONE', ( #59291 ), #7784, .T. ) ;
#3076 = VECTOR ( 'NONE', #65996, 1000.000000000000000 ) ;
#3077 = ORIENTED_EDGE ( 'NONE', *, *, #17757, .F. ) ;
#3078 = DIRECTION ( 'NONE',  ( 0.7585478161175706058, 0.6516173805718080692, -0.000000000000000000 ) ) ;
#3079 = VERTEX_POINT ( 'NONE', #23601 ) ;
#3080 = DIRECTION ( 'NONE',  ( 0.000000000000000000, 0.000000000000000000, 1.000000000000000000 ) ) ;
#3081 = SURFACE_SIDE_STYLE ('',( #47438 ) ) ;
#3082 = EDGE_CURVE ( 'NONE', #11035, #30392, #7038, .T. ) ;
#3083 = ORIENTED_EDGE ( 'NONE', *, *, #51760, .F. ) ;
#3084 = DIRECTION ( 'NONE',  ( -1.000000000000000000, 0.000000000000000000, 0.000000000000000000 ) ) ;
#3085 = ORIENTED_EDGE ( 'NONE', *, *, #72418, .F. ) ;
#3086 = CYLINDRICAL_SURFACE ( 'NONE', #33629, 2.649999999999985700 ) ;
#3087 = EDGE_CURVE ( 'NONE', #19149, #56343, #52163, .T. ) ;
#3088 = ORIENTED_EDGE ( 'NONE', *, *, #35130, .F. ) ;
#3089 = ORIENTED_EDGE ( 'NONE', *, *, #20403, .T. ) ;
#3090 = ORIENTED_EDGE ( 'NONE', *, *, #57635, .T. ) ;
#3091 = CARTESIAN_POINT ( 'NONE',  ( 95.00000000000000000, -212.6630814284392557, 78.37156250086714238 ) ) ;
#3092 = CYLINDRICAL_SURFACE ( 'NONE', #1703, 16.00000000000000000 ) ;
#3093 = AXIS2_PLACEMENT_3D ( 'NONE', #6227, #58442, #35148 ) ;
#3094 = DIRECTION ( 'NONE',  ( -1.000000000000000000, -0.000000000000000000, -0.000000000000000000 ) ) ;
#3095 = ORIENTED_EDGE ( 'NONE', *, *, #27938, .T. ) ;
#3096 = ORIENTED_EDGE ( 'NONE', *, *, #22042, .T. ) ;
#3097 = DIRECTION ( 'NONE',  ( -1.000000000000000000, 0.000000000000000000, 0.000000000000000000 ) ) ;
#3098 = ORIENTED_EDGE ( 'NONE', *, *, #3316, .T. ) ;
#3099 = LINE ( 'NONE', #53462, #15602 ) ;
#3100 = LINE ( 'NONE', #65497, #63562 ) ;
#3101 = EDGE_CURVE ( 'NONE', #39686, #2973, #6963, .T. ) ;
#3102 = CARTESIAN_POINT ( 'NONE',  ( -92.69370383062502583, 88.66845928578038638, 79.27114583420048177 ) ) ;
#3103 = EDGE_CURVE ( 'NONE', #27761, #71554, #57819, .T. ) ;
#3104 = VERTEX_POINT ( 'NONE', #708 ) ;
#3105 = CARTESIAN_POINT ( 'NONE',  ( 96.15314808468748708, 91.99731107132950569, 78.63614583420047666 ) ) ;
#3106 = ORIENTED_EDGE ( 'NONE', *, *, #7489, .T. ) ;
#3107 = DIRECTION ( 'NONE',  ( 0.000000000000000000, 0.000000000000000000, -1.000000000000000000 ) ) ;
#3108 = PLANE ( 'NONE',  #225 ) ;
#3109 = VECTOR ( 'NONE', #31359, 1000.000000000000114 ) ;
#3110 = LINE ( 'NONE', #13974, #72763 ) ;
#3111 = FACE_OUTER_BOUND ( 'NONE', #7678, .T. ) ;
#3112 = CARTESIAN_POINT ( 'NONE',  ( -96.15314808468745866, -211.9973110713294489, 82.76364583420047438 ) ) ;
#3113 = DIRECTION ( 'NONE',  ( -1.000000000000000000, 0.000000000000000000, -0.000000000000000000 ) ) ;
#3114 = CARTESIAN_POINT ( 'NONE',  ( 10.00000000000000000, -74.18225833017913828, 34.94270380257611919 ) ) ;
#3115 = AXIS2_PLACEMENT_3D ( 'NONE', #27651, #44207, #67132 ) ;
#3116 = CYLINDRICAL_SURFACE ( 'NONE', #52674, 31.99999999999999289 ) ;
#3117 = EDGE_LOOP ( 'NONE', ( #50067, #147, #54726, #4155 ) ) ;
#3118 = EDGE_CURVE ( 'NONE', #1974, #40171, #7423, .T. ) ;
#3119 = EDGE_CURVE ( 'NONE', #8248, #67112, #13420, .T. ) ;
#3120 = EDGE_LOOP ( 'NONE', ( #22259, #41839, #68535, #67491 ) ) ;
#3121 = CARTESIAN_POINT ( 'NONE',  ( 10.00000000000000000, -33.00180498840035170, -17.80606268964575278 ) ) ;
#3122 = CARTESIAN_POINT ( 'NONE',  ( -96.32500000000001705, 92.29496732002878900, 75.92416666666666458 ) ) ;
#3123 = CARTESIAN_POINT ( 'NONE',  ( -92.35000000000003695, 89.99999988321006583, 84.68187499741277691 ) ) ;
#3124 = CARTESIAN_POINT ( 'NONE',  ( -97.30629616937501680, 88.66845928578038638, 84.61572916753380014 ) ) ;
#3125 = DIRECTION ( 'NONE',  ( -1.000000000000000000, -0.000000000000000000, -0.000000000000000000 ) ) ;
#3126 = CARTESIAN_POINT ( 'NONE',  ( 21.07894319797337701, -103.8699611390234878, 5.500000000000000000 ) ) ;
#3127 = AXIS2_PLACEMENT_3D ( 'NONE', #9089, #71491, #65882 ) ;
#3128 = DIRECTION ( 'NONE',  ( 1.000000000000000000, 1.427937372958405461E-15, 7.962523111839130290E-16 ) ) ;
#3129 = VERTEX_POINT ( 'NONE', #29966 ) ;
#3130 = LINE ( 'NONE', #61360, #42832 ) ;
#3131 = CARTESIAN_POINT ( 'NONE',  ( 10.00000000000000000, 12.93880638057426502, -76.41127070299258150 ) ) ;
#3132 = CARTESIAN_POINT ( 'NONE',  ( 0.000000000000000000, -37.01155633439063308, 6.555932627142289526 ) ) ;
#3133 = DIRECTION ( 'NONE',  ( -1.000000000000000000, -0.000000000000000000, 0.000000000000000000 ) ) ;
#3134 = DIRECTION ( 'NONE',  ( -1.000000000000000000, -0.000000000000000000, 0.000000000000000000 ) ) ;
#3135 = CARTESIAN_POINT ( 'NONE',  ( 94.99999999999998579, 86.94004357329502852, 86.34874999999999545 ) ) ;
#3136 = CARTESIAN_POINT ( 'NONE',  ( -92.69370383062498320, -211.3315407142195852, 82.44614583420049314 ) ) ;
#3137 =( NAMED_UNIT ( * ) PLANE_ANGLE_UNIT ( ) SI_UNIT ( $, .RADIAN. ) );
#3138 = CARTESIAN_POINT ( 'NONE',  ( 15.00000000000000000, 20.85821328998756385, 10.92862929874494249 ) ) ;
#3139 =( BOUNDED_CURVE ( )  B_SPLINE_CURVE ( 2, ( #61169, #31830, #50234, #73168, #26935, #3303, #72783 ),
 .UNSPECIFIED., .F., .F. ) 
 B_SPLINE_CURVE_WITH_KNOTS ( ( 3, 2, 2, 3 ),
 ( 0.5624999999999997780, 0.5694444444444440867, 0.5763888888888885065, 0.5833333333333329263 ),
 .UNSPECIFIED. ) 
 CURVE ( )  GEOMETRIC_REPRESENTATION_ITEM ( )  RATIONAL_B_SPLINE_CURVE ( ( 1.000000000000004219, 0.8660254037844343777, 1.000000000000000000, 0.8660254037844387076, 1.000000000000000000, 0.8660254037844472563, 0.9999999999999914513 ) ) 
 REPRESENTATION_ITEM ( '' )  );
#3140 = DIRECTION ( 'NONE',  ( 1.000000000000000000, 0.000000000000000000, 0.000000000000000000 ) ) ;
#3141 = DIRECTION ( 'NONE',  ( 2.603472992746261562E-14, 2.546204323184492723E-14, -1.000000000000000000 ) ) ;
#3142 = CARTESIAN_POINT ( 'NONE',  ( 21.07894319797337701, -103.8699611390234878, 5.500000000000000000 ) ) ;
#3143 = ORIENTED_EDGE ( 'NONE', *, *, #55555, .T. ) ;
#3144 = LINE ( 'NONE', #43723, #13744 ) ;
#3145 = DIRECTION ( 'NONE',  ( -1.000000000000000000, 0.000000000000000000, 0.000000000000000000 ) ) ;
#3146 = DIRECTION ( 'NONE',  ( 0.000000000000000000, 0.000000000000000000, 1.000000000000000000 ) ) ;
#3147 = EDGE_CURVE ( 'NONE', #37997, #28262, #3390, .T. ) ;
#3148 = DIRECTION ( 'NONE',  ( 1.000000000000000000, 0.000000000000000000, 0.000000000000000000 ) ) ;
#3149 = ORIENTED_EDGE ( 'NONE', *, *, #18241, .F. ) ;
#3150 = EDGE_CURVE ( 'NONE', #32694, #28480, #57410, .T. ) ;
#3151 = DIRECTION ( 'NONE',  ( -1.000000000000000000, -0.000000000000000000, -0.000000000000000000 ) ) ;
#3152 = SURFACE_STYLE_USAGE ( .BOTH. , #60287 ) ;
#3153 = ORIENTED_EDGE ( 'NONE', *, *, #48309, .F. ) ;
#3154 = ADVANCED_FACE ( 'NONE', ( #41624 ), #45400, .T. ) ;
#3155 =( BOUNDED_CURVE ( )  B_SPLINE_CURVE ( 2, ( #18720, #47669, #41300, #2221, #24740, #58580, #64598, #11979, #36019 ),
 .UNSPECIFIED., .F., .F. ) 
 B_SPLINE_CURVE_WITH_KNOTS ( ( 3, 2, 2, 2, 3 ),
 ( 0.2540073681283129825, 0.2540075594717653429, 0.2610633250126476734, 0.2681190905535301150, 0.2751748541904411316 ),
 .UNSPECIFIED. ) 
 CURVE ( )  GEOMETRIC_REPRESENTATION_ITEM ( )  RATIONAL_B_SPLINE_CURVE ( ( 0.9999927337532901195, 0.9999963667781166521, 1.000000000000000000, 0.8660254037844387076, 1.000000000000000000, 0.8660254037844387076, 1.000000000000000000, 0.8660254037844387076, 1.000000000000000000 ) ) 
 REPRESENTATION_ITEM ( '' )  );
#3156 = CARTESIAN_POINT ( 'NONE',  ( 11.99999999999999822, -31.47745569255092235, -68.26794271651296242 ) ) ;
#3157 = VECTOR ( 'NONE', #57271, 1000.000000000000000 ) ;
#3158 = VERTEX_POINT ( 'NONE', #70180 ) ;
#3159 = ADVANCED_FACE ( 'NONE', ( #6678 ), #52528, .T. ) ;
#3160 = LINE ( 'NONE', #28270, #49031 ) ;
#3161 = ORIENTED_EDGE ( 'NONE', *, *, #62752, .T. ) ;
#3162 = AXIS2_PLACEMENT_3D ( 'NONE', #12087, #72814, #66832 ) ;
#3163 = EDGE_CURVE ( 'NONE', #24796, #40037, #29745, .T. ) ;
#3164 = ORIENTED_EDGE ( 'NONE', *, *, #5446, .F. ) ;
#3165 = CIRCLE ( 'NONE', #12728, 31.99999999999998579 ) ;
#3166 = ORIENTED_EDGE ( 'NONE', *, *, #69522, .F. ) ;
#3167 = VERTEX_POINT ( 'NONE', #12676 ) ;
#3168 = DIRECTION ( 'NONE',  ( 1.000000000000000000, 1.427937372958405461E-15, 7.962523111839130290E-16 ) ) ;
#3169 = VERTEX_POINT ( 'NONE', #35609 ) ;
#3170 = PRODUCT_DEFINITION_SHAPE ( 'NONE', 'NONE',  #3585 ) ;
#3171 = CIRCLE ( 'NONE', #27161, 82.00000000000000000 ) ;
#3172 = ORIENTED_EDGE ( 'NONE', *, *, #71341, .F. ) ;
#3173 = CARTESIAN_POINT ( 'NONE',  ( 94.99999999999998579, 92.66308142843935514, 75.67281250086716682 ) ) ;
#3174 = CARTESIAN_POINT ( 'NONE',  ( 5.000000000000000000, -15.48615015657555993, -39.04073710021360455 ) ) ;
#3175 = EDGE_CURVE ( 'NONE', #16273, #62438, #39382, .T. ) ;
#3176 = CARTESIAN_POINT ( 'NONE',  ( 18.80329974962065265, -105.8248132807389084, 5.500000000000000000 ) ) ;
#3177 = ORIENTED_EDGE ( 'NONE', *, *, #12405, .T. ) ;
#3178 = ORIENTED_EDGE ( 'NONE', *, *, #39219, .F. ) ;
#3179 = VERTEX_POINT ( 'NONE', #42006 ) ;
#3180 = CARTESIAN_POINT ( 'NONE',  ( 22.94323693612312809, -114.6983135802921083, 5.500000000000000000 ) ) ;
#3181 = VERTEX_POINT ( 'NONE', #64943 ) ;
#3182 = CARTESIAN_POINT ( 'NONE',  ( 95.00000000000000000, -212.6630814284392557, 87.89656250086713385 ) ) ;
#3183 = CARTESIAN_POINT ( 'NONE',  ( 0.000000000000000000, 0.000000000000000000, -125.0000000000000000 ) ) ;
#3184 = CARTESIAN_POINT ( 'NONE',  ( 0.000000000000000000, 0.000000000000000000, 0.000000000000000000 ) ) ;
#3185 = DIRECTION ( 'NONE',  ( 1.000000000000000000, -0.000000000000000000, -0.000000000000000000 ) ) ;
#3186 = DIRECTION ( 'NONE',  ( -1.000000000000000000, -0.000000000000000000, -0.000000000000000000 ) ) ;
#3187 = DIRECTION ( 'NONE',  ( -0.000000000000000000, 0.000000000000000000, 1.000000000000000000 ) ) ;
#3188 = FACE_OUTER_BOUND ( 'NONE', #56711, .T. ) ;
#3189 = CYLINDRICAL_SURFACE ( 'NONE', #48045, 31.99999999999998579 ) ;
#3190 = CARTESIAN_POINT ( 'NONE',  ( -97.64999999999994884, -208.4700217866474645, 76.05645833506761733 ) ) ;
#3191 = EDGE_CURVE ( 'NONE', #20908, #68902, #3286, .T. ) ;
#3192 = CARTESIAN_POINT ( 'NONE',  ( -95.00000000000002842, 92.66308142843932671, 89.00781250086716057 ) ) ;
#3193 = ADVANCED_FACE ( 'NONE', ( #25073 ), #72408, .T. ) ;
#3194 = ORIENTED_EDGE ( 'NONE', *, *, #57075, .T. ) ;
#3196 = CARTESIAN_POINT ( 'NONE',  ( -96.15314808468752972, 91.99731107132950569, 88.90197916753380980 ) ) ;
#3195 = CARTESIAN_POINT ( 'NONE',  ( 96.32499999999997442, 92.29496732002878900, 75.26270833506764291 ) ) ;
#3197 = B_SPLINE_CURVE_WITH_KNOTS ( 'NONE', 1,
 ( #32318, #48878 ),
 .UNSPECIFIED., .F., .F.,
 ( 2, 2 ),
 ( 0.000000000000000000, 1.000000000000000000 ),
 .UNSPECIFIED. ) ;
#3198 = ORIENTED_EDGE ( 'NONE', *, *, #7259, .F. ) ;
#3199 = CARTESIAN_POINT ( 'NONE',  ( 96.15314808468748708, 91.99731107132950569, 74.98489583420048632 ) ) ;
#3200 = CARTESIAN_POINT ( 'NONE',  ( 11.99999999999999822, 0.000000000000000000, 0.000000000000000000 ) ) ;
#3201 = DIRECTION ( 'NONE',  ( -1.000000000000000000, 0.000000000000000000, -0.000000000000000000 ) ) ;
#3202 = DIRECTION ( 'NONE',  ( 1.000000000000000000, -0.000000000000000000, -0.000000000000000000 ) ) ;
#3203 = CARTESIAN_POINT ( 'NONE',  ( 5.999999999999999112, 56.15606465354958488, 59.75363087400094741 ) ) ;
#3204 = CARTESIAN_POINT ( 'NONE',  ( 10.00000000000000000, -58.39081064771787766, 50.95692526931307498 ) ) ;
#3205 = ADVANCED_BREP_SHAPE_REPRESENTATION ( '', ( #14123, #43395 ), #57869 ) ;
#3206 = CARTESIAN_POINT ( 'NONE',  ( -97.64999999999994884, -211.5299782133524218, 87.51291666666666913 ) ) ;
#3207 = CARTESIAN_POINT ( 'NONE',  ( 10.00000000000000000, 26.08949754953062694, -27.05870788708203989 ) ) ;
#3208 = ORIENTED_EDGE ( 'NONE', *, *, #14740, .F. ) ;
#3209 = CLOSED_SHELL ( 'NONE', ( #57203, #31036, #20088, #28833, #54894, #49126, #28029, #28766, #34130, #28070, #26735, #5093, #10361, #1314, #15329, #69939, #39757, #67651, #38725, #66344, #58630, #67974, #5871, #34646, #53935, #15977, #72459, #48983, #48808, #1509, #1229, #10961, #55057, #45402, #28792, #8383, #13223, #27732, #22656, #11603, #12155, #69842, #9923, #19792, #43645, #43497, #34918, #13086, #59323, #3075, #30479, #70400, #55004, #8997, #17002, #48617, #31552, #37795, #31221, #73056, #44118, #8487, #72637, #25954, #54931, #57492, #4868, #39139, #17323, #54320, #33477, #37552, #57875, #71129, #45958, #33810, #36988, #38884, #55455, #32575, #11870, #64124, #3193, #39458, #68778, #59976, #39116, #5385, #36936, #16895, #48040, #28760, #6559, #43113, #64786, #11704, #20603, #53300, #50223, #39582, #18254, #61298, #64041, #7399, #27915, #25603, #37438, #24431, #24115, #54898, #19929, #30535, #20534, #1007, #50604, #30656, #21228, #18391, #27564, #66804, #13799, #36325, #39120, #12156, #5998, #14452, #34425, #4456, #21969, #71548, #30441, #9937, #57400, #32843, #6874, #58909, #38559, #8844, #27650, #71267, #3159, #11771, #28261, #18653, #44166, #41118, #61530, #14606, #22687, #65133, #36503, #18074, #47696, #60215, #33068, #11241, #34617, #40472, #74064, #62990, #19518, #23118, #8432, #16182, #640, #4532, #50256, #69252, #49760, #27514, #44918, #20862, #64105 ) ) ;
#3210 = EDGE_LOOP ( 'NONE', ( #28468, #25337, #66049, #46841 ) ) ;
#3211 = DIRECTION ( 'NONE',  ( 1.000000000000000000, -0.000000000000000000, -0.000000000000000000 ) ) ;
#3212 = DIRECTION ( 'NONE',  ( 1.000000000000000000, -0.000000000000000000, 0.000000000000000000 ) ) ;
#3213 = CARTESIAN_POINT ( 'NONE',  ( 0.000000000000000000, 0.000000000000000000, -6.000000000000000000 ) ) ;
#3214 = CARTESIAN_POINT ( 'NONE',  ( 0.000000000000000000, -35.47612816024506088, -22.48208911017539435 ) ) ;
#3215 = CARTESIAN_POINT ( 'NONE',  ( 92.35000000009272014, 90.00001381026685010, 80.55392363656929433 ) ) ;
#3216 = CARTESIAN_POINT ( 'NONE',  ( -92.69370383062499741, -210.9303297190751891, 74.84209033237941355 ) ) ;
#3217 = AXIS2_PLACEMENT_3D ( 'NONE', #63207, #69202, #47015 ) ;
#3218 = ORIENTED_EDGE ( 'NONE', *, *, #2113, .F. ) ;
#3219 = CARTESIAN_POINT ( 'NONE',  ( -95.00000000000002842, 92.66308142843932671, 82.49906250086714010 ) ) ;
#3220 = CARTESIAN_POINT ( 'NONE',  ( -10.00000000000000000, 0.000000000000000000, 0.000000000000000000 ) ) ;
#3221 = DIRECTION ( 'NONE',  ( 0.000000000000000000, 0.000000000000000000, 1.000000000000000000 ) ) ;
#3222 = CARTESIAN_POINT ( 'NONE',  ( -97.65000000000007674, 91.52997821335250705, 79.15208333333333712 ) ) ;
#3223 = AXIS2_PLACEMENT_3D ( 'NONE', #73039, #21545, #15918 ) ;
#3224 = CARTESIAN_POINT ( 'NONE',  ( 0.000000000000000000, 0.000000000000000000, 0.000000000000000000 ) ) ;
#3225 = CARTESIAN_POINT ( 'NONE',  ( 0.000000000000000000, 40.68715046381927891, 10.41901085202092858 ) ) ;
#3226 = DIRECTION ( 'NONE',  ( 0.000000000000000000, 0.000000000000000000, -1.000000000000000000 ) ) ;
#3227 = CIRCLE ( 'NONE', #30751, 16.00000000000000000 ) ;
#3228 =( NAMED_UNIT ( * ) PLANE_ANGLE_UNIT ( ) SI_UNIT ( $, .RADIAN. ) );
#3229 = DIRECTION ( 'NONE',  ( -0.000000000000000000, -0.000000000000000000, 1.000000000000000000 ) ) ;
#3230 = DIRECTION ( 'NONE',  ( 0.000000000000000000, 0.000000000000000000, 1.000000000000000000 ) ) ;
#3231 = EDGE_CURVE ( 'NONE', #21174, #44951, #29813, .T. ) ;
#3232 = VECTOR ( 'NONE', #63871, 1000.000000000000000 ) ;
#3233 = CARTESIAN_POINT ( 'NONE',  ( 97.30629616937498838, 88.66845928578035796, 84.98614583420047097 ) ) ;
#3234 = CARTESIAN_POINT ( 'NONE',  ( -97.30629616937495996, -209.9999999999999716, 81.54656250086715374 ) ) ;
#3235 = DIRECTION ( 'NONE',  ( -1.000000000000000000, 0.000000000000000000, 0.000000000000000000 ) ) ;
#3236 = ORIENTED_EDGE ( 'NONE', *, *, #70742, .T. ) ;
#3237 = LINE ( 'NONE', #14855, #10050 ) ;
#3238 = CARTESIAN_POINT ( 'NONE',  ( -92.34999999999999432, -211.5299782133524502, 78.83458333333334167 ) ) ;
#3239 = CARTESIAN_POINT ( 'NONE',  ( 10.00000000000000000, -51.29473840253178452, -63.97538442413483750 ) ) ;
#3240 = AXIS2_PLACEMENT_3D ( 'NONE', #7476, #24760, #40578 ) ;
#3241 = ADVANCED_FACE ( 'NONE', ( #9636 ), #26175, .F. ) ;
#3242 = CARTESIAN_POINT ( 'NONE',  ( 92.69370383062501162, -208.6684592857803011, 82.60489583420047666 ) ) ;
#3243 = ORIENTED_EDGE ( 'NONE', *, *, #55243, .F. ) ;
#3244 = EDGE_CURVE ( 'NONE', #56046, #13831, #62250, .T. ) ;
#3245 = DIRECTION ( 'NONE',  ( -1.000000000000000000, -0.000000000000000000, -0.000000000000000000 ) ) ;
#3246 = EDGE_LOOP ( 'NONE', ( #22765, #11489, #8962, #73622, #29290, #732 ) ) ;
#3247 = DIRECTION ( 'NONE',  ( 0.000000000000000000, 0.9135454576426063067, -0.4067366430757881068 ) ) ;
#3248 = EDGE_LOOP ( 'NONE', ( #1894, #52391, #11295, #71249 ) ) ;
#3249 = EDGE_CURVE ( 'NONE', #46616, #36077, #39445, .T. ) ;
#3250 = EDGE_CURVE ( 'NONE', #46252, #45911, #14903, .T. ) ;
#3251 = CARTESIAN_POINT ( 'NONE',  ( -97.65000000000001990, 90.00001433786178495, 79.28437450583712121 ) ) ;
#3252 = ORIENTED_EDGE ( 'NONE', *, *, #64700, .T. ) ;
#3253 = CARTESIAN_POINT ( 'NONE',  ( 96.15314808468750130, -211.9973110713294489, 77.94822916753382458 ) ) ;
#3254 = LINE ( 'NONE', #59262, #45303 ) ;
#3255 = CARTESIAN_POINT ( 'NONE',  ( 0.000000000000000000, 0.000000000000000000, 125.0000000000000000 ) ) ;
#3256 = PLANE ( 'NONE',  #1521 ) ;
#3257 = EDGE_CURVE ( 'NONE', #43589, #21187, #37020, .T. ) ;
#3258 = AXIS2_PLACEMENT_3D ( 'NONE', #65054, #2668, #47740 ) ;
#3259 = DIRECTION ( 'NONE',  ( 0.000000000000000000, -0.5224985647159560154, 0.8526401643540879594 ) ) ;
#3260 = CARTESIAN_POINT ( 'NONE',  ( 93.67500000000001137, -207.7050326799711968, 81.63916666666666799 ) ) ;
#3261 = AXIS2_PLACEMENT_3D ( 'NONE', #32711, #72563, #62054 ) ;
#3262 = ORIENTED_EDGE ( 'NONE', *, *, #15719, .T. ) ;
#3263 = EDGE_LOOP ( 'NONE', ( #11188, #40862, #20039, #22412 ) ) ;
#3264 = EDGE_LOOP ( 'NONE', ( #63569, #11796, #22892, #36153 ) ) ;
#3265 = ORIENTED_EDGE ( 'NONE', *, *, #71338, .T. ) ;
#3266 = LINE ( 'NONE', #71272, #46651 ) ;
#3267 = CARTESIAN_POINT ( 'NONE',  ( -93.84685191531254134, 91.99731107132950569, 83.87489583420048689 ) ) ;
#3268 = AXIS2_PLACEMENT_3D ( 'NONE', #46731, #17775, #6153 ) ;
#3269 = CARTESIAN_POINT ( 'NONE',  ( 97.64999999994533653, 89.99998298270493535, 88.49187441316099978 ) ) ;
#3270 = CIRCLE ( 'NONE', #34469, 77.49899999999999523 ) ;
#3271 = CARTESIAN_POINT ( 'NONE',  ( 12.13205353604972991, -140.1820037904669789, -5.500000000000000000 ) ) ;
#3272 =( BOUNDED_CURVE ( )  B_SPLINE_CURVE ( 2, ( #8654, #66178, #71783, #55248, #21028, #66899, #38331 ),
 .UNSPECIFIED., .F., .F. ) 
 B_SPLINE_CURVE_WITH_KNOTS ( ( 3, 2, 2, 3 ),
 ( 0.9583333333333337034, 0.9652777777777781232, 0.9722222222222225430, 0.9791666666666669627 ),
 .UNSPECIFIED. ) 
 CURVE ( )  GEOMETRIC_REPRESENTATION_ITEM ( )  RATIONAL_B_SPLINE_CURVE ( ( 0.9999999999999935607, 0.8660254037844451469, 1.000000000000000000, 0.8660254037844387076, 1.000000000000000000, 0.8660254037844322683, 1.000000000000006439 ) ) 
 REPRESENTATION_ITEM ( '' )  );
#3273 = CARTESIAN_POINT ( 'NONE',  ( 92.34999999999999432, 91.52997821335252127, 75.97708333333333997 ) ) ;
#3274 = DIRECTION ( 'NONE',  ( -1.000000000000000000, -0.000000000000000000, 0.000000000000000000 ) ) ;
#3275 = ORIENTED_EDGE ( 'NONE', *, *, #38816, .F. ) ;
#3276 = CARTESIAN_POINT ( 'NONE',  ( -97.64999999999994884, -211.5299782133524502, 87.59229166840096070 ) ) ;
#3278 = VERTEX_POINT ( 'NONE', #48374 ) ;
#3277 = EDGE_CURVE ( 'NONE', #8216, #44755, #45467, .T. ) ;
#3279 = DIRECTION ( 'NONE',  ( 1.000000000000000000, 0.000000000000000000, 0.000000000000000000 ) ) ;
#3280 = CIRCLE ( 'NONE', #32050, 77.49899999999999523 ) ;
#3281 = EDGE_LOOP ( 'NONE', ( #56265, #48763, #11453, #36038 ) ) ;
#3282 = CARTESIAN_POINT ( 'NONE',  ( -97.65000000000001990, 91.52997821335253548, 82.40645833506762585 ) ) ;
#3284 = EDGE_CURVE ( 'NONE', #38750, #8033, #66778, .T. ) ;
#3283 = VERTEX_POINT ( 'NONE', #43125 ) ;
#3285 = CARTESIAN_POINT ( 'NONE',  ( 97.30629616937498838, 90.00000000000002842, 88.21406250086714351 ) ) ;
#3286 = LINE ( 'NONE', #8149, #68208 ) ;
#3287 = CYLINDRICAL_SURFACE ( 'NONE', #69048, 32.00000000000000000 ) ;
#3288 = CARTESIAN_POINT ( 'NONE',  ( -97.64995850092664398, 88.46999782714635785, 83.78229332575388355 ) ) ;
#3289 = DIRECTION ( 'NONE',  ( -1.000000000000000000, -0.000000000000000000, -0.000000000000000000 ) ) ;
#3290 = DIRECTION ( 'NONE',  ( -1.000000000000000000, -0.000000000000000000, 0.000000000000000000 ) ) ;
#3291 = ORIENTED_EDGE ( 'NONE', *, *, #48064, .T. ) ;
#3292 = CARTESIAN_POINT ( 'NONE',  ( 95.00000000000000000, -206.9400435732949575, 77.77624999999999034 ) ) ;
#3293 = DIRECTION ( 'NONE',  ( 0.000000000000000000, -0.5877852522924802425, 0.8090169943749422332 ) ) ;
#3294 = ORIENTED_EDGE ( 'NONE', *, *, #52699, .F. ) ;
#3295 = AXIS2_PLACEMENT_3D ( 'NONE', #5928, #35579, #35949 ) ;
#3296 = ORIENTED_EDGE ( 'NONE', *, *, #13435, .F. ) ;
#3297 = DIRECTION ( 'NONE',  ( 0.000000000000000000, 0.000000000000000000, 1.000000000000000000 ) ) ;
#3298 = VECTOR ( 'NONE', #35506, 1000.000000000000000 ) ;
#3299 = DIRECTION ( 'NONE',  ( 0.000000000000000000, 0.000000000000000000, 1.000000000000000000 ) ) ;
#3300 = DIRECTION ( 'NONE',  ( -0.3311129884571295534, -0.9435911131814398445, 0.000000000000000000 ) ) ;
#3301 = CARTESIAN_POINT ( 'NONE',  ( -93.84685191531248449, -208.0026889286704943, 85.14489583420048291 ) ) ;
#3302 = ORIENTED_EDGE ( 'NONE', *, *, #8745, .T. ) ;
#3303 = CARTESIAN_POINT ( 'NONE',  ( 92.35000000000012221, -211.5299782133525071, 81.16291666666667481 ) ) ;
#3304 = EDGE_LOOP ( 'NONE', ( #7755, #15074, #34763, #514 ) ) ;
#3305 = CARTESIAN_POINT ( 'NONE',  ( 5.000000000000000000, 56.15606465355042332, -59.75363087400017292 ) ) ;
#3306 = CARTESIAN_POINT ( 'NONE',  ( 93.84685191531248449, 88.00268892867053694, 89.27239583420049485 ) ) ;
#3307 = CARTESIAN_POINT ( 'NONE',  ( 0.000000000000000000, 0.000000000000000000, -54.99999999999998579 ) ) ;
#3308 = CARTESIAN_POINT ( 'NONE',  ( 94.99999999999998579, 87.33691857156068750, 76.46656250086712703 ) ) ;
#3309 = LINE ( 'NONE', #54414, #17262 ) ;
#3310 = CARTESIAN_POINT ( 'NONE',  ( 10.00000000000000000, -80.28980883073768382, 16.65972982744906972 ) ) ;
#3311 = CARTESIAN_POINT ( 'NONE',  ( 0.7800914985199594032, -118.7188063167744900, 2.500000000000000000 ) ) ;
#3312 = CARTESIAN_POINT ( 'NONE',  ( -1.648146632869002426, -4.821944789745372439, -6.000000000000000000 ) ) ;
#3313 = DIRECTION ( 'NONE',  ( -1.000000000000000000, 0.000000000000000000, -0.000000000000000000 ) ) ;
#3314 = DIRECTION ( 'NONE',  ( -1.000000000000000000, 0.000000000000000000, 0.000000000000000000 ) ) ;
#3315 =( REPRESENTATION_RELATIONSHIP ('NONE','NONE', #31117, #27826 ) REPRESENTATION_RELATIONSHIP_WITH_TRANSFORMATION ( #59472 )SHAPE_REPRESENTATION_RELATIONSHIP( ) );
#3316 = EDGE_CURVE ( 'NONE', #56423, #51311, #48011, .T. ) ;
#3317 = PRESENTATION_LAYER_ASSIGNMENT (  '', '', ( #51307 ) ) ;
#3318 = LINE ( 'NONE', #48409, #55252 ) ;
#3319 = AXIS2_PLACEMENT_3D ( 'NONE', #9727, #33771, #67615 ) ;
#3320 = CARTESIAN_POINT ( 'NONE',  ( 92.34999999999999432, 90.00000000000002842, 89.36499999999999488 ) ) ;
#3321 = ORIENTED_EDGE ( 'NONE', *, *, #25537, .F. ) ;
#3322 = CARTESIAN_POINT ( 'NONE',  ( -92.69370383062504004, 90.00000000000004263, 81.70531250086713726 ) ) ;
#3323 = DIRECTION ( 'NONE',  ( -1.000000000000000000, 0.000000000000000000, 0.000000000000000000 ) ) ;
#3324 = EDGE_CURVE ( 'NONE', #50948, #41513, #8535, .T. ) ;
#3325 = VECTOR ( 'NONE', #22983, 1000.000000000000000 ) ;
#3326 = CIRCLE ( 'NONE', #44190, 32.00000000000000000 ) ;
#3327 = EDGE_CURVE ( 'NONE', #52875, #6755, #27398, .T. ) ;
#3328 = DIRECTION ( 'NONE',  ( -0.000000000000000000, -1.000000000000000000, -0.000000000000000000 ) ) ;
#3329 = VERTEX_POINT ( 'NONE', #54389 ) ;
#3330 = DIRECTION ( 'NONE',  ( 1.000000000000000000, 0.000000000000000000, 0.000000000000000000 ) ) ;
#3331 = LINE ( 'NONE', #42787, #3611 ) ;
#3332 = DIRECTION ( 'NONE',  ( 0.000000000000000000, 0.9510565162951544194, -0.3090169943749446757 ) ) ;
#3333 = EDGE_CURVE ( 'NONE', #63423, #58064, #43504, .T. ) ;
#3334 = DIRECTION ( 'NONE',  ( 1.000000000000000000, 0.000000000000000000, 0.000000000000000000 ) ) ;
#3335 = CARTESIAN_POINT ( 'NONE',  ( 96.15314808468750130, -211.9973110713294489, 79.85322916753381151 ) ) ;
#3336 = AXIS2_PLACEMENT_3D ( 'NONE', #19855, #26977, #20223 ) ;
#3337 = ORIENTED_EDGE ( 'NONE', *, *, #58501, .T. ) ;
#3338 = VERTEX_POINT ( 'NONE', #66056 ) ;
#3339 = VECTOR ( 'NONE', #3361, 1000.000000000000114 ) ;
#3340 = DIRECTION ( 'NONE',  ( -1.000000000000000000, 7.571543891232750625E-15, 2.563413034563919882E-14 ) ) ;
#3341 = EDGE_CURVE ( 'NONE', #51387, #24434, #32181, .T. ) ;
#3342 = DIRECTION ( 'NONE',  ( 0.000000000000000000, 0.8090169943749447867, 0.5877852522924769119 ) ) ;
#3343 = CARTESIAN_POINT ( 'NONE',  ( -10.00000000000000000, 0.000000000000000000, 0.000000000000000000 ) ) ;
#3345 = VERTEX_POINT ( 'NONE', #42375 ) ;
#3344 = EDGE_CURVE ( 'NONE', #24268, #66486, #2920, .T. ) ;
#3346 = CARTESIAN_POINT ( 'NONE',  ( 93.84685191531249870, -208.0026889286704943, 75.72572916753382799 ) ) ;
#3347 = ORIENTED_EDGE ( 'NONE', *, *, #60288, .F. ) ;
#3348 = DIRECTION ( 'NONE',  ( 0.000000000000000000, 0.5877852522924685852, 0.8090169943749507819 ) ) ;
#3349 = ORIENTED_EDGE ( 'NONE', *, *, #46529, .F. ) ;
#3350 = EDGE_CURVE ( 'NONE', #19670, #60432, #68257, .T. ) ;
#3351 = ORIENTED_EDGE ( 'NONE', *, *, #14574, .T. ) ;
#3352 = DIRECTION ( 'NONE',  ( -1.000000000000000000, 0.000000000000000000, -0.000000000000000000 ) ) ;
#3353 = FACE_OUTER_BOUND ( 'NONE', #57335, .T. ) ;
#3354 = VERTEX_POINT ( 'NONE', #49111 ) ;
#3355 = DIRECTION ( 'NONE',  ( 0.8191520442889890230, 1.003171929053521295E-16, -0.5735764363510501562 ) ) ;
#3356 = CARTESIAN_POINT ( 'NONE',  ( 95.00000000000000000, -213.0599564267049857, 79.44312500173428759 ) ) ;
#3357 = CARTESIAN_POINT ( 'NONE',  ( 94.99999999999998579, 86.94004357329500010, 85.07874999999999943 ) ) ;
#3358 = ORIENTED_EDGE ( 'NONE', *, *, #17803, .T. ) ;
#3359 = DIRECTION ( 'NONE',  ( -1.000000000000000000, 0.000000000000000000, 0.000000000000000000 ) ) ;
#3360 = EDGE_CURVE ( 'NONE', #56357, #68556, #30997, .T. ) ;
#3361 = DIRECTION ( 'NONE',  ( 0.9227826878668540234, 0.3853207896976547087, -0.000000000000000000 ) ) ;
#3362 = ORIENTED_EDGE ( 'NONE', *, *, #10881, .F. ) ;
#3363 = CYLINDRICAL_SURFACE ( 'NONE', #39251, 77.49899999999999523 ) ;
#3364 =( BOUNDED_CURVE ( )  B_SPLINE_CURVE ( 2, ( #47605, #11536, #51773, #53613, #37070, #42712, #26143 ),
 .UNSPECIFIED., .F., .F. ) 
 B_SPLINE_CURVE_WITH_KNOTS ( ( 3, 2, 2, 3 ),
 ( 0.5833333333333329263, 0.5902777777777776791, 0.5972222222222223209, 0.6041666666666670737 ),
 .UNSPECIFIED. ) 
 CURVE ( )  GEOMETRIC_REPRESENTATION_ITEM ( )  RATIONAL_B_SPLINE_CURVE ( ( 1.000000000000008660, 0.8660254037844301589, 1.000000000000000000, 0.8660254037844387076, 1.000000000000000000, 0.8660254037844301589, 1.000000000000008660 ) ) 
 REPRESENTATION_ITEM ( '' )  );
#3365 = CARTESIAN_POINT ( 'NONE',  ( -92.69370383062504004, 90.00000000000004263, 88.84906250086716284 ) ) ;
#3366 = CARTESIAN_POINT ( 'NONE',  ( 93.84685191531248449, 88.00268892867053694, 82.76364583420047438 ) ) ;
#3367 = EDGE_LOOP ( 'NONE', ( #6658, #24611, #8874, #51856 ) ) ;
#3368 = LINE ( 'NONE', #71745, #33612 ) ;
#3369 = VERTEX_POINT ( 'NONE', #22028 ) ;
#3370 = CARTESIAN_POINT ( 'NONE',  ( 0.000000000000000000, -41.91543099594819921, 2.663952781846001816 ) ) ;
#3371 = ORIENTED_EDGE ( 'NONE', *, *, #21136, .T. ) ;
#3372 = ORIENTED_EDGE ( 'NONE', *, *, #26905, .F. ) ;
#3373 = CIRCLE ( 'NONE', #47726, 31.99999999999998934 ) ;
#3374 = ORIENTED_EDGE ( 'NONE', *, *, #72333, .T. ) ;
#3375 = ORIENTED_EDGE ( 'NONE', *, *, #36266, .T. ) ;
#3376 = CARTESIAN_POINT ( 'NONE',  ( 0.000000000000000000, 10.30890764327382136, 81.34940948281339956 ) ) ;
#3377 = CARTESIAN_POINT ( 'NONE',  ( 11.99999999999999822, -63.18004540532995605, -44.88180994100445531 ) ) ;
#3378 = ORIENTED_EDGE ( 'NONE', *, *, #63066, .F. ) ;
#3379 = DIRECTION ( 'NONE',  ( 0.000000000000000000, 0.9876883405951382144, -0.1564344650402276493 ) ) ;
#3380 = CARTESIAN_POINT ( 'NONE',  ( -96.15314808468747287, -208.0026889286704943, 78.74197916753381321 ) ) ;
#3381 = EDGE_LOOP ( 'NONE', ( #68818, #29763, #35375, #48631 ) ) ;
#3382 = DIRECTION ( 'NONE',  ( -0.000000000000000000, -0.000000000000000000, 1.000000000000000000 ) ) ;
#3383 = DIRECTION ( 'NONE',  ( 0.000000000000000000, -0.9969173337331287410, 0.07845909572783495156 ) ) ;
#3384 = CARTESIAN_POINT ( 'NONE',  ( 97.64999999999997726, 89.99997826787402744, 89.12687425009507081 ) ) ;
#3385 = DIRECTION ( 'NONE',  ( -1.000000000000000000, 0.000000000000000000, -0.000000000000000000 ) ) ;
#3386 = CARTESIAN_POINT ( 'NONE',  ( 0.000000000000000000, 0.000000000000000000, -5.500000000000000000 ) ) ;
#3387 = CIRCLE ( 'NONE', #33341, 77.49900000000000944 ) ;
#3388 = CARTESIAN_POINT ( 'NONE',  ( 6.000000000000000000, 76.69515212746016175, 29.01471420065590578 ) ) ;
#3390 = CIRCLE ( 'NONE', #15380, 77.49900000000002365 ) ;
#3389 = CARTESIAN_POINT ( 'NONE',  ( 94.99999999999998579, 92.66308142843932671, 86.94406250086714749 ) ) ;
#3391 = CYLINDRICAL_SURFACE ( 'NONE', #42381, 42.00000000000000000 ) ;
#3392 = CARTESIAN_POINT ( 'NONE',  ( 10.00000000000000000, 27.05870788708231700, 26.08949754953034272 ) ) ;
#3393 = CIRCLE ( 'NONE', #35763, 42.00000000000000000 ) ;
#3394 = CARTESIAN_POINT ( 'NONE',  ( 95.04693102382874770, -212.6495843973424940, 75.00000002508419072 ) ) ;
#3395 = AXIS2_PLACEMENT_3D ( 'NONE', #30919, #53862, #18898 ) ;
#3396 = CARTESIAN_POINT ( 'NONE',  ( -92.35000000000000853, -210.0000001051137701, 86.58687499784845443 ) ) ;
#3397 = CARTESIAN_POINT ( 'NONE',  ( 15.00000000000000000, 20.85821328998741109, -10.92862929874522671 ) ) ;
#3398 = CYLINDRICAL_SURFACE ( 'NONE', #36230, 82.00000000000000000 ) ;
#3399 = CIRCLE ( 'NONE', #18982, 37.49900000000000233 ) ;
#3400 = DIRECTION ( 'NONE',  ( -0.000000000000000000, -0.000000000000000000, 1.000000000000000000 ) ) ;
#3401 = CARTESIAN_POINT ( 'NONE',  ( 97.64999999999821512, 90.00000306648260562, 75.79187510780352000 ) ) ;
#3402 = EDGE_CURVE ( 'NONE', #46548, #64355, #67522, .T. ) ;
#3403 = EDGE_CURVE ( 'NONE', #68341, #45880, #56231, .T. ) ;
#3404 = PLANE ( 'NONE',  #42489 ) ;
#3405 = CARTESIAN_POINT ( 'NONE',  ( 97.30629616937498838, 90.00000000000002842, 89.48406250086715374 ) ) ;
#3406 = DIRECTION ( 'NONE',  ( 0.000000000000000000, 0.000000000000000000, 1.000000000000000000 ) ) ;
#3407 = EDGE_CURVE ( 'NONE', #14315, #53082, #7509, .T. ) ;
#3408 = FACE_OUTER_BOUND ( 'NONE', #15745, .T. ) ;
#3409 = CARTESIAN_POINT ( 'NONE',  ( -94.99999999999997158, -213.0599564267049857, 88.88875000000000171 ) ) ;
#3410 = EDGE_CURVE ( 'NONE', #58605, #30791, #29028, .T. ) ;
#3411 = CARTESIAN_POINT ( 'NONE',  ( 6.000000000000000000, -29.01471420065616513, 76.69515212746007649 ) ) ;
#3412 = EDGE_CURVE ( 'NONE', #5010, #3531, #52627, .T. ) ;
#3413 = EDGE_LOOP ( 'NONE', ( #10470, #25244, #45684, #45485 ) ) ;
#3414 = DIRECTION ( 'NONE',  ( -1.000000000000000000, -0.000000000000000000, -0.000000000000000000 ) ) ;
#3415 = DIRECTION ( 'NONE',  ( 0.000000000000000000, 0.000000000000000000, 1.000000000000000000 ) ) ;
#3416 = VECTOR ( 'NONE', #19366, 1000.000000000000000 ) ;
#3417 = VECTOR ( 'NONE', #56473, 1000.000000000000000 ) ;
#3418 = DIRECTION ( 'NONE',  ( 1.000000000000000000, 1.427937372958405461E-15, 7.962523111839130290E-16 ) ) ;
#3419 = VECTOR ( 'NONE', #71589, 1000.000000000000000 ) ;
#3420 = ORIENTED_EDGE ( 'NONE', *, *, #4156, .F. ) ;
#3421 = ORIENTED_EDGE ( 'NONE', *, *, #2614, .T. ) ;
#3422 = LINE ( 'NONE', #32695, #33508 ) ;
#3423 = DIRECTION ( 'NONE',  ( 0.000000000000000000, 0.000000000000000000, 1.000000000000000000 ) ) ;
#3424 = ORIENTED_EDGE ( 'NONE', *, *, #36379, .F. ) ;
#3425 = CARTESIAN_POINT ( 'NONE',  ( 97.30629616937498838, -208.6684592857803295, 82.39322916753381776 ) ) ;
#3426 = CARTESIAN_POINT ( 'NONE',  ( 95.00000000000000000, -207.3369185715606307, 83.92781250086716227 ) ) ;
#3427 = ORIENTED_EDGE ( 'NONE', *, *, #42184, .T. ) ;
#3428 = CARTESIAN_POINT ( 'NONE',  ( 92.69370383062501162, -211.3315407142195852, 85.40947916753380298 ) ) ;
#3429 = CIRCLE ( 'NONE', #56287, 31.99999999999999645 ) ;
#3430 = ORIENTED_EDGE ( 'NONE', *, *, #68282, .F. ) ;
#3431 = FACE_BOUND ( 'NONE', #1885, .T. ) ;
#3432 = ORIENTED_EDGE ( 'NONE', *, *, #69590, .F. ) ;
#3433 = EDGE_CURVE ( 'NONE', #52810, #22408, #54512, .T. ) ;
#3434 = EDGE_CURVE ( 'NONE', #64359, #61324, #13010, .T. ) ;
#3435 = CARTESIAN_POINT ( 'NONE',  ( -97.30629616937501680, 91.33154071421968467, 78.31864583420050963 ) ) ;
#3436 = AXIS2_PLACEMENT_3D ( 'NONE', #73311, #3084, #21823 ) ;
#3437 = ORIENTED_EDGE ( 'NONE', *, *, #44984, .F. ) ;
#3438 = VERTEX_POINT ( 'NONE', #10001 ) ;
#3439 = AXIS2_PLACEMENT_3D ( 'NONE', #55501, #14153, #61149 ) ;
#3440 = CARTESIAN_POINT ( 'NONE',  ( -3.000000000000000000, -10.45096189432314837, -21.10159698893440350 ) ) ;
#3441 = AXIS2_PLACEMENT_3D ( 'NONE', #58800, #70422, #64445 ) ;
#3442 = VERTEX_POINT ( 'NONE', #44225 ) ;
#3443 = DIRECTION ( 'NONE',  ( -1.000000000000000000, 0.000000000000000000, 0.000000000000000000 ) ) ;
#3444 = CARTESIAN_POINT ( 'NONE',  ( -92.35000000010070664, 90.00002309722640348, 83.41187580057902551 ) ) ;
#3445 = VECTOR ( 'NONE', #58676, 1000.000000000000114 ) ;
#3446 = ORIENTED_EDGE ( 'NONE', *, *, #45007, .F. ) ;
#3447 = DIRECTION ( 'NONE',  ( -0.000000000000000000, -0.000000000000000000, 1.000000000000000000 ) ) ;
#3448 = EDGE_CURVE ( 'NONE', #53520, #54954, #56247, .T. ) ;
#3449 = ORIENTED_EDGE ( 'NONE', *, *, #73309, .T. ) ;
#3450 = FACE_OUTER_BOUND ( 'NONE', #20245, .T. ) ;
#3451 = VERTEX_POINT ( 'NONE', #74271 ) ;
#3452 = ORIENTED_EDGE ( 'NONE', *, *, #7714, .F. ) ;
#3453 = ORIENTED_EDGE ( 'NONE', *, *, #16539, .F. ) ;
#3454 = CARTESIAN_POINT ( 'NONE',  ( 92.69370383062501162, -208.6684592857803011, 78.15989583420048348 ) ) ;
#3455 = FACE_OUTER_BOUND ( 'NONE', #45313, .T. ) ;
#3456 = ORIENTED_EDGE ( 'NONE', *, *, #11366, .T. ) ;
#3457 = VERTEX_POINT ( 'NONE', #22787 ) ;
#3458 = ORIENTED_EDGE ( 'NONE', *, *, #49891, .F. ) ;
#3459 = CARTESIAN_POINT ( 'NONE',  ( -94.99999999999997158, -213.0599564267049857, 84.44374999999999432 ) ) ;
#3460 = CARTESIAN_POINT ( 'NONE',  ( 5.000000000000002665, 22.90783923731629912, 78.73519480814962890 ) ) ;
#3461 = CARTESIAN_POINT ( 'NONE',  ( -93.84685191531254134, 91.99731107132950569, 78.15989583420049769 ) ) ;
#3462 = EDGE_LOOP ( 'NONE', ( #44510, #51328, #29841, #41810 ) ) ;
#3463 = CARTESIAN_POINT ( 'NONE',  ( 94.99999999999998579, 87.33691857156068750, 76.46656250086712703 ) ) ;
#3464 = ORIENTED_EDGE ( 'NONE', *, *, #9569, .F. ) ;
#3465 = DIRECTION ( 'NONE',  ( 1.000000000000000000, 0.000000000000000000, 0.000000000000000000 ) ) ;
#3466 = CARTESIAN_POINT ( 'NONE',  ( -96.15314808468747287, -208.0026889286704943, 89.53697916753381492 ) ) ;
#3467 = AXIS2_PLACEMENT_3D ( 'NONE', #13316, #1711, #24598 ) ;
#3468 = CARTESIAN_POINT ( 'NONE',  ( -23.30023580412278861, -123.4057321492263384, -2.500000000000000000 ) ) ;
#3469 = DIRECTION ( 'NONE',  ( 0.000000000000000000, 0.000000000000000000, -1.000000000000000000 ) ) ;
#3470 = DIRECTION ( 'NONE',  ( -0.000000000000000000, -0.000000000000000000, 1.000000000000000000 ) ) ;
#3471 = CARTESIAN_POINT ( 'NONE',  ( -94.99999999999997158, -207.3369185715606307, 79.32406250086714294 ) ) ;
#3472 = AXIS2_PLACEMENT_3D ( 'NONE', #10217, #62491, #33511 ) ;
#3473 = CARTESIAN_POINT ( 'NONE',  ( 11.99999999999999822, 20.40083707022882820, 72.35432306680490910 ) ) ;
#3474 = DIRECTION ( 'NONE',  ( 1.000000000000000000, -0.000000000000000000, -0.000000000000000000 ) ) ;
#3475 = DIRECTION ( 'NONE',  ( -1.000000000000000000, 0.000000000000000000, 0.000000000000000000 ) ) ;
#3476 = EDGE_LOOP ( 'NONE', ( #9812, #6944, #5386, #24783 ) ) ;
#3477 = ORIENTED_EDGE ( 'NONE', *, *, #11438, .T. ) ;
#3478 = LINE ( 'NONE', #50793, #52891 ) ;
#3479 = CIRCLE ( 'NONE', #59879, 31.99999999999998934 ) ;
#3480 = CARTESIAN_POINT ( 'NONE',  ( -3.000000000000000000, -3.948201729842348850, 23.21447184625293048 ) ) ;
#3481 = DIRECTION ( 'NONE',  ( 0.000000000000000000, 0.000000000000000000, 1.000000000000000000 ) ) ;
#3482 = CARTESIAN_POINT ( 'NONE',  ( -92.69370383062504004, 90.00000000000004263, 85.51531250086713953 ) ) ;
#3483 = CYLINDRICAL_SURFACE ( 'NONE', #28666, 16.00000000000000000 ) ;
#3484 = LINE ( 'NONE', #7994, #39798 ) ;
#3485 = ORIENTED_EDGE ( 'NONE', *, *, #55841, .F. ) ;
#3486 = DIRECTION ( 'NONE',  ( 0.000000000000000000, 0.000000000000000000, -1.000000000000000000 ) ) ;
#3487 = AXIS2_PLACEMENT_3D ( 'NONE', #58012, #13255, #70754 ) ;
#3488 = AXIS2_PLACEMENT_3D ( 'NONE', #55970, #14996, #61618 ) ;
#3489 = CARTESIAN_POINT ( 'NONE',  ( 5.000000000000000000, -16.65560815589439159, 38.55633173627004595 ) ) ;
#3490 = CARTESIAN_POINT ( 'NONE',  ( -97.64999999999996305, -209.9999999999999716, 90.00000000000000000 ) ) ;
#3491 = AXIS2_PLACEMENT_3D ( 'NONE', #40604, #16936, #5666 ) ;
#3492 = CARTESIAN_POINT ( 'NONE',  ( 0.000000000000000000, 12.26510123303259725, 35.53030884539089840 ) ) ;
#3493 = EDGE_CURVE ( 'NONE', #57268, #14085, #39329, .T. ) ;
#3494 = CARTESIAN_POINT ( 'NONE',  ( -2.018853055115723105, 4.607917337070899677, -0.5666985376598566715 ) ) ;
#3495 = CARTESIAN_POINT ( 'NONE',  ( -12.50000000000000000, -107.5000000000000000, 2.500000000000000000 ) ) ;
#3496 = CARTESIAN_POINT ( 'NONE',  ( -93.84685191531248449, -208.0026889286704943, 82.60489583420049087 ) ) ;
#3497 = VECTOR ( 'NONE', #72553, 1000.000000000000000 ) ;
#3498 = AXIS2_PLACEMENT_3D ( 'NONE', #61744, #27517, #38059 ) ;
#3499 = EDGE_CURVE ( 'NONE', #40964, #62894, #11121, .T. ) ;
#3500 = LINE ( 'NONE', #62107, #44887 ) ;
#3501 = TOROIDAL_SURFACE ( 'NONE', #49085, 18.00000000000000000, 3.300000000000000266 ) ;
#3502 = EDGE_CURVE ( 'NONE', #31031, #23968, #72707, .T. ) ;
#3503 = DIRECTION ( 'NONE',  ( 0.000000000000000000, 0.000000000000000000, 1.000000000000000000 ) ) ;
#3504 = DIRECTION ( 'NONE',  ( -1.000000000000000000, -0.000000000000000000, -0.000000000000000000 ) ) ;
#3505 = FACE_OUTER_BOUND ( 'NONE', #33164, .T. ) ;
#3506 = ORIENTED_EDGE ( 'NONE', *, *, #243, .F. ) ;
#3507 = PLANE ( 'NONE',  #24549 ) ;
#3508 = CYLINDRICAL_SURFACE ( 'NONE', #41890, 16.00000000000000000 ) ;
#3509 = FACE_BOUND ( 'NONE', #1459, .T. ) ;
#3510 = DIRECTION ( 'NONE',  ( -0.000000000000000000, -0.000000000000000000, 1.000000000000000000 ) ) ;
#3511 = ADVANCED_FACE ( 'NONE', ( #73892 ), #39706, .F. ) ;
#3512 = ORIENTED_EDGE ( 'NONE', *, *, #53638, .T. ) ;
#3513 = CIRCLE ( 'NONE', #21504, 31.99999999999999289 ) ;
#3514 = EDGE_CURVE ( 'NONE', #12638, #64991, #4384, .T. ) ;
#3515 = CARTESIAN_POINT ( 'NONE',  ( -93.67500000000003979, 92.29496732002878900, 75.89770833506763381 ) ) ;
#3516 = SURFACE_STYLE_FILL_AREA ( #32785 ) ;
#3517 = ORIENTED_EDGE ( 'NONE', *, *, #14277, .F. ) ;
#3518 = AXIS2_PLACEMENT_3D ( 'NONE', #59122, #19618, #7247 ) ;
#3519 = DIRECTION ( 'NONE',  ( -0.000000000000000000, -0.000000000000000000, -1.000000000000000000 ) ) ;
#3520 = LINE ( 'NONE', #54994, #37599 ) ;
#3521 = ORIENTED_EDGE ( 'NONE', *, *, #48324, .F. ) ;
#3522 = AXIS2_PLACEMENT_3D ( 'NONE', #57326, #53167, #34384 ) ;
#3523 = AXIS2_PLACEMENT_3D ( 'NONE', #3775, #72529, #21033 ) ;
#3524 = CARTESIAN_POINT ( 'NONE',  ( 11.99999999999999822, 0.000000000000000000, 0.000000000000000000 ) ) ;
#3525 = AXIS2_PLACEMENT_3D ( 'NONE', #7787, #30705, #352 ) ;
#3526 = EDGE_LOOP ( 'NONE', ( #43877, #10858, #22393, #6256 ) ) ;
#3527 = LINE ( 'NONE', #26053, #73000 ) ;
#3528 = EDGE_CURVE ( 'NONE', #63719, #49170, #54172, .T. ) ;
#3529 = EDGE_CURVE ( 'NONE', #65294, #46548, #73146, .T. ) ;
#3530 = AXIS2_PLACEMENT_3D ( 'NONE', #73271, #61268, #55246 ) ;
#3531 = VERTEX_POINT ( 'NONE', #17868 ) ;
#3532 = ORIENTED_EDGE ( 'NONE', *, *, #62824, .T. ) ;
#3533 = CIRCLE ( 'NONE', #40765, 31.99999999999998579 ) ;
#3534 = EDGE_LOOP ( 'NONE', ( #9717, #49196, #61310, #60382 ) ) ;
#3535 = EDGE_LOOP ( 'NONE', ( #35759, #37357, #71112, #37446 ) ) ;
#3536 = EDGE_LOOP ( 'NONE', ( #57725, #27089 ) ) ;
#3537 = EDGE_LOOP ( 'NONE', ( #43275, #49723, #49201, #1769 ) ) ;
#3538 = CARTESIAN_POINT ( 'NONE',  ( 92.69370383062498320, 91.33154071421968467, 77.04864583420048518 ) ) ;
#3539 = CARTESIAN_POINT ( 'NONE',  ( 0.000000000000000000, -38.55633173626998911, -16.65560815589452304 ) ) ;
#3540 = CYLINDRICAL_SURFACE ( 'NONE', #38042, 82.00000000000000000 ) ;
#3541 = ORIENTED_EDGE ( 'NONE', *, *, #14309, .F. ) ;
#3543 = VERTEX_POINT ( 'NONE', #40813 ) ;
#3542 = AXIS2_PLACEMENT_3D ( 'NONE', #20647, #60510, #54854 ) ;
#3544 = ORIENTED_EDGE ( 'NONE', *, *, #2065, .T. ) ;
#3545 = CARTESIAN_POINT ( 'NONE',  ( 97.30629616937498838, 91.33154071421968467, 87.47322916753381605 ) ) ;
#3546 = VERTEX_POINT ( 'NONE', #46825 ) ;
#3547 = CARTESIAN_POINT ( 'NONE',  ( 95.00000000000000000, -212.6630814284392557, 89.16656250086712987 ) ) ;
#3548 = AXIS2_PLACEMENT_3D ( 'NONE', #44001, #67298, #27055 ) ;
#3549 = VECTOR ( 'NONE', #50670, 1000.000000000000000 ) ;
#3550 = DIRECTION ( 'NONE',  ( 0.06036602427439052843, 0.9981763086315480482, 1.977699523466503551E-17 ) ) ;
#3551 = CARTESIAN_POINT ( 'NONE',  ( 11.99999999999999822, -6.903761155837269570, -77.19088730480530103 ) ) ;
#3552 = CARTESIAN_POINT ( 'NONE',  ( 11.99999999999999822, 0.000000000000000000, 0.000000000000000000 ) ) ;
#3553 = CARTESIAN_POINT ( 'NONE',  ( 94.99999999999998579, 93.05995642670504253, 77.85562500173431033 ) ) ;
#3554 = CARTESIAN_POINT ( 'NONE',  ( -92.34999999999999432, -208.4700217866474645, 84.09979166840098230 ) ) ;
#3555 = FACE_OUTER_BOUND ( 'NONE', #56420, .T. ) ;
#3556 = CIRCLE ( 'NONE', #29919, 16.00000000000000711 ) ;
#3557 = CARTESIAN_POINT ( 'NONE',  ( 5.000000000000002665, 44.99326035066052043, 68.55367621811159040 ) ) ;
#3558 = CARTESIAN_POINT ( 'NONE',  ( -96.32499999999996021, -212.2949673200287179, 76.85020833506763438 ) ) ;
#3559 = CARTESIAN_POINT ( 'NONE',  ( -92.69370383062502583, 91.33154071421968467, 88.26697916753381890 ) ) ;
#3560 = ORIENTED_EDGE ( 'NONE', *, *, #32899, .F. ) ;
#3562 = CARTESIAN_POINT ( 'NONE',  ( -93.84685191531252713, 88.00268892867056536, 87.94947916753380923 ) ) ;
#3561 = CARTESIAN_POINT ( 'NONE',  ( 93.84685191531248449, 91.99731107132950569, 88.26697916753380468 ) ) ;
#3563 = EDGE_LOOP ( 'NONE', ( #62760, #42019, #42563, #74132 ) ) ;
#3564 = PLANE ( 'NONE',  #49057 ) ;
#3565 = CARTESIAN_POINT ( 'NONE',  ( 10.00000000000000000, -10.96151621346461447, -35.95386929396268272 ) ) ;
#3566 = CYLINDRICAL_SURFACE ( 'NONE', #43922, 2.649999999999985700 ) ;
#3567 = FACE_OUTER_BOUND ( 'NONE', #46877, .T. ) ;
#3568 = CARTESIAN_POINT ( 'NONE',  ( 12.50000000000000000, -132.5000000000000000, 40.00000000000000000 ) ) ;
#3569 = CARTESIAN_POINT ( 'NONE',  ( -2.977765906491215642, 0.000000000000000000, 0.000000000000000000 ) ) ;
#3570 = DIRECTION ( 'NONE',  ( -1.000000000000000000, -0.000000000000000000, -0.000000000000000000 ) ) ;
#3571 = LINE ( 'NONE', #71209, #52794 ) ;
#3572 = ORIENTED_EDGE ( 'NONE', *, *, #2231, .F. ) ;
#3573 = ORIENTED_EDGE ( 'NONE', *, *, #24608, .F. ) ;
#3574 = CARTESIAN_POINT ( 'NONE',  ( -96.32500000000001705, 92.29496732002878900, 82.90916666666666401 ) ) ;
#3575 = CARTESIAN_POINT ( 'NONE',  ( 0.000000000000000000, 0.000000000000000000, -43.79999999999998295 ) ) ;
#3576 = CYLINDRICAL_SURFACE ( 'NONE', #66928, 12.50000000000000000 ) ;
#3577 = DIRECTION ( 'NONE',  ( 0.000000000000000000, 0.000000000000000000, 1.000000000000000000 ) ) ;
#3578 = EDGE_CURVE ( 'NONE', #53383, #63709, #51752, .T. ) ;
#3579 = CARTESIAN_POINT ( 'NONE',  ( 0.000000000000000000, 2.946379043147425492, -75.11764819372145041 ) ) ;
#3580 = DIRECTION ( 'NONE',  ( -1.000000000000000000, -0.000000000000000000, 0.000000000000000000 ) ) ;
#3581 =( BOUNDED_CURVE ( )  B_SPLINE_CURVE ( 2, ( #8612, #61597, #2997, #25889, #72845, #21344, #20627 ),
 .UNSPECIFIED., .F., .F. ) 
 B_SPLINE_CURVE_WITH_KNOTS ( ( 3, 2, 2, 3 ),
 ( 0.02116741234835334273, 0.02822306216366812434, 0.03527882770458510425, 0.04233441017615420521 ),
 .UNSPECIFIED. ) 
 CURVE ( )  GEOMETRIC_REPRESENTATION_ITEM ( )  RATIONAL_B_SPLINE_CURVE ( ( 0.9999956052857933431, 0.8660276011775827065, 1.000000000000000000, 0.8660254037844387076, 1.000000000000000000, 0.8660288798979544067, 0.9999930479533516436 ) ) 
 REPRESENTATION_ITEM ( '' )  );
#3582 = DIRECTION ( 'NONE',  ( -0.6516173805718079581, 0.7585478161175704948, 0.000000000000000000 ) ) ;
#3583 = AXIS2_PLACEMENT_3D ( 'NONE', #69198, #34986, #16576 ) ;
#3584 = ORIENTED_EDGE ( 'NONE', *, *, #2089, .T. ) ;
#3585 = PRODUCT_DEFINITION ( 'UNKNOWN', '', #40042, #37882 ) ;
#3586 = CARTESIAN_POINT ( 'NONE',  ( -92.69370383062502583, 91.33154071421968467, 83.02822916753379445 ) ) ;
#3587 = EDGE_CURVE ( 'NONE', #51903, #72660, #70099, .T. ) ;
#3589 = CARTESIAN_POINT ( 'NONE',  ( 92.34999999999999432, 90.00000000000002842, 82.45937500173430124 ) ) ;
#3588 = CIRCLE ( 'NONE', #71971, 77.49899999999999523 ) ;
#3590 = CYLINDRICAL_SURFACE ( 'NONE', #58274, 16.00000000000000000 ) ;
#3591 = CARTESIAN_POINT ( 'NONE',  ( 11.99999999999999822, 26.01480285779837232, 70.53064760720326376 ) ) ;
#3592 = EDGE_CURVE ( 'NONE', #14025, #14710, #46080, .T. ) ;
#3593 = DIRECTION ( 'NONE',  ( -1.000000000000000000, -0.000000000000000000, 0.000000000000000000 ) ) ;
#3594 = AXIS2_PLACEMENT_3D ( 'NONE', #45396, #32971, #39006 ) ;
#3595 = DIRECTION ( 'NONE',  ( -1.000000000000000000, 0.000000000000000000, -0.000000000000000000 ) ) ;
#3596 = FACE_OUTER_BOUND ( 'NONE', #73753, .T. ) ;
#3597 = DIRECTION ( 'NONE',  ( -1.000000000000000000, 0.000000000000000000, -0.000000000000000000 ) ) ;
#3598 = LINE ( 'NONE', #66002, #53293 ) ;
#3599 = EDGE_CURVE ( 'NONE', #30760, #39726, #45765, .T. ) ;
#3600 =( BOUNDED_CURVE ( )  B_SPLINE_CURVE ( 2, ( #32303, #38333, #61271, #9760, #61641, #27034, #3401 ),
 .UNSPECIFIED., .F., .F. ) 
 B_SPLINE_CURVE_WITH_KNOTS ( ( 3, 2, 2, 3 ),
 ( 0.8890265259358468564, 0.8960822236920598094, 0.9031379892329426395, 0.9101937466091534201 ),
 .UNSPECIFIED. ) 
 CURVE ( )  GEOMETRIC_REPRESENTATION_ITEM ( )  RATIONAL_B_SPLINE_CURVE ( ( 0.9999974258394828119, 0.8660266908770624106, 1.000000000000000000, 0.8660254037844387076, 1.000000000000000000, 0.8660254037844387076, 1.000000000000000000 ) ) 
 REPRESENTATION_ITEM ( '' )  );
#3601 = EDGE_CURVE ( 'NONE', #22350, #20056, #59793, .T. ) ;
#3602 = CARTESIAN_POINT ( 'NONE',  ( 92.69370383062498320, 90.00000000000002842, 80.91156250086716284 ) ) ;
#3603 = CARTESIAN_POINT ( 'NONE',  ( -92.69370383062498320, -211.3315407142195852, 82.44614583420049314 ) ) ;
#3604 = CARTESIAN_POINT ( 'NONE',  ( 97.64999999999999147, 90.00000000000002842, 90.00000000000000000 ) ) ;
#3605 = VECTOR ( 'NONE', #35262, 1000.000000000000000 ) ;
#3606 = VERTEX_POINT ( 'NONE', #69738 ) ;
#3607 = CYLINDRICAL_SURFACE ( 'NONE', #16067, 77.49899999999999523 ) ;
#3608 = CARTESIAN_POINT ( 'NONE',  ( -97.64999999999994884, -211.5299782133524502, 77.35291666666665833 ) ) ;
#3609 = DIRECTION ( 'NONE',  ( -1.000000000000000000, 0.000000000000000000, 0.000000000000000000 ) ) ;
#3610 = AXIS2_PLACEMENT_3D ( 'NONE', #57742, #62274, #57006 ) ;
#3611 = VECTOR ( 'NONE', #3700, 1000.000000000000000 ) ;
#3613 = ADVANCED_FACE ( 'NONE', ( #69014 ), #6599, .T. ) ;
#3612 = CARTESIAN_POINT ( 'NONE',  ( 92.69370383062501162, -208.6684592857803011, 83.87489583420047268 ) ) ;
#3614 = ORIENTED_EDGE ( 'NONE', *, *, #35996, .T. ) ;
#3615 = EDGE_CURVE ( 'NONE', #14221, #69250, #35890, .T. ) ;
#3616 = CARTESIAN_POINT ( 'NONE',  ( 11.99999999999999822, 0.000000000000000000, 0.000000000000000000 ) ) ;
#3617 = VERTEX_POINT ( 'NONE', #6240 ) ;
#3618 = CARTESIAN_POINT ( 'NONE',  ( 0.000000000000000000, -11.95096189432345390, 23.69967320028757385 ) ) ;
#3619 = EDGE_LOOP ( 'NONE', ( #32437, #43961, #12188, #63772 ) ) ;
#3620 = CYLINDRICAL_SURFACE ( 'NONE', #44325, 16.00000000000000000 ) ;
#3621 = CARTESIAN_POINT ( 'NONE',  ( 92.69370383062501162, -211.3315407142195852, 77.15447916753382174 ) ) ;
#3622 = LINE ( 'NONE', #64911, #16461 ) ;
#3623 = DIRECTION ( 'NONE',  ( 1.000000000000000000, 0.000000000000000000, 0.000000000000000000 ) ) ;
#3624 = CARTESIAN_POINT ( 'NONE',  ( -95.79297114439312111, 87.49569407151190603, 74.98272308147875265 ) ) ;
#3625 = CARTESIAN_POINT ( 'NONE',  ( 92.69370383062498320, 88.66845928578037217, 87.94947916753382344 ) ) ;
#3626 = CARTESIAN_POINT ( 'NONE',  ( 11.99999999999999822, -5.256550761633395297, 77.32052557432841411 ) ) ;
#3627 = CARTESIAN_POINT ( 'NONE',  ( 92.35000000000002274, -208.4700217866474645, 82.96208333333333940 ) ) ;
#3628 = ORIENTED_EDGE ( 'NONE', *, *, #36380, .T. ) ;
#3629 = ORIENTED_EDGE ( 'NONE', *, *, #43544, .F. ) ;
#3630 = CIRCLE ( 'NONE', #25192, 15.99999999999999822 ) ;
#3631 = ORIENTED_EDGE ( 'NONE', *, *, #67763, .T. ) ;
#3632 = VERTEX_POINT ( 'NONE', #64117 ) ;
#3633 = DIRECTION ( 'NONE',  ( -1.000000000000000000, -0.000000000000000000, -0.000000000000000000 ) ) ;
#3634 =( NAMED_UNIT ( * ) PLANE_ANGLE_UNIT ( ) SI_UNIT ( $, .RADIAN. ) );
#3635 = CARTESIAN_POINT ( 'NONE',  ( -93.84685191531252713, 88.00268892867056536, 84.29822916753381890 ) ) ;
#3636 = FACE_OUTER_BOUND ( 'NONE', #71266, .T. ) ;
#3637 = CIRCLE ( 'NONE', #34847, 37.49900000000000944 ) ;
#3638 = CARTESIAN_POINT ( 'NONE',  ( 4.999999999999999112, -41.91543099594819921, 2.663952781846001816 ) ) ;
#3639 = CARTESIAN_POINT ( 'NONE',  ( 92.34999999999999432, 91.52997821335252127, 76.61208333333333087 ) ) ;
#3640 = DIRECTION ( 'NONE',  ( -1.000000000000000000, -0.000000000000000000, -0.000000000000000000 ) ) ;
#3641 = ORIENTED_EDGE ( 'NONE', *, *, #43555, .F. ) ;
#3642 = CARTESIAN_POINT ( 'NONE',  ( -93.67499999999998295, -207.7050326799711968, 86.05770833506763040 ) ) ;
#3643 = ORIENTED_EDGE ( 'NONE', *, *, #24107, .F. ) ;
#3644 = DIRECTION ( 'NONE',  ( 3.035766082959412415E-16, 1.000000000000000000, 0.000000000000000000 ) ) ;
#3645 = ORIENTED_EDGE ( 'NONE', *, *, #8579, .F. ) ;
#3646 = CARTESIAN_POINT ( 'NONE',  ( -96.32500000000001705, 92.29496732002878900, 81.71854166840095957 ) ) ;
#3647 = ORIENTED_EDGE ( 'NONE', *, *, #5984, .T. ) ;
#3648 = CARTESIAN_POINT ( 'NONE',  ( 94.99999999999998579, 87.33691857156068750, 88.05531250086716000 ) ) ;
#3649 = CARTESIAN_POINT ( 'NONE',  ( 1.029419772574596825, -118.9089936151275140, -2.500000000000000000 ) ) ;
#3651 = ADVANCED_FACE ( 'NONE', ( #63376 ), #264, .F. ) ;
#3650 = CYLINDRICAL_SURFACE ( 'NONE', #24652, 77.49899999999999523 ) ;
#3652 = CARTESIAN_POINT ( 'NONE',  ( -93.67500000000003979, 87.70503267997129626, 83.94104166840097037 ) ) ;
#3653 = AXIS2_PLACEMENT_3D ( 'NONE', #56460, #12425, #69210 ) ;
#3654 = CARTESIAN_POINT ( 'NONE',  ( 11.99999999999999822, 65.59268652807263322, -36.72794159290169347 ) ) ;
#3655 = CARTESIAN_POINT ( 'NONE',  ( -94.99999999999997158, -209.9999999999999716, 90.00000000000000000 ) ) ;
#3656 = ORIENTED_EDGE ( 'NONE', *, *, #33586, .T. ) ;
#3657 = CARTESIAN_POINT ( 'NONE',  ( -93.67500000000003979, 92.29496732002878900, 80.97770833506763211 ) ) ;
#3658 = AXIS2_PLACEMENT_3D ( 'NONE', #24375, #64239, #748 ) ;
#3659 = VECTOR ( 'NONE', #29771, 1000.000000000000000 ) ;
#3661 = DIRECTION ( 'NONE',  ( 0.000000000000000000, 0.8660254037844432595, 0.4999999999999919509 ) ) ;
#3660 = VECTOR ( 'NONE', #51991, 1000.000000000000000 ) ;
#3662 = EDGE_LOOP ( 'NONE', ( #41472, #31624, #59306, #41796 ) ) ;
#3663 = EDGE_LOOP ( 'NONE', ( #30039, #23208, #71126, #73318 ) ) ;
#3664 = EDGE_CURVE ( 'NONE', #39943, #70504, #14551, .T. ) ;
#3665 = CARTESIAN_POINT ( 'NONE',  ( 10.00000000000000000, 0.000000000000000000, 0.000000000000000000 ) ) ;
#3666 = AXIS2_PLACEMENT_3D ( 'NONE', #36154, #52331, #24505 ) ;
#3667 = CIRCLE ( 'NONE', #45681, 31.99999999999998934 ) ;
#3668 = ADVANCED_FACE ( 'NONE', ( #12596 ), #58456, .T. ) ;
#3669 = CARTESIAN_POINT ( 'NONE',  ( 10.00000000000000000, -36.73666225445845157, -65.58780272294114866 ) ) ;
#3670 = CARTESIAN_POINT ( 'NONE',  ( -92.35000000000003695, 89.99999999755290503, 75.15687493081163950 ) ) ;
#3671 = CARTESIAN_POINT ( 'NONE',  ( -97.30629616937495996, -209.9999999999999716, 84.08656250086716000 ) ) ;
#3672 = VERTEX_POINT ( 'NONE', #7338 ) ;
#3673 = DIRECTION ( 'NONE',  ( -1.000000000000000000, -0.000000000000000000, -0.000000000000000000 ) ) ;
#3674 = ORIENTED_EDGE ( 'NONE', *, *, #6333, .T. ) ;
#3675 = EDGE_CURVE ( 'NONE', #56198, #49339, #56591, .T. ) ;
#3676 = DIRECTION ( 'NONE',  ( 0.000000000000000000, -0.9510565162951544194, 0.3090169943749450088 ) ) ;
#3677 = DIRECTION ( 'NONE',  ( -0.000000000000000000, -0.000000000000000000, -1.000000000000000000 ) ) ;
#3678 = CARTESIAN_POINT ( 'NONE',  ( 0.000000000000000000, 0.000000000000000000, 0.000000000000000000 ) ) ;
#3679 = CARTESIAN_POINT ( 'NONE',  ( 97.30629616937498838, 91.33154071421968467, 77.31322916753380525 ) ) ;
#3680 = CARTESIAN_POINT ( 'NONE',  ( 11.99999999999999822, 0.000000000000000000, 0.000000000000000000 ) ) ;
#3681 = DIRECTION ( 'NONE',  ( -1.000000000000000000, 0.000000000000000000, 0.000000000000000000 ) ) ;
#3682 = CARTESIAN_POINT ( 'NONE',  ( -2.499999999999970690, 73.00000000000001421, -204.9999999999999716 ) ) ;
#3683 = CARTESIAN_POINT ( 'NONE',  ( 94.99999999999998579, 90.00000000000002842, 90.00000000000000000 ) ) ;
#3684 = CARTESIAN_POINT ( 'NONE',  ( -23.42219527698293646, -121.9106984081423803, -2.500000000000000000 ) ) ;
#3685 = DIRECTION ( 'NONE',  ( -1.000000000000000000, 0.000000000000000000, -0.000000000000000000 ) ) ;
#3686 = EDGE_CURVE ( 'NONE', #12875, #7056, #52079, .T. ) ;
#3687 = CYLINDRICAL_SURFACE ( 'NONE', #44428, 42.00000000000000000 ) ;
#3688 = DIRECTION ( 'NONE',  ( 0.000000000000000000, 0.5000000000000009992, 0.8660254037844380415 ) ) ;
#3689 = ORIENTED_EDGE ( 'NONE', *, *, #67565, .T. ) ;
#3690 = CARTESIAN_POINT ( 'NONE',  ( -92.69370383062505425, 91.33154071421968467, 83.02822916753379445 ) ) ;
#3691 = CIRCLE ( 'NONE', #45707, 31.99999999999998579 ) ;
#3692 = CARTESIAN_POINT ( 'NONE',  ( 12.00000000000000000, -20.55727247249725664, 16.78983467731313084 ) ) ;
#3693 = VECTOR ( 'NONE', #45817, 1000.000000000000114 ) ;
#3695 = EDGE_CURVE ( 'NONE', #35038, #69246, #13220, .T. ) ;
#3694 = CYLINDRICAL_SURFACE ( 'NONE', #11424, 31.99999999999998579 ) ;
#3696 = EDGE_CURVE ( 'NONE', #27913, #12388, #53560, .T. ) ;
#3697 = VERTEX_POINT ( 'NONE', #71950 ) ;
#3698 = LINE ( 'NONE', #32605, #43884 ) ;
#3699 = EDGE_CURVE ( 'NONE', #63343, #24857, #63791, .T. ) ;
#3700 = DIRECTION ( 'NONE',  ( -1.000000000000000000, 0.000000000000000000, 0.000000000000000000 ) ) ;
#3701 = FACE_OUTER_BOUND ( 'NONE', #71447, .T. ) ;
#3702 = CIRCLE ( 'NONE', #34924, 42.00000000000000000 ) ;
#3703 = CIRCLE ( 'NONE', #13285, 31.99999999999999289 ) ;
#3704 = FACE_OUTER_BOUND ( 'NONE', #37853, .T. ) ;
#3705 = CARTESIAN_POINT ( 'NONE',  ( 96.15314808468748708, -208.0026889286704943, 77.52489583420047836 ) ) ;
#3706 = CIRCLE ( 'NONE', #13286, 37.49900000000000233 ) ;
#3707 = EDGE_LOOP ( 'NONE', ( #55650, #35318, #18488, #33643 ) ) ;
#3708 = VECTOR ( 'NONE', #36218, 1000.000000000000000 ) ;
#3710 = ORIENTED_EDGE ( 'NONE', *, *, #37785, .T. ) ;
#3709 =( BOUNDED_CURVE ( )  B_SPLINE_CURVE ( 2, ( #41441, #19244, #12856, #52347, #895, #42196, #41086 ),
 .UNSPECIFIED., .F., .F. ) 
 B_SPLINE_CURVE_WITH_KNOTS ( ( 3, 2, 2, 3 ),
 ( 0.8749999999999997780, 0.8819444444444441977, 0.8888888888888886175, 0.8958333333333331483 ),
 .UNSPECIFIED. ) 
 CURVE ( )  GEOMETRIC_REPRESENTATION_ITEM ( )  RATIONAL_B_SPLINE_CURVE ( ( 1.000000000000004219, 0.8660254037844343777, 1.000000000000000000, 0.8660254037844387076, 1.000000000000000000, 0.8660254037844430375, 0.9999999999999956701 ) ) 
 REPRESENTATION_ITEM ( '' )  );
#3711 = PLANE ( 'NONE',  #34380 ) ;
#3712 = DIRECTION ( 'NONE',  ( 0.000000000000000000, 0.000000000000000000, 1.000000000000000000 ) ) ;
#3713 = DIRECTION ( 'NONE',  ( -1.000000000000000000, 0.000000000000000000, 0.000000000000000000 ) ) ;
#3714 = CYLINDRICAL_SURFACE ( 'NONE', #5094, 77.49899999999999523 ) ;
#3715 = CARTESIAN_POINT ( 'NONE',  ( 96.15314808468750130, -211.9973110713294489, 75.40822916753381833 ) ) ;
#3716 = ORIENTED_EDGE ( 'NONE', *, *, #32088, .F. ) ;
#3717 = CARTESIAN_POINT ( 'NONE',  ( -92.34999999999999432, -209.9999999999999716, 87.77749999999998920 ) ) ;
#3718 = EDGE_LOOP ( 'NONE', ( #6494, #39883, #7441, #3218 ) ) ;
#3719 = ORIENTED_EDGE ( 'NONE', *, *, #48491, .F. ) ;
#3720 = CARTESIAN_POINT ( 'NONE',  ( 11.99999999999999822, -65.64334221924937651, 41.19522573413711797 ) ) ;
#3721 = CARTESIAN_POINT ( 'NONE',  ( 10.00000000000000000, -6.903761155838323837, 77.19088730480521576 ) ) ;
#3722 = EDGE_LOOP ( 'NONE', ( #73607, #73304, #12847, #40772 ) ) ;
#3723 = DIRECTION ( 'NONE',  ( 0.000000000000000000, -0.9876883405951393247, 0.1564344650402207104 ) ) ;
#3724 = CARTESIAN_POINT ( 'NONE',  ( 97.64999999999997726, -211.5299782133524502, 80.81895833506764859 ) ) ;
#3725 = CARTESIAN_POINT ( 'NONE',  ( 92.34999999999999432, 90.00000000000002842, 86.82500000000000284 ) ) ;
#3726 = VERTEX_POINT ( 'NONE', #43778 ) ;
#3727 = DIRECTION ( 'NONE',  ( 0.000000000000000000, 0.5877852522924684742, 0.8090169943749506709 ) ) ;
#3728 = VERTEX_POINT ( 'NONE', #14813 ) ;
#3729 = DIRECTION ( 'NONE',  ( -1.000000000000000000, 0.000000000000000000, -0.000000000000000000 ) ) ;
#3730 = CARTESIAN_POINT ( 'NONE',  ( -97.30629616937501680, 88.66845928578038638, 84.13947916753383538 ) ) ;
#3731 = CARTESIAN_POINT ( 'NONE',  ( 93.84685191531248449, 91.99731107132950569, 83.18697916753382060 ) ) ;
#3732 = ORIENTED_EDGE ( 'NONE', *, *, #10251, .T. ) ;
#3733 = EDGE_CURVE ( 'NONE', #71136, #42455, #6009, .T. ) ;
#3734 = CIRCLE ( 'NONE', #36122, 31.99999999999998934 ) ;
#3735 = CIRCLE ( 'NONE', #48154, 32.50000000000000000 ) ;
#3736 = FACE_OUTER_BOUND ( 'NONE', #44081, .T. ) ;
#3737 = VERTEX_POINT ( 'NONE', #60694 ) ;
#3738 = DIRECTION ( 'NONE',  ( 0.000000000000000000, 0.000000000000000000, 1.000000000000000000 ) ) ;
#3739 = AXIS2_PLACEMENT_3D ( 'NONE', #53575, #25001, #63769 ) ;
#3740 = ORIENTED_EDGE ( 'NONE', *, *, #40999, .T. ) ;
#3741 = ORIENTED_EDGE ( 'NONE', *, *, #2780, .T. ) ;
#3742 = ADVANCED_FACE ( 'NONE', ( #31358 ), #59577, .F. ) ;
#3743 = DIRECTION ( 'NONE',  ( -1.000000000000000000, 0.000000000000000000, 0.000000000000000000 ) ) ;
#3744 = EDGE_CURVE ( 'NONE', #6114, #3457, #7316, .T. ) ;
#3745 = EDGE_LOOP ( 'NONE', ( #41723, #41040, #62519, #34905 ) ) ;
#3746 = DIRECTION ( 'NONE',  ( -1.000000000000000000, 0.000000000000000000, 0.000000000000000000 ) ) ;
#3747 = CARTESIAN_POINT ( 'NONE',  ( 96.32499999999997442, 92.29496732002878900, 88.59770833506763665 ) ) ;
#3748 = ORIENTED_EDGE ( 'NONE', *, *, #13332, .T. ) ;
#3749 = CARTESIAN_POINT ( 'NONE',  ( 0.000000000000000000, 0.000000000000000000, 0.000000000000000000 ) ) ;
#3750 = CARTESIAN_POINT ( 'NONE',  ( -93.84685191531247028, -211.9973110713294489, 78.42447916753381776 ) ) ;
#3751 = ORIENTED_EDGE ( 'NONE', *, *, #27938, .F. ) ;
#3752 = DIRECTION ( 'NONE',  ( 0.000000000000000000, 0.000000000000000000, -1.000000000000000000 ) ) ;
#3753 = CARTESIAN_POINT ( 'NONE',  ( 10.00000000000000000, 35.53030884539084866, 12.26510123303271982 ) ) ;
#3754 = DIRECTION ( 'NONE',  ( -1.000000000000000000, -0.000000000000000000, -0.000000000000000000 ) ) ;
#3755 = DIRECTION ( 'NONE',  ( -1.000000000000000000, -0.000000000000000000, -0.000000000000000000 ) ) ;
#3756 = AXIS2_PLACEMENT_3D ( 'NONE', #18711, #48399, #64586 ) ;
#3757 = ADVANCED_FACE ( 'NONE', ( #25365 ), #8809, .F. ) ;
#3758 = CARTESIAN_POINT ( 'NONE',  ( 11.99999999999999822, 0.000000000000000000, 0.000000000000000000 ) ) ;
#3759 = AXIS2_PLACEMENT_3D ( 'NONE', #73157, #68280, #22036 ) ;
#3760 = AXIS2_PLACEMENT_3D ( 'NONE', #41274, #46179, #1096 ) ;
#3761 = CARTESIAN_POINT ( 'NONE',  ( -96.32500000000001705, 87.70503267997129626, 89.47083333333333144 ) ) ;
#3762 = CARTESIAN_POINT ( 'NONE',  ( 97.30629616937498838, 88.66845928578035796, 87.36739583420047950 ) ) ;
#3763 = DIRECTION ( 'NONE',  ( 0.000000000000000000, 0.000000000000000000, 1.000000000000000000 ) ) ;
#3764 = VECTOR ( 'NONE', #14383, 1000.000000000000114 ) ;
#3765 = CARTESIAN_POINT ( 'NONE',  ( 0.000000000000000000, -31.46837873495025306, 68.27212725128265447 ) ) ;
#3766 = CARTESIAN_POINT ( 'NONE',  ( -93.67500000000003979, 87.70503267997129626, 87.03666666666666174 ) ) ;
#3767 = CARTESIAN_POINT ( 'NONE',  ( 15.00000000000000000, -0.9646360437375368635, -23.52805723605589705 ) ) ;
#3768 = DIRECTION ( 'NONE',  ( 0.000000000000000000, 0.000000000000000000, 1.000000000000000000 ) ) ;
#3769 = CARTESIAN_POINT ( 'NONE',  ( -97.64999999998390479, 89.99999393654049129, 88.17456390440148084 ) ) ;
#3770 = EDGE_CURVE ( 'NONE', #3354, #73774, #12137, .T. ) ;
#3771 = CARTESIAN_POINT ( 'NONE',  ( 0.000000000000000000, 75.54627589209944460, 17.28742895386110945 ) ) ;
#3772 = ADVANCED_FACE ( 'NONE', ( #2098 ), #26463, .T. ) ;
#3773 = CARTESIAN_POINT ( 'NONE',  ( 10.00000000000000000, 35.38097989696512968, 12.42422080174651100 ) ) ;
#3774 = CYLINDRICAL_SURFACE ( 'NONE', #65297, 37.49900000000000233 ) ;
#3775 = CARTESIAN_POINT ( 'NONE',  ( 10.00000000000000000, -6.555932627142143865, -37.01155633439065440 ) ) ;
#3776 = DIRECTION ( 'NONE',  ( 1.000000000000000000, 1.427937372958405461E-15, 7.962523111839130290E-16 ) ) ;
#3777 = CARTESIAN_POINT ( 'NONE',  ( -92.34999999999999432, -209.9999999999999716, 89.04749999999999943 ) ) ;
#3778 = CARTESIAN_POINT ( 'NONE',  ( 35.50000000000000711, -120.0000000000000000, 2.500000000000000000 ) ) ;
#3779 = EDGE_CURVE ( 'NONE', #18854, #33851, #58952, .T. ) ;
#3780 = PRODUCT ( 'slow gear_ISO - Spur gear 2M 80T 20PA 12FW ---S80A75H50L38.0N', 'slow gear_ISO - Spur gear 2M 80T 20PA 12FW ---S80A75H50L38.0N', '', ( #46341 ) ) ;
#3781 = ADVANCED_FACE ( 'NONE', ( #65225 ), #65592, .T. ) ;
#3782 = CARTESIAN_POINT ( 'NONE',  ( 11.99999999999999822, 24.73286445877808148, -73.44644590900034586 ) ) ;
#3783 = LINE ( 'NONE', #37976, #49067 ) ;
#3784 = DIRECTION ( 'NONE',  ( 7.962523111839282146E-16, -1.065814103640130873E-14, -1.000000000000000000 ) ) ;
#3785 = CARTESIAN_POINT ( 'NONE',  ( -3.000000000000000000, 0.000000000000000000, 0.000000000000000000 ) ) ;
#3786 = MECHANICAL_DESIGN_GEOMETRIC_PRESENTATION_REPRESENTATION (  '', ( #37375 ), #63789 ) ;
#3787 = CIRCLE ( 'NONE', #48209, 82.00000000000000000 ) ;
#3788 = VECTOR ( 'NONE', #44721, 1000.000000000000000 ) ;
#3789 = AXIS2_PLACEMENT_3D ( 'NONE', #20001, #65893, #54961 ) ;
#3790 = EDGE_LOOP ( 'NONE', ( #65870, #31513, #9705, #21632 ) ) ;
#3791 = VERTEX_POINT ( 'NONE', #54310 ) ;
#3792 = DIRECTION ( 'NONE',  ( -1.000000000000000000, 0.000000000000000000, -0.000000000000000000 ) ) ;
#3793 = DIRECTION ( 'NONE',  ( -1.000000000000000000, 0.000000000000000000, 0.000000000000000000 ) ) ;
#3794 = EDGE_LOOP ( 'NONE', ( #37080, #23623, #12025, #62762 ) ) ;
#3795 =( BOUNDED_CURVE ( )  B_SPLINE_CURVE ( 2, ( #4462, #21725, #44681, #39028, #46899, #63823, #70167, #1443, #17572 ),
 .UNSPECIFIED., .F., .F. ) 
 B_SPLINE_CURVE_WITH_KNOTS ( ( 3, 2, 2, 2, 3 ),
 ( 0.7196881748034549275, 0.7267438507108832102, 0.7337996162517648191, 0.7408553817926463170, 0.7408554641864679713 ),
 .UNSPECIFIED. ) 
 CURVE ( )  GEOMETRIC_REPRESENTATION_ITEM ( )  RATIONAL_B_SPLINE_CURVE ( ( 0.9999965961303334261, 0.8660271057408929218, 1.000000000000000000, 0.8660254037844387076, 1.000000000000000000, 0.8660254037844387076, 1.000000000000000000, 0.9999984355093834987, 0.9999968710553057694 ) ) 
 REPRESENTATION_ITEM ( '' )  );
#3796 = CARTESIAN_POINT ( 'NONE',  ( 92.69370383062501162, -211.3315407142195852, 81.44072916753380298 ) ) ;
#3797 = CARTESIAN_POINT ( 'NONE',  ( 95.00000000000000000, -212.6630814284392557, 83.61031250086715261 ) ) ;
#3798 = ORIENTED_EDGE ( 'NONE', *, *, #38873, .F. ) ;
#3799 = CARTESIAN_POINT ( 'NONE',  ( 97.30629616937498838, -211.3315407142195852, 84.98614583420047097 ) ) ;
#3800 = ORIENTED_EDGE ( 'NONE', *, *, #45855, .T. ) ;
#3801 = FACE_OUTER_BOUND ( 'NONE', #55805, .T. ) ;
#3802 = ORIENTED_EDGE ( 'NONE', *, *, #30312, .F. ) ;
#3803 = CIRCLE ( 'NONE', #62628, 77.49899999999999523 ) ;
#3804 = CARTESIAN_POINT ( 'NONE',  ( -93.84685191531254134, 91.99731107132950569, 76.88989583420048746 ) ) ;
#3805 = VECTOR ( 'NONE', #34128, 1000.000000000000000 ) ;
#3806 = ORIENTED_EDGE ( 'NONE', *, *, #39083, .F. ) ;
#3807 = ORIENTED_EDGE ( 'NONE', *, *, #11540, .T. ) ;
#3808 = DIRECTION ( 'NONE',  ( 0.000000000000000000, 0.000000000000000000, -1.000000000000000000 ) ) ;
#3809 = AXIS2_PLACEMENT_3D ( 'NONE', #14565, #38996, #10411 ) ;
#3810 = VERTEX_POINT ( 'NONE', #20464 ) ;
#3811 = FACE_OUTER_BOUND ( 'NONE', #61527, .T. ) ;
#3812 = DIRECTION ( 'NONE',  ( 0.000000000000000000, 0.000000000000000000, 1.000000000000000000 ) ) ;
#3813 = ORIENTED_EDGE ( 'NONE', *, *, #56366, .T. ) ;
#3814 = CARTESIAN_POINT ( 'NONE',  ( 11.99999999999999822, 0.000000000000000000, 0.000000000000000000 ) ) ;
#3815 = ORIENTED_EDGE ( 'NONE', *, *, #24842, .F. ) ;
#3816 = CARTESIAN_POINT ( 'NONE',  ( 0.000000000000000000, 3.894527615417891830, 81.90746397400390322 ) ) ;
#3817 = EDGE_LOOP ( 'NONE', ( #39411, #48534, #33782, #25634 ) ) ;
#3818 = EDGE_CURVE ( 'NONE', #65052, #23772, #2835, .T. ) ;
#3819 = ORIENTED_EDGE ( 'NONE', *, *, #29963, .F. ) ;
#3820 = ORIENTED_EDGE ( 'NONE', *, *, #58000, .F. ) ;
#3821 = CARTESIAN_POINT ( 'NONE',  ( 92.69370383062501162, -208.6684592857803011, 74.98489583420048632 ) ) ;
#3822 = FACE_OUTER_BOUND ( 'NONE', #9408, .T. ) ;
#3824 = EDGE_CURVE ( 'NONE', #44376, #71645, #71578, .T. ) ;
#3823 = ORIENTED_EDGE ( 'NONE', *, *, #1137, .F. ) ;
#3825 = ORIENTED_EDGE ( 'NONE', *, *, #61696, .F. ) ;
#3826 = ORIENTED_EDGE ( 'NONE', *, *, #48864, .F. ) ;
#3827 = DIRECTION ( 'NONE',  ( 0.1850432970638656860, -0.9827303690289285187, 0.000000000000000000 ) ) ;
#3828 = EDGE_CURVE ( 'NONE', #25432, #11811, #30985, .T. ) ;
#3829 = CARTESIAN_POINT ( 'NONE',  ( -18.24502636017238899, -100.7225776329765665, 5.500000000000000000 ) ) ;
#3830 = CARTESIAN_POINT ( 'NONE',  ( -96.15314808468752972, 91.99731107132950569, 76.36072916753381890 ) ) ;
#3831 = ORIENTED_EDGE ( 'NONE', *, *, #73557, .F. ) ;
#3832 = CARTESIAN_POINT ( 'NONE',  ( 97.30629616937498838, 90.00000000000002842, 75.99031250086714806 ) ) ;
#3833 = ORIENTED_EDGE ( 'NONE', *, *, #21695, .T. ) ;
#3834 = CARTESIAN_POINT ( 'NONE',  ( 10.00000000000000000, 0.000000000000000000, 0.000000000000000000 ) ) ;
#3835 = CARTESIAN_POINT ( 'NONE',  ( 0.000000000000000000, 22.48208911017500355, 35.47612816024530957 ) ) ;
#3836 = CARTESIAN_POINT ( 'NONE',  ( 25.81725066941077529, -113.8380548628854854, 5.500000000000000000 ) ) ;
#3837 = LINE ( 'NONE', #66964, #44023 ) ;
#3838 = DIRECTION ( 'NONE',  ( 0.000000000000000000, -0.2334453638558921240, -0.9723699203976797767 ) ) ;
#3839 = CARTESIAN_POINT ( 'NONE',  ( -96.15314808468745866, -211.9973110713294489, 80.22364583420046813 ) ) ;
#3840 = ADVANCED_FACE ( 'NONE', ( #20076 ), #43030, .T. ) ;
#3841 = CIRCLE ( 'NONE', #45866, 42.00000000000000000 ) ;
#3842 = CARTESIAN_POINT ( 'NONE',  ( 97.64999999999999147, -209.9999999999999716, 90.00000000000000000 ) ) ;
#3843 = LINE ( 'NONE', #60249, #15107 ) ;
#3844 = CARTESIAN_POINT ( 'NONE',  ( 6.000000000000000000, -81.96053171279901051, -2.543863470249253300 ) ) ;
#3845 = ORIENTED_EDGE ( 'NONE', *, *, #52508, .T. ) ;
#3846 = VERTEX_POINT ( 'NONE', #60331 ) ;
#3847 = CARTESIAN_POINT ( 'NONE',  ( -15.50000000000000000, 1.898202538678397557E-15, -4.400000000000001243 ) ) ;
#3848 = CARTESIAN_POINT ( 'NONE',  ( 10.00000000000000000, -75.11725578898470701, 2.956366410620372864 ) ) ;
#3849 = DIRECTION ( 'NONE',  ( 0.000000000000000000, -1.000000000000000000, 0.000000000000000000 ) ) ;
#3850 = CIRCLE ( 'NONE', #5088, 82.00000000000000000 ) ;
#3851 = CARTESIAN_POINT ( 'NONE',  ( -96.15314808468751551, 88.00268892867056536, 82.76364583420047438 ) ) ;
#3852 = DIRECTION ( 'NONE',  ( -1.000000000000000000, -0.000000000000000000, -0.000000000000000000 ) ) ;
#3853 = FACE_OUTER_BOUND ( 'NONE', #12917, .T. ) ;
#3854 = ADVANCED_FACE ( 'NONE', ( #5042 ), #21559, .T. ) ;
#3855 = AXIS2_PLACEMENT_3D ( 'NONE', #66042, #14514, #8882 ) ;
#3856 = VERTEX_POINT ( 'NONE', #50117 ) ;
#3857 = EDGE_CURVE ( 'NONE', #62068, #11372, #21743, .T. ) ;
#3858 = CARTESIAN_POINT ( 'NONE',  ( 11.99999999999999822, 0.000000000000000000, 0.000000000000000000 ) ) ;
#3859 = CIRCLE ( 'NONE', #68690, 77.49899999999999523 ) ;
#3860 = EDGE_CURVE ( 'NONE', #15417, #51502, #68564, .T. ) ;
#3862 = EDGE_CURVE ( 'NONE', #60009, #42672, #36123, .T. ) ;
#3861 = DIRECTION ( 'NONE',  ( 0.000000000000000000, 0.000000000000000000, 1.000000000000000000 ) ) ;
#3863 = CARTESIAN_POINT ( 'NONE',  ( -92.34999999999999432, -209.9999999999999716, 90.00000000000000000 ) ) ;
#3864 = CIRCLE ( 'NONE', #13445, 42.00000000000000000 ) ;
#3865 = DIRECTION ( 'NONE',  ( 0.000000000000000000, 0.000000000000000000, -1.000000000000000000 ) ) ;
#3866 = CARTESIAN_POINT ( 'NONE',  ( -92.35003071824209542, -208.4700040514621264, 79.01979289519869099 ) ) ;
#3867 = CARTESIAN_POINT ( 'NONE',  ( -94.99999999999997158, -207.3369185715606307, 83.29281250086717137 ) ) ;
#3868 = CIRCLE ( 'NONE', #26644, 77.49899999999999523 ) ;
#3869 = FACE_OUTER_BOUND ( 'NONE', #27647, .T. ) ;
#3870 = EDGE_CURVE ( 'NONE', #55006, #43075, #3735, .T. ) ;
#3871 = ORIENTED_EDGE ( 'NONE', *, *, #25873, .T. ) ;
#3872 = DIRECTION ( 'NONE',  ( 0.000000000000000000, 0.000000000000000000, 1.000000000000000000 ) ) ;
#3873 = DIRECTION ( 'NONE',  ( -1.000000000000000000, -0.000000000000000000, 0.000000000000000000 ) ) ;
#3874 = PLANE ( 'NONE',  #22596 ) ;
#3875 = ORIENTED_EDGE ( 'NONE', *, *, #451, .F. ) ;
#3876 = ADVANCED_FACE ( 'NONE', ( #55409 ), #15928, .T. ) ;
#3877 = CARTESIAN_POINT ( 'NONE',  ( 0.000000000000000000, 10.96151621346540317, -35.95386929396244113 ) ) ;
#3878 = CARTESIAN_POINT ( 'NONE',  ( 11.99999999999999822, -51.03279382321048985, -55.19960302592120627 ) ) ;
#3879 = FACE_OUTER_BOUND ( 'NONE', #30347, .T. ) ;
#3880 = DIRECTION ( 'NONE',  ( 0.000000000000000000, -0.9238795325112822976, -0.3826834323651006065 ) ) ;
#3881 = EDGE_LOOP ( 'NONE', ( #65203, #38921, #68388, #512 ) ) ;
#3882 = DIRECTION ( 'NONE',  ( 0.000000000000000000, 1.000000000000000000, 0.000000000000000000 ) ) ;
#3883 = ORIENTED_EDGE ( 'NONE', *, *, #7508, .F. ) ;
#3884 = CARTESIAN_POINT ( 'NONE',  ( -92.35000000000012221, 90.00000071509187194, 85.31687502647973531 ) ) ;
#3885 = DIRECTION ( 'NONE',  ( 0.000000000000000000, 0.000000000000000000, 1.000000000000000000 ) ) ;
#3886 = EDGE_LOOP ( 'NONE', ( #8169, #58773, #8952, #62257 ) ) ;
#3887 = CARTESIAN_POINT ( 'NONE',  ( -10.43921258969510824, -98.89258801967538659, 5.500000000000000000 ) ) ;
#3888 = COLOUR_RGB ( '', 0.08235294, 0.09019608, 0.10196078) ;
#3889 = CIRCLE ( 'NONE', #45917, 82.00000000000000000 ) ;
#3890 = ORIENTED_EDGE ( 'NONE', *, *, #10454, .F. ) ;
#3891 = DIRECTION ( 'NONE',  ( -1.000000000000000000, -0.000000000000000000, 0.000000000000000000 ) ) ;
#3892 = AXIS2_PLACEMENT_3D ( 'NONE', #61637, #9380, #39079 ) ;
#3893 = ORIENTED_EDGE ( 'NONE', *, *, #2331, .T. ) ;
#3894 = ORIENTED_EDGE ( 'NONE', *, *, #59094, .F. ) ;
#3895 = VERTEX_POINT ( 'NONE', #16674 ) ;
#3896 = ORIENTED_EDGE ( 'NONE', *, *, #65370, .F. ) ;
#3897 = LINE ( 'NONE', #26799, #73147 ) ;
#3898 = VECTOR ( 'NONE', #1746, 1000.000000000000000 ) ;
#3899 = EDGE_LOOP ( 'NONE', ( #61490, #28946, #72561, #15672 ) ) ;
#3900 = AXIS2_PLACEMENT_3D ( 'NONE', #42745, #48748, #2192 ) ;
#3901 = ORIENTED_EDGE ( 'NONE', *, *, #28803, .F. ) ;
#3902 = CARTESIAN_POINT ( 'NONE',  ( 92.69370383062498320, 91.33154071421968467, 76.41364583420049428 ) ) ;
#3903 = CARTESIAN_POINT ( 'NONE',  ( 96.32499999999998863, -212.2949673200287179, 89.02104166840096866 ) ) ;
#3904 = CARTESIAN_POINT ( 'NONE',  ( 10.00000000000000000, 0.000000000000000000, 0.000000000000000000 ) ) ;
#3905 = VERTEX_POINT ( 'NONE', #51245 ) ;
#3906 = VERTEX_POINT ( 'NONE', #61433 ) ;
#3907 = EDGE_CURVE ( 'NONE', #72957, #57222, #31340, .T. ) ;
#3908 = EDGE_LOOP ( 'NONE', ( #42750, #9621 ) ) ;
#3909 = CARTESIAN_POINT ( 'NONE',  ( 92.69370383062498320, 90.00000000000002842, 89.64281250086713726 ) ) ;
#3910 = VECTOR ( 'NONE', #47247, 1000.000000000000000 ) ;
#3911 = EDGE_LOOP ( 'NONE', ( #5013, #19866, #17811, #55294 ) ) ;
#3912 = CARTESIAN_POINT ( 'NONE',  ( 93.84685191531251292, -211.9973110713294489, 85.30364583420046642 ) ) ;
#3913 = AXIS2_PLACEMENT_3D ( 'NONE', #26014, #54957, #50429 ) ;
#3914 = DIRECTION ( 'NONE',  ( 1.000000000000000000, 0.000000000000000000, -5.551115123125782702E-17 ) ) ;
#3915 = DIRECTION ( 'NONE',  ( -1.000000000000000000, -0.000000000000000000, -0.000000000000000000 ) ) ;
#3916 = ADVANCED_FACE ( 'NONE', ( #3932 ), #26829, .T. ) ;
#3917 = CYLINDRICAL_SURFACE ( 'NONE', #6593, 2.649999999999985700 ) ;
#3918 = DIRECTION ( 'NONE',  ( -0.000000000000000000, -0.000000000000000000, 1.000000000000000000 ) ) ;
#3919 = DIRECTION ( 'NONE',  ( 0.000000000000000000, 0.000000000000000000, 1.000000000000000000 ) ) ;
#3920 = FACE_OUTER_BOUND ( 'NONE', #21453, .T. ) ;
#3921 = EDGE_CURVE ( 'NONE', #19207, #32694, #61362, .T. ) ;
#3922 = DIRECTION ( 'NONE',  ( -1.000000000000000000, 0.000000000000000000, -0.000000000000000000 ) ) ;
#3923 = ADVANCED_FACE ( 'NONE', ( #5415 ), #50876, .F. ) ;
#3924 = CARTESIAN_POINT ( 'NONE',  ( -93.67499999999998295, -212.2949673200287179, 76.32104166840096582 ) ) ;
#3925 = CARTESIAN_POINT ( 'NONE',  ( 0.000000000000000000, -120.0000000000000000, -2.500000000000000000 ) ) ;
#3926 = ORIENTED_EDGE ( 'NONE', *, *, #20561, .F. ) ;
#3927 = UNCERTAINTY_MEASURE_WITH_UNIT (LENGTH_MEASURE( 1.000000000000000082E-05 ), #1311, 'distance_accuracy_value', 'NONE');
#3929 = CARTESIAN_POINT ( 'NONE',  ( -95.00000000000002842, 92.66308142843932671, 87.57906250086713840 ) ) ;
#3928 = CARTESIAN_POINT ( 'NONE',  ( 96.15314808468748708, 91.99731107132950569, 88.79614583420047325 ) ) ;
#3930 = ORIENTED_EDGE ( 'NONE', *, *, #18930, .T. ) ;
#3931 = DIRECTION ( 'NONE',  ( -1.000000000000000000, 0.000000000000000000, 0.000000000000000000 ) ) ;
#3932 = FACE_OUTER_BOUND ( 'NONE', #23383, .T. ) ;
#3933 = CARTESIAN_POINT ( 'NONE',  ( 10.00000000000000000, 27.05870788708267582, -26.08949754952995903 ) ) ;
#3934 = DIRECTION ( 'NONE',  ( -1.000000000000000000, -0.000000000000000000, 0.000000000000000000 ) ) ;
#3935 = CARTESIAN_POINT ( 'NONE',  ( 10.00000000000000000, 66.50666863322055633, -39.78640506895536078 ) ) ;
#3936 = LINE ( 'NONE', #31362, #55736 ) ;
#3937 = LINE ( 'NONE', #45262, #14568 ) ;
#3938 = CARTESIAN_POINT ( 'NONE',  ( -18.12185313557660038, -104.9634299478706794, 5.500000000000000000 ) ) ;
#3939 = ORIENTED_EDGE ( 'NONE', *, *, #73833, .T. ) ;
#3940 = ADVANCED_FACE ( 'NONE', ( #33207 ), #45640, .F. ) ;
#3941 = ORIENTED_EDGE ( 'NONE', *, *, #25151, .F. ) ;
#3942 = EDGE_CURVE ( 'NONE', #37865, #23298, #67465, .T. ) ;
#3943 = CARTESIAN_POINT ( 'NONE',  ( -93.67500000000003979, 92.29496732002878900, 82.80333333333332746 ) ) ;
#3944 = CARTESIAN_POINT ( 'NONE',  ( 10.00000000000000000, 5.202137450156389953, 37.22597642581160216 ) ) ;
#3945 = CARTESIAN_POINT ( 'NONE',  ( 0.000000000000000000, -20.40083707022829174, -72.35432306680507963 ) ) ;
#3946 = DIRECTION ( 'NONE',  ( -0.000000000000000000, -0.000000000000000000, -1.000000000000000000 ) ) ;
#3947 = FACE_OUTER_BOUND ( 'NONE', #45265, .T. ) ;
#3948 = DIRECTION ( 'NONE',  ( 0.000000000000000000, 0.4539904997395477482, -0.8910065241883674547 ) ) ;
#3949 = DIRECTION ( 'NONE',  ( 0.000000000000000000, -0.8910065241883627918, -0.4539904997395568520 ) ) ;
#3950 = ORIENTED_EDGE ( 'NONE', *, *, #64499, .F. ) ;
#3951 = CARTESIAN_POINT ( 'NONE',  ( -96.15314808468752972, 91.99731107132950569, 80.64697916753381435 ) ) ;
#3952 = MECHANICAL_DESIGN_GEOMETRIC_PRESENTATION_REPRESENTATION (  '', ( #71150 ), #383 ) ;
#3953 = LINE ( 'NONE', #26854, #13909 ) ;
#3954 = EDGE_CURVE ( 'NONE', #63285, #12380, #57771, .T. ) ;
#3955 = EDGE_CURVE ( 'NONE', #73325, #19590, #61054, .T. ) ;
#3956 = FACE_BOUND ( 'NONE', #21147, .T. ) ;
#3957 = AXIS2_PLACEMENT_3D ( 'NONE', #28761, #17850, #69726 ) ;
#3958 = DIRECTION ( 'NONE',  ( -0.000000000000000000, -0.000000000000000000, 1.000000000000000000 ) ) ;
#3959 = DIRECTION ( 'NONE',  ( 0.000000000000000000, -0.9238795325112906243, 0.3826834323650805114 ) ) ;
#3960 = CARTESIAN_POINT ( 'NONE',  ( 5.000000000000002665, 8.966570791700698706, 81.50828551894228724 ) ) ;
#3961 = DIRECTION ( 'NONE',  ( -1.000000000000000000, -0.000000000000000000, -0.000000000000000000 ) ) ;
#3962 = CARTESIAN_POINT ( 'NONE',  ( 5.999999999999999112, -60.67117009219097667, -55.16347631943106933 ) ) ;
#3963 = CIRCLE ( 'NONE', #72358, 82.00000000000000000 ) ;
#3964 = CARTESIAN_POINT ( 'NONE',  ( 92.69370383062498320, 90.00000000000002842, 80.27656250086714351 ) ) ;
#3965 = CARTESIAN_POINT ( 'NONE',  ( -93.84685191531247028, -211.9973110713294489, 82.39322916753381776 ) ) ;
#3966 = CARTESIAN_POINT ( 'NONE',  ( -3.759344165985237129, 0.000000000000000000, -19.05560546998412974 ) ) ;
#3967 = ORIENTED_EDGE ( 'NONE', *, *, #55706, .T. ) ;
#3968 = CARTESIAN_POINT ( 'NONE',  ( 97.64999999999999147, -210.0000000207152198, 80.87187500099602744 ) ) ;
#3969 = CARTESIAN_POINT ( 'NONE',  ( -97.64999999999994884, -208.4700217866474645, 78.51708333333334622 ) ) ;
#3970 = CYLINDRICAL_SURFACE ( 'NONE', #59384, 16.00000000000000000 ) ;
#3971 = VECTOR ( 'NONE', #31374, 1000.000000000000000 ) ;
#3972 = AXIS2_PLACEMENT_3D ( 'NONE', #23270, #45845, #62011 ) ;
#3973 = CARTESIAN_POINT ( 'NONE',  ( -97.30629616937501680, 88.66845928578038638, 77.78947916753381264 ) ) ;
#3974 = CARTESIAN_POINT ( 'NONE',  ( 97.30629616937498838, -209.9999999999999716, 83.61031250086713840 ) ) ;
#3975 = VERTEX_POINT ( 'NONE', #39612 ) ;
#3976 = DIRECTION ( 'NONE',  ( -1.000000000000000000, 0.000000000000000000, 0.000000000000000000 ) ) ;
#3977 = ORIENTED_EDGE ( 'NONE', *, *, #66110, .F. ) ;
#3978 = CYLINDRICAL_SURFACE ( 'NONE', #60827, 42.00000000000000000 ) ;
#3979 = ORIENTED_EDGE ( 'NONE', *, *, #4510, .T. ) ;
#3980 = CARTESIAN_POINT ( 'NONE',  ( -92.35000000000010800, -208.4700217866473793, 83.38541666666667140 ) ) ;
#3981 = EDGE_LOOP ( 'NONE', ( #42997, #28643, #28390, #44014 ) ) ;
#3982 = ORIENTED_EDGE ( 'NONE', *, *, #17730, .F. ) ;
#3983 = DIRECTION ( 'NONE',  ( 0.000000000000000000, -0.5224985647159380298, -0.8526401643540988395 ) ) ;
#3984 = CARTESIAN_POINT ( 'NONE',  ( 95.00000000000000000, -209.9999999999999716, 90.00000000000000000 ) ) ;
#3985 = CARTESIAN_POINT ( 'NONE',  ( 11.99999999999999822, 72.35160999960844208, -20.41045688087747223 ) ) ;
#3986 = CARTESIAN_POINT ( 'NONE',  ( 10.00000000000000000, -73.73191006444561424, -14.66109333815538918 ) ) ;
#3987 = CARTESIAN_POINT ( 'NONE',  ( 96.15314808468748708, 91.99731107132950569, 88.31989583420048007 ) ) ;
#3988 = CARTESIAN_POINT ( 'NONE',  ( -96.32500000000001705, 87.70503267997129626, 83.20020833506764291 ) ) ;
#3989 = CARTESIAN_POINT ( 'NONE',  ( 96.32499999999998863, -212.2949673200287179, 82.59166666666665435 ) ) ;
#3990 = EDGE_CURVE ( 'NONE', #70803, #36870, #41096, .T. ) ;
#3991 = ORIENTED_EDGE ( 'NONE', *, *, #36938, .F. ) ;
#3992 = PRODUCT_DEFINITION_FORMATION_WITH_SPECIFIED_SOURCE ( 'ANY', '', #50605, .NOT_KNOWN. ) ;
#3993 = ORIENTED_EDGE ( 'NONE', *, *, #22530, .T. ) ;
#3994 = EDGE_CURVE ( 'NONE', #63158, #20698, #12504, .T. ) ;
#3995 = ORIENTED_EDGE ( 'NONE', *, *, #69770, .T. ) ;
#3996 = ORIENTED_EDGE ( 'NONE', *, *, #50257, .T. ) ;
#3997 = CARTESIAN_POINT ( 'NONE',  ( 11.99999999999999822, 0.000000000000000000, 0.000000000000000000 ) ) ;
#3998 = CIRCLE ( 'NONE', #27967, 82.00000000000000000 ) ;
#3999 =( NAMED_UNIT ( * ) PLANE_ANGLE_UNIT ( ) SI_UNIT ( $, .RADIAN. ) );
#4000 = LINE ( 'NONE', #39691, #71492 ) ;
#4001 = EDGE_CURVE ( 'NONE', #43677, #19971, #53038, .T. ) ;
#4002 = LINE ( 'NONE', #31798, #68843 ) ;
#4003 = CARTESIAN_POINT ( 'NONE',  ( 97.64999322989702080, -211.5299821220732213, 82.72395806468929891 ) ) ;
#4004 = FACE_OUTER_BOUND ( 'NONE', #70162, .T. ) ;
#4005 = LINE ( 'NONE', #66413, #10388 ) ;
#4007 = ORIENTED_EDGE ( 'NONE', *, *, #55576, .F. ) ;
#4006 = EDGE_CURVE ( 'NONE', #32135, #66160, #3787, .T. ) ;
#4008 = CARTESIAN_POINT ( 'NONE',  ( -97.64999999999994884, -211.5299782133524502, 85.68729166840097378 ) ) ;
#4009 = VERTEX_POINT ( 'NONE', #6150 ) ;
#4010 = DIRECTION ( 'NONE',  ( -1.000000000000000000, -0.000000000000000000, 0.000000000000000000 ) ) ;
#4011 = VERTEX_POINT ( 'NONE', #29057 ) ;
#4012 = CARTESIAN_POINT ( 'NONE',  ( -97.65000000000001990, 91.52997821335253548, 84.31145833506762699 ) ) ;
#4013 = VECTOR ( 'NONE', #72739, 1000.000000000000000 ) ;
#4014 =( BOUNDED_CURVE ( )  B_SPLINE_CURVE ( 2, ( #14802, #64844, #65958, #36624, #54301, #70448, #71570 ),
 .UNSPECIFIED., .F., .F. ) 
 B_SPLINE_CURVE_WITH_KNOTS ( ( 3, 2, 2, 3 ),
 ( 0.7708333333333328152, 0.7777777777777775681, 0.7847222222222222099, 0.7916666666666669627 ),
 .UNSPECIFIED. ) 
 CURVE ( )  GEOMETRIC_REPRESENTATION_ITEM ( )  RATIONAL_B_SPLINE_CURVE ( ( 1.000000000000010658, 0.8660254037844280495, 1.000000000000000000, 0.8660254037844387076, 1.000000000000000000, 0.8660254037844322683, 1.000000000000006439 ) ) 
 REPRESENTATION_ITEM ( '' )  );
#4015 = EDGE_CURVE ( 'NONE', #55000, #14315, #42727, .T. ) ;
#4016 = ORIENTED_EDGE ( 'NONE', *, *, #50828, .T. ) ;
#4017 = CARTESIAN_POINT ( 'NONE',  ( 92.69370383062498320, 91.33154071421968467, 84.66864583420047552 ) ) ;
#4018 = VECTOR ( 'NONE', #69227, 1000.000000000000000 ) ;
#4019 = DIRECTION ( 'NONE',  ( 0.000000000000000000, -0.3826834323650772363, -0.9238795325112919565 ) ) ;
#4020 = CARTESIAN_POINT ( 'NONE',  ( -97.64999999999996305, -209.9999999999999716, 75.39499999999999602 ) ) ;
#4021 = FACE_OUTER_BOUND ( 'NONE', #13527, .T. ) ;
#4023 = AXIS2_PLACEMENT_3D ( 'NONE', #47173, #57720, #70084 ) ;
#4022 = LINE ( 'NONE', #20916, #29433 ) ;
#4024 = DIRECTION ( 'NONE',  ( -1.000000000000000000, 0.000000000000000000, -0.000000000000000000 ) ) ;
#4025 = ORIENTED_EDGE ( 'NONE', *, *, #32418, .T. ) ;
#4026 = CARTESIAN_POINT ( 'NONE',  ( -97.64999999947052345, 90.00003365185393989, 81.18829462297244959 ) ) ;
#4027 = CONICAL_SURFACE ( 'NONE', #46037, 13.71319123027096865, 1.361356816555593596 ) ;
#4028 = CONICAL_SURFACE ( 'NONE', #24450, 2.649999999999999467, 1.029744258676654312 ) ;
#4029 = DIRECTION ( 'NONE',  ( -1.000000000000000000, -0.000000000000000000, -0.000000000000000000 ) ) ;
#4030 = ORIENTED_EDGE ( 'NONE', *, *, #43706, .F. ) ;
#4031 = ORIENTED_EDGE ( 'NONE', *, *, #58982, .F. ) ;
#4032 = EDGE_CURVE ( 'NONE', #66307, #24726, #2626, .T. ) ;
#4033 = ADVANCED_FACE ( 'NONE', ( #64027 ), #24530, .T. ) ;
#4034 = CYLINDRICAL_SURFACE ( 'NONE', #19186, 82.00000000000000000 ) ;
#4035 = CYLINDRICAL_SURFACE ( 'NONE', #45006, 82.00000000000000000 ) ;
#4036 = FACE_OUTER_BOUND ( 'NONE', #4823, .T. ) ;
#4037 = CARTESIAN_POINT ( 'NONE',  ( -97.30629616937495996, -209.9999999999999716, 84.72156250086715090 ) ) ;
#4038 = VERTEX_POINT ( 'NONE', #1284 ) ;
#4039 = DIRECTION ( 'NONE',  ( 0.000000000000000000, 0.000000000000000000, 1.000000000000000000 ) ) ;
#4040 = ORIENTED_EDGE ( 'NONE', *, *, #26910, .F. ) ;
#4041 = DIRECTION ( 'NONE',  ( 0.000000000000000000, 0.000000000000000000, 1.000000000000000000 ) ) ;
#4042 = EDGE_CURVE ( 'NONE', #23530, #42393, #39793, .T. ) ;
#4043 = EDGE_CURVE ( 'NONE', #29886, #68784, #43456, .T. ) ;
#4044 = CARTESIAN_POINT ( 'NONE',  ( 0.000000000000000000, 0.000000000000000000, 0.000000000000000000 ) ) ;
#4045 = CARTESIAN_POINT ( 'NONE',  ( 0.000000000000000000, 59.03342792756328095, -46.54456581323744757 ) ) ;
#4046 = CARTESIAN_POINT ( 'NONE',  ( 92.69370383062498320, 88.66845928578035796, 79.53572916753380184 ) ) ;
#4047 = LINE ( 'NONE', #26942, #70051 ) ;
#4048 = DIRECTION ( 'NONE',  ( -1.000000000000000000, 0.000000000000000000, -0.000000000000000000 ) ) ;
#4049 = CARTESIAN_POINT ( 'NONE',  ( 11.99999999999999822, 0.000000000000000000, 0.000000000000000000 ) ) ;
#4050 = DIRECTION ( 'NONE',  ( 1.000000000000000000, -3.035766082959412415E-16, 0.000000000000000000 ) ) ;
#4051 = CARTESIAN_POINT ( 'NONE',  ( 10.00000000000000000, -16.45098606841102651, -33.79645857604531045 ) ) ;
#4052 = DIRECTION ( 'NONE',  ( 0.000000000000000000, 0.000000000000000000, 1.000000000000000000 ) ) ;
#4053 = ORIENTED_EDGE ( 'NONE', *, *, #60375, .F. ) ;
#4054 = CARTESIAN_POINT ( 'NONE',  ( 0.5480546763151027401, -96.50639159107802811, -2.500000000000000000 ) ) ;
#4055 = CARTESIAN_POINT ( 'NONE',  ( 11.99999999999999822, -63.97538442413463855, 51.29473840253199057 ) ) ;
#4056 = ORIENTED_EDGE ( 'NONE', *, *, #28445, .T. ) ;
#4057 = CARTESIAN_POINT ( 'NONE',  ( -95.00000000000002842, 87.33691857156074434, 84.72156250086713669 ) ) ;
#4058 = DIRECTION ( 'NONE',  ( 1.000000000000000000, -0.000000000000000000, -0.000000000000000000 ) ) ;
#4059 = CIRCLE ( 'NONE', #20834, 82.00000000000000000 ) ;
#4060 = LINE ( 'NONE', #43543, #52267 ) ;
#4061 = VERTEX_POINT ( 'NONE', #34329 ) ;
#4062 = DIRECTION ( 'NONE',  ( -1.000000000000000000, 0.000000000000000000, -0.000000000000000000 ) ) ;
#4064 = CARTESIAN_POINT ( 'NONE',  ( 0.000000000000000000, 60.67117009219135326, 55.16347631943062169 ) ) ;
#4063 = AXIS2_PLACEMENT_3D ( 'NONE', #33719, #56671, #28071 ) ;
#4065 = DIRECTION ( 'NONE',  ( 0.000000000000000000, 0.8910065241883691201, -0.4539904997395446951 ) ) ;
#4066 = EDGE_CURVE ( 'NONE', #38196, #69125, #18510, .T. ) ;
#4067 = AXIS2_PLACEMENT_3D ( 'NONE', #69393, #57383, #35187 ) ;
#4068 = CARTESIAN_POINT ( 'NONE',  ( 10.00000000000000000, 0.000000000000000000, 0.000000000000000000 ) ) ;
#4069 = VECTOR ( 'NONE', #43982, 1000.000000000000000 ) ;
#4070 = CARTESIAN_POINT ( 'NONE',  ( 92.69370383062501162, -211.3315407142195852, 77.15447916753382174 ) ) ;
#4071 = ORIENTED_EDGE ( 'NONE', *, *, #71960, .F. ) ;
#4072 = EDGE_CURVE ( 'NONE', #40306, #13957, #7249, .T. ) ;
#4073 = ORIENTED_EDGE ( 'NONE', *, *, #21116, .T. ) ;
#4074 = EDGE_CURVE ( 'NONE', #428, #4451, #59340, .T. ) ;
#4075 = CARTESIAN_POINT ( 'NONE',  ( 97.25633982090076302, -209.4495095149827364, 74.79348190356850523 ) ) ;
#4076 = CARTESIAN_POINT ( 'NONE',  ( 11.99999999999999822, -41.76106447765533147, 62.50884508063410294 ) ) ;
#4077 = EDGE_CURVE ( 'NONE', #61415, #47972, #12865, .T. ) ;
#4078 = CARTESIAN_POINT ( 'NONE',  ( -3.000000000000000000, 5.835314593368772229, -22.81335362449846826 ) ) ;
#4079 = DIRECTION ( 'NONE',  ( 0.6575728627325955200, -0.7533909544171997208, 0.000000000000000000 ) ) ;
#4080 =( NAMED_UNIT ( * ) PLANE_ANGLE_UNIT ( ) SI_UNIT ( $, .RADIAN. ) );
#4081 = CARTESIAN_POINT ( 'NONE',  ( 95.00000000000000000, -207.3369185715606307, 77.57781250086715374 ) ) ;
#4082 = VECTOR ( 'NONE', #68738, 1000.000000000000000 ) ;
#4083 = EDGE_CURVE ( 'NONE', #28695, #64186, #24225, .T. ) ;
#4084 = EDGE_LOOP ( 'NONE', ( #40160, #53720, #50854, #26797 ) ) ;
#4085 = DIRECTION ( 'NONE',  ( -1.000000000000000000, 0.000000000000000000, 0.000000000000000000 ) ) ;
#4086 = ORIENTED_EDGE ( 'NONE', *, *, #48411, .T. ) ;
#4087 = ORIENTED_EDGE ( 'NONE', *, *, #33857, .T. ) ;
#4088 = LINE ( 'NONE', #55568, #41757 ) ;
#4089 = SURFACE_SIDE_STYLE ('',( #9707 ) ) ;
#4090 = DIRECTION ( 'NONE',  ( -0.2867529058022035837, 0.9580045777625452175, 0.000000000000000000 ) ) ;
#4091 = ORIENTED_EDGE ( 'NONE', *, *, #34732, .T. ) ;
#4092 = DIRECTION ( 'NONE',  ( -1.000000000000000000, 0.000000000000000000, -0.000000000000000000 ) ) ;
#4093 = CARTESIAN_POINT ( 'NONE',  ( 96.32499999999998863, -212.2949673200287179, 79.49604166840096298 ) ) ;
#4094 = CARTESIAN_POINT ( 'NONE',  ( 94.99999999999998579, 93.05995642670504253, 80.31624999999998238 ) ) ;
#4095 = ORIENTED_EDGE ( 'NONE', *, *, #28169, .T. ) ;
#4096 = CARTESIAN_POINT ( 'NONE',  ( 0.000000000000000000, -18.13022148937263012, 15.02647892043544608 ) ) ;
#4097 = EDGE_LOOP ( 'NONE', ( #8400, #30258, #58601, #31056 ) ) ;
#4098 = CARTESIAN_POINT ( 'NONE',  ( 10.00000000000000000, 26.01480285779933510, -70.53064760720289428 ) ) ;
#4099 = AXIS2_PLACEMENT_3D ( 'NONE', #48912, #30144, #57462 ) ;
#4100 = ORIENTED_EDGE ( 'NONE', *, *, #45139, .F. ) ;
#4101 = DIRECTION ( 'NONE',  ( 0.000000000000000000, 0.000000000000000000, 1.000000000000000000 ) ) ;
#4102 = CARTESIAN_POINT ( 'NONE',  ( -97.30629616937501680, 90.00000000000004263, 83.45156250086715488 ) ) ;
#4103 = EDGE_CURVE ( 'NONE', #12963, #67396, #69287, .T. ) ;
#4104 = CARTESIAN_POINT ( 'NONE',  ( 93.84685191531248449, 88.00268892867053694, 79.58864583420047722 ) ) ;
#4105 = VERTEX_POINT ( 'NONE', #40718 ) ;
#4106 = CARTESIAN_POINT ( 'NONE',  ( -94.99999999999997158, -213.0599564267049857, 78.80812500173429669 ) ) ;
#4107 = DIRECTION ( 'NONE',  ( -1.000000000000000000, 0.000000000000000000, -0.000000000000000000 ) ) ;
#4108 = ORIENTED_EDGE ( 'NONE', *, *, #30953, .T. ) ;
#4109 = CARTESIAN_POINT ( 'NONE',  ( 10.00000000000000000, 12.26510123303259725, 35.53030884539089840 ) ) ;
#4110 = CARTESIAN_POINT ( 'NONE',  ( -94.99999999999997158, -207.3369185715606307, 79.32406250086714294 ) ) ;
#4111 = AXIS2_PLACEMENT_3D ( 'NONE', #65108, #1251, #1615 ) ;
#4112 = ORIENTED_EDGE ( 'NONE', *, *, #22693, .T. ) ;
#4113 = ORIENTED_EDGE ( 'NONE', *, *, #71182, .F. ) ;
#4114 = DIRECTION ( 'NONE',  ( -1.000000000000000000, 0.000000000000000000, 0.000000000000000000 ) ) ;
#4115 = EDGE_CURVE ( 'NONE', #70536, #73020, #8594, .T. ) ;
#4116 = ORIENTED_EDGE ( 'NONE', *, *, #60967, .F. ) ;
#4117 = EDGE_CURVE ( 'NONE', #2620, #56468, #28682, .T. ) ;
#4118 = DIRECTION ( 'NONE',  ( 0.000000000000000000, 0.000000000000000000, 1.000000000000000000 ) ) ;
#4119 = CIRCLE ( 'NONE', #46126, 82.00000000000000000 ) ;
#4120 = DIRECTION ( 'NONE',  ( -0.000000000000000000, -0.9135454576426059736, 0.4067366430757887730 ) ) ;
#4121 = VERTEX_POINT ( 'NONE', #36540 ) ;
#4122 = CARTESIAN_POINT ( 'NONE',  ( -92.69370383062498320, -209.9999999999999716, 79.16531250086714522 ) ) ;
#4123 = ORIENTED_EDGE ( 'NONE', *, *, #3244, .F. ) ;
#4124 = EDGE_CURVE ( 'NONE', #464, #73769, #58993, .T. ) ;
#4125 = AXIS2_PLACEMENT_3D ( 'NONE', #11430, #27616, #22735 ) ;
#4126 = DIRECTION ( 'NONE',  ( -1.000000000000000000, 0.000000000000000000, -0.000000000000000000 ) ) ;
#4127 = CARTESIAN_POINT ( 'NONE',  ( 0.000000000000000000, 0.000000000000000000, 0.000000000000000000 ) ) ;
#4128 = CARTESIAN_POINT ( 'NONE',  ( 10.00000000000000000, 0.000000000000000000, 0.000000000000000000 ) ) ;
#4129 = ADVANCED_BREP_SHAPE_REPRESENTATION ( '', ( #12047, #43395 ), #72282 ) ;
#4130 = CARTESIAN_POINT ( 'NONE',  ( 10.00000000000000000, 9.188173127307297960, 40.98264845739753071 ) ) ;
#4131 = AXIS2_PLACEMENT_3D ( 'NONE', #11065, #55812, #33988 ) ;
#4132 = AXIS2_PLACEMENT_3D ( 'NONE', #35377, #46656, #33892 ) ;
#4133 = CARTESIAN_POINT ( 'NONE',  ( 93.67500000000001137, -207.7050326799711968, 82.35354166840096468 ) ) ;
#4134 = CARTESIAN_POINT ( 'NONE',  ( 96.15314808468748708, 88.00268892867053694, 89.21947916753380525 ) ) ;
#4135 = CYLINDRICAL_SURFACE ( 'NONE', #54173, 82.00000000000000000 ) ;
#4136 = LINE ( 'NONE', #50338, #9954 ) ;
#4137 = CYLINDRICAL_SURFACE ( 'NONE', #71660, 32.00000000000000000 ) ;
#4138 = DIRECTION ( 'NONE',  ( 0.000000000000000000, -0.3090169943749349057, -0.9510565162951577500 ) ) ;
#4139 = CARTESIAN_POINT ( 'NONE',  ( -96.32500000000001705, 87.70503267997129626, 87.64520833506762187 ) ) ;
#4140 = AXIS2_PLACEMENT_3D ( 'NONE', #59967, #66700, #15565 ) ;
#4141 = CARTESIAN_POINT ( 'NONE',  ( 0.000000000000000000, 0.000000000000000000, 0.000000000000000000 ) ) ;
#4142 = DIRECTION ( 'NONE',  ( 1.000000000000000000, 0.000000000000000000, 0.000000000000000000 ) ) ;
#4143 = AXIS2_PLACEMENT_3D ( 'NONE', #45244, #21544, #27177 ) ;
#4144 = DIRECTION ( 'NONE',  ( 1.000000000000000000, -0.000000000000000000, -0.000000000000000000 ) ) ;
#4145 = DIRECTION ( 'NONE',  ( -1.000000000000000000, 0.000000000000000000, -0.000000000000000000 ) ) ;
#4146 = CARTESIAN_POINT ( 'NONE',  ( -97.64999999999996305, -209.9999999999999716, 83.01499999999998636 ) ) ;
#4147 = EDGE_CURVE ( 'NONE', #15890, #15888, #57823, .T. ) ;
#4148 = DIRECTION ( 'NONE',  ( 0.000000000000000000, 0.000000000000000000, 1.000000000000000000 ) ) ;
#4149 = CARTESIAN_POINT ( 'NONE',  ( 10.00000000000000000, 0.000000000000000000, 0.000000000000000000 ) ) ;
#4150 = CARTESIAN_POINT ( 'NONE',  ( 10.00000000000000000, -71.91182617369167929, -28.89263327155822481 ) ) ;
#4151 = CARTESIAN_POINT ( 'NONE',  ( -10.00000000000000000, 0.000000000000000000, 0.000000000000000000 ) ) ;
#4152 = DIRECTION ( 'NONE',  ( 0.000000000000000000, 0.000000000000000000, 1.000000000000000000 ) ) ;
#4153 = CIRCLE ( 'NONE', #20932, 82.00000000000000000 ) ;
#4154 = CARTESIAN_POINT ( 'NONE',  ( 92.69370383062501162, -211.3315407142195852, 87.94947916753382344 ) ) ;
#4155 = ORIENTED_EDGE ( 'NONE', *, *, #22922, .T. ) ;
#4156 = EDGE_CURVE ( 'NONE', #21857, #16649, #22997, .T. ) ;
#4157 = VERTEX_POINT ( 'NONE', #3468 ) ;
#4159 = EDGE_CURVE ( 'NONE', #17752, #15096, #18200, .T. ) ;
#4158 = CARTESIAN_POINT ( 'NONE',  ( 10.00000000000000000, -37.58145647212455032, 16.68533520207890319 ) ) ;
#4160 = CARTESIAN_POINT ( 'NONE',  ( 0.000000000000000000, 38.55633173627010279, 16.65560815589424593 ) ) ;
#4161 = ORIENTED_EDGE ( 'NONE', *, *, #67886, .F. ) ;
#4162 = CARTESIAN_POINT ( 'NONE',  ( 93.84685191531251292, -211.9973110713294489, 77.68364583420047609 ) ) ;
#4163 = CARTESIAN_POINT ( 'NONE',  ( 92.69370383062501162, -211.3315407142195852, 83.50447916753383026 ) ) ;
#4164 = VECTOR ( 'NONE', #12813, 1000.000000000000000 ) ;
#4165 = ORIENTED_EDGE ( 'NONE', *, *, #22883, .T. ) ;
#4166 = VECTOR ( 'NONE', #8705, 1000.000000000000000 ) ;
#4167 = CARTESIAN_POINT ( 'NONE',  ( 96.15314808468748708, -208.0026889286704943, 87.68489583420048916 ) ) ;
#4168 = EDGE_CURVE ( 'NONE', #19312, #6682, #16079, .T. ) ;
#4169 = EDGE_CURVE ( 'NONE', #35224, #26348, #9083, .T. ) ;
#4170 = EDGE_LOOP ( 'NONE', ( #2196, #10893 ) ) ;
#4171 = DIRECTION ( 'NONE',  ( 0.000000000000000000, 1.053567635648656885E-14, 1.000000000000000000 ) ) ;
#4172 = ORIENTED_EDGE ( 'NONE', *, *, #48042, .T. ) ;
#4173 = CIRCLE ( 'NONE', #10114, 31.99999999999998224 ) ;
#4174 = PLANE ( 'NONE',  #20075 ) ;
#4175 = ORIENTED_EDGE ( 'NONE', *, *, #3231, .F. ) ;
#4176 = ORIENTED_EDGE ( 'NONE', *, *, #8054, .T. ) ;
#4177 = DIRECTION ( 'NONE',  ( 0.000000000000000000, 0.8526401643540897357, 0.5224985647159527957 ) ) ;
#4178 = VERTEX_POINT ( 'NONE', #31274 ) ;
#4179 = CARTESIAN_POINT ( 'NONE',  ( 15.00000000000000000, -10.45096189432344502, -21.10159698893425784 ) ) ;
#4180 = CARTESIAN_POINT ( 'NONE',  ( 96.32499999999998863, -207.7050326799711968, 89.23270833506762756 ) ) ;
#4181 = ORIENTED_EDGE ( 'NONE', *, *, #62951, .F. ) ;
#4182 = DIRECTION ( 'NONE',  ( 0.000000000000000000, -0.9876883405951358830, -0.1564344650402420822 ) ) ;
#4183 = AXIS2_PLACEMENT_3D ( 'NONE', #59354, #30027, #29647 ) ;
#4184 = EDGE_LOOP ( 'NONE', ( #23491, #19316, #36047, #73859 ) ) ;
#4185 = FACE_OUTER_BOUND ( 'NONE', #47158, .T. ) ;
#4186 = EDGE_CURVE ( 'NONE', #55121, #39963, #53474, .T. ) ;
#4187 = ORIENTED_EDGE ( 'NONE', *, *, #30719, .T. ) ;
#4188 = VECTOR ( 'NONE', #2189, 1000.000000000000227 ) ;
#4189 = EDGE_LOOP ( 'NONE', ( #13945, #38307, #39494, #6690 ) ) ;
#4190 = ORIENTED_EDGE ( 'NONE', *, *, #65389, .F. ) ;
#4191 = CARTESIAN_POINT ( 'NONE',  ( 95.00000000000000000, -207.3369185715606307, 74.87906250086713555 ) ) ;
#4192 = CARTESIAN_POINT ( 'NONE',  ( 11.99999999999999822, 77.32052557432841411, 5.256550761633121738 ) ) ;
#4193 = ORIENTED_EDGE ( 'NONE', *, *, #31760, .F. ) ;
#4194 = EDGE_LOOP ( 'NONE', ( #24713, #15446, #61971 ) ) ;
#4195 = ORIENTED_EDGE ( 'NONE', *, *, #45143, .F. ) ;
#4196 = CARTESIAN_POINT ( 'NONE',  ( -92.34999999999996589, -211.5299782133524502, 84.54958333333334508 ) ) ;
#4197 = CARTESIAN_POINT ( 'NONE',  ( -92.34999999999990905, -208.4700217866474929, 88.46541666666664128 ) ) ;
#4198 = CARTESIAN_POINT ( 'NONE',  ( -96.15314808468751551, 88.00268892867056536, 75.93739583420048689 ) ) ;
#4199 = EDGE_CURVE ( 'NONE', #32740, #72643, #756, .T. ) ;
#4200 = EDGE_CURVE ( 'NONE', #11638, #64091, #65005, .T. ) ;
#4201 = EDGE_LOOP ( 'NONE', ( #10088, #15057 ) ) ;
#4202 = CARTESIAN_POINT ( 'NONE',  ( 92.69370383062498320, 88.66845928578037217, 77.63072916753380071 ) ) ;
#4203 = ORIENTED_EDGE ( 'NONE', *, *, #69812, .T. ) ;
#4204 =( LENGTH_UNIT ( ) NAMED_UNIT ( * ) SI_UNIT ( .MILLI., .METRE. ) );
#4205 = CARTESIAN_POINT ( 'NONE',  ( -93.84685191531248449, -208.0026889286704943, 88.79614583420047325 ) ) ;
#4206 = ORIENTED_EDGE ( 'NONE', *, *, #70890, .F. ) ;
#4207 = ADVANCED_FACE ( 'NONE', ( #71116, #8723 ), #3108, .T. ) ;
#4208 = CARTESIAN_POINT ( 'NONE',  ( 0.7207917504152147048, -5.357353380764381612, -1.325189086772950331 ) ) ;
#4209 = LINE ( 'NONE', #56447, #25979 ) ;
#4210 = DIRECTION ( 'NONE',  ( -0.000000000000000000, -0.000000000000000000, -1.000000000000000000 ) ) ;
#4211 = CARTESIAN_POINT ( 'NONE',  ( -93.84685191531248449, -208.0026889286704943, 78.63614583420047666 ) ) ;
#4212 = CARTESIAN_POINT ( 'NONE',  ( 11.99999999999999822, 41.19522573413826194, -65.64334221924865176 ) ) ;
#4213 = DIRECTION ( 'NONE',  ( 0.000000000000000000, -0.5000000000000012212, -0.8660254037844380415 ) ) ;
#4214 = CARTESIAN_POINT ( 'NONE',  ( -97.64999999999996305, -209.9999999999999716, 84.28499999999999659 ) ) ;
#4215 = EDGE_LOOP ( 'NONE', ( #56432, #33445, #45255, #50926 ) ) ;
#4216 = AXIS2_PLACEMENT_3D ( 'NONE', #73132, #22014, #26903 ) ;
#4217 = ORIENTED_EDGE ( 'NONE', *, *, #66382, .T. ) ;
#4218 = DIRECTION ( 'NONE',  ( 0.9966891607226785466, 0.08130631524010119293, -0.000000000000000000 ) ) ;
#4219 = CARTESIAN_POINT ( 'NONE',  ( 11.99999999999999822, 0.000000000000000000, 0.000000000000000000 ) ) ;
#4220 = DIRECTION ( 'NONE',  ( -0.000000000000000000, -0.000000000000000000, 1.000000000000000000 ) ) ;
#4221 = CARTESIAN_POINT ( 'NONE',  ( -95.00000000000002842, 92.66308142843932671, 82.49906250086714010 ) ) ;
#4222 = CARTESIAN_POINT ( 'NONE',  ( 10.00000000000000000, -5.202137450156129717, -37.22597642581163768 ) ) ;
#4223 = CARTESIAN_POINT ( 'NONE',  ( 0.000000000000000000, 0.000000000000000000, -54.99999999999998579 ) ) ;
#4224 = AXIS2_PLACEMENT_3D ( 'NONE', #43272, #54892, #47772 ) ;
#4225 = ORIENTED_EDGE ( 'NONE', *, *, #52828, .F. ) ;
#4226 = CIRCLE ( 'NONE', #33011, 31.99999999999998579 ) ;
#4227 = CARTESIAN_POINT ( 'NONE',  ( 97.64999999999602665, -210.0000045800691737, 76.42687486206342840 ) ) ;
#4229 = DIRECTION ( 'NONE',  ( -1.000000000000000000, 7.677074106448950501E-15, 2.598394312951952234E-14 ) ) ;
#4228 = CIRCLE ( 'NONE', #47413, 31.99999999999998934 ) ;
#4230 = DIRECTION ( 'NONE',  ( 0.000000000000000000, 0.3090169943749450088, -0.9510565162951544194 ) ) ;
#4231 = CARTESIAN_POINT ( 'NONE',  ( -1.332830945733270545, 5.003992386592893915, -0.8603634151101617888 ) ) ;
#4232 = CARTESIAN_POINT ( 'NONE',  ( 93.67500000000001137, -207.7050326799711968, 88.70354166840097321 ) ) ;
#4233 = CARTESIAN_POINT ( 'NONE',  ( -93.84685191531248449, -208.0026889286704943, 79.42989583420049371 ) ) ;
#4234 = CIRCLE ( 'NONE', #64274, 12.49999999999999645 ) ;
#4235 = CARTESIAN_POINT ( 'NONE',  ( -92.34999999999999432, -209.9999999999999716, 87.22187500173430408 ) ) ;
#4236 = ADVANCED_FACE ( 'NONE', ( #20368 ), #2010, .T. ) ;
#4237 =( BOUNDED_CURVE ( )  B_SPLINE_CURVE ( 2, ( #23300, #40581, #34562, #46226, #39102, #63529, #62427 ),
 .UNSPECIFIED., .F., .F. ) 
 B_SPLINE_CURVE_WITH_KNOTS ( ( 3, 2, 2, 3 ),
 ( 0.6350190250602294473, 0.6420746642234487211, 0.6491304297643658572, 0.6561861948943049638 ),
 .UNSPECIFIED. ) 
 CURVE ( )  GEOMETRIC_REPRESENTATION_ITEM ( )  RATIONAL_B_SPLINE_CURVE ( ( 0.9999952007765371409, 0.8660278034391509783, 1.000000000000000000, 0.8660254037844387076, 1.000000000000000000, 0.8660254037844387076, 1.000000000000000000 ) ) 
 REPRESENTATION_ITEM ( '' )  );
#4238 = ORIENTED_EDGE ( 'NONE', *, *, #26477, .F. ) ;
#4239 = LINE ( 'NONE', #50063, #59899 ) ;
#4240 = VECTOR ( 'NONE', #48745, 1000.000000000000000 ) ;
#4241 = EDGE_CURVE ( 'NONE', #66971, #59392, #8403, .T. ) ;
#4242 = CARTESIAN_POINT ( 'NONE',  ( 10.00000000000000000, -5.202137450156129717, -37.22597642581163768 ) ) ;
#4243 = DIRECTION ( 'NONE',  ( 0.000000000000000000, 0.000000000000000000, 1.000000000000000000 ) ) ;
#4244 = ORIENTED_EDGE ( 'NONE', *, *, #37598, .F. ) ;
#4245 = DIRECTION ( 'NONE',  ( 1.000000000000000000, 0.000000000000000000, 0.000000000000000000 ) ) ;
#4246 = DIRECTION ( 'NONE',  ( -1.000000000000000000, 0.000000000000000000, 0.000000000000000000 ) ) ;
#4247 = EDGE_CURVE ( 'NONE', #42384, #68050, #23768, .T. ) ;
#4248 = CONICAL_SURFACE ( 'NONE', #34229, 17.45460580326810174, 1.361356816555583826 ) ;
#4249 = EDGE_CURVE ( 'NONE', #6916, #55524, #10947, .T. ) ;
#4250 = CARTESIAN_POINT ( 'NONE',  ( 11.99999999999999822, -75.11764819372149304, 2.946379043146075905 ) ) ;
#4251 = ORIENTED_EDGE ( 'NONE', *, *, #46885, .T. ) ;
#4252 = LINE ( 'NONE', #15508, #23496 ) ;
#4253 = ORIENTED_EDGE ( 'NONE', *, *, #70967, .T. ) ;
#4254 = CARTESIAN_POINT ( 'NONE',  ( -92.35000000000003695, 90.00000000000004263, 80.15749999999999886 ) ) ;
#4255 = DIRECTION ( 'NONE',  ( -1.000000000000000000, -0.000000000000000000, 0.000000000000000000 ) ) ;
#4256 = VERTEX_POINT ( 'NONE', #62466 ) ;
#4257 = DIRECTION ( 'NONE',  ( 0.000000000000000000, -0.1045284632676570791, 0.9945218953682730678 ) ) ;
#4258 = ADVANCED_FACE ( 'NONE', ( #44047 ), #21846, .F. ) ;
#4259 = ORIENTED_EDGE ( 'NONE', *, *, #30626, .T. ) ;
#4260 = DIRECTION ( 'NONE',  ( 0.9135454576426004225, 0.4067366430758009854, 0.000000000000000000 ) ) ;
#4261 = AXIS2_PLACEMENT_3D ( 'NONE', #73789, #4288, #50495 ) ;
#4262 = CARTESIAN_POINT ( 'NONE',  ( 26.50000000000000355, -120.0000000000000000, -64.00000000000000000 ) ) ;
#4263 = ORIENTED_EDGE ( 'NONE', *, *, #22560, .F. ) ;
#4264 = EDGE_LOOP ( 'NONE', ( #29324, #56595, #9271, #5112 ) ) ;
#4265 = ORIENTED_EDGE ( 'NONE', *, *, #55749, .F. ) ;
#4266 = CARTESIAN_POINT ( 'NONE',  ( 2.117611129180199558, -93.54218975225703048, 5.500000000000000000 ) ) ;
#4267 = ORIENTED_EDGE ( 'NONE', *, *, #23102, .T. ) ;
#4268 = EDGE_CURVE ( 'NONE', #42280, #23222, #27805, .T. ) ;
#4269 = ORIENTED_EDGE ( 'NONE', *, *, #12824, .F. ) ;
#4270 = CARTESIAN_POINT ( 'NONE',  ( 97.30629616937498838, 91.33154071421968467, 74.93197916753381094 ) ) ;
#4271 = AXIS2_PLACEMENT_3D ( 'NONE', #41588, #29553, #64905 ) ;
#4272 = CARTESIAN_POINT ( 'NONE',  ( -35.50000000000000711, -120.0000000000000000, 5.500000000000000000 ) ) ;
#4273 = EDGE_CURVE ( 'NONE', #54553, #47718, #20355, .T. ) ;
#4275 = CARTESIAN_POINT ( 'NONE',  ( 6.078523336270777024E-16, 5.773502691896261751, -6.000000000000000000 ) ) ;
#4274 = AXIS2_PLACEMENT_3D ( 'NONE', #30254, #17869, #47186 ) ;
#4276 = ORIENTED_EDGE ( 'NONE', *, *, #57134, .F. ) ;
#4277 = ORIENTED_EDGE ( 'NONE', *, *, #42626, .F. ) ;
#4278 = EDGE_LOOP ( 'NONE', ( #38221, #4962, #18769, #45811 ) ) ;
#4279 = CARTESIAN_POINT ( 'NONE',  ( 92.69370383062498320, 91.33154071421968467, 89.58989583420047609 ) ) ;
#4281 = EDGE_LOOP ( 'NONE', ( #54923, #43602, #71072, #26070 ) ) ;
#4280 = EDGE_CURVE ( 'NONE', #62636, #53174, #70531, .T. ) ;
#4282 = VECTOR ( 'NONE', #73942, 1000.000000000000227 ) ;
#4283 = CARTESIAN_POINT ( 'NONE',  ( 97.30629616937498838, -211.3315407142195852, 86.73239583420047438 ) ) ;
#4284 = DIRECTION ( 'NONE',  ( -5.551115123125782702E-17, 0.000000000000000000, -1.000000000000000000 ) ) ;
#4285 = DIRECTION ( 'NONE',  ( 0.000000000000000000, 0.000000000000000000, 1.000000000000000000 ) ) ;
#4286 = CARTESIAN_POINT ( 'NONE',  ( -96.32499999999996021, -207.7050326799711968, 80.36916666666665776 ) ) ;
#4287 = CARTESIAN_POINT ( 'NONE',  ( 10.00000000000000000, -0.8828120875898013420, -37.48860685352291711 ) ) ;
#4288 = DIRECTION ( 'NONE',  ( -1.000000000000000000, 0.000000000000000000, 0.000000000000000000 ) ) ;
#4289 = CIRCLE ( 'NONE', #22302, 37.49900000000000944 ) ;
#4290 = CARTESIAN_POINT ( 'NONE',  ( -92.34999999999999432, -209.9999999999999716, 82.69749999999999091 ) ) ;
#4291 = CARTESIAN_POINT ( 'NONE',  ( 11.99999999999999822, 33.71516098798741012, 74.74816331893441657 ) ) ;
#4292 = CARTESIAN_POINT ( 'NONE',  ( -94.99999999999997158, -207.3369185715606307, 87.57906250086713840 ) ) ;
#4293 = CARTESIAN_POINT ( 'NONE',  ( -93.84685191531252713, 88.00268892867056536, 84.29822916753381890 ) ) ;
#4294 = EDGE_CURVE ( 'NONE', #20558, #12759, #42209, .T. ) ;
#4295 = ORIENTED_EDGE ( 'NONE', *, *, #19924, .F. ) ;
#4297 = CARTESIAN_POINT ( 'NONE',  ( -95.00000000000002842, 92.66308142843932671, 86.94406250086714749 ) ) ;
#4296 = CARTESIAN_POINT ( 'NONE',  ( 94.99999999999998579, 87.33691857156068750, 89.16656250086712987 ) ) ;
#4298 = AXIS2_PLACEMENT_3D ( 'NONE', #3665, #44891, #34704 ) ;
#4299 = ORIENTED_EDGE ( 'NONE', *, *, #15009, .F. ) ;
#4300 = CARTESIAN_POINT ( 'NONE',  ( 97.30629616937498838, 89.06967028092473981, 74.84209033237942776 ) ) ;
#4301 = ADVANCED_FACE ( 'NONE', ( #55318 ), #62084, .T. ) ;
#4302 = DIRECTION ( 'NONE',  ( 0.000000000000000000, 0.9876883405951371042, 0.1564344650402346715 ) ) ;
#4303 = CARTESIAN_POINT ( 'NONE',  ( -95.00000000000002842, 90.00000000000004263, 90.00000000000000000 ) ) ;
#4304 = DIRECTION ( 'NONE',  ( -1.000000000000000000, -0.000000000000000000, -0.000000000000000000 ) ) ;
#4305 = AXIS2_PLACEMENT_3D ( 'NONE', #15931, #17416, #16305 ) ;
#4306 = CARTESIAN_POINT ( 'NONE',  ( -96.15314808468745866, -211.9973110713294489, 89.11364583420048291 ) ) ;
#4307 = ADVANCED_FACE ( 'NONE', ( #21089 ), #43686, .T. ) ;
#4308 = CARTESIAN_POINT ( 'NONE',  ( -95.00000000000002842, 90.00000000000004263, 90.00000000000000000 ) ) ;
#4309 = CARTESIAN_POINT ( 'NONE',  ( 0.000000000000000000, 77.49459641780886443, 0.8261519478433866359 ) ) ;
#4310 = CARTESIAN_POINT ( 'NONE',  ( 0.000000000000000000, 0.000000000000000000, 0.000000000000000000 ) ) ;
#4311 = ORIENTED_EDGE ( 'NONE', *, *, #64511, .T. ) ;
#4312 = VERTEX_POINT ( 'NONE', #22222 ) ;
#4313 = CARTESIAN_POINT ( 'NONE',  ( -97.65000000000001990, 90.00000000000004263, 80.47499999999999432 ) ) ;
#4314 = CARTESIAN_POINT ( 'NONE',  ( 10.00000000000000000, -55.20638768913724448, -51.02545421589383068 ) ) ;
#4315 = CARTESIAN_POINT ( 'NONE',  ( 97.64999999999989200, -208.4700217866474077, 75.76541666666668107 ) ) ;
#4316 = FACE_OUTER_BOUND ( 'NONE', #44759, .T. ) ;
#4317 = CARTESIAN_POINT ( 'NONE',  ( 0.000000000000000000, 0.000000000000000000, -0.3851141460153411078 ) ) ;
#4318 = DIRECTION ( 'NONE',  ( -1.000000000000000000, -0.000000000000000000, -0.000000000000000000 ) ) ;
#4319 = DIRECTION ( 'NONE',  ( 0.000000000000000000, 0.000000000000000000, 1.000000000000000000 ) ) ;
#4320 = DIRECTION ( 'NONE',  ( -1.000000000000000000, 0.000000000000000000, -0.000000000000000000 ) ) ;
#4321 = EDGE_LOOP ( 'NONE', ( #45299, #29200, #72111, #52967 ) ) ;
#4322 = CARTESIAN_POINT ( 'NONE',  ( -96.15314808468752972, 91.99731107132950569, 81.91697916753381037 ) ) ;
#4323 = LINE ( 'NONE', #37786, #64382 ) ;
#4324 = DIRECTION ( 'NONE',  ( -0.000000000000000000, -0.000000000000000000, -1.000000000000000000 ) ) ;
#4325 = FACE_OUTER_BOUND ( 'NONE', #33187, .T. ) ;
#4326 = PLANE ( 'NONE',  #72878 ) ;
#4327 = DIRECTION ( 'NONE',  ( 0.000000000000000000, 0.000000000000000000, 1.000000000000000000 ) ) ;
#4328 = CARTESIAN_POINT ( 'NONE',  ( -93.84685191531247028, -211.9973110713294489, 89.37822916753381719 ) ) ;
#4329 = FACE_OUTER_BOUND ( 'NONE', #41240, .T. ) ;
#4330 = CARTESIAN_POINT ( 'NONE',  ( 96.15314808468748708, 88.00268892867053694, 79.21822916753382060 ) ) ;
#4331 = CARTESIAN_POINT ( 'NONE',  ( -92.69370383062498320, -209.9999999999999716, 83.13406250086715943 ) ) ;
#4332 = FACE_OUTER_BOUND ( 'NONE', #71681, .T. ) ;
#4333 = ORIENTED_EDGE ( 'NONE', *, *, #17757, .T. ) ;
#4334 = DIRECTION ( 'NONE',  ( -1.000000000000000000, -0.000000000000000000, -0.000000000000000000 ) ) ;
#4335 = CARTESIAN_POINT ( 'NONE',  ( -97.64999999999994884, -211.5299782133524502, 77.98791666666664923 ) ) ;
#4336 = EDGE_CURVE ( 'NONE', #22617, #32997, #35008, .T. ) ;
#4337 = CARTESIAN_POINT ( 'NONE',  ( 10.00000000000000000, -46.21855187248583974, -62.20884554314070414 ) ) ;
#4338 = ADVANCED_FACE ( 'NONE', ( #9451 ), #61708, .F. ) ;
#4339 = CIRCLE ( 'NONE', #25938, 37.49900000000000944 ) ;
#4340 = CIRCLE ( 'NONE', #30712, 2.649999999999985700 ) ;
#4341 = EDGE_CURVE ( 'NONE', #69813, #62636, #18489, .T. ) ;
#4342 = CARTESIAN_POINT ( 'NONE',  ( -97.30629616937501680, 88.66845928578038638, 79.05947916753382287 ) ) ;
#4343 = CARTESIAN_POINT ( 'NONE',  ( 93.84685191531249870, -208.0026889286704943, 80.64697916753381435 ) ) ;
#4344 = VERTEX_POINT ( 'NONE', #50783 ) ;
#4345 = ORIENTED_EDGE ( 'NONE', *, *, #14696, .T. ) ;
#4346 = VECTOR ( 'NONE', #5332, 1000.000000000000000 ) ;
#4347 = CARTESIAN_POINT ( 'NONE',  ( 5.822613034544236399, -142.8165987265839760, 5.500000000000000000 ) ) ;
#4348 = EDGE_LOOP ( 'NONE', ( #29664, #31807, #63172, #69094 ) ) ;
#4349 = FACE_OUTER_BOUND ( 'NONE', #73662, .T. ) ;
#4350 = ORIENTED_EDGE ( 'NONE', *, *, #62756, .F. ) ;
#4351 = VERTEX_POINT ( 'NONE', #34607 ) ;
#4352 = ORIENTED_EDGE ( 'NONE', *, *, #36729, .F. ) ;
#4353 = CARTESIAN_POINT ( 'NONE',  ( 92.69370383062501162, -208.6684592857803295, 76.41364583420049428 ) ) ;
#4354 = CARTESIAN_POINT ( 'NONE',  ( 0.000000000000000000, 0.000000000000000000, 0.000000000000000000 ) ) ;
#4355 = DIRECTION ( 'NONE',  ( 0.000000000000000000, 0.8910065241883657894, 0.4539904997395510788 ) ) ;
#4356 = CARTESIAN_POINT ( 'NONE',  ( -11.99999999999999645, 1.574895783703496238E-15, -12.85999999999999943 ) ) ;
#4357 = CARTESIAN_POINT ( 'NONE',  ( 97.30629616937498838, 91.33154071421968467, 86.99697916753382287 ) ) ;
#4358 = CARTESIAN_POINT ( 'NONE',  ( 2.499999999999988454, -65.00000000000000000, -290.0000000000000568 ) ) ;
#4359 = CARTESIAN_POINT ( 'NONE',  ( 95.00000000000000000, -213.0599564267049857, 76.82374999999998977 ) ) ;
#4360 = ORIENTED_EDGE ( 'NONE', *, *, #1175, .F. ) ;
#4361 = ORIENTED_EDGE ( 'NONE', *, *, #67415, .T. ) ;
#4362 = VERTEX_POINT ( 'NONE', #447 ) ;
#4363 = EDGE_LOOP ( 'NONE', ( #18841, #70340, #60405, #40949 ) ) ;
#4364 = FACE_OUTER_BOUND ( 'NONE', #32659, .T. ) ;
#4365 = EDGE_CURVE ( 'NONE', #9063, #35752, #34989, .T. ) ;
#4366 = ADVANCED_FACE ( 'NONE', ( #68469 ), #74087, .T. ) ;
#4367 = CLOSED_SHELL ( 'NONE', ( #25388, #28567, #60637, #50250, #27416, #7301, #42177, #42548, #11987, #70442, #66033, #19959, #65638, #15108, #25792, #9334, #18733, #49473, #54238, #29272, #36587, #60870, #61668, #41937, #52385, #28921, #67624, #57032, #26316, #20773, #39146, #21995, #26792, #33722, #1773, #15820, #22720, #49421, #6485, #45364, #27395, #36906, #20292, #23971, #50768, #30057, #41315, #44432, #61945, #28448, #43966, #67494, #10806, #1657, #29456, #18250, #50142, #40580, #22057, #55922, #28579, #41491, #43375, #42536, #63668, #51958, #63318, #71549, #36842, #20966, #5146, #73667, #71017, #49614, #69432, #62769, #53229, #46463, #49480, #19537, #6930, #32403, #68929, #13002, #9789, #11445, #69342, #65724, #24938, #18691, #19450, #38989, #67194, #7209, #17178, #19852, #32062, #64163, #3668, #29851, #52649, #44833, #12285, #43426, #69781, #22231, #53047, #48181, #44744, #66709, #42711, #71081, #61915, #11988, #29026, #61626, #31080, #49282, #37467, #487, #15020, #18823, #64615, #20119, #17410, #18648, #1132, #40142, #65689, #44395, #35983, #29036, #4307, #30028, #40470, #22471, #10195, #66638, #10938, #47313, #6208, #37851, #7241, #26292, #7125, #31705, #67839, #62025, #23128, #65013, #26225, #41693, #38731, #10714, #26669, #24719, #72870, #16905, #54160, #9058, #62036, #61651, #10089, #51762, #11717, #71372, #969, #70695, #31468, #2503, #51277, #23349, #47561, #18085, #56877, #52276, #50767, #30058, #29753, #54691, #44938, #69863, #21189, #53273, #459, #68232, #47144, #6712, #56440, #40554, #71431, #36845, #57143, #15469, #35963, #52130, #51344, #53414, #69279, #23827, #7079, #59588, #52596, #23293, #69105, #42461, #39080, #26149, #3940, #62220, #62570, #12799, #66817, #22480, #16630, #11624, #21700, #21477, #4429, #47783, #72705, #19102, #71456, #20729, #28710, #7329, #29938, #23433, #52873, #55513, #15120, #17466, #53457, #49657, #41756, #60849, #67165, #63980, #25860, #41971, #36396, #41736, #11783, #25626 ) ) ;
#4368 = DIRECTION ( 'NONE',  ( 0.000000000000000000, 0.000000000000000000, 1.000000000000000000 ) ) ;
#4369 = CARTESIAN_POINT ( 'NONE',  ( -12.50000000000000000, -132.5000000000000000, -40.00000000000000000 ) ) ;
#4370 = CARTESIAN_POINT ( 'NONE',  ( 95.00000000000000000, -213.0599564267049857, 82.61812500173428475 ) ) ;
#4371 = CARTESIAN_POINT ( 'NONE',  ( 0.000000000000000000, 74.74816331893477184, -33.71516098798660011 ) ) ;
#4372 = DIRECTION ( 'NONE',  ( -0.7533909544171996098, -0.6575728627325955200, 7.625282249115660656E-32 ) ) ;
#4373 = EDGE_LOOP ( 'NONE', ( #40029, #34840, #1883, #44041 ) ) ;
#4374 = CARTESIAN_POINT ( 'NONE',  ( -94.99999999999997158, -213.0599564267049857, 81.34812500173430294 ) ) ;
#4375 = VERTEX_POINT ( 'NONE', #22981 ) ;
#4376 = DIRECTION ( 'NONE',  ( -1.000000000000000000, 0.000000000000000000, -0.000000000000000000 ) ) ;
#4377 = EDGE_CURVE ( 'NONE', #69721, #16255, #57925, .T. ) ;
#4378 = ORIENTED_EDGE ( 'NONE', *, *, #60273, .T. ) ;
#4380 = CARTESIAN_POINT ( 'NONE',  ( -96.32500000000001705, 92.29496732002878900, 83.62354166840097491 ) ) ;
#4379 = CARTESIAN_POINT ( 'NONE',  ( 93.67499999999999716, 87.70503267997126784, 82.56520833506762358 ) ) ;
#4381 = ORIENTED_EDGE ( 'NONE', *, *, #39501, .F. ) ;
#4382 = CARTESIAN_POINT ( 'NONE',  ( 96.15314808468748708, 91.99731107132950569, 84.50989583420049200 ) ) ;
#4383 = AXIS2_PLACEMENT_3D ( 'NONE', #36541, #59488, #20736 ) ;
#4384 = LINE ( 'NONE', #62648, #33767 ) ;
#4385 = CARTESIAN_POINT ( 'NONE',  ( 11.99999999999999822, 74.65491531819118620, -8.830959090342659579 ) ) ;
#4386 = DIRECTION ( 'NONE',  ( -1.000000000000000000, -0.000000000000000000, -0.000000000000000000 ) ) ;
#4387 = DIRECTION ( 'NONE',  ( 0.000000000000000000, 0.000000000000000000, -1.000000000000000000 ) ) ;
#4388 = LINE ( 'NONE', #69654, #37159 ) ;
#4389 = VERTEX_POINT ( 'NONE', #16960 ) ;
#4390 = CARTESIAN_POINT ( 'NONE',  ( 15.00000000000000000, -10.45096189432344502, -21.10159698893425784 ) ) ;
#4391 = CARTESIAN_POINT ( 'NONE',  ( 11.99999999999999822, -18.89407956138310496, 75.16055320797023853 ) ) ;
#4392 = DIRECTION ( 'NONE',  ( -1.000000000000000000, 0.000000000000000000, 0.000000000000000000 ) ) ;
#4393 = ORIENTED_EDGE ( 'NONE', *, *, #68628, .F. ) ;
#4394 = AXIS2_PLACEMENT_3D ( 'NONE', #51611, #62925, #46347 ) ;
#4395 = ORIENTED_EDGE ( 'NONE', *, *, #6229, .F. ) ;
#4396 = CIRCLE ( 'NONE', #17571, 82.00000000000000000 ) ;
#4397 = PRODUCT_DEFINITION_SHAPE ( 'NONE', 'NONE',  #37077 ) ;
#4398 = CARTESIAN_POINT ( 'NONE',  ( 11.99999999999999822, 50.95692526931329525, 58.39081064771768581 ) ) ;
#4399 = AXIS2_PLACEMENT_3D ( 'NONE', #29425, #547, #70020 ) ;
#4400 = AXIS2_PLACEMENT_3D ( 'NONE', #40542, #40180, #57473 ) ;
#4401 = CARTESIAN_POINT ( 'NONE',  ( -97.65000000000001990, 90.00000000000004263, 79.91937500173429498 ) ) ;
#4402 = CYLINDRICAL_SURFACE ( 'NONE', #55754, 77.49899999999999523 ) ;
#4403 = CARTESIAN_POINT ( 'NONE',  ( -93.84685191531248449, -208.0026889286704943, 81.33489583420049485 ) ) ;
#4404 = ORIENTED_EDGE ( 'NONE', *, *, #60095, .T. ) ;
#4405 = CARTESIAN_POINT ( 'NONE',  ( 10.00000000000000000, 38.55633173627010990, 16.65560815589424593 ) ) ;
#4406 = ORIENTED_EDGE ( 'NONE', *, *, #30646, .T. ) ;
#4407 = CARTESIAN_POINT ( 'NONE',  ( -92.35000000000000853, -209.9999996502046429, 77.69687501385436690 ) ) ;
#4408 = FACE_BOUND ( 'NONE', #61031, .T. ) ;
#4409 = AXIS2_PLACEMENT_3D ( 'NONE', #48070, #48796, #60831 ) ;
#4410 = DIRECTION ( 'NONE',  ( 0.000000000000000000, 0.000000000000000000, 1.000000000000000000 ) ) ;
#4411 = CARTESIAN_POINT ( 'NONE',  ( 96.15314808468748708, 91.99731107132950569, 78.00114583420048575 ) ) ;
#4412 = CARTESIAN_POINT ( 'NONE',  ( 97.64999999999999147, -209.9999999999999716, 90.00000000000000000 ) ) ;
#4413 = CARTESIAN_POINT ( 'NONE',  ( 10.00000000000000000, 0.9569279952884557350, -2.499999999999984457 ) ) ;
#4414 = DIRECTION ( 'NONE',  ( 0.000000000000000000, -0.5877852522924802425, 0.8090169943749422332 ) ) ;
#4415 = CARTESIAN_POINT ( 'NONE',  ( 10.00000000000000000, -30.84782396557201878, -21.32104025579148399 ) ) ;
#4416 = PLANE ( 'NONE',  #70025 ) ;
#4417 = CARTESIAN_POINT ( 'NONE',  ( 93.67500000000001137, -212.2949673200287179, 84.39083333333333314 ) ) ;
#4418 = DIRECTION ( 'NONE',  ( 0.000000000000000000, 0.000000000000000000, 1.000000000000000000 ) ) ;
#4419 = DIRECTION ( 'NONE',  ( -1.000000000000000000, -0.000000000000000000, -0.000000000000000000 ) ) ;
#4420 = CARTESIAN_POINT ( 'NONE',  ( 94.99999999999998579, 86.94004357329502852, 76.90312500173429555 ) ) ;
#4421 = ORIENTED_EDGE ( 'NONE', *, *, #49055, .F. ) ;
#4422 = EDGE_CURVE ( 'NONE', #11744, #36763, #50613, .T. ) ;
#4423 = CARTESIAN_POINT ( 'NONE',  ( -97.30629616937501680, 90.00000000000004263, 82.65781250086713783 ) ) ;
#4424 = CYLINDRICAL_SURFACE ( 'NONE', #25131, 31.99999999999998579 ) ;
#4425 = ADVANCED_FACE ( 'NONE', ( #22601, #45547 ), #5690, .T. ) ;
#4426 = EDGE_CURVE ( 'NONE', #43916, #51617, #15649, .T. ) ;
#4427 = DIRECTION ( 'NONE',  ( 0.9227826878668540234, 0.3853207896976547087, -0.000000000000000000 ) ) ;
#4428 = VERTEX_POINT ( 'NONE', #41008 ) ;
#4429 = ADVANCED_FACE ( 'NONE', ( #57557 ), #29694, .F. ) ;
#4430 = DIRECTION ( 'NONE',  ( -0.000000000000000000, -0.000000000000000000, 1.000000000000000000 ) ) ;
#4431 = CARTESIAN_POINT ( 'NONE',  ( 99.99999999999998579, 95.00000000000002842, -90.00000000000000000 ) ) ;
#4432 = DIRECTION ( 'NONE',  ( 0.000000000000000000, 0.8526401643540936215, -0.5224985647159469115 ) ) ;
#4433 = AXIS2_PLACEMENT_3D ( 'NONE', #64364, #12838, #11365 ) ;
#4434 = EDGE_CURVE ( 'NONE', #35261, #72991, #20612, .T. ) ;
#4435 = DIRECTION ( 'NONE',  ( 0.000000000000000000, -0.9238795325112906243, 0.3826834323650805114 ) ) ;
#4436 = CARTESIAN_POINT ( 'NONE',  ( 93.84685191531251292, -211.9973110713294489, 77.20739583420048291 ) ) ;
#4437 = CIRCLE ( 'NONE', #44033, 37.49900000000001654 ) ;
#4438 = VERTEX_POINT ( 'NONE', #12048 ) ;
#4439 = AXIS2_PLACEMENT_3D ( 'NONE', #30977, #609, #58086 ) ;
#4440 = ORIENTED_EDGE ( 'NONE', *, *, #14063, .F. ) ;
#4441 = EDGE_CURVE ( 'NONE', #38665, #42030, #30216, .T. ) ;
#4442 = EDGE_CURVE ( 'NONE', #41319, #32106, #57870, .T. ) ;
#4443 = FACE_OUTER_BOUND ( 'NONE', #55082, .T. ) ;
#4444 = DIRECTION ( 'NONE',  ( -0.000000000000000000, -0.000000000000000000, 1.000000000000000000 ) ) ;
#4445 =( BOUNDED_CURVE ( )  B_SPLINE_CURVE ( 2, ( #30532, #911, #12141, #46738, #53115, #29791, #11758 ),
 .UNSPECIFIED., .F., .T. ) 
 B_SPLINE_CURVE_WITH_KNOTS ( ( 3, 2, 2, 3 ),
 ( 0.6250000000000003331, 0.6319444444444446418, 0.6388888888888890616, 0.6458333333333334814 ),
 .UNSPECIFIED. ) 
 CURVE ( )  GEOMETRIC_REPRESENTATION_ITEM ( )  RATIONAL_B_SPLINE_CURVE ( ( 0.9999999999999935607, 0.8660254037844451469, 1.000000000000000000, 0.8660254037844387076, 1.000000000000000000, 0.8660254037844365982, 1.000000000000002220 ) ) 
 REPRESENTATION_ITEM ( '' )  );
#4446 = FACE_OUTER_BOUND ( 'NONE', #31443, .T. ) ;
#4447 = FACE_OUTER_BOUND ( 'NONE', #40989, .T. ) ;
#4448 = FACE_OUTER_BOUND ( 'NONE', #26548, .T. ) ;
#4449 = AXIS2_PLACEMENT_3D ( 'NONE', #52576, #63881, #7088 ) ;
#4450 = CARTESIAN_POINT ( 'NONE',  ( 95.00000000000000000, -213.0599564267049857, 86.98374999999998636 ) ) ;
#4451 = VERTEX_POINT ( 'NONE', #11667 ) ;
#4452 = DIRECTION ( 'NONE',  ( -1.000000000000000000, 0.000000000000000000, -0.000000000000000000 ) ) ;
#4453 = ORIENTED_EDGE ( 'NONE', *, *, #65373, .F. ) ;
#4454 = EDGE_LOOP ( 'NONE', ( #26529, #56816, #23611, #27016 ) ) ;
#4455 = CARTESIAN_POINT ( 'NONE',  ( 13.83832728059186046, -142.6495187161941089, 5.500000000000000000 ) ) ;
#4456 = ADVANCED_FACE ( 'NONE', ( #6065 ), #35708, .T. ) ;
#4457 = EDGE_CURVE ( 'NONE', #8687, #55876, #23340, .T. ) ;
#4458 = AXIS2_PLACEMENT_3D ( 'NONE', #14119, #43096, #25784 ) ;
#4459 =( LENGTH_UNIT ( ) NAMED_UNIT ( * ) SI_UNIT ( .MILLI., .METRE. ) );
#4460 = CARTESIAN_POINT ( 'NONE',  ( 0.000000000000000000, -3.894527615417340272, -81.90746397400393164 ) ) ;
#4461 = VERTEX_POINT ( 'NONE', #23702 ) ;
#4462 = CARTESIAN_POINT ( 'NONE',  ( 92.35000000010806787, -209.9999848944895007, 78.64888723592486031 ) ) ;
#4463 = CARTESIAN_POINT ( 'NONE',  ( 92.35000000000000853, -209.9999999999999716, 80.55437500173430010 ) ) ;
#4464 = CARTESIAN_POINT ( 'NONE',  ( 93.67499999999998295, 92.29496732002878900, 82.27416666666665890 ) ) ;
#4465 = EDGE_LOOP ( 'NONE', ( #58724, #69348, #48995, #19993 ) ) ;
#4466 = DIRECTION ( 'NONE',  ( 0.000000000000000000, 0.3090169943749412340, 0.9510565162951556406 ) ) ;
#4467 = ORIENTED_EDGE ( 'NONE', *, *, #48547, .T. ) ;
#4468 = CARTESIAN_POINT ( 'NONE',  ( 0.000000000000000000, 0.000000000000000000, 0.000000000000000000 ) ) ;
#4469 = EDGE_LOOP ( 'NONE', ( #27550, #28544, #35900, #23981 ) ) ;
#4470 = CARTESIAN_POINT ( 'NONE',  ( 0.000000000000000000, 35.91791733033570466, -68.67312586194960033 ) ) ;
#4471 = CARTESIAN_POINT ( 'NONE',  ( -97.30629616937501680, 88.66845928578038638, 82.86947916753379673 ) ) ;
#4472 = CARTESIAN_POINT ( 'NONE',  ( 93.84685191531248449, 88.00268892867053694, 77.68364583420047609 ) ) ;
#4473 = ORIENTED_EDGE ( 'NONE', *, *, #49381, .T. ) ;
#4474 = FACE_OUTER_BOUND ( 'NONE', #12027, .T. ) ;
#4475 = DIRECTION ( 'NONE',  ( -1.000000000000000000, -0.000000000000000000, -0.000000000000000000 ) ) ;
#4476 = CARTESIAN_POINT ( 'NONE',  ( 0.000000000000000000, 0.000000000000000000, 0.000000000000000000 ) ) ;
#4477 = DIRECTION ( 'NONE',  ( -1.000000000000000000, -0.000000000000000000, 0.000000000000000000 ) ) ;
#4478 = ORIENTED_EDGE ( 'NONE', *, *, #7311, .F. ) ;
#4479 = DIRECTION ( 'NONE',  ( -1.000000000000000000, -0.000000000000000000, -0.000000000000000000 ) ) ;
#4480 = CARTESIAN_POINT ( 'NONE',  ( -94.99999999999997158, -207.3369185715606307, 81.86406250086714920 ) ) ;
#4481 = ORIENTED_EDGE ( 'NONE', *, *, #4684, .T. ) ;
#4482 = EDGE_LOOP ( 'NONE', ( #60567, #58334, #36925, #2709 ) ) ;
#4483 = DIRECTION ( 'NONE',  ( 0.000000000000000000, -0.000000000000000000, -1.000000000000000000 ) ) ;
#4484 = ORIENTED_EDGE ( 'NONE', *, *, #3277, .T. ) ;
#4485 = LINE ( 'NONE', #15363, #4789 ) ;
#4486 = FACE_OUTER_BOUND ( 'NONE', #74137, .T. ) ;
#4487 = VERTEX_POINT ( 'NONE', #46638 ) ;
#4488 = CARTESIAN_POINT ( 'NONE',  ( -92.69370383062498320, -208.6684592857803011, 74.77322916753379900 ) ) ;
#4489 = EDGE_LOOP ( 'NONE', ( #46240, #12111, #67970, #67216 ) ) ;
#4490 = LINE ( 'NONE', #15001, #50657 ) ;
#4491 = AXIS2_PLACEMENT_3D ( 'NONE', #368, #13797, #36740 ) ;
#4492 = CARTESIAN_POINT ( 'NONE',  ( 0.000000000000000000, 16.65560815589411092, 38.55633173627015253 ) ) ;
#4493 = CARTESIAN_POINT ( 'NONE',  ( 0.000000000000000000, -75.16055320797016748, -18.89407956138335365 ) ) ;
#4494 = CARTESIAN_POINT ( 'NONE',  ( 10.00000000000000000, 0.000000000000000000, 0.000000000000000000 ) ) ;
#4495 = AXIS2_PLACEMENT_3D ( 'NONE', #43658, #38374, #61315 ) ;
#4496 = CARTESIAN_POINT ( 'NONE',  ( 11.99999999999999822, -28.89263327155796190, 71.91182617369179297 ) ) ;
#4497 = AXIS2_PLACEMENT_3D ( 'NONE', #65055, #41729, #25549 ) ;
#4498 = CARTESIAN_POINT ( 'NONE',  ( -97.65000000000001990, 90.00000000000004263, 89.36499999999999488 ) ) ;
#4499 = CARTESIAN_POINT ( 'NONE',  ( 92.69370383062498320, 88.66845928578035796, 88.42572916753381662 ) ) ;
#4500 = ADVANCED_FACE ( 'NONE', ( #63940 ), #35362, .T. ) ;
#4501 = VECTOR ( 'NONE', #45288, 1000.000000000000000 ) ;
#4502 = CARTESIAN_POINT ( 'NONE',  ( -10.00000000000000000, 0.000000000000000000, 0.000000000000000000 ) ) ;
#4503 = CARTESIAN_POINT ( 'NONE',  ( 96.32499999999998863, 87.70503267997126784, 81.40104166840096411 ) ) ;
#4504 = DIRECTION ( 'NONE',  ( 0.000000000000000000, 0.000000000000000000, 1.000000000000000000 ) ) ;
#4505 = LINE ( 'NONE', #71776, #60422 ) ;
#4506 = EDGE_CURVE ( 'NONE', #71815, #43675, #27859, .T. ) ;
#4507 = DIRECTION ( 'NONE',  ( -1.000000000000000000, 0.000000000000000000, 0.000000000000000000 ) ) ;
#4508 = CYLINDRICAL_SURFACE ( 'NONE', #5942, 31.99999999999999289 ) ;
#4509 = LINE ( 'NONE', #17258, #65123 ) ;
#4510 = EDGE_CURVE ( 'NONE', #33146, #2617, #36823, .T. ) ;
#4511 = CARTESIAN_POINT ( 'NONE',  ( 11.99999999999999822, -31.47745569255189224, 68.26794271651249346 ) ) ;
#4512 = DIRECTION ( 'NONE',  ( 0.000000000000000000, 0.000000000000000000, 1.000000000000000000 ) ) ;
#4513 = EDGE_CURVE ( 'NONE', #67963, #12692, #37216, .T. ) ;
#4514 = FACE_OUTER_BOUND ( 'NONE', #12098, .T. ) ;
#4515 = DIRECTION ( 'NONE',  ( 0.000000000000000000, 0.9510565162951523099, 0.3090169943749517811 ) ) ;
#4516 = DIRECTION ( 'NONE',  ( -1.000000000000000000, 0.000000000000000000, 0.000000000000000000 ) ) ;
#4517 = VECTOR ( 'NONE', #28646, 1000.000000000000000 ) ;
#4518 = EDGE_CURVE ( 'NONE', #39945, #5325, #48483, .T. ) ;
#4519 = CARTESIAN_POINT ( 'NONE',  ( -97.64999999999994884, -211.5299782133524502, 84.97291666666666288 ) ) ;
#4520 = AXIS2_PLACEMENT_3D ( 'NONE', #62533, #11009, #73406 ) ;
#4521 = CARTESIAN_POINT ( 'NONE',  ( 0.000000000000000000, 0.000000000000000000, -20.00000000000000000 ) ) ;
#4522 = EDGE_CURVE ( 'NONE', #21534, #43826, #73468, .T. ) ;
#4523 = DIRECTION ( 'NONE',  ( 0.000000000000000000, 0.000000000000000000, 1.000000000000000000 ) ) ;
#4524 = LINE ( 'NONE', #61285, #1095 ) ;
#4525 = SURFACE_STYLE_USAGE ( .BOTH. , #56392 ) ;
#4526 = CARTESIAN_POINT ( 'NONE',  ( 97.64999999999999147, -209.9999999999999716, 85.23749999999999716 ) ) ;
#4527 = CARTESIAN_POINT ( 'NONE',  ( 93.84685191531249870, -208.0026889286704943, 89.69572916753382685 ) ) ;
#4528 = EDGE_LOOP ( 'NONE', ( #12096, #4752, #50982, #43232 ) ) ;
#4529 = VERTEX_POINT ( 'NONE', #70652 ) ;
#4530 = EDGE_CURVE ( 'NONE', #68973, #52875, #3026, .T. ) ;
#4531 = CARTESIAN_POINT ( 'NONE',  ( -12.49999999999999645, 0.000000000000000000, 53.20000000000001705 ) ) ;
#4532 = ADVANCED_FACE ( 'NONE', ( #7157 ), #13528, .T. ) ;
#4533 = CARTESIAN_POINT ( 'NONE',  ( 0.000000000000000000, 0.8828120875905820508, -37.48860685352290290 ) ) ;
#4534 = EDGE_LOOP ( 'NONE', ( #47252, #6336, #57708, #44476 ) ) ;
#4535 = CARTESIAN_POINT ( 'NONE',  ( 0.000000000000000000, 0.000000000000000000, 42.00000000000001421 ) ) ;
#4536 = CARTESIAN_POINT ( 'NONE',  ( 92.69370383062501162, -209.9999999999999716, 78.84781250086714977 ) ) ;
#4537 = VECTOR ( 'NONE', #73302, 1000.000000000000000 ) ;
#4538 = ORIENTED_EDGE ( 'NONE', *, *, #61867, .T. ) ;
#4539 = CARTESIAN_POINT ( 'NONE',  ( 97.30629616937498838, -209.9999999999999716, 86.30906250086715659 ) ) ;
#4540 = AXIS2_PLACEMENT_3D ( 'NONE', #9660, #43887, #60438 ) ;
#4541 = ORIENTED_EDGE ( 'NONE', *, *, #18001, .F. ) ;
#4542 = CARTESIAN_POINT ( 'NONE',  ( 1.301042606982605321E-15, 5.773502691896264416, -5.553418012614792509 ) ) ;
#4543 = EDGE_LOOP ( 'NONE', ( #52155, #56620, #25910, #2241 ) ) ;
#4544 = CARTESIAN_POINT ( 'NONE',  ( -92.69370383062502583, 88.66845928578038638, 75.46114583420049371 ) ) ;
#4545 = CONICAL_SURFACE ( 'NONE', #57339, 14.53333333333331545, 0.3490658503988688377 ) ;
#4546 = VERTEX_POINT ( 'NONE', #31183 ) ;
#4547 = CARTESIAN_POINT ( 'NONE',  ( -6.880223345695647197, -142.5202692415819854, 5.500000000000000000 ) ) ;
#4548 = AXIS2_PLACEMENT_3D ( 'NONE', #59057, #13182, #12803 ) ;
#4549 = ORIENTED_EDGE ( 'NONE', *, *, #28533, .F. ) ;
#4550 = CARTESIAN_POINT ( 'NONE',  ( -97.65000000000001990, 90.00000000000004263, 77.29999999999999716 ) ) ;
#4551 = CARTESIAN_POINT ( 'NONE',  ( 93.67500000000001137, -207.7050326799711968, 88.70354166840097321 ) ) ;
#4552 = VERTEX_POINT ( 'NONE', #8639 ) ;
#4553 = DIRECTION ( 'NONE',  ( 0.000000000000000000, 0.000000000000000000, -1.000000000000000000 ) ) ;
#4554 = ORIENTED_EDGE ( 'NONE', *, *, #68957, .T. ) ;
#4555 = DIRECTION ( 'NONE',  ( -0.000000000000000000, -0.000000000000000000, -1.000000000000000000 ) ) ;
#4556 = ORIENTED_EDGE ( 'NONE', *, *, #26728, .T. ) ;
#4557 = ORIENTED_EDGE ( 'NONE', *, *, #66619, .T. ) ;
#4558 = VERTEX_POINT ( 'NONE', #47380 ) ;
#4559 = CARTESIAN_POINT ( 'NONE',  ( 95.00000000000000000, -207.3369185715606307, 75.51406250086714067 ) ) ;
#4560 = ITEM_DEFINED_TRANSFORMATION ( 'NONE', 'NONE', #50815,  #43395 ) ;
#4561 = DIRECTION ( 'NONE',  ( 0.000000000000000000, 0.000000000000000000, 1.000000000000000000 ) ) ;
#4562 = EDGE_LOOP ( 'NONE', ( #37373, #61114, #9038, #63480 ) ) ;
#4563 = CIRCLE ( 'NONE', #44206, 16.00000000000000000 ) ;
#4564 = ORIENTED_EDGE ( 'NONE', *, *, #35656, .F. ) ;
#4565 = AXIS2_PLACEMENT_3D ( 'NONE', #45059, #16479, #56721 ) ;
#4566 = ORIENTED_EDGE ( 'NONE', *, *, #65697, .F. ) ;
#4567 = CARTESIAN_POINT ( 'NONE',  ( 6.377742925735834234, -145.7647898336708181, 5.500000000000000000 ) ) ;
#4568 = DIRECTION ( 'NONE',  ( -0.000000000000000000, -1.000000000000000000, -0.000000000000000000 ) ) ;
#4569 = AXIS2_PLACEMENT_3D ( 'NONE', #6286, #1041, #34845 ) ;
#4570 = VECTOR ( 'NONE', #45189, 1000.000000000000114 ) ;
#4571 = CARTESIAN_POINT ( 'NONE',  ( -93.33920801875069628, 88.39975876321990711, 74.80065669543250806 ) ) ;
#4572 = ADVANCED_FACE ( 'NONE', ( #53387 ), #7888, .T. ) ;
#4573 = VERTEX_POINT ( 'NONE', #25186 ) ;
#4574 = CARTESIAN_POINT ( 'NONE',  ( 97.30629616937498838, 91.33154071421968467, 78.58322916753381548 ) ) ;
#4575 = VECTOR ( 'NONE', #68501, 1000.000000000000000 ) ;
#4576 = VERTEX_POINT ( 'NONE', #54134 ) ;
#4577 = CARTESIAN_POINT ( 'NONE',  ( 10.00000000000000000, 0.000000000000000000, 0.000000000000000000 ) ) ;
#4578 = ORIENTED_EDGE ( 'NONE', *, *, #42854, .T. ) ;
#4579 = CARTESIAN_POINT ( 'NONE',  ( 2.381231458764692110, -4.398698068175666442, -0.5078976954043025183 ) ) ;
#4580 = DIRECTION ( 'NONE',  ( 0.000000000000000000, 8.881784197001252323E-16, 1.000000000000000000 ) ) ;
#4581 = CARTESIAN_POINT ( 'NONE',  ( -92.34999999999999432, -210.0000000255707278, 84.04687500080852658 ) ) ;
#4582 = CARTESIAN_POINT ( 'NONE',  ( -97.30629616937497417, -208.6684592857803295, 79.42989583420047950 ) ) ;
#4583 = DIRECTION ( 'NONE',  ( -0.000000000000000000, 0.000000000000000000, 1.000000000000000000 ) ) ;
#4584 = DIRECTION ( 'NONE',  ( 0.000000000000000000, -0.9876883405951359940, -0.1564344650402420267 ) ) ;
#4585 = CARTESIAN_POINT ( 'NONE',  ( 0.000000000000000000, 5.939536975864662969E-16, -4.700000000000000178 ) ) ;
#4586 = VERTEX_POINT ( 'NONE', #20272 ) ;
#4587 = EDGE_LOOP ( 'NONE', ( #54556, #11819, #45649, #6919 ) ) ;
#4588 = DIRECTION ( 'NONE',  ( -1.000000000000000000, 0.000000000000000000, 0.000000000000000000 ) ) ;
#4589 = EDGE_CURVE ( 'NONE', #32411, #35173, #59400, .T. ) ;
#4590 = CARTESIAN_POINT ( 'NONE',  ( 93.67499999999998295, 92.29496732002878900, 84.81416666666666515 ) ) ;
#4591 = EDGE_CURVE ( 'NONE', #66007, #3283, #55451, .T. ) ;
#4592 = CARTESIAN_POINT ( 'NONE',  ( 92.69400202757779539, -209.0535479562711600, 74.89836836546776055 ) ) ;
#4593 = CARTESIAN_POINT ( 'NONE',  ( -93.84685191531252713, 88.00268892867056536, 80.32947916753380468 ) ) ;
#4594 = DIRECTION ( 'NONE',  ( -1.000000000000000000, -0.000000000000000000, 0.000000000000000000 ) ) ;
#4595 = LINE ( 'NONE', #44062, #43459 ) ;
#4596 = VECTOR ( 'NONE', #57520, 1000.000000000000000 ) ;
#4597 = ORIENTED_EDGE ( 'NONE', *, *, #71131, .T. ) ;
#4598 =( GEOMETRIC_REPRESENTATION_CONTEXT ( 3 ) GLOBAL_UNCERTAINTY_ASSIGNED_CONTEXT ( ( #6034 ) ) GLOBAL_UNIT_ASSIGNED_CONTEXT ( ( #60719, #43805, #49782 ) ) REPRESENTATION_CONTEXT ( 'NONE', 'WORKASPACE' ) );
#4599 = AXIS2_PLACEMENT_3D ( 'NONE', #42041, #64977, #13455 ) ;
#4600 = ADVANCED_FACE ( 'NONE', ( #41727 ), #43237, .F. ) ;
#4601 = ADVANCED_FACE ( 'NONE', ( #48844 ), #66162, .F. ) ;
#4602 = DIRECTION ( 'NONE',  ( -1.000000000000000000, -0.000000000000000000, 0.000000000000000000 ) ) ;
#4603 = DIRECTION ( 'NONE',  ( -0.000000000000000000, -0.000000000000000000, 1.000000000000000000 ) ) ;
#4605 = CIRCLE ( 'NONE', #29793, 77.49899999999999523 ) ;
#4604 = DIRECTION ( 'NONE',  ( -1.000000000000000000, -0.000000000000000000, -0.000000000000000000 ) ) ;
#4606 = LINE ( 'NONE', #9852, #48955 ) ;
#4607 = CARTESIAN_POINT ( 'NONE',  ( -93.67499999999998295, -207.7050326799711968, 79.07270833506763097 ) ) ;
#4608 = CARTESIAN_POINT ( 'NONE',  ( -92.69370383062498320, -209.9999999999999716, 78.05406250086716113 ) ) ;
#4609 = AXIS2_PLACEMENT_3D ( 'NONE', #43719, #49336, #66995 ) ;
#4610 = DIRECTION ( 'NONE',  ( -1.000000000000000000, -0.000000000000000000, -0.000000000000000000 ) ) ;
#4611 = ORIENTED_EDGE ( 'NONE', *, *, #21739, .T. ) ;
#4612 = EDGE_CURVE ( 'NONE', #52257, #7655, #14637, .T. ) ;
#4613 = DIRECTION ( 'NONE',  ( -1.000000000000000000, -0.000000000000000000, -0.000000000000000000 ) ) ;
#4614 = CARTESIAN_POINT ( 'NONE',  ( -96.32500000000001705, 87.70503267997129626, 80.66020833506763665 ) ) ;
#4615 = FACE_OUTER_BOUND ( 'NONE', #18932, .T. ) ;
#4616 = ORIENTED_EDGE ( 'NONE', *, *, #60012, .T. ) ;
#4617 = DIRECTION ( 'NONE',  ( 0.000000000000000000, 0.000000000000000000, 1.000000000000000000 ) ) ;
#4618 = DIRECTION ( 'NONE',  ( 0.000000000000000000, -0.1045284632676558301, -0.9945218953682731788 ) ) ;
#4619 = CIRCLE ( 'NONE', #38245, 31.99999999999999289 ) ;
#4620 = UNCERTAINTY_MEASURE_WITH_UNIT (LENGTH_MEASURE( 1.000000000000000082E-05 ), #71885, 'distance_accuracy_value', 'NONE');
#4621 = VECTOR ( 'NONE', #15272, 1000.000000000000114 ) ;
#4623 = CYLINDRICAL_SURFACE ( 'NONE', #45172, 77.49899999999999523 ) ;
#4622 = AXIS2_PLACEMENT_3D ( 'NONE', #11804, #47155, #52405 ) ;
#4624 = ORIENTED_EDGE ( 'NONE', *, *, #32987, .T. ) ;
#4625 = EDGE_CURVE ( 'NONE', #63684, #13514, #39903, .T. ) ;
#4626 = LINE ( 'NONE', #15507, #62479 ) ;
#4627 = LINE ( 'NONE', #33531, #46307 ) ;
#4628 = ORIENTED_EDGE ( 'NONE', *, *, #34209, .T. ) ;
#4629 = CIRCLE ( 'NONE', #43054, 37.49900000000000233 ) ;
#4630 = CARTESIAN_POINT ( 'NONE',  ( 93.84685191531251292, -211.9973110713294489, 87.84364583420047268 ) ) ;
#4631 = EDGE_CURVE ( 'NONE', #21975, #60113, #59039, .T. ) ;
#4632 = VERTEX_POINT ( 'NONE', #53752 ) ;
#4633 = DIRECTION ( 'NONE',  ( -1.000000000000000000, 0.000000000000000000, 0.000000000000000000 ) ) ;
#4634 = ORIENTED_EDGE ( 'NONE', *, *, #42625, .T. ) ;
#4635 = CARTESIAN_POINT ( 'NONE',  ( -48.80839716909612491, -10.37454508288793065, -5.500000000000000000 ) ) ;
#4636 = ORIENTED_EDGE ( 'NONE', *, *, #59330, .T. ) ;
#4637 = CARTESIAN_POINT ( 'NONE',  ( -20.62008904684763166, -131.2721749321093512, -2.500000000000000000 ) ) ;
#4638 = ORIENTED_EDGE ( 'NONE', *, *, #34806, .T. ) ;
#4639 = ORIENTED_EDGE ( 'NONE', *, *, #25137, .F. ) ;
#4640 = VERTEX_POINT ( 'NONE', #10478 ) ;
#4641 = CARTESIAN_POINT ( 'NONE',  ( 4.999999999999999112, 40.98264845739763018, -9.188173127306860977 ) ) ;
#4642 = ORIENTED_EDGE ( 'NONE', *, *, #10287, .T. ) ;
#4643 = ORIENTED_EDGE ( 'NONE', *, *, #52705, .T. ) ;
#4644 = CARTESIAN_POINT ( 'NONE',  ( 94.99999999999998579, 87.33691857156068750, 77.26031250086714408 ) ) ;
#4645 = DIRECTION ( 'NONE',  ( -1.000000000000000000, 0.000000000000000000, -0.000000000000000000 ) ) ;
#4646 = CARTESIAN_POINT ( 'NONE',  ( 95.00000000000000000, -209.9999999999999716, 90.00000000000000000 ) ) ;
#4647 = CIRCLE ( 'NONE', #61088, 31.99999999999999289 ) ;
#4648 = ORIENTED_EDGE ( 'NONE', *, *, #28854, .F. ) ;
#4649 = VECTOR ( 'NONE', #69948, 1000.000000000000000 ) ;
#4650 = EDGE_LOOP ( 'NONE', ( #11852, #64157, #68463, #41870 ) ) ;
#4651 = ORIENTED_EDGE ( 'NONE', *, *, #73424, .F. ) ;
#4652 = CARTESIAN_POINT ( 'NONE',  ( 94.99999999999998579, 92.66308142843935514, 88.21406250086714351 ) ) ;
#4653 = ORIENTED_EDGE ( 'NONE', *, *, #69543, .F. ) ;
#4654 = CARTESIAN_POINT ( 'NONE',  ( 96.15314808468748708, -208.0026889286704943, 84.98614583420047097 ) ) ;
#4655 = DIRECTION ( 'NONE',  ( -1.000000000000000000, -0.000000000000000000, 0.000000000000000000 ) ) ;
#4656 = CONICAL_SURFACE ( 'NONE', #25025, 5.000000000000000888, 1.047197551196596299 ) ;
#4657 = CARTESIAN_POINT ( 'NONE',  ( -93.67500000000003979, 92.29496732002878900, 77.16770833506762983 ) ) ;
#4658 = CARTESIAN_POINT ( 'NONE',  ( 0.000000000000000000, 0.000000000000000000, 125.0000000000000000 ) ) ;
#4659 = VECTOR ( 'NONE', #44360, 1000.000000000000000 ) ;
#4660 = DIRECTION ( 'NONE',  ( 1.000000000000000000, 0.000000000000000000, 0.000000000000000000 ) ) ;
#4661 = CARTESIAN_POINT ( 'NONE',  ( 1.499592026101426168, -120.0349822133818094, -2.500000000000000000 ) ) ;
#4662 = FACE_OUTER_BOUND ( 'NONE', #24144, .T. ) ;
#4663 = CARTESIAN_POINT ( 'NONE',  ( -97.30629616937497417, -208.6684592857803011, 87.04989583420048405 ) ) ;
#4664 = CARTESIAN_POINT ( 'NONE',  ( -97.30629616937501680, 91.33154071421968467, 85.93864583420048575 ) ) ;
#4665 = ORIENTED_EDGE ( 'NONE', *, *, #33113, .T. ) ;
#4667 = CARTESIAN_POINT ( 'NONE',  ( -97.30629616937501680, 91.33154071421968467, 85.77989583420048803 ) ) ;
#4666 = CARTESIAN_POINT ( 'NONE',  ( 97.30629616937498838, 91.33154071421968467, 89.37822916753381719 ) ) ;
#4668 = ORIENTED_EDGE ( 'NONE', *, *, #30390, .T. ) ;
#4669 = CARTESIAN_POINT ( 'NONE',  ( 11.99999999999999822, -8.830959090341869100, -74.65491531819127147 ) ) ;
#4670 = CARTESIAN_POINT ( 'NONE',  ( -92.34999999999999432, -211.5299782133524218, 80.81895833506763438 ) ) ;
#4671 = CARTESIAN_POINT ( 'NONE',  ( 0.000000000000000000, 12.93880638057313703, 76.41127070299276625 ) ) ;
#4672 = DIRECTION ( 'NONE',  ( -1.000000000000000000, -0.000000000000000000, -0.000000000000000000 ) ) ;
#4673 = CARTESIAN_POINT ( 'NONE',  ( -92.69370383062498320, -209.9999999999999716, 88.69031250086715090 ) ) ;
#4674 = CARTESIAN_POINT ( 'NONE',  ( -97.65000000000001990, 90.00000000000004263, 90.00000000000000000 ) ) ;
#4675 = EDGE_CURVE ( 'NONE', #52450, #18128, #7523, .T. ) ;
#4676 = PLANE ( 'NONE',  #26590 ) ;
#4677 = LINE ( 'NONE', #51633, #26259 ) ;
#4678 = VERTEX_POINT ( 'NONE', #32286 ) ;
#4679 = VECTOR ( 'NONE', #40232, 1000.000000000000000 ) ;
#4680 = VERTEX_POINT ( 'NONE', #27775 ) ;
#4681 = EDGE_CURVE ( 'NONE', #590, #53279, #72233, .T. ) ;
#4682 = AXIS2_PLACEMENT_3D ( 'NONE', #52695, #1243, #25594 ) ;
#4683 = CARTESIAN_POINT ( 'NONE',  ( -95.00000000000002842, 93.05995642670501411, 82.22124999999999773 ) ) ;
#4684 = EDGE_CURVE ( 'NONE', #28756, #67162, #44713, .T. ) ;
#4685 = FACE_OUTER_BOUND ( 'NONE', #13111, .T. ) ;
#4686 = DIRECTION ( 'NONE',  ( -1.000000000000000000, -0.000000000000000000, -0.000000000000000000 ) ) ;
#4687 = DIRECTION ( 'NONE',  ( -1.000000000000000000, 0.000000000000000000, 0.000000000000000000 ) ) ;
#4688 = CARTESIAN_POINT ( 'NONE',  ( -0.0004442498507136653329, 0.001194404164628348752, -70.59999999999999432 ) ) ;
#4689 = LINE ( 'NONE', #15941, #27928 ) ;
#4690 = CARTESIAN_POINT ( 'NONE',  ( -10.00000000000000000, 0.000000000000000000, 0.000000000000000000 ) ) ;
#4691 = DIRECTION ( 'NONE',  ( 1.000000000000000000, 0.000000000000000000, 0.000000000000000000 ) ) ;
#4692 =( BOUNDED_CURVE ( )  B_SPLINE_CURVE ( 2, ( #58874, #6981, #64145, #14093, #37043, #70128, #19371 ),
 .UNSPECIFIED., .F., .F. ) 
 B_SPLINE_CURVE_WITH_KNOTS ( ( 3, 2, 2, 3 ),
 ( 0.8958333333333331483, 0.9027777777777775681, 0.9097222222222218768, 0.9166666666666662966 ),
 .UNSPECIFIED. ) 
 CURVE ( )  GEOMETRIC_REPRESENTATION_ITEM ( )  RATIONAL_B_SPLINE_CURVE ( ( 1.000000000000004219, 0.8660254037844343777, 1.000000000000000000, 0.8660254037844387076, 1.000000000000000000, 0.8660254037844451469, 0.9999999999999935607 ) ) 
 REPRESENTATION_ITEM ( '' )  );
#4693 = ORIENTED_EDGE ( 'NONE', *, *, #27120, .F. ) ;
#4694 = CARTESIAN_POINT ( 'NONE',  ( -92.69370383062502583, 91.33154071421968467, 80.48822916753383083 ) ) ;
#4695 = EDGE_CURVE ( 'NONE', #59768, #27866, #73254, .T. ) ;
#4696 = DIRECTION ( 'NONE',  ( 0.9997280174009349762, -0.02332147558787674158, 0.000000000000000000 ) ) ;
#4697 = CARTESIAN_POINT ( 'NONE',  ( 10.00000000000000000, 6.555932627142952995, -37.01155633439051940 ) ) ;
#4698 = DIRECTION ( 'NONE',  ( 0.000000000000000000, 1.000000000000000000, 0.000000000000000000 ) ) ;
#4699 = DIRECTION ( 'NONE',  ( 0.000000000000000000, 0.000000000000000000, 1.000000000000000000 ) ) ;
#4700 = CYLINDRICAL_SURFACE ( 'NONE', #54500, 31.99999999999999289 ) ;
#4701 = CARTESIAN_POINT ( 'NONE',  ( -93.84685191531248449, -208.0026889286704943, 88.95489583420049939 ) ) ;
#4702 = AXIS2_PLACEMENT_3D ( 'NONE', #39515, #74078, #66952 ) ;
#4703 = EDGE_CURVE ( 'NONE', #12767, #38196, #66297, .T. ) ;
#4704 = VECTOR ( 'NONE', #44882, 1000.000000000000000 ) ;
#4705 = EDGE_CURVE ( 'NONE', #30043, #52797, #26653, .T. ) ;
#4706 = CARTESIAN_POINT ( 'NONE',  ( 92.69370383062498320, 91.33154071421968467, 80.85864583420048746 ) ) ;
#4707 = EDGE_CURVE ( 'NONE', #53279, #27772, #48256, .T. ) ;
#4708 = AXIS2_PLACEMENT_3D ( 'NONE', #50936, #23482, #46794 ) ;
#4709 = VECTOR ( 'NONE', #60900, 1000.000000000000000 ) ;
#4710 = CARTESIAN_POINT ( 'NONE',  ( -93.84685191531248449, -208.0026889286704943, 78.79489583420048859 ) ) ;
#4711 = CARTESIAN_POINT ( 'NONE',  ( 11.99999999999999822, 0.000000000000000000, 0.000000000000000000 ) ) ;
#4712 = ORIENTED_EDGE ( 'NONE', *, *, #4083, .F. ) ;
#4713 = CARTESIAN_POINT ( 'NONE',  ( 10.00000000000000000, 0.000000000000000000, 0.000000000000000000 ) ) ;
#4714 = DIRECTION ( 'NONE',  ( 0.000000000000000000, -0.000000000000000000, 1.000000000000000000 ) ) ;
#4715 = CARTESIAN_POINT ( 'NONE',  ( 10.00000000000000000, -0.8828120875898013420, -37.48860685352291711 ) ) ;
#4716 = CIRCLE ( 'NONE', #34682, 16.00000000000000000 ) ;
#4717 = VECTOR ( 'NONE', #6370, 1000.000000000000000 ) ;
#4718 = CARTESIAN_POINT ( 'NONE',  ( -92.69370383062504004, 90.00000000000004263, 78.05406250086716113 ) ) ;
#4719 = CARTESIAN_POINT ( 'NONE',  ( 97.30629616937498838, -211.3315407142195852, 80.38239583420049428 ) ) ;
#4720 = EDGE_LOOP ( 'NONE', ( #43881, #62723, #19486, #53336 ) ) ;
#4721 = EDGE_CURVE ( 'NONE', #63684, #72004, #4490, .T. ) ;
#4722 = CARTESIAN_POINT ( 'NONE',  ( -35.50000000000000711, -120.0000000000000000, -5.500000000000000000 ) ) ;
#4723 = EDGE_LOOP ( 'NONE', ( #17058, #45039, #72051 ) ) ;
#4724 = DIRECTION ( 'NONE',  ( 1.000000000000000000, 0.000000000000000000, 0.000000000000000000 ) ) ;
#4725 = ORIENTED_EDGE ( 'NONE', *, *, #35646, .T. ) ;
#4726 = VECTOR ( 'NONE', #73917, 1000.000000000000000 ) ;
#4727 = CARTESIAN_POINT ( 'NONE',  ( -97.65000000000004832, -208.4700217866475214, 83.59708333333334451 ) ) ;
#4728 = VECTOR ( 'NONE', #3792, 1000.000000000000000 ) ;
#4729 = VECTOR ( 'NONE', #50882, 1000.000000000000000 ) ;
#4730 = ORIENTED_EDGE ( 'NONE', *, *, #27899, .F. ) ;
#4731 = VERTEX_POINT ( 'NONE', #45081 ) ;
#4732 = ORIENTED_EDGE ( 'NONE', *, *, #8407, .T. ) ;
#4733 = CIRCLE ( 'NONE', #37140, 77.49900000000000944 ) ;
#4734 = CARTESIAN_POINT ( 'NONE',  ( 93.84685191531249870, -208.0026889286704943, 76.36072916753381890 ) ) ;
#4735 = ORIENTED_EDGE ( 'NONE', *, *, #8430, .T. ) ;
#4736 =( REPRESENTATION_RELATIONSHIP ('NONE','NONE', #31117, #49787 ) REPRESENTATION_RELATIONSHIP_WITH_TRANSFORMATION ( #60590 )SHAPE_REPRESENTATION_RELATIONSHIP( ) );
#4737 = CARTESIAN_POINT ( 'NONE',  ( 10.00000000000000000, 70.53064760720316428, -26.01480285779861035 ) ) ;
#4738 = CARTESIAN_POINT ( 'NONE',  ( 15.00000000000000000, -0.9646360437372099028, 23.52805723605590771 ) ) ;
#4739 = CARTESIAN_POINT ( 'NONE',  ( 97.30629616937498838, 91.33154071421968467, 86.36197916753383197 ) ) ;
#4740 = DIRECTION ( 'NONE',  ( 1.000000000000000000, 0.000000000000000000, 0.000000000000000000 ) ) ;
#4741 = CARTESIAN_POINT ( 'NONE',  ( 92.35000000000002274, -208.4700217866474645, 78.51708333333334622 ) ) ;
#4742 = ORIENTED_EDGE ( 'NONE', *, *, #39248, .F. ) ;
#4743 = ORIENTED_EDGE ( 'NONE', *, *, #63274, .T. ) ;
#4744 = ORIENTED_EDGE ( 'NONE', *, *, #8488, .F. ) ;
#4745 = ORIENTED_EDGE ( 'NONE', *, *, #22268, .T. ) ;
#4746 = CARTESIAN_POINT ( 'NONE',  ( 10.00000000000000000, 21.32104025579114648, 30.84782396557224970 ) ) ;
#4747 = CARTESIAN_POINT ( 'NONE',  ( -12.50000000000000000, 1.530808498934191521E-15, -4.400000000000001243 ) ) ;
#4748 = CARTESIAN_POINT ( 'NONE',  ( 10.00000000000000000, -27.13269053701114331, 25.88420570971391754 ) ) ;
#4749 = DIRECTION ( 'NONE',  ( 0.000000000000000000, 0.000000000000000000, 1.000000000000000000 ) ) ;
#4750 = CARTESIAN_POINT ( 'NONE',  ( 0.000000000000000000, 0.000000000000000000, 0.000000000000000000 ) ) ;
#4751 = CARTESIAN_POINT ( 'NONE',  ( 0.000000000000000000, -77.19088730480518734, -6.903761155838607166 ) ) ;
#4752 = ORIENTED_EDGE ( 'NONE', *, *, #36804, .T. ) ;
#4753 = CARTESIAN_POINT ( 'NONE',  ( -97.64999999999996305, -209.9999999999999716, 81.18937500173430521 ) ) ;
#4754 = VERTEX_POINT ( 'NONE', #8999 ) ;
#4755 = CYLINDRICAL_SURFACE ( 'NONE', #12267, 31.99999999999999289 ) ;
#4756 = ORIENTED_EDGE ( 'NONE', *, *, #4117, .T. ) ;
#4758 = CARTESIAN_POINT ( 'NONE',  ( -97.65000000000001990, 90.00000000000004263, 83.72937500173429726 ) ) ;
#4757 = CARTESIAN_POINT ( 'NONE',  ( 97.64999999999997726, 91.52997821335252127, 84.09979166840095388 ) ) ;
#4759 = AXIS2_PLACEMENT_3D ( 'NONE', #47824, #43324, #3107 ) ;
#4760 = ORIENTED_EDGE ( 'NONE', *, *, #67736, .T. ) ;
#4761 = CARTESIAN_POINT ( 'NONE',  ( 92.69370383062498320, 88.66845928578037217, 83.50447916753383026 ) ) ;
#4762 = CARTESIAN_POINT ( 'NONE',  ( -96.32499999999996021, -207.7050326799711968, 86.71916666666666629 ) ) ;
#4763 = AXIS2_PLACEMENT_3D ( 'NONE', #43745, #73772, #33928 ) ;
#4764 = CARTESIAN_POINT ( 'NONE',  ( -89.99999999999998579, -124.0000000000000142, -40.00000000000002132 ) ) ;
#4765 = AXIS2_PLACEMENT_3D ( 'NONE', #20948, #43172, #55168 ) ;
#4766 = EDGE_CURVE ( 'NONE', #30680, #18834, #38651, .T. ) ;
#4767 = CARTESIAN_POINT ( 'NONE',  ( -95.00000000000002842, 90.00000000000004263, 90.00000000000000000 ) ) ;
#4768 = CARTESIAN_POINT ( 'NONE',  ( 97.65000000000000568, 91.52997821335252127, 81.55979166840097605 ) ) ;
#4769 = CIRCLE ( 'NONE', #9571, 12.49999999999999822 ) ;
#4770 = CARTESIAN_POINT ( 'NONE',  ( 10.00000000000000000, -34.94270380257693631, 74.18225833017875459 ) ) ;
#4771 = ORIENTED_EDGE ( 'NONE', *, *, #69406, .T. ) ;
#4772 = DIRECTION ( 'NONE',  ( -0.000000000000000000, 0.1045284632676559550, -0.9945218953682731788 ) ) ;
#4773 = DIRECTION ( 'NONE',  ( -1.000000000000000000, 0.000000000000000000, 0.000000000000000000 ) ) ;
#4774 = DIRECTION ( 'NONE',  ( 1.000000000000000000, 0.000000000000000000, 0.000000000000000000 ) ) ;
#4775 = ORIENTED_EDGE ( 'NONE', *, *, #9395, .F. ) ;
#4776 = EDGE_CURVE ( 'NONE', #1966, #43631, #31922, .T. ) ;
#4777 = ORIENTED_EDGE ( 'NONE', *, *, #38167, .T. ) ;
#4778 = EDGE_CURVE ( 'NONE', #22408, #58433, #16125, .T. ) ;
#4779 = VECTOR ( 'NONE', #23199, 1000.000000000000000 ) ;
#4780 = EDGE_CURVE ( 'NONE', #9094, #31764, #25449, .T. ) ;
#4781 = DIRECTION ( 'NONE',  ( -0.000000000000000000, -0.000000000000000000, 1.000000000000000000 ) ) ;
#4782 = CARTESIAN_POINT ( 'NONE',  ( -96.32500000000001705, 87.70503267997129626, 80.02520833506763154 ) ) ;
#4783 = CARTESIAN_POINT ( 'NONE',  ( 5.000000000000000000, -26.79245525562690844, -32.34446384430000876 ) ) ;
#4784 = EDGE_CURVE ( 'NONE', #36276, #32331, #35053, .T. ) ;
#4785 = CARTESIAN_POINT ( 'NONE',  ( -97.30629616937497417, -211.3315407142195852, 81.59947916753381492 ) ) ;
#4786 = ORIENTED_EDGE ( 'NONE', *, *, #5636, .T. ) ;
#4787 = FACE_BOUND ( 'NONE', #26242, .T. ) ;
#4788 = ORIENTED_EDGE ( 'NONE', *, *, #64050, .T. ) ;
#4789 = VECTOR ( 'NONE', #48838, 1000.000000000000000 ) ;
#4790 = EDGE_CURVE ( 'NONE', #54282, #37558, #36228, .T. ) ;
#4791 = DIRECTION ( 'NONE',  ( 1.000000000000000000, 0.000000000000000000, 0.000000000000000000 ) ) ;
#4792 = VECTOR ( 'NONE', #58107, 1000.000000000000000 ) ;
#4793 = LINE ( 'NONE', #21290, #39538 ) ;
#4794 = LINE ( 'NONE', #56657, #38165 ) ;
#4795 = CARTESIAN_POINT ( 'NONE',  ( 10.00000000000000000, -14.66109333815513160, 73.73191006444567108 ) ) ;
#4796 = DIRECTION ( 'NONE',  ( -1.000000000000000000, -0.000000000000000000, -0.000000000000000000 ) ) ;
#4797 = CARTESIAN_POINT ( 'NONE',  ( 0.000000000000000000, -120.0000000000000000, 2.500000000000000000 ) ) ;
#4798 = DIRECTION ( 'NONE',  ( 1.000000000000000000, -0.000000000000000000, 0.000000000000000000 ) ) ;
#4799 = DIRECTION ( 'NONE',  ( -1.000000000000000000, -0.000000000000000000, 0.000000000000000000 ) ) ;
#4800 = CARTESIAN_POINT ( 'NONE',  ( 2.499999999999984457, -73.00000000000001421, -208.2999999999999261 ) ) ;
#4801 = CARTESIAN_POINT ( 'NONE',  ( 11.99999999999999822, 55.38113227695783536, 54.21277698773694453 ) ) ;
#4802 = DIRECTION ( 'NONE',  ( 1.000000000000000000, 0.000000000000000000, 0.000000000000000000 ) ) ;
#4803 = EDGE_CURVE ( 'NONE', #17390, #70908, #9740, .T. ) ;
#4804 = DIRECTION ( 'NONE',  ( -1.000000000000000000, -0.000000000000000000, -0.000000000000000000 ) ) ;
#4805 = CARTESIAN_POINT ( 'NONE',  ( 12.50000000000000000, -107.5000000000000000, 2.500000000000000000 ) ) ;
#4806 = CARTESIAN_POINT ( 'NONE',  ( 92.34999999999993747, 91.52997821335250705, 89.31208333333333371 ) ) ;
#4807 = VERTEX_POINT ( 'NONE', #27017 ) ;
#4808 = CARTESIAN_POINT ( 'NONE',  ( -92.69370383062504004, 90.00000000000004263, 79.80031250086713612 ) ) ;
#4809 = EDGE_CURVE ( 'NONE', #30790, #33107, #61758, .T. ) ;
#4810 = EDGE_CURVE ( 'NONE', #32525, #38945, #2686, .T. ) ;
#4811 = LINE ( 'NONE', #44653, #21320 ) ;
#4812 = EDGE_CURVE ( 'NONE', #5732, #30754, #5607, .T. ) ;
#4813 = ORIENTED_EDGE ( 'NONE', *, *, #52101, .F. ) ;
#4815 = CARTESIAN_POINT ( 'NONE',  ( -7.400000000000013678, -1.437934995148992251E-13, -12.50000000000023093 ) ) ;
#4814 = AXIS2_PLACEMENT_3D ( 'NONE', #7524, #7885, #59036 ) ;
#4816 = LINE ( 'NONE', #32970, #33573 ) ;
#4817 = CARTESIAN_POINT ( 'NONE',  ( 0.000000000000000000, 36.72794159290241822, 65.59268652807223532 ) ) ;
#4818 = VECTOR ( 'NONE', #15183, 1000.000000000000000 ) ;
#4819 = CIRCLE ( 'NONE', #48049, 42.00000000000000000 ) ;
#4820 = CARTESIAN_POINT ( 'NONE',  ( 97.64999999999999147, -210.0000000198592716, 85.95187500101400246 ) ) ;
#4821 = CARTESIAN_POINT ( 'NONE',  ( 97.30629616937498838, -209.9999999999999716, 76.14906250086716000 ) ) ;
#4822 = ORIENTED_EDGE ( 'NONE', *, *, #8818, .T. ) ;
#4823 = EDGE_LOOP ( 'NONE', ( #70800, #29051, #11659, #42017 ) ) ;
#4824 = LINE ( 'NONE', #21711, #40453 ) ;
#4825 = FACE_OUTER_BOUND ( 'NONE', #45978, .T. ) ;
#4826 = CARTESIAN_POINT ( 'NONE',  ( -97.64999999950698850, -210.0000320324311076, 85.63541623677365067 ) ) ;
#4827 = DIRECTION ( 'NONE',  ( -1.000000000000000000, 0.000000000000000000, 0.000000000000000000 ) ) ;
#4828 = FACE_OUTER_BOUND ( 'NONE', #65834, .T. ) ;
#4829 = CIRCLE ( 'NONE', #24027, 16.00000000000000000 ) ;
#4830 = CARTESIAN_POINT ( 'NONE',  ( 96.32499999999998863, -207.7050326799711968, 87.88333333333332575 ) ) ;
#4831 = ORIENTED_EDGE ( 'NONE', *, *, #62916, .T. ) ;
#4832 = CARTESIAN_POINT ( 'NONE',  ( 92.34999999999999432, 90.00000000000002842, 90.00000000000000000 ) ) ;
#4833 = ORIENTED_EDGE ( 'NONE', *, *, #12635, .T. ) ;
#4834 = AXIS2_PLACEMENT_3D ( 'NONE', #13457, #6716, #40938 ) ;
#4835 = EDGE_LOOP ( 'NONE', ( #72208, #13219, #66492, #60132 ) ) ;
#4836 = CARTESIAN_POINT ( 'NONE',  ( 0.000000000000000000, -27.75498641678764855, 31.52238457039590358 ) ) ;
#4837 = CIRCLE ( 'NONE', #13229, 37.49900000000000233 ) ;
#4838 = AXIS2_PLACEMENT_3D ( 'NONE', #67813, #28317, #34336 ) ;
#4839 = CARTESIAN_POINT ( 'NONE',  ( 0.000000000000000000, -15.48615015657610527, 39.04073710021338428 ) ) ;
#4840 = AXIS2_PLACEMENT_3D ( 'NONE', #39585, #62532, #67026 ) ;
#4841 = VERTEX_POINT ( 'NONE', #33787 ) ;
#4842 = CARTESIAN_POINT ( 'NONE',  ( -92.34999999999999432, -210.0000000983656605, 80.23687499810813506 ) ) ;
#4843 = CARTESIAN_POINT ( 'NONE',  ( 95.00000000000000000, -206.9400435732949575, 80.39562500173431658 ) ) ;
#4845 = AXIS2_PLACEMENT_3D ( 'NONE', #32784, #54988, #49350 ) ;
#4844 = CARTESIAN_POINT ( 'NONE',  ( 94.99999999999998579, 86.94004357329500010, 81.26874999999999716 ) ) ;
#4846 = ORIENTED_EDGE ( 'NONE', *, *, #59697, .F. ) ;
#4847 = DIRECTION ( 'NONE',  ( 1.000000000000000000, -0.000000000000000000, -0.000000000000000000 ) ) ;
#4848 = ORIENTED_EDGE ( 'NONE', *, *, #49124, .F. ) ;
#4849 = CARTESIAN_POINT ( 'NONE',  ( 5.999999999999999112, -74.74816331893453025, 33.71516098798714722 ) ) ;
#4850 = EDGE_LOOP ( 'NONE', ( #36781, #6697, #23042, #734 ) ) ;
#4851 = CARTESIAN_POINT ( 'NONE',  ( 11.99999999999999822, -75.11725578898466438, -2.956366410621452001 ) ) ;
#4852 = CARTESIAN_POINT ( 'NONE',  ( -95.00000000000002842, 87.33691857156074434, 84.88031250086713442 ) ) ;
#4853 = CARTESIAN_POINT ( 'NONE',  ( 96.15314808468748708, 91.99731107132950569, 79.90614583420047268 ) ) ;
#4854 = VERTEX_POINT ( 'NONE', #69477 ) ;
#4855 = CARTESIAN_POINT ( 'NONE',  ( -0.0004442498512760095037, 0.001194404164628348752, -49.00000000000000000 ) ) ;
#4856 = CARTESIAN_POINT ( 'NONE',  ( 0.000000000000000000, -65.64334221924882229, -41.19522573413803457 ) ) ;
#4857 = CARTESIAN_POINT ( 'NONE',  ( 11.99999999999999822, 49.70050353004889132, 59.46389618801982380 ) ) ;
#4858 = ADVANCED_FACE ( 'NONE', ( #11225 ), #28889, .T. ) ;
#4859 = LINE ( 'NONE', #40159, #28726 ) ;
#4860 = ORIENTED_EDGE ( 'NONE', *, *, #45851, .F. ) ;
#4861 = DIRECTION ( 'NONE',  ( -0.02332147558787823691, -0.9997280174009349762, 0.000000000000000000 ) ) ;
#4862 = CARTESIAN_POINT ( 'NONE',  ( -96.15314808468747287, -208.0026889286704943, 76.83697916753381207 ) ) ;
#4863 = ORIENTED_EDGE ( 'NONE', *, *, #62424, .F. ) ;
#4864 = EDGE_CURVE ( 'NONE', #46823, #55642, #23619, .T. ) ;
#4865 = ORIENTED_EDGE ( 'NONE', *, *, #70498, .T. ) ;
#4866 = CARTESIAN_POINT ( 'NONE',  ( 92.34999999999996589, 88.47002178664753558, 79.89291666666666458 ) ) ;
#4867 = EDGE_CURVE ( 'NONE', #23574, #50963, #22895, .T. ) ;
#4868 = ADVANCED_FACE ( 'NONE', ( #29241 ), #62763, .T. ) ;
#4869 = ORIENTED_EDGE ( 'NONE', *, *, #31668, .T. ) ;
#4870 = DIRECTION ( 'NONE',  ( 0.000000000000000000, 0.8660254037844384856, 0.5000000000000004441 ) ) ;
#4871 = CARTESIAN_POINT ( 'NONE',  ( -2.977765906491215642, 1.885622467823562354E-15, 15.39727592589476579 ) ) ;
#4872 = ORIENTED_EDGE ( 'NONE', *, *, #52524, .T. ) ;
#4873 = CARTESIAN_POINT ( 'NONE',  ( -97.30629616937497417, -208.6684592857803011, 77.52489583420046415 ) ) ;
#4874 = EDGE_LOOP ( 'NONE', ( #43949, #50686, #42365, #54032 ) ) ;
#4875 = CARTESIAN_POINT ( 'NONE',  ( 94.99999999999998579, 93.05995642670504253, 88.65062500173428361 ) ) ;
#4876 = FACE_OUTER_BOUND ( 'NONE', #11519, .T. ) ;
#4877 = CARTESIAN_POINT ( 'NONE',  ( 0.000000000000000000, 1.467624384280025174, -2.542000000000001592 ) ) ;
#4878 = CARTESIAN_POINT ( 'NONE',  ( 10.00000000000000000, 0.000000000000000000, 0.000000000000000000 ) ) ;
#4879 = VECTOR ( 'NONE', #35632, 1000.000000000000000 ) ;
#4880 = CARTESIAN_POINT ( 'NONE',  ( 0.000000000000000000, -35.92658777277502935, -10.74501242461320594 ) ) ;
#4881 = AXIS2_PLACEMENT_3D ( 'NONE', #69394, #17893, #8094 ) ;
#4882 = SURFACE_STYLE_FILL_AREA ( #17249 ) ;
#4884 = CARTESIAN_POINT ( 'NONE',  ( 97.30629616937498838, 90.00000000000002842, 84.24531250086714351 ) ) ;
#4883 = VECTOR ( 'NONE', #50976, 1000.000000000000000 ) ;
#4885 = DIRECTION ( 'NONE',  ( 1.000000000000000000, 0.000000000000000000, -0.000000000000000000 ) ) ;
#4886 = CARTESIAN_POINT ( 'NONE',  ( -92.34999999999999432, -209.9999998456625860, 79.60187500750915035 ) ) ;
#4887 = DIRECTION ( 'NONE',  ( 0.000000000000000000, 0.7071067811865487940, -0.7071067811865462405 ) ) ;
#4888 = DIRECTION ( 'NONE',  ( -1.000000000000000000, 5.236901059551556403E-15, 2.618450529775778123E-14 ) ) ;
#4889 = EDGE_CURVE ( 'NONE', #24772, #16853, #3841, .T. ) ;
#4890 = CARTESIAN_POINT ( 'NONE',  ( 10.00000000000000000, 51.03279382321088065, 55.19960302592086521 ) ) ;
#4891 = DIRECTION ( 'NONE',  ( -1.000000000000000000, 1.047380211910311281E-14, 2.618450529775778123E-14 ) ) ;
#4892 = LINE ( 'NONE', #49963, #37491 ) ;
#4893 = DIRECTION ( 'NONE',  ( -1.000000000000000000, -0.000000000000000000, -0.000000000000000000 ) ) ;
#4894 = CARTESIAN_POINT ( 'NONE',  ( 10.00000000000000000, 73.44644590900094272, -24.73286445877628026 ) ) ;
#4895 = AXIS2_PLACEMENT_3D ( 'NONE', #50606, #51731, #10389 ) ;
#4896 = CARTESIAN_POINT ( 'NONE',  ( -7.543218489614351263, -11.91259227951415056, 0.000000000000000000 ) ) ;
#4897 = CARTESIAN_POINT ( 'NONE',  ( 10.00000000000000000, 0.000000000000000000, 0.000000000000000000 ) ) ;
#4898 = AXIS2_PLACEMENT_3D ( 'NONE', #60949, #15833, #20359 ) ;
#4899 = EDGE_CURVE ( 'NONE', #26229, #19675, #35399, .T. ) ;
#4900 = EDGE_CURVE ( 'NONE', #71560, #20201, #53085, .T. ) ;
#4901 = DIRECTION ( 'NONE',  ( 0.000000000000000000, 0.000000000000000000, 1.000000000000000000 ) ) ;
#4902 = CARTESIAN_POINT ( 'NONE',  ( -96.32499999999996021, -207.7050326799711968, 84.81416666666666515 ) ) ;
#4903 = AXIS2_PLACEMENT_3D ( 'NONE', #40235, #68815, #57903 ) ;
#4904 =( BOUNDED_CURVE ( )  B_SPLINE_CURVE ( 2, ( #65978, #20083, #66346, #49025, #59969, #3206, #2486 ),
 .UNSPECIFIED., .F., .F. ) 
 B_SPLINE_CURVE_WITH_KNOTS ( ( 3, 2, 2, 3 ),
 ( 0.1458333333333334536, 0.1527777777777778734, 0.1597222222222222654, 0.1666666666666666852 ),
 .UNSPECIFIED. ) 
 CURVE ( )  GEOMETRIC_REPRESENTATION_ITEM ( )  RATIONAL_B_SPLINE_CURVE ( ( 0.9999999999999978906, 0.8660254037844408170, 1.000000000000000000, 0.8660254037844387076, 1.000000000000000000, 0.8660254037844381525, 1.000000000000000444 ) ) 
 REPRESENTATION_ITEM ( '' )  );
#4905 = PLANE ( 'NONE',  #40732 ) ;
#4906 = DIRECTION ( 'NONE',  ( -1.000000000000000000, 0.000000000000000000, -0.000000000000000000 ) ) ;
#4907 = LINE ( 'NONE', #33817, #54603 ) ;
#4908 = CARTESIAN_POINT ( 'NONE',  ( 93.84685191531251292, -211.9973110713294489, 87.36739583420049371 ) ) ;
#4909 = ORIENTED_EDGE ( 'NONE', *, *, #68184, .F. ) ;
#4910 = ORIENTED_EDGE ( 'NONE', *, *, #42193, .T. ) ;
#4911 = DIRECTION ( 'NONE',  ( 0.9827303690289282967, 0.1850432970638667407, -0.000000000000000000 ) ) ;
#4912 = ORIENTED_EDGE ( 'NONE', *, *, #39645, .T. ) ;
#4913 = FACE_OUTER_BOUND ( 'NONE', #54628, .T. ) ;
#4914 = CARTESIAN_POINT ( 'NONE',  ( 97.30629616937498838, -211.3315407142195852, 78.47739583420047893 ) ) ;
#4915 = ORIENTED_EDGE ( 'NONE', *, *, #55685, .F. ) ;
#4916 = CARTESIAN_POINT ( 'NONE',  ( 96.15314808468750130, -211.9973110713294489, 83.66322916753382799 ) ) ;
#4917 = AXIS2_PLACEMENT_3D ( 'NONE', #69766, #19370, #29165 ) ;
#4918 = ORIENTED_EDGE ( 'NONE', *, *, #41592, .F. ) ;
#4919 = CARTESIAN_POINT ( 'NONE',  ( 10.00000000000000000, 0.000000000000000000, 0.000000000000000000 ) ) ;
#4920 = ORIENTED_EDGE ( 'NONE', *, *, #54975, .T. ) ;
#4921 = CIRCLE ( 'NONE', #34910, 82.00000000000000000 ) ;
#4922 = FACE_OUTER_BOUND ( 'NONE', #32370, .T. ) ;
#4923 = LINE ( 'NONE', #23669, #14876 ) ;
#4924 = ORIENTED_EDGE ( 'NONE', *, *, #29692, .F. ) ;
#4925 = DIRECTION ( 'NONE',  ( 0.000000000000000000, 0.000000000000000000, -1.000000000000000000 ) ) ;
#4926 = FACE_OUTER_BOUND ( 'NONE', #14042, .T. ) ;
#4927 = VERTEX_POINT ( 'NONE', #40175 ) ;
#4928 = DIRECTION ( 'NONE',  ( 0.000000000000000000, -0.1564344650402381687, 0.9876883405951365491 ) ) ;
#4929 = ORIENTED_EDGE ( 'NONE', *, *, #41501, .T. ) ;
#4930 = CARTESIAN_POINT ( 'NONE',  ( 10.00000000000000000, 36.72794159290241822, 65.59268652807223532 ) ) ;
#4931 = ORIENTED_EDGE ( 'NONE', *, *, #63199, .T. ) ;
#4932 = EDGE_CURVE ( 'NONE', #65643, #65194, #63129, .T. ) ;
#4933 = CIRCLE ( 'NONE', #1373, 62.50000000000000000 ) ;
#4934 = ORIENTED_EDGE ( 'NONE', *, *, #4522, .F. ) ;
#4935 = VERTEX_POINT ( 'NONE', #46189 ) ;
#4936 = CARTESIAN_POINT ( 'NONE',  ( 93.84685191531249870, -208.0026889286704943, 75.56697916753381605 ) ) ;
#4937 = CIRCLE ( 'NONE', #33732, 16.00000000000000000 ) ;
#4938 = ITEM_DEFINED_TRANSFORMATION ( 'NONE', 'NONE', #22006,  #43395 ) ;
#4939 = LINE ( 'NONE', #54933, #37867 ) ;
#4940 = EDGE_LOOP ( 'NONE', ( #47533, #47636, #13608, #32918 ) ) ;
#4941 = VECTOR ( 'NONE', #37203, 1000.000000000000114 ) ;
#4942 = ORIENTED_EDGE ( 'NONE', *, *, #66718, .T. ) ;
#4943 = ADVANCED_FACE ( 'NONE', ( #35268 ), #58196, .T. ) ;
#4944 = ORIENTED_EDGE ( 'NONE', *, *, #60867, .T. ) ;
#4945 = FACE_OUTER_BOUND ( 'NONE', #3536, .T. ) ;
#4946 = CIRCLE ( 'NONE', #70914, 31.99999999999998224 ) ;
#4947 = LINE ( 'NONE', #11298, #56306 ) ;
#4948 = EDGE_CURVE ( 'NONE', #52639, #15350, #7469, .T. ) ;
#4949 = CARTESIAN_POINT ( 'NONE',  ( -95.00000000000002842, 87.33691857156074434, 75.99031250086716227 ) ) ;
#4950 = VERTEX_POINT ( 'NONE', #29604 ) ;
#4951 = EDGE_LOOP ( 'NONE', ( #55296, #68665, #38832, #49643 ) ) ;
#4952 = SURFACE_SIDE_STYLE ('',( #9080 ) ) ;
#4953 = CARTESIAN_POINT ( 'NONE',  ( -94.99999999999997158, -207.3369185715606307, 85.03906250086714635 ) ) ;
#4955 = ORIENTED_EDGE ( 'NONE', *, *, #72326, .F. ) ;
#4954 = EDGE_CURVE ( 'NONE', #32656, #47166, #58903, .T. ) ;
#4956 = CARTESIAN_POINT ( 'NONE',  ( 96.91640186574987581, -211.8303114255586479, 74.99954695036826990 ) ) ;
#4957 = CARTESIAN_POINT ( 'NONE',  ( 0.000000000000000000, 36.73666225445988687, -65.58780272294035285 ) ) ;
#4958 = CARTESIAN_POINT ( 'NONE',  ( -97.30629616937495996, -209.9999999999999716, 78.84781250086714977 ) ) ;
#4959 = FACE_OUTER_BOUND ( 'NONE', #13933, .T. ) ;
#4960 = DIRECTION ( 'NONE',  ( -1.000000000000000000, 0.000000000000000000, 0.000000000000000000 ) ) ;
#4961 = LINE ( 'NONE', #21854, #11881 ) ;
#4962 = ORIENTED_EDGE ( 'NONE', *, *, #18672, .F. ) ;
#4963 = CARTESIAN_POINT ( 'NONE',  ( 0.000000000000000000, -81.34940948281328588, -10.30890764327469000 ) ) ;
#4964 = CARTESIAN_POINT ( 'NONE',  ( -1.355716935723729089, -119.3581031311870362, -2.500000000000000000 ) ) ;
#4965 = EDGE_CURVE ( 'NONE', #27241, #65977, #17086, .T. ) ;
#4966 = DIRECTION ( 'NONE',  ( -0.000000000000000000, -0.000000000000000000, 1.000000000000000000 ) ) ;
#4967 = EDGE_CURVE ( 'NONE', #72633, #23298, #55048, .T. ) ;
#4968 = CARTESIAN_POINT ( 'NONE',  ( -97.30629616937501680, 91.33154071421968467, 80.69989583420048973 ) ) ;
#4969 = DIRECTION ( 'NONE',  ( 1.000000000000000000, 0.000000000000000000, 0.000000000000000000 ) ) ;
#4970 = CARTESIAN_POINT ( 'NONE',  ( 11.99999999999999822, 0.000000000000000000, 0.000000000000000000 ) ) ;
#4971 = VERTEX_POINT ( 'NONE', #71213 ) ;
#4972 = DIRECTION ( 'NONE',  ( 1.000000000000000000, 0.000000000000000000, 0.000000000000000000 ) ) ;
#4973 = VECTOR ( 'NONE', #29994, 1000.000000000000000 ) ;
#4974 = LINE ( 'NONE', #44066, #35230 ) ;
#4975 = DIRECTION ( 'NONE',  ( -3.061616997868382648E-16, -1.000000000000000000, 0.000000000000000000 ) ) ;
#4976 = EDGE_CURVE ( 'NONE', #52268, #28753, #8460, .T. ) ;
#4977 = DIRECTION ( 'NONE',  ( -1.000000000000000000, 0.000000000000000000, 0.000000000000000000 ) ) ;
#4978 = CARTESIAN_POINT ( 'NONE',  ( -97.65000000000001990, 90.00000000000004263, 90.00000000000000000 ) ) ;
#4979 = AXIS2_PLACEMENT_3D ( 'NONE', #45562, #10573, #21864 ) ;
#4980 = CARTESIAN_POINT ( 'NONE',  ( 97.64999999994533653, -210.0000170172949367, 88.49187441316098557 ) ) ;
#4981 = CARTESIAN_POINT ( 'NONE',  ( -93.84685191531248449, -208.0026889286704943, 80.69989583420047552 ) ) ;
#4982 = CARTESIAN_POINT ( 'NONE',  ( 11.99999999999999822, 60.67117009219215618, -55.16347631942976903 ) ) ;
#4983 = EDGE_LOOP ( 'NONE', ( #43169, #58255, #2871, #36329 ) ) ;
#4984 = CARTESIAN_POINT ( 'NONE',  ( -93.07557990970633455, 88.17815826261617929, 75.00000000000001421 ) ) ;
#4985 = LINE ( 'NONE', #62499, #73098 ) ;
#4986 = CARTESIAN_POINT ( 'NONE',  ( 0.000000000000000000, -11.30684508768284680, -76.66974797899850103 ) ) ;
#4987 = VERTEX_POINT ( 'NONE', #20837 ) ;
#4988 = CARTESIAN_POINT ( 'NONE',  ( 92.34999999999999432, 89.99996514701891215, 77.37937620717863751 ) ) ;
#4989 = CARTESIAN_POINT ( 'NONE',  ( 92.35000000000000853, -209.9999999999999716, 84.92000000000000171 ) ) ;
#4990 = AXIS2_PLACEMENT_3D ( 'NONE', #28690, #5421, #60790 ) ;
#4991 = CIRCLE ( 'NONE', #6226, 15.50000000000000000 ) ;
#4992 = LINE ( 'NONE', #9866, #20406 ) ;
#4993 = ORIENTED_EDGE ( 'NONE', *, *, #43578, .F. ) ;
#4994 = CARTESIAN_POINT ( 'NONE',  ( -96.32500000000001705, 92.29496732002878900, 76.00354166840097037 ) ) ;
#4995 = DIRECTION ( 'NONE',  ( 1.000000000000000000, 0.000000000000000000, 0.000000000000000000 ) ) ;
#4996 = ORIENTED_EDGE ( 'NONE', *, *, #33929, .T. ) ;
#4997 = AXIS2_PLACEMENT_3D ( 'NONE', #59062, #13910, #7556 ) ;
#4998 = CARTESIAN_POINT ( 'NONE',  ( 92.69370383062501162, -211.3315407142195852, 88.42572916753381662 ) ) ;
#4999 = DIRECTION ( 'NONE',  ( 0.000000000000000000, 0.9969173337331281859, -0.07845909572784180719 ) ) ;
#5000 = ORIENTED_EDGE ( 'NONE', *, *, #5384, .T. ) ;
#5001 = EDGE_CURVE ( 'NONE', #59827, #71846, #68716, .T. ) ;
#5002 = FACE_OUTER_BOUND ( 'NONE', #67402, .T. ) ;
#5003 = ORIENTED_EDGE ( 'NONE', *, *, #30145, .F. ) ;
#5004 = FACE_OUTER_BOUND ( 'NONE', #41187, .T. ) ;
#5005 = ORIENTED_EDGE ( 'NONE', *, *, #25811, .F. ) ;
#5006 = LINE ( 'NONE', #4637, #7197 ) ;
#5007 = ORIENTED_EDGE ( 'NONE', *, *, #29761, .F. ) ;
#5008 = ORIENTED_EDGE ( 'NONE', *, *, #8201, .F. ) ;
#5009 = EDGE_CURVE ( 'NONE', #36701, #2723, #3889, .T. ) ;
#5010 = VERTEX_POINT ( 'NONE', #30999 ) ;
#5011 = CYLINDRICAL_SURFACE ( 'NONE', #8326, 31.99999999999998579 ) ;
#5012 = EDGE_CURVE ( 'NONE', #23404, #8315, #71552, .T. ) ;
#5013 = ORIENTED_EDGE ( 'NONE', *, *, #55166, .F. ) ;
#5014 = PRODUCT_DEFINITION_SHAPE ( 'NONE', 'NONE',  #40833 ) ;
#5015 = ORIENTED_EDGE ( 'NONE', *, *, #35075, .F. ) ;
#5016 = CARTESIAN_POINT ( 'NONE',  ( 92.34999999999999432, 90.00000000000002842, 87.45999999999999375 ) ) ;
#5017 = LINE ( 'NONE', #33182, #46791 ) ;
#5018 = FACE_BOUND ( 'NONE', #34003, .T. ) ;
#5019 = ORIENTED_EDGE ( 'NONE', *, *, #55166, .T. ) ;
#5020 = ADVANCED_FACE ( 'NONE', ( #66710 ), #71588, .T. ) ;
#5021 = ORIENTED_EDGE ( 'NONE', *, *, #5621, .F. ) ;
#5022 = ORIENTED_EDGE ( 'NONE', *, *, #65799, .F. ) ;
#5023 = CARTESIAN_POINT ( 'NONE',  ( 97.30629616937498838, 90.00000000000002842, 88.69031250086715090 ) ) ;
#5024 = ORIENTED_EDGE ( 'NONE', *, *, #6649, .F. ) ;
#5025 = CARTESIAN_POINT ( 'NONE',  ( 95.00000000000000000, -207.3369185715606307, 86.30906250086715659 ) ) ;
#5026 = DIRECTION ( 'NONE',  ( -0.000000000000000000, -0.000000000000000000, 1.000000000000000000 ) ) ;
#5028 = CARTESIAN_POINT ( 'NONE',  ( -12.00000000000000000, 0.000000000000000000, -17.30399999999999849 ) ) ;
#5027 = AXIS2_PLACEMENT_3D ( 'NONE', #69938, #34253, #69581 ) ;
#5029 = CARTESIAN_POINT ( 'NONE',  ( -95.00000000000002842, 93.05995642670504253, 77.85562500173431033 ) ) ;
#5030 = CYLINDRICAL_SURFACE ( 'NONE', #49971, 14.09999999999999964 ) ;
#5031 = DIRECTION ( 'NONE',  ( 0.000000000000000000, 0.000000000000000000, 1.000000000000000000 ) ) ;
#5032 = CARTESIAN_POINT ( 'NONE',  ( 10.00000000000000000, 0.000000000000000000, 0.000000000000000000 ) ) ;
#5033 = CARTESIAN_POINT ( 'NONE',  ( -97.30629616937497417, -211.3315407142195852, 86.52072916753381548 ) ) ;
#5034 = CARTESIAN_POINT ( 'NONE',  ( -95.00000000000002842, 92.66308142843932671, 84.56281250086716739 ) ) ;
#5035 = AXIS2_PLACEMENT_3D ( 'NONE', #4767, #26919, #11123 ) ;
#5036 = ORIENTED_EDGE ( 'NONE', *, *, #11805, .T. ) ;
#5038 = CARTESIAN_POINT ( 'NONE',  ( -92.69370383062502583, 88.66845928578038638, 85.46239583420047836 ) ) ;
#5037 = CARTESIAN_POINT ( 'NONE',  ( 92.69370383062498320, 91.33154071421968467, 86.41489583420047893 ) ) ;
#5039 = ORIENTED_EDGE ( 'NONE', *, *, #64663, .T. ) ;
#5040 = FACE_BOUND ( 'NONE', #44481, .T. ) ;
#5041 = ADVANCED_FACE ( 'NONE', ( #20089 ), #9561, .T. ) ;
#5042 = FACE_OUTER_BOUND ( 'NONE', #32724, .T. ) ;
#5043 = DIRECTION ( 'NONE',  ( 8.090853898039833646E-17, -9.269810975720164453E-17, 1.000000000000000000 ) ) ;
#5044 = DIRECTION ( 'NONE',  ( 0.000000000000000000, 0.000000000000000000, 1.000000000000000000 ) ) ;
#5045 = DIRECTION ( 'NONE',  ( 0.02332147558787822997, 0.9997280174009349762, 0.000000000000000000 ) ) ;
#5046 = CARTESIAN_POINT ( 'NONE',  ( 10.00000000000000000, 36.73666225445894185, 65.58780272294090707 ) ) ;
#5047 = DIRECTION ( 'NONE',  ( 0.000000000000000000, 0.5877852522924683631, 0.8090169943749510040 ) ) ;
#5048 = CARTESIAN_POINT ( 'NONE',  ( -13.05994868825747446, -139.5943292883446532, -5.500000000000000000 ) ) ;
#5049 = VECTOR ( 'NONE', #15711, 1000.000000000000000 ) ;
#5050 = CARTESIAN_POINT ( 'NONE',  ( 11.99999999999999822, -2.946379043145784582, -75.11764819372150725 ) ) ;
#5051 = ORIENTED_EDGE ( 'NONE', *, *, #50820, .T. ) ;
#5052 = AXIS2_PLACEMENT_3D ( 'NONE', #1449, #701, #36713 ) ;
#5053 = EDGE_LOOP ( 'NONE', ( #16686, #40975, #46032, #69757 ) ) ;
#5054 = CARTESIAN_POINT ( 'NONE',  ( -95.00000000000002842, 93.05995642670501411, 82.85625000000000284 ) ) ;
#5055 = ADVANCED_FACE ( 'NONE', ( #25739, #66350 ), #9186, .F. ) ;
#5056 = CARTESIAN_POINT ( 'NONE',  ( -2.499999999999970690, 73.00000000000001421, -208.2999999999999545 ) ) ;
#5057 = EDGE_CURVE ( 'NONE', #66402, #69599, #37412, .T. ) ;
#5058 = CYLINDRICAL_SURFACE ( 'NONE', #44187, 2.649999999999985700 ) ;
#5059 = DIRECTION ( 'NONE',  ( 0.000000000000000000, 0.000000000000000000, -1.000000000000000000 ) ) ;
#5060 = CARTESIAN_POINT ( 'NONE',  ( -93.67499999999998295, -212.2949673200287179, 76.95604166840095672 ) ) ;
#5061 = DIRECTION ( 'NONE',  ( -1.000000000000000000, 0.000000000000000000, 0.000000000000000000 ) ) ;
#5062 = DIRECTION ( 'NONE',  ( 1.000000000000000000, 0.000000000000000000, 0.000000000000000000 ) ) ;
#5063 = CARTESIAN_POINT ( 'NONE',  ( -94.99999999999997158, -206.9400435732949575, 79.68124999999999147 ) ) ;
#5064 = EDGE_CURVE ( 'NONE', #12875, #64628, #26844, .T. ) ;
#5065 = ORIENTED_EDGE ( 'NONE', *, *, #45505, .F. ) ;
#5066 = CARTESIAN_POINT ( 'NONE',  ( -96.15314808468751551, 88.00268892867056536, 78.95364583420047211 ) ) ;
#5067 = DIRECTION ( 'NONE',  ( 0.7585478161175723821, 0.6516173805718057377, 0.000000000000000000 ) ) ;
#5068 = LINE ( 'NONE', #63313, #58589 ) ;
#5069 = FACE_OUTER_BOUND ( 'NONE', #24527, .T. ) ;
#5070 = FACE_OUTER_BOUND ( 'NONE', #42634, .T. ) ;
#5071 = DIRECTION ( 'NONE',  ( -1.000000000000000000, 0.000000000000000000, 0.000000000000000000 ) ) ;
#5072 = CARTESIAN_POINT ( 'NONE',  ( -92.69370383062498320, -209.9999999999999716, 89.48406250086715374 ) ) ;
#5073 =( LENGTH_UNIT ( ) NAMED_UNIT ( * ) SI_UNIT ( .MILLI., .METRE. ) );
#5074 = VECTOR ( 'NONE', #17177, 1000.000000000000000 ) ;
#5075 = CARTESIAN_POINT ( 'NONE',  ( 96.15314808468748708, 88.00268892867053694, 80.48822916753381662 ) ) ;
#5076 = CARTESIAN_POINT ( 'NONE',  ( -92.69370383062498320, -211.3315407142195852, 78.63614583420046245 ) ) ;
#5077 = CARTESIAN_POINT ( 'NONE',  ( 10.00000000000000000, 27.13269053701096922, 25.88420570971410228 ) ) ;
#5078 = VERTEX_POINT ( 'NONE', #37775 ) ;
#5079 = COLOUR_RGB ( '', 0.66274510, 0.83137255, 0.94901961) ;
#5080 = CARTESIAN_POINT ( 'NONE',  ( -97.65000000000001990, 90.00000000000004263, 86.90437500173429441 ) ) ;
#5081 = VECTOR ( 'NONE', #56739, 1000.000000000000000 ) ;
#5082 = FACE_OUTER_BOUND ( 'NONE', #19163, .T. ) ;
#5083 = CARTESIAN_POINT ( 'NONE',  ( 19.12409105625795291, -101.5943176906707919, 2.500000000000000000 ) ) ;
#5084 = CIRCLE ( 'NONE', #42317, 37.49900000000000233 ) ;
#5085 = CARTESIAN_POINT ( 'NONE',  ( -93.84685191531252713, 88.00268892867056536, 78.58322916753382970 ) ) ;
#5086 = CARTESIAN_POINT ( 'NONE',  ( 97.30629616937498838, -209.9999999999999716, 79.16531250086714522 ) ) ;
#5087 = ORIENTED_EDGE ( 'NONE', *, *, #25952, .F. ) ;
#5088 = AXIS2_PLACEMENT_3D ( 'NONE', #4494, #54864, #20657 ) ;
#5089 = CARTESIAN_POINT ( 'NONE',  ( 0.000000000000000000, 0.000000000000000000, 0.000000000000000000 ) ) ;
#5090 = ORIENTED_EDGE ( 'NONE', *, *, #38272, .T. ) ;
#5091 = DIRECTION ( 'NONE',  ( -1.000000000000000000, -0.000000000000000000, -0.000000000000000000 ) ) ;
#5092 = VERTEX_POINT ( 'NONE', #49033 ) ;
#5093 = ADVANCED_FACE ( 'NONE', ( #20476 ), #32109, .T. ) ;
#5094 = AXIS2_PLACEMENT_3D ( 'NONE', #26607, #67585, #39391 ) ;
#5095 = CARTESIAN_POINT ( 'NONE',  ( 0.000000000000000000, 54.21277698773752007, -55.38113227695726692 ) ) ;
#5096 = AXIS2_PLACEMENT_3D ( 'NONE', #32089, #26821, #2829 ) ;
#5097 = ORIENTED_EDGE ( 'NONE', *, *, #65471, .T. ) ;
#5098 = EDGE_LOOP ( 'NONE', ( #27168, #7224, #66127, #58066 ) ) ;
#5099 = ADVANCED_FACE ( 'NONE', ( #2492 ), #38129, .T. ) ;
#5100 = ORIENTED_EDGE ( 'NONE', *, *, #58569, .F. ) ;
#5101 = CARTESIAN_POINT ( 'NONE',  ( 96.66078148566039374, -211.6002521295064867, 74.80065602173002048 ) ) ;
#5102 = EDGE_CURVE ( 'NONE', #40486, #17454, #32480, .T. ) ;
#5103 = VERTEX_POINT ( 'NONE', #55425 ) ;
#5104 = FACE_OUTER_BOUND ( 'NONE', #9949, .T. ) ;
#5105 = DIRECTION ( 'NONE',  ( 0.000000000000000000, 0.000000000000000000, -1.000000000000000000 ) ) ;
#5106 = CARTESIAN_POINT ( 'NONE',  ( 96.15314808468748708, 91.99731107132950569, 87.68489583420048916 ) ) ;
#5107 = DIRECTION ( 'NONE',  ( -1.000000000000000000, 0.000000000000000000, -0.000000000000000000 ) ) ;
#5108 = CARTESIAN_POINT ( 'NONE',  ( 95.00000000000000000, -213.0599564267049857, 79.36374999999999602 ) ) ;
#5109 = ORIENTED_EDGE ( 'NONE', *, *, #59353, .T. ) ;
#5110 = ADVANCED_FACE ( 'NONE', ( #70853 ), #37024, .T. ) ;
#5111 = ORIENTED_EDGE ( 'NONE', *, *, #27610, .F. ) ;
#5112 = ORIENTED_EDGE ( 'NONE', *, *, #49124, .T. ) ;
#5113 = VERTEX_POINT ( 'NONE', #32847 ) ;
#5114 = DIRECTION ( 'NONE',  ( -3.035766082959412415E-16, -1.000000000000000000, -0.000000000000000000 ) ) ;
#5115 = LINE ( 'NONE', #73130, #69154 ) ;
#5116 = CARTESIAN_POINT ( 'NONE',  ( 2.117611129180199558, -93.54218975225703048, 2.500000000000000000 ) ) ;
#5117 = CYLINDRICAL_SURFACE ( 'NONE', #69036, 42.00000000000000000 ) ;
#5118 = CARTESIAN_POINT ( 'NONE',  ( 10.00000000000000000, 0.000000000000000000, 0.000000000000000000 ) ) ;
#5119 = CARTESIAN_POINT ( 'NONE',  ( 94.99999999999998579, 86.94004357329502852, 83.88812500173429498 ) ) ;
#5120 = ORIENTED_EDGE ( 'NONE', *, *, #28333, .T. ) ;
#5121 = CARTESIAN_POINT ( 'NONE',  ( -92.34999999999999432, -211.5299782133524502, 83.35895833506762642 ) ) ;
#5122 = ORIENTED_EDGE ( 'NONE', *, *, #31292, .F. ) ;
#5123 = ORIENTED_EDGE ( 'NONE', *, *, #33243, .T. ) ;
#5125 = CARTESIAN_POINT ( 'NONE',  ( -93.67500000000003979, 92.29496732002878900, 79.07270833506763097 ) ) ;
#5124 = CARTESIAN_POINT ( 'NONE',  ( 94.99999999999998579, 93.05995642670504253, 83.57062500173429953 ) ) ;
#5126 =( BOUNDED_CURVE ( )  B_SPLINE_CURVE ( 2, ( #20494, #43808, #21208, #31755, #14844, #65620, #44160 ),
 .UNSPECIFIED., .F., .F. ) 
 B_SPLINE_CURVE_WITH_KNOTS ( ( 3, 2, 2, 3 ),
 ( 0.1666666666666666852, 0.1736111111111111049, 0.1805555555555554970, 0.1874999999999999167 ),
 .UNSPECIFIED. ) 
 CURVE ( )  GEOMETRIC_REPRESENTATION_ITEM ( )  RATIONAL_B_SPLINE_CURVE ( ( 0.9999999999999994449, 0.8660254037844392627, 1.000000000000000000, 0.8660254037844387076, 1.000000000000000000, 0.8660254037844402619, 0.9999999999999984457 ) ) 
 REPRESENTATION_ITEM ( '' )  );
#5127 = ORIENTED_EDGE ( 'NONE', *, *, #3434, .T. ) ;
#5128 = CARTESIAN_POINT ( 'NONE',  ( 97.30629616937498838, 90.00000000000002842, 82.49906250086715431 ) ) ;
#5129 = EDGE_CURVE ( 'NONE', #41007, #12200, #1953, .T. ) ;
#5130 = CARTESIAN_POINT ( 'NONE',  ( 92.34999999999989484, 91.52997821335247863, 83.59708333333334451 ) ) ;
#5131 = CARTESIAN_POINT ( 'NONE',  ( 11.99999999999999822, 75.11764819372149304, 29.05362095685338275 ) ) ;
#5132 = CYLINDRICAL_SURFACE ( 'NONE', #5035, 2.649999999999985700 ) ;
#5133 = CARTESIAN_POINT ( 'NONE',  ( 11.99999999999999822, 39.78640506895698792, -66.50666863321958999 ) ) ;
#5134 = DIRECTION ( 'NONE',  ( 0.000000000000000000, 0.9945218953682731788, -0.1045284632676558162 ) ) ;
#5135 = ORIENTED_EDGE ( 'NONE', *, *, #26144, .T. ) ;
#5136 = DIRECTION ( 'NONE',  ( 1.000000000000000000, 1.427937372958405461E-15, 7.962523111839130290E-16 ) ) ;
#5137 = DIRECTION ( 'NONE',  ( 0.08130631524010120681, -0.9966891607226784355, 0.000000000000000000 ) ) ;
#5138 = DIRECTION ( 'NONE',  ( 0.000000000000000000, 0.000000000000000000, -1.000000000000000000 ) ) ;
#5139 = EDGE_LOOP ( 'NONE', ( #14067, #9558, #45126, #27072 ) ) ;
#5140 = AXIS2_PLACEMENT_3D ( 'NONE', #1694, #47512, #18198 ) ;
#5141 = ORIENTED_EDGE ( 'NONE', *, *, #30022, .T. ) ;
#5142 = FACE_OUTER_BOUND ( 'NONE', #14590, .T. ) ;
#5143 = AXIS2_PLACEMENT_3D ( 'NONE', #51445, #58854, #7 ) ;
#5144 = EDGE_CURVE ( 'NONE', #24191, #27546, #52352, .T. ) ;
#5145 = DIRECTION ( 'NONE',  ( 0.000000000000000000, 0.000000000000000000, -1.000000000000000000 ) ) ;
#5146 = ADVANCED_FACE ( 'NONE', ( #27956 ), #16315, .T. ) ;
#5147 = DIRECTION ( 'NONE',  ( 0.000000000000000000, 0.000000000000000000, 1.000000000000000000 ) ) ;
#5148 = CARTESIAN_POINT ( 'NONE',  ( 10.00000000000000000, 0.000000000000000000, 0.000000000000000000 ) ) ;
#5149 = CIRCLE ( 'NONE', #68782, 31.99999999999998934 ) ;
#5150 = CARTESIAN_POINT ( 'NONE',  ( -97.30629616937497417, -208.6684592857803011, 82.76364583420048859 ) ) ;
#5151 = ORIENTED_EDGE ( 'NONE', *, *, #48297, .F. ) ;
#5152 = DIRECTION ( 'NONE',  ( 0.000000000000000000, 0.000000000000000000, 1.000000000000000000 ) ) ;
#5153 = ORIENTED_EDGE ( 'NONE', *, *, #59149, .T. ) ;
#5154 = CARTESIAN_POINT ( 'NONE',  ( 11.99999999999999822, 0.000000000000000000, 0.000000000000000000 ) ) ;
#5155 = AXIS2_PLACEMENT_3D ( 'NONE', #20479, #19357, #42310 ) ;
#5156 = AXIS2_PLACEMENT_3D ( 'NONE', #61720, #20384, #26749 ) ;
#5157 = CARTESIAN_POINT ( 'NONE',  ( -97.50728577674108521, -210.3406226724060559, 74.92458348457978445 ) ) ;
#5158 = DIRECTION ( 'NONE',  ( 0.000000000000000000, 0.000000000000000000, 1.000000000000000000 ) ) ;
#5159 = CARTESIAN_POINT ( 'NONE',  ( 95.00000000000000000, -209.9999999999999716, 90.00000000000000000 ) ) ;
#5160 = CYLINDRICAL_SURFACE ( 'NONE', #22035, 16.00000000000000000 ) ;
#5161 = DIRECTION ( 'NONE',  ( 0.000000000000000000, 0.000000000000000000, 1.000000000000000000 ) ) ;
#5162 = FACE_OUTER_BOUND ( 'NONE', #11175, .T. ) ;
#5163 = DIRECTION ( 'NONE',  ( 0.000000000000000000, 0.000000000000000000, 1.000000000000000000 ) ) ;
#5164 = DIRECTION ( 'NONE',  ( 0.000000000000000000, 0.000000000000000000, -1.000000000000000000 ) ) ;
#5165 = CARTESIAN_POINT ( 'NONE',  ( 5.000000000000000000, 74.74816331893430288, 33.71516098798768013 ) ) ;
#5166 = DIRECTION ( 'NONE',  ( 0.000000000000000000, 0.000000000000000000, -1.000000000000000000 ) ) ;
#5167 = DIRECTION ( 'NONE',  ( 0.000000000000000000, 0.000000000000000000, 1.000000000000000000 ) ) ;
#5168 = CARTESIAN_POINT ( 'NONE',  ( -93.84685191531248449, -208.0026889286704943, 89.58989583420049030 ) ) ;
#5169 = CARTESIAN_POINT ( 'NONE',  ( 10.00000000000000178, 12.24744871391589207, -2.500000000000000000 ) ) ;
#5170 = ORIENTED_EDGE ( 'NONE', *, *, #10122, .F. ) ;
#5171 = LINE ( 'NONE', #34454, #8829 ) ;
#5172 = CARTESIAN_POINT ( 'NONE',  ( -96.15314808468751551, 88.00268892867056536, 79.58864583420047722 ) ) ;
#5173 = CARTESIAN_POINT ( 'NONE',  ( 0.000000000000000000, -41.76106447765443619, -62.50884508063471401 ) ) ;
#5174 = EDGE_CURVE ( 'NONE', #1439, #47477, #65567, .T. ) ;
#5175 = ORIENTED_EDGE ( 'NONE', *, *, #20763, .F. ) ;
#5176 = CYLINDRICAL_SURFACE ( 'NONE', #28241, 77.49899999999999523 ) ;
#5177 = CARTESIAN_POINT ( 'NONE',  ( -3.000000000000000000, 23.59884966291538078, -12.14883922797231541 ) ) ;
#5178 = LINE ( 'NONE', #22082, #11985 ) ;
#5179 = EDGE_CURVE ( 'NONE', #65292, #28695, #16294, .T. ) ;
#5180 = AXIS2_PLACEMENT_3D ( 'NONE', #58080, #46808, #69724 ) ;
#5181 = CARTESIAN_POINT ( 'NONE',  ( 10.00000000000000000, 17.28742895386084655, 75.54627589209950145 ) ) ;
#5182 = CARTESIAN_POINT ( 'NONE',  ( 92.69370383062501162, -211.3315407142195852, 75.88447916753382572 ) ) ;
#5183 = ADVANCED_FACE ( 'NONE', ( #67445 ), #27198, .T. ) ;
#5184 = AXIS2_PLACEMENT_3D ( 'NONE', #13484, #8955, #36780 ) ;
#5185 = EDGE_LOOP ( 'NONE', ( #13673, #18299, #60395, #6570 ) ) ;
#5186 = EDGE_CURVE ( 'NONE', #58816, #13817, #21110, .T. ) ;
#5187 = ORIENTED_EDGE ( 'NONE', *, *, #5789, .T. ) ;
#5188 = CARTESIAN_POINT ( 'NONE',  ( -92.34999999999999432, -208.4700217866474645, 81.55979166840097605 ) ) ;
#5189 = CARTESIAN_POINT ( 'NONE',  ( 10.00000000000000000, 11.30684508768452545, -76.66974797899825944 ) ) ;
#5190 = CIRCLE ( 'NONE', #17151, 77.49900000000000944 ) ;
#5191 = CARTESIAN_POINT ( 'NONE',  ( 92.34999999999999432, 90.00000000000002842, 90.00000000000000000 ) ) ;
#5192 = CARTESIAN_POINT ( 'NONE',  ( -10.00000000000000000, 0.000000000000000000, 0.000000000000000000 ) ) ;
#5193 = CIRCLE ( 'NONE', #17197, 42.00000000000000000 ) ;
#5194 = CARTESIAN_POINT ( 'NONE',  ( 0.000000000000000000, 0.000000000000000000, 0.000000000000000000 ) ) ;
#5195 = CARTESIAN_POINT ( 'NONE',  ( 95.00000000000000000, -206.9400435732949575, 89.20624999999999716 ) ) ;
#5196 = EDGE_CURVE ( 'NONE', #9195, #74276, #47526, .T. ) ;
#5197 = ORIENTED_EDGE ( 'NONE', *, *, #25289, .T. ) ;
#5198 = DIRECTION ( 'NONE',  ( -1.000000000000000000, 0.000000000000000000, 0.000000000000000000 ) ) ;
#5199 = ORIENTED_EDGE ( 'NONE', *, *, #1774, .T. ) ;
#5200 = AXIS2_PLACEMENT_3D ( 'NONE', #59692, #60805, #31476 ) ;
#5201 = ORIENTED_EDGE ( 'NONE', *, *, #21799, .T. ) ;
#5202 = DIRECTION ( 'NONE',  ( 1.000000000000000000, 0.000000000000000000, 0.000000000000000000 ) ) ;
#5203 = AXIS2_PLACEMENT_3D ( 'NONE', #62774, #10490, #33409 ) ;
#5204 =( NAMED_UNIT ( * ) PLANE_ANGLE_UNIT ( ) SI_UNIT ( $, .RADIAN. ) );
#5205 = CARTESIAN_POINT ( 'NONE',  ( 0.000000000000000000, 0.000000000000000000, 0.000000000000000000 ) ) ;
#5206 = EDGE_LOOP ( 'NONE', ( #33260, #1437, #57752, #63829 ) ) ;
#5207 = FACE_OUTER_BOUND ( 'NONE', #24415, .T. ) ;
#5208 = CARTESIAN_POINT ( 'NONE',  ( 93.67500000000001137, -207.7050326799711968, 76.63854166840096127 ) ) ;
#5209 = CARTESIAN_POINT ( 'NONE',  ( 93.67499999999998295, 92.29496732002878900, 82.90916666666666401 ) ) ;
#5210 = ORIENTED_EDGE ( 'NONE', *, *, #56209, .F. ) ;
#5211 = DIRECTION ( 'NONE',  ( 9.814797785686868941E-17, -1.000000000000000000, 0.000000000000000000 ) ) ;
#5212 = ORIENTED_EDGE ( 'NONE', *, *, #27406, .F. ) ;
#5213 = FACE_BOUND ( 'NONE', #20889, .T. ) ;
#5214 = ADVANCED_FACE ( 'NONE', ( #4685 ), #56920, .F. ) ;
#5215 = EDGE_LOOP ( 'NONE', ( #8543, #50370, #54130, #65513 ) ) ;
#5216 = CARTESIAN_POINT ( 'NONE',  ( -97.65000000000001990, 88.47002178664754979, 88.86229166840097093 ) ) ;
#5217 = CARTESIAN_POINT ( 'NONE',  ( -96.15314808468751551, 88.00268892867056536, 84.19239583420049655 ) ) ;
#5218 = CARTESIAN_POINT ( 'NONE',  ( 97.30629616937498838, 91.33154071421968467, 77.31322916753380525 ) ) ;
#5219 = EDGE_CURVE ( 'NONE', #5960, #20594, #9103, .T. ) ;
#5220 = ORIENTED_EDGE ( 'NONE', *, *, #60553, .F. ) ;
#5221 = CARTESIAN_POINT ( 'NONE',  ( 10.00000000000000000, 16.65560815589464028, -38.55633173626993937 ) ) ;
#5222 = CYLINDRICAL_SURFACE ( 'NONE', #54450, 2.649999999999985700 ) ;
#5223 = CARTESIAN_POINT ( 'NONE',  ( 11.99999999999999822, 0.000000000000000000, 0.000000000000000000 ) ) ;
#5224 = DIRECTION ( 'NONE',  ( -1.000000000000000000, 7.571544473058805744E-15, 2.612289469705706870E-14 ) ) ;
#5225 = ORIENTED_EDGE ( 'NONE', *, *, #49422, .T. ) ;
#5226 = CARTESIAN_POINT ( 'NONE',  ( 0.000000000000000000, 0.000000000000000000, 0.000000000000000000 ) ) ;
#5227 = EDGE_CURVE ( 'NONE', #55546, #26437, #7918, .T. ) ;
#5228 = CARTESIAN_POINT ( 'NONE',  ( -94.99999999999997158, -212.6630814284392557, 78.37156250086714238 ) ) ;
#5229 = ORIENTED_EDGE ( 'NONE', *, *, #61687, .F. ) ;
#5230 = ORIENTED_EDGE ( 'NONE', *, *, #11316, .F. ) ;
#5231 = CARTESIAN_POINT ( 'NONE',  ( 0.000000000000000000, 0.000000000000000000, 0.000000000000000000 ) ) ;
#5232 = ORIENTED_EDGE ( 'NONE', *, *, #67900, .T. ) ;
#5233 = EDGE_CURVE ( 'NONE', #22100, #20743, #33218, .T. ) ;
#5234 = CARTESIAN_POINT ( 'NONE',  ( 94.99999999999998579, 86.94004357329502852, 78.09374999999998579 ) ) ;
#5235 = VECTOR ( 'NONE', #63781, 1000.000000000000000 ) ;
#5236 = DIRECTION ( 'NONE',  ( 0.000000000000000000, 0.000000000000000000, -1.000000000000000000 ) ) ;
#5237 = VERTEX_POINT ( 'NONE', #5056 ) ;
#5238 = CARTESIAN_POINT ( 'NONE',  ( -97.30629616937495996, -209.9999999999999716, 89.80156250086714920 ) ) ;
#5239 = EDGE_LOOP ( 'NONE', ( #16836, #34230, #21273, #30327 ) ) ;
#5240 = DIRECTION ( 'NONE',  ( 0.000000000000000000, 0.000000000000000000, 1.000000000000000000 ) ) ;
#5241 = CARTESIAN_POINT ( 'NONE',  ( -97.65000000000001990, 90.00000000000004263, 90.00000000000000000 ) ) ;
#5242 = DIRECTION ( 'NONE',  ( 0.000000000000000000, -0.9723699203976789995, 0.2334453638558957045 ) ) ;
#5243 = ADVANCED_FACE ( 'NONE', ( #38505 ), #61817, .T. ) ;
#5244 = EDGE_CURVE ( 'NONE', #40498, #64759, #54337, .T. ) ;
#5245 = DIRECTION ( 'NONE',  ( 0.000000000000000000, 0.000000000000000000, 1.000000000000000000 ) ) ;
#5246 = CIRCLE ( 'NONE', #72447, 82.00000000000000000 ) ;
#5247 = CARTESIAN_POINT ( 'NONE',  ( 10.00000000000000000, 27.13269053701132094, -25.88420570971372570 ) ) ;
#5248 = CARTESIAN_POINT ( 'NONE',  ( 93.84685191531248449, 88.00268892867053694, 84.03364583420047040 ) ) ;
#5249 = DIRECTION ( 'NONE',  ( 0.000000000000000000, 0.9945218953682730678, 0.1045284632676570929 ) ) ;
#5250 = DIRECTION ( 'NONE',  ( -2.628368902995175337E-16, -1.000000000000000000, 0.000000000000000000 ) ) ;
#5251 = DIRECTION ( 'NONE',  ( 0.000000000000000000, 0.5224985647159441360, 0.8526401643540952868 ) ) ;
#5252 = CYLINDRICAL_SURFACE ( 'NONE', #51971, 31.99999999999999289 ) ;
#5253 = DIRECTION ( 'NONE',  ( 0.000000000000000000, 0.2334453638558990907, 0.9723699203976781114 ) ) ;
#5254 = DIRECTION ( 'NONE',  ( -1.000000000000000000, 0.000000000000000000, -0.000000000000000000 ) ) ;
#5255 = DIRECTION ( 'NONE',  ( -1.000000000000000000, 0.000000000000000000, 0.000000000000000000 ) ) ;
#5256 = AXIS2_PLACEMENT_3D ( 'NONE', #22374, #15983, #10725 ) ;
#5257 = DIRECTION ( 'NONE',  ( -1.000000000000000000, 0.000000000000000000, 0.000000000000000000 ) ) ;
#5258 = AXIS2_PLACEMENT_3D ( 'NONE', #64695, #70678, #65075 ) ;
#5259 = CARTESIAN_POINT ( 'NONE',  ( 6.509281303079589520, -14.89695620656361008, 0.000000000000000000 ) ) ;
#5260 = DIRECTION ( 'NONE',  ( 1.000000000000000000, -0.000000000000000000, -0.000000000000000000 ) ) ;
#5261 = AXIS2_PLACEMENT_3D ( 'NONE', #15296, #53673, #2214 ) ;
#5262 = CARTESIAN_POINT ( 'NONE',  ( 15.00000000000000000, -22.32062822937469093, 14.36278369418830181 ) ) ;
#5263 = VECTOR ( 'NONE', #37232, 1000.000000000000000 ) ;
#5264 = VECTOR ( 'NONE', #57386, 1000.000000000000000 ) ;
#5265 = DIRECTION ( 'NONE',  ( 0.000000000000000000, -0.8910065241883626808, -0.4539904997395569075 ) ) ;
#5266 = CARTESIAN_POINT ( 'NONE',  ( -97.64999999999994884, -208.4700217866474645, 85.50208333333331723 ) ) ;
#5267 = CARTESIAN_POINT ( 'NONE',  ( 0.000000000000000000, 0.000000000000000000, 0.000000000000000000 ) ) ;
#5268 = ORIENTED_EDGE ( 'NONE', *, *, #30286, .T. ) ;
#5269 = CARTESIAN_POINT ( 'NONE',  ( 0.000000000000000000, 0.000000000000000000, 0.000000000000000000 ) ) ;
#5270 = LINE ( 'NONE', #39092, #21522 ) ;
#5271 = CARTESIAN_POINT ( 'NONE',  ( 10.00000000000000000, 0.000000000000000000, 0.000000000000000000 ) ) ;
#5272 = AXIS2_PLACEMENT_3D ( 'NONE', #12852, #53824, #32641 ) ;
#5273 = CARTESIAN_POINT ( 'NONE',  ( -12.49999999999999645, 0.000000000000000000, -20.00000000000000000 ) ) ;
#5274 = EDGE_CURVE ( 'NONE', #69665, #1704, #28322, .T. ) ;
#5275 = CARTESIAN_POINT ( 'NONE',  ( 93.84685191531249870, -208.0026889286704943, 85.88572916753381037 ) ) ;
#5276 = EDGE_CURVE ( 'NONE', #43742, #6773, #39994, .T. ) ;
#5277 = ORIENTED_EDGE ( 'NONE', *, *, #6145, .T. ) ;
#5278 = EDGE_CURVE ( 'NONE', #71840, #7986, #25890, .T. ) ;
#5279 = ORIENTED_EDGE ( 'NONE', *, *, #59405, .T. ) ;
#5280 = EDGE_CURVE ( 'NONE', #32631, #19363, #55951, .T. ) ;
#5281 = CARTESIAN_POINT ( 'NONE',  ( -3.961125083139900749, -143.2122702051246677, 5.500000000000000000 ) ) ;
#5282 = VERTEX_POINT ( 'NONE', #73067 ) ;
#5283 = AXIS2_PLACEMENT_3D ( 'NONE', #34153, #52176, #51072 ) ;
#5284 = PLANE ( 'NONE',  #58151 ) ;
#5285 = CARTESIAN_POINT ( 'NONE',  ( 97.30629616937498838, -209.9999999999999716, 76.62531250086713897 ) ) ;
#5286 = ORIENTED_EDGE ( 'NONE', *, *, #66475, .F. ) ;
#5287 = CARTESIAN_POINT ( 'NONE',  ( 93.84685191531251292, -211.9973110713294489, 82.92239583420048632 ) ) ;
#5288 = AXIS2_PLACEMENT_3D ( 'NONE', #44072, #66991, #33144 ) ;
#5289 = VERTEX_POINT ( 'NONE', #21570 ) ;
#5290 = DIRECTION ( 'NONE',  ( -7.962523111839282146E-16, 1.065814103640130873E-14, 1.000000000000000000 ) ) ;
#5291 = VERTEX_POINT ( 'NONE', #44526 ) ;
#5292 = ORIENTED_EDGE ( 'NONE', *, *, #65095, .T. ) ;
#5293 = CARTESIAN_POINT ( 'NONE',  ( -97.30629616937501680, 91.33154071421968467, 75.14364583420049826 ) ) ;
#5294 = EDGE_CURVE ( 'NONE', #65590, #20976, #67934, .T. ) ;
#5295 = CARTESIAN_POINT ( 'NONE',  ( 10.00000000000000000, 30.00120703465205452, 22.64427369931179967 ) ) ;
#5296 = ORIENTED_EDGE ( 'NONE', *, *, #28508, .T. ) ;
#5297 = LINE ( 'NONE', #68056, #47341 ) ;
#5298 = CARTESIAN_POINT ( 'NONE',  ( 97.64999999999997726, -208.4700217866474645, 85.36979166840096411 ) ) ;
#5299 = EDGE_CURVE ( 'NONE', #49118, #68933, #12879, .T. ) ;
#5300 = ORIENTED_EDGE ( 'NONE', *, *, #126, .F. ) ;
#5301 = DIRECTION ( 'NONE',  ( 0.9227826878668540234, 0.3853207896976547087, 0.000000000000000000 ) ) ;
#5302 = CIRCLE ( 'NONE', #72451, 77.49900000000000944 ) ;
#5303 = ORIENTED_EDGE ( 'NONE', *, *, #28509, .T. ) ;
#5304 = DIRECTION ( 'NONE',  ( 0.000000000000000000, 0.000000000000000000, -1.000000000000000000 ) ) ;
#5305 = VECTOR ( 'NONE', #19744, 1000.000000000000000 ) ;
#5306 = ORIENTED_EDGE ( 'NONE', *, *, #30784, .T. ) ;
#5307 = ORIENTED_EDGE ( 'NONE', *, *, #68793, .F. ) ;
#5308 = CIRCLE ( 'NONE', #14886, 16.00000000000000355 ) ;
#5309 = VERTEX_POINT ( 'NONE', #6521 ) ;
#5310 = CARTESIAN_POINT ( 'NONE',  ( 92.69370383062501162, -209.9999999999999716, 75.03781250086713328 ) ) ;
#5311 = EDGE_CURVE ( 'NONE', #28632, #47641, #35501, .T. ) ;
#5313 = ADVANCED_FACE ( 'NONE', ( #53120 ), #41466, .T. ) ;
#5312 = AXIS2_PLACEMENT_3D ( 'NONE', #30093, #42874, #65070 ) ;
#5314 = FACE_OUTER_BOUND ( 'NONE', #25079, .T. ) ;
#5315 = ORIENTED_EDGE ( 'NONE', *, *, #26233, .F. ) ;
#5316 = ORIENTED_EDGE ( 'NONE', *, *, #19427, .F. ) ;
#5317 = ORIENTED_EDGE ( 'NONE', *, *, #5543, .T. ) ;
#5318 = LINE ( 'NONE', #67708, #47931 ) ;
#5319 = CARTESIAN_POINT ( 'NONE',  ( -97.30629616937501680, 91.33154071421968467, 75.77864583420048916 ) ) ;
#5320 = ORIENTED_EDGE ( 'NONE', *, *, #3333, .F. ) ;
#5321 = CARTESIAN_POINT ( 'NONE',  ( 96.15314808468748708, 88.00268892867053694, 75.24947916753380639 ) ) ;
#5322 = ORIENTED_EDGE ( 'NONE', *, *, #53876, .T. ) ;
#5323 = DIRECTION ( 'NONE',  ( 0.000000000000000000, 0.000000000000000000, 1.000000000000000000 ) ) ;
#5324 = CARTESIAN_POINT ( 'NONE',  ( -94.99999999999997158, -212.6630814284392557, 84.72156250086713669 ) ) ;
#5325 = VERTEX_POINT ( 'NONE', #24542 ) ;
#5326 = CARTESIAN_POINT ( 'NONE',  ( -8.000000000000007105, 20.20000000000007390, 2.076830587532255432E-13 ) ) ;
#5327 = DIRECTION ( 'NONE',  ( 0.000000000000000000, -0.5877852522924624790, -0.8090169943749551118 ) ) ;
#5328 = LINE ( 'NONE', #34992, #18842 ) ;
#5329 = CARTESIAN_POINT ( 'NONE',  ( -93.84685191531248449, -208.0026889286704943, 76.09614583420047040 ) ) ;
#5330 = AXIS2_PLACEMENT_3D ( 'NONE', #10273, #56525, #38483 ) ;
#5331 = CARTESIAN_POINT ( 'NONE',  ( 11.99999999999999822, -70.52718814184240159, -26.02418014898383802 ) ) ;
#5332 = DIRECTION ( 'NONE',  ( -1.000000000000000000, -0.000000000000000000, -0.000000000000000000 ) ) ;
#5333 = FACE_OUTER_BOUND ( 'NONE', #49638, .T. ) ;
#5334 = CARTESIAN_POINT ( 'NONE',  ( -97.65000000000001990, 90.00000000000004263, 76.66499999999999204 ) ) ;
#5335 = CARTESIAN_POINT ( 'NONE',  ( 93.65592807507104567, -207.9734350352808860, 74.86703477254889094 ) ) ;
#5336 = CARTESIAN_POINT ( 'NONE',  ( -92.69370383062502583, 91.33154071421968467, 82.39322916753381776 ) ) ;
#5337 = DIRECTION ( 'NONE',  ( -1.000000000000000000, 0.000000000000000000, 0.000000000000000000 ) ) ;
#5338 = DIRECTION ( 'NONE',  ( -1.000000000000000000, -0.000000000000000000, -0.000000000000000000 ) ) ;
#5339 = AXIS2_PLACEMENT_3D ( 'NONE', #7437, #47652, #70555 ) ;
#5340 =( BOUNDED_CURVE ( )  B_SPLINE_CURVE ( 2, ( #27654, #4003, #32906, #4370, #29127, #64103, #6939, #17487, #981 ),
 .UNSPECIFIED., .F., .F. ) 
 B_SPLINE_CURVE_WITH_KNOTS ( ( 3, 2, 2, 2, 3 ),
 ( 0.4445132602971393343, 0.4515689946164714308, 0.4586247601573539279, 0.4656805256982364249, 0.4656806970056959760 ),
 .UNSPECIFIED. ) 
 CURVE ( )  GEOMETRIC_REPRESENTATION_ITEM ( )  RATIONAL_B_SPLINE_CURVE ( ( 0.9999988143381259853, 0.8660259966179989499, 1.000000000000000000, 0.8660254037844387076, 1.000000000000000000, 0.8660254037844387076, 1.000000000000000000, 0.9999967472207530461, 0.9999934945994550795 ) ) 
 REPRESENTATION_ITEM ( '' )  );
#5341 = ORIENTED_EDGE ( 'NONE', *, *, #13557, .T. ) ;
#5342 = FACE_OUTER_BOUND ( 'NONE', #18332, .T. ) ;
#5343 = LINE ( 'NONE', #17709, #14889 ) ;
#5344 = DIRECTION ( 'NONE',  ( -8.587739980083048116E-16, -1.065814103640131346E-14, -1.000000000000000000 ) ) ;
#5345 = VECTOR ( 'NONE', #36420, 1000.000000000000000 ) ;
#5346 = DIRECTION ( 'NONE',  ( 1.000000000000000000, 0.000000000000000000, -0.000000000000000000 ) ) ;
#5347 = CARTESIAN_POINT ( 'NONE',  ( -0.7207917504152121513, 5.357353380764376283, -1.325189086772940117 ) ) ;
#5348 = DIRECTION ( 'NONE',  ( -0.000000000000000000, -0.000000000000000000, -1.000000000000000000 ) ) ;
#5349 = CARTESIAN_POINT ( 'NONE',  ( -97.30629616937497417, -208.6684592857803011, 80.22364583420048234 ) ) ;
#5350 = CARTESIAN_POINT ( 'NONE',  ( 11.99999999999999822, 49.70050353004975818, -59.46389618801909904 ) ) ;
#5351 = AXIS2_PLACEMENT_3D ( 'NONE', #5575, #22860, #334 ) ;
#5352 = EDGE_LOOP ( 'NONE', ( #50749, #72211, #49808, #25522 ) ) ;
#5353 = VECTOR ( 'NONE', #32779, 1000.000000000000000 ) ;
#5354 = CARTESIAN_POINT ( 'NONE',  ( 0.000000000000000000, -35.53030884539077050, -12.26510123303296851 ) ) ;
#5355 = CARTESIAN_POINT ( 'NONE',  ( -0.9515373497862389396, -96.47140937769621871, 5.500000000000000000 ) ) ;
#5356 = LINE ( 'NONE', #74121, #59792 ) ;
#5357 = CARTESIAN_POINT ( 'NONE',  ( 11.99999999999999822, 23.16143007188426850, 73.95703589263983702 ) ) ;
#5359 = EDGE_CURVE ( 'NONE', #16188, #70424, #46746, .T. ) ;
#5358 = CARTESIAN_POINT ( 'NONE',  ( 0.000000000000000000, 0.000000000000000000, 0.000000000000000000 ) ) ;
#5360 = AXIS2_PLACEMENT_3D ( 'NONE', #38055, #55344, #44449 ) ;
#5361 = AXIS2_PLACEMENT_3D ( 'NONE', #22738, #45676, #15965 ) ;
#5362 = EDGE_CURVE ( 'NONE', #75, #7432, #54715, .T. ) ;
#5363 = CARTESIAN_POINT ( 'NONE',  ( -42.50000000000000000, 0.000000000000000000, 0.000000000000000000 ) ) ;
#5364 = ORIENTED_EDGE ( 'NONE', *, *, #70095, .T. ) ;
#5365 = EDGE_CURVE ( 'NONE', #70250, #6931, #61320, .T. ) ;
#5366 = LINE ( 'NONE', #57223, #36039 ) ;
#5367 = LINE ( 'NONE', #56855, #23554 ) ;
#5368 = ORIENTED_EDGE ( 'NONE', *, *, #53039, .T. ) ;
#5369 = AXIS2_PLACEMENT_3D ( 'NONE', #34199, #68430, #67675 ) ;
#5370 = EDGE_CURVE ( 'NONE', #49109, #15896, #69667, .T. ) ;
#5371 = CARTESIAN_POINT ( 'NONE',  ( 95.00000000000000000, -212.6630814284392557, 87.89656250086713385 ) ) ;
#5372 = FACE_OUTER_BOUND ( 'NONE', #50172, .T. ) ;
#5373 = EDGE_LOOP ( 'NONE', ( #8314, #19514, #952, #13113 ) ) ;
#5374 = VECTOR ( 'NONE', #24707, 1000.000000000000000 ) ;
#5375 = CARTESIAN_POINT ( 'NONE',  ( 10.00000000000000000, -2.956366410621191765, 75.11725578898467859 ) ) ;
#5376 = ORIENTED_EDGE ( 'NONE', *, *, #5294, .T. ) ;
#5377 = DIRECTION ( 'NONE',  ( -0.000000000000000000, 0.4999999999999921174, -0.8660254037844432595 ) ) ;
#5378 = EDGE_LOOP ( 'NONE', ( #48113, #10172, #24183, #42277 ) ) ;
#5379 = CARTESIAN_POINT ( 'NONE',  ( 97.64999999999999147, -209.9999999999999716, 82.06250000000000000 ) ) ;
#5380 = ORIENTED_EDGE ( 'NONE', *, *, #18856, .T. ) ;
#5381 = ORIENTED_EDGE ( 'NONE', *, *, #15027, .T. ) ;
#5382 = ORIENTED_EDGE ( 'NONE', *, *, #63596, .T. ) ;
#5383 = CARTESIAN_POINT ( 'NONE',  ( 0.000000000000000000, 9.615535125379096826, -24.73947219025904687 ) ) ;
#5384 = EDGE_CURVE ( 'NONE', #13441, #37581, #64335, .T. ) ;
#5385 = ADVANCED_FACE ( 'NONE', ( #58016 ), #41833, .T. ) ;
#5386 = ORIENTED_EDGE ( 'NONE', *, *, #59816, .T. ) ;
#5387 = ORIENTED_EDGE ( 'NONE', *, *, #34446, .T. ) ;
#5388 = CARTESIAN_POINT ( 'NONE',  ( 93.67499999999999716, 87.70503267997126784, 86.93083333333332519 ) ) ;
#5389 = CARTESIAN_POINT ( 'NONE',  ( -92.35000000000003695, 90.00000000000004263, 90.00000000000000000 ) ) ;
#5390 = DIRECTION ( 'NONE',  ( 0.3090169943749448977, 0.9510565162951543083, 0.000000000000000000 ) ) ;
#5391 = ORIENTED_EDGE ( 'NONE', *, *, #70773, .F. ) ;
#5392 = ORIENTED_EDGE ( 'NONE', *, *, #55365, .F. ) ;
#5393 = ORIENTED_EDGE ( 'NONE', *, *, #47773, .F. ) ;
#5394 = CARTESIAN_POINT ( 'NONE',  ( 92.69370383062498320, 91.33154071421968467, 84.50989583420046358 ) ) ;
#5395 = VERTEX_POINT ( 'NONE', #64779 ) ;
#5396 = CARTESIAN_POINT ( 'NONE',  ( 97.30629616937498838, -211.3315407142195852, 86.09739583420048348 ) ) ;
#5397 = EDGE_CURVE ( 'NONE', #69906, #25992, #17531, .T. ) ;
#5398 = EDGE_CURVE ( 'NONE', #49261, #48383, #188, .T. ) ;
#5399 = CIRCLE ( 'NONE', #70187, 82.00000000000000000 ) ;
#5400 = DIRECTION ( 'NONE',  ( 1.000000000000000000, 0.000000000000000000, -5.551115123125782702E-17 ) ) ;
#5401 = LINE ( 'NONE', #23776, #16340 ) ;
#5402 = CARTESIAN_POINT ( 'NONE',  ( 0.000000000000000000, 22.48208911017551515, -35.47612816024499693 ) ) ;
#5403 = FACE_OUTER_BOUND ( 'NONE', #35707, .T. ) ;
#5404 = CARTESIAN_POINT ( 'NONE',  ( 10.00000000000000000, -78.73519480814938731, -22.90783923731713756 ) ) ;
#5405 = LINE ( 'NONE', #16664, #11997 ) ;
#5406 = LINE ( 'NONE', #15920, #5882 ) ;
#5407 = CARTESIAN_POINT ( 'NONE',  ( -93.84685191531248449, -208.0026889286704943, 87.52614583420047722 ) ) ;
#5408 = CARTESIAN_POINT ( 'NONE',  ( -93.84685191531254134, 91.99731107132950569, 85.77989583420048803 ) ) ;
#5409 = ORIENTED_EDGE ( 'NONE', *, *, #34014, .F. ) ;
#5411 = CARTESIAN_POINT ( 'NONE',  ( -97.30629616937501680, 90.00000000000004263, 83.92781250086714806 ) ) ;
#5410 = CARTESIAN_POINT ( 'NONE',  ( 96.15314808468748708, 88.00268892867053694, 84.13947916753380696 ) ) ;
#5412 = ORIENTED_EDGE ( 'NONE', *, *, #1804, .F. ) ;
#5413 = CARTESIAN_POINT ( 'NONE',  ( 10.00000000000000000, -35.91791733033426226, -68.67312586195033930 ) ) ;
#5414 = VECTOR ( 'NONE', #55886, 1000.000000000000000 ) ;
#5415 = FACE_OUTER_BOUND ( 'NONE', #14412, .T. ) ;
#5416 = DIRECTION ( 'NONE',  ( -0.000000000000000000, -0.000000000000000000, 1.000000000000000000 ) ) ;
#5417 = LINE ( 'NONE', #58007, #27215 ) ;
#5418 = CARTESIAN_POINT ( 'NONE',  ( -95.00000000000002842, 93.05995642670504253, 86.66624999999999091 ) ) ;
#5419 = DIRECTION ( 'NONE',  ( 0.000000000000000000, -0.5877852522924801315, 0.8090169943749423442 ) ) ;
#5420 = CARTESIAN_POINT ( 'NONE',  ( 10.00000000000000000, 46.54456581323805153, 59.03342792756280488 ) ) ;
#5421 = DIRECTION ( 'NONE',  ( -1.000000000000000000, 0.000000000000000000, 0.000000000000000000 ) ) ;
#5422 = AXIS2_PLACEMENT_3D ( 'NONE', #20026, #49343, #42981 ) ;
#5423 = CYLINDRICAL_SURFACE ( 'NONE', #22696, 31.99999999999998579 ) ;
#5424 = ORIENTED_EDGE ( 'NONE', *, *, #21799, .F. ) ;
#5425 = ORIENTED_EDGE ( 'NONE', *, *, #11475, .T. ) ;
#5426 = CARTESIAN_POINT ( 'NONE',  ( -95.00000000000002842, 93.05995642670501411, 78.41125000000000966 ) ) ;
#5427 = CARTESIAN_POINT ( 'NONE',  ( -100.0000000000260059, -214.9999999999999716, 75.00000000001300293 ) ) ;
#5428 = CARTESIAN_POINT ( 'NONE',  ( 5.000000000000002665, -78.73519480814971416, 22.90783923731600069 ) ) ;
#5429 = LINE ( 'NONE', #56556, #54340 ) ;
#5430 = CARTESIAN_POINT ( 'NONE',  ( -97.64999999999996305, -208.4700217866474645, 89.94708333333332462 ) ) ;
#5431 = CARTESIAN_POINT ( 'NONE',  ( -96.32500000000001705, 87.70503267997129626, 86.37520833506764006 ) ) ;
#5432 = FACE_OUTER_BOUND ( 'NONE', #20715, .T. ) ;
#5433 = EDGE_LOOP ( 'NONE', ( #48980, #66613, #16684, #21842 ) ) ;
#5434 = CARTESIAN_POINT ( 'NONE',  ( -92.69370383062502583, 91.33154071421968467, 78.58322916753381548 ) ) ;
#5435 = AXIS2_PLACEMENT_3D ( 'NONE', #29881, #46449, #64481 ) ;
#5436 = PLANE ( 'NONE',  #23539 ) ;
#5437 = LINE ( 'NONE', #10681, #57047 ) ;
#5438 = DIRECTION ( 'NONE',  ( 0.000000000000000000, 0.2079116908177664480, -0.9781476007338041345 ) ) ;
#5439 = CYLINDRICAL_SURFACE ( 'NONE', #36880, 37.49900000000000233 ) ;
#5440 = CIRCLE ( 'NONE', #47432, 31.99999999999998934 ) ;
#5441 = DIRECTION ( 'NONE',  ( -0.000000000000000000, -0.000000000000000000, 1.000000000000000000 ) ) ;
#5442 = DIRECTION ( 'NONE',  ( 1.000000000000000000, 0.000000000000000000, 0.000000000000000000 ) ) ;
#5443 = ADVANCED_FACE ( 'NONE', ( #46009 ), #52752, .T. ) ;
#5444 = SURFACE_STYLE_FILL_AREA ( #16331 ) ;
#5445 = EDGE_CURVE ( 'NONE', #59396, #38665, #25943, .T. ) ;
#5446 = EDGE_CURVE ( 'NONE', #72954, #36972, #33416, .T. ) ;
#5447 = CARTESIAN_POINT ( 'NONE',  ( 96.15314808468748708, 91.99731107132950569, 78.15989583420049769 ) ) ;
#5448 = EDGE_CURVE ( 'NONE', #24686, #22781, #40386, .T. ) ;
#5449 = CARTESIAN_POINT ( 'NONE',  ( -94.99999999999997158, -212.6630814284392557, 78.53031250086715431 ) ) ;
#5450 = CARTESIAN_POINT ( 'NONE',  ( 10.00000000000000000, -37.01155633439063308, 6.555932627142289526 ) ) ;
#5451 = ORIENTED_EDGE ( 'NONE', *, *, #23662, .T. ) ;
#5452 = DIRECTION ( 'NONE',  ( 1.000000000000000000, 0.000000000000000000, 0.000000000000000000 ) ) ;
#5453 = CARTESIAN_POINT ( 'NONE',  ( -93.67499999999998295, -207.7050326799711968, 75.81833333333332803 ) ) ;
#5454 = DIRECTION ( 'NONE',  ( -1.000000000000000000, 0.000000000000000000, 0.000000000000000000 ) ) ;
#5455 = AXIS2_PLACEMENT_3D ( 'NONE', #15260, #20537, #66043 ) ;
#5456 = EDGE_CURVE ( 'NONE', #16527, #66304, #66259, .T. ) ;
#5457 = CARTESIAN_POINT ( 'NONE',  ( -96.15314808468752972, 91.99731107132950569, 76.99572916753382401 ) ) ;
#5458 = CARTESIAN_POINT ( 'NONE',  ( 96.15314808468750130, -211.9973110713294489, 80.96447916753380980 ) ) ;
#5459 = ORIENTED_EDGE ( 'NONE', *, *, #38976, .F. ) ;
#5460 = DIRECTION ( 'NONE',  ( 0.000000000000000000, 0.000000000000000000, 1.000000000000000000 ) ) ;
#5461 = EDGE_LOOP ( 'NONE', ( #16299, #28936, #3820, #70069 ) ) ;
#5462 = VECTOR ( 'NONE', #21281, 1000.000000000000000 ) ;
#5463 = EDGE_CURVE ( 'NONE', #23087, #53667, #60875, .T. ) ;
#5464 = CARTESIAN_POINT ( 'NONE',  ( -97.64999999999996305, -208.4700217866474645, 88.12145833506765769 ) ) ;
#5465 = VERTEX_POINT ( 'NONE', #47840 ) ;
#5466 = PLANE ( 'NONE',  #40740 ) ;
#5467 = AXIS2_PLACEMENT_3D ( 'NONE', #64610, #30380, #53326 ) ;
#5468 = EDGE_LOOP ( 'NONE', ( #47206, #51966, #6133, #7628 ) ) ;
#5469 = ORIENTED_EDGE ( 'NONE', *, *, #17302, .T. ) ;
#5470 = AXIS2_PLACEMENT_3D ( 'NONE', #69128, #51825, #371 ) ;
#5471 = EDGE_LOOP ( 'NONE', ( #64129, #62753, #17020, #67015 ) ) ;
#5472 = CARTESIAN_POINT ( 'NONE',  ( 95.00000000000000000, -212.6630814284392557, 76.62531250086715318 ) ) ;
#5473 = EDGE_CURVE ( 'NONE', #48807, #37410, #37972, .T. ) ;
#5474 = EDGE_CURVE ( 'NONE', #23517, #26896, #54774, .T. ) ;
#5475 = VERTEX_POINT ( 'NONE', #72243 ) ;
#5476 = DIRECTION ( 'NONE',  ( 0.5000000000000009992, 0.8660254037844381525, -0.000000000000000000 ) ) ;
#5477 = CARTESIAN_POINT ( 'NONE',  ( 10.00000000000000000, -65.64334221924882229, -41.19522573413803457 ) ) ;
#5478 = CARTESIAN_POINT ( 'NONE',  ( 92.69370383062498320, 91.33154071421968467, 82.76364583420048859 ) ) ;
#5479 = CARTESIAN_POINT ( 'NONE',  ( 96.32499999999998863, -207.7050326799711968, 77.72333333333332916 ) ) ;
#5480 = VECTOR ( 'NONE', #50881, 1000.000000000000000 ) ;
#5481 = ORIENTED_EDGE ( 'NONE', *, *, #7819, .T. ) ;
#5482 = ORIENTED_EDGE ( 'NONE', *, *, #59825, .T. ) ;
#5483 = ORIENTED_EDGE ( 'NONE', *, *, #24029, .T. ) ;
#5484 = ORIENTED_EDGE ( 'NONE', *, *, #28477, .F. ) ;
#5485 = CARTESIAN_POINT ( 'NONE',  ( 2.500000000000029754, 73.00000000000001421, -204.9999999999999716 ) ) ;
#5486 = DIRECTION ( 'NONE',  ( -1.000000000000000000, 0.000000000000000000, -0.000000000000000000 ) ) ;
#5487 = CIRCLE ( 'NONE', #13871, 77.49900000000000944 ) ;
#5488 = CARTESIAN_POINT ( 'NONE',  ( 11.99999999999999822, 0.000000000000000000, 0.000000000000000000 ) ) ;
#5489 = CARTESIAN_POINT ( 'NONE',  ( -42.50000000000000000, 0.000000000000000000, 0.000000000000000000 ) ) ;
#5490 = LINE ( 'NONE', #28386, #37178 ) ;
#5491 = DIRECTION ( 'NONE',  ( -1.000000000000000000, -0.000000000000000000, 0.000000000000000000 ) ) ;
#5492 = ORIENTED_EDGE ( 'NONE', *, *, #26971, .T. ) ;
#5493 = CARTESIAN_POINT ( 'NONE',  ( -96.32499999999996021, -212.2949673200287179, 83.83520833506763381 ) ) ;
#5494 = ORIENTED_EDGE ( 'NONE', *, *, #45595, .T. ) ;
#5495 = DIRECTION ( 'NONE',  ( 0.000000000000000000, 0.000000000000000000, 1.000000000000000000 ) ) ;
#5496 = VERTEX_POINT ( 'NONE', #14734 ) ;
#5498 = CARTESIAN_POINT ( 'NONE',  ( -97.65000000000001990, 91.52997821335253548, 81.13645833506764404 ) ) ;
#5497 = CARTESIAN_POINT ( 'NONE',  ( 92.34999999999999432, 91.52997821335252127, 79.23145833506762870 ) ) ;
#5499 = ORIENTED_EDGE ( 'NONE', *, *, #59426, .T. ) ;
#5500 = CARTESIAN_POINT ( 'NONE',  ( 92.69370383062498320, 91.33154071421968467, 82.76364583420048859 ) ) ;
#5501 = DIRECTION ( 'NONE',  ( 0.000000000000000000, 0.000000000000000000, 1.000000000000000000 ) ) ;
#5502 = DIRECTION ( 'NONE',  ( -1.000000000000000000, 0.000000000000000000, -0.000000000000000000 ) ) ;
#5503 = CYLINDRICAL_SURFACE ( 'NONE', #45826, 42.00000000000000000 ) ;
#5504 = CARTESIAN_POINT ( 'NONE',  ( 94.99999999999998579, 93.05995642670504253, 81.66562500173431260 ) ) ;
#5505 = DIRECTION ( 'NONE',  ( -1.000000000000000000, 0.000000000000000000, -0.000000000000000000 ) ) ;
#5506 = VERTEX_POINT ( 'NONE', #43698 ) ;
#5507 = DIRECTION ( 'NONE',  ( 1.000000000000000000, 0.000000000000000000, 0.000000000000000000 ) ) ;
#5508 = DIRECTION ( 'NONE',  ( 0.000000000000000000, 0.000000000000000000, 1.000000000000000000 ) ) ;
#5509 = DIRECTION ( 'NONE',  ( -0.08130631524010122069, 0.9966891607226784355, 0.000000000000000000 ) ) ;
#5510 = ORIENTED_EDGE ( 'NONE', *, *, #53695, .T. ) ;
#5511 = VERTEX_POINT ( 'NONE', #60618 ) ;
#5512 = CARTESIAN_POINT ( 'NONE',  ( 10.00000000000000000, 5.202137450156907761, -37.22597642581151689 ) ) ;
#5513 = EDGE_CURVE ( 'NONE', #72105, #27765, #15102, .T. ) ;
#5514 = DIRECTION ( 'NONE',  ( -1.000000000000000000, 0.000000000000000000, -0.000000000000000000 ) ) ;
#5515 = CYLINDRICAL_SURFACE ( 'NONE', #11441, 31.99999999999999289 ) ;
#5516 = FACE_OUTER_BOUND ( 'NONE', #55866, .T. ) ;
#5517 = CARTESIAN_POINT ( 'NONE',  ( -97.30629616937497417, -208.6684592857803011, 80.85864583420048746 ) ) ;
#5518 = VERTEX_POINT ( 'NONE', #48939 ) ;
#5519 = CIRCLE ( 'NONE', #39091, 35.50000000000000711 ) ;
#5520 = VERTEX_POINT ( 'NONE', #30540 ) ;
#5521 = DIRECTION ( 'NONE',  ( 0.000000000000000000, 0.000000000000000000, 1.000000000000000000 ) ) ;
#5522 = VECTOR ( 'NONE', #2467, 1000.000000000000000 ) ;
#5523 = CARTESIAN_POINT ( 'NONE',  ( -96.25799313130249857, -212.2877248121365312, 74.97309184317589370 ) ) ;
#5524 = FILL_AREA_STYLE ('',( #57018 ) ) ;
#5525 = CIRCLE ( 'NONE', #43931, 31.99999999999998579 ) ;
#5526 = FACE_OUTER_BOUND ( 'NONE', #28371, .T. ) ;
#5527 = DIRECTION ( 'NONE',  ( -1.000000000000000000, -0.000000000000000000, 0.000000000000000000 ) ) ;
#5528 = CARTESIAN_POINT ( 'NONE',  ( 92.35000000003357457, 89.99999234487445676, 78.01464417100922333 ) ) ;
#5529 = EDGE_CURVE ( 'NONE', #8511, #24726, #3171, .T. ) ;
#5530 = CIRCLE ( 'NONE', #40283, 2.649999999999985700 ) ;
#5531 = CARTESIAN_POINT ( 'NONE',  ( -97.64999999999996305, -209.9999999999999716, 79.20499999999999829 ) ) ;
#5532 = CARTESIAN_POINT ( 'NONE',  ( 95.00000000000000000, -209.9999999999999716, 75.00000000000000000 ) ) ;
#5533 = DIRECTION ( 'NONE',  ( -1.000000000000000000, -0.000000000000000000, 0.000000000000000000 ) ) ;
#5534 = EDGE_CURVE ( 'NONE', #59559, #60502, #42220, .T. ) ;
#5535 = CARTESIAN_POINT ( 'NONE',  ( 10.00000000000000000, 0.000000000000000000, 0.000000000000000000 ) ) ;
#5536 = AXIS2_PLACEMENT_3D ( 'NONE', #62950, #39623, #33972 ) ;
#5537 = AXIS2_PLACEMENT_3D ( 'NONE', #54589, #44053, #15093 ) ;
#5538 = CARTESIAN_POINT ( 'NONE',  ( 92.69370383062498320, 88.66845928578035796, 86.67947916753382742 ) ) ;
#5539 = EDGE_CURVE ( 'NONE', #71364, #29066, #29577, .T. ) ;
#5540 = CARTESIAN_POINT ( 'NONE',  ( -92.69370383062498320, -209.9999999999999716, 88.84906250086716284 ) ) ;
#5541 = CARTESIAN_POINT ( 'NONE',  ( 93.67499999999999716, 87.70503267997126784, 82.48583333333333201 ) ) ;
#5542 = EDGE_LOOP ( 'NONE', ( #1153, #37017, #56985, #63447 ) ) ;
#5543 = EDGE_CURVE ( 'NONE', #40961, #24049, #31285, .T. ) ;
#5544 = CARTESIAN_POINT ( 'NONE',  ( -3.000000000000000000, 20.85821328998756385, -10.92862929874494959 ) ) ;
#5545 = CARTESIAN_POINT ( 'NONE',  ( -97.30629616937501680, 88.66845928578038638, 78.26572916753380582 ) ) ;
#5546 = VECTOR ( 'NONE', #20690, 1000.000000000000000 ) ;
#5547 = DIRECTION ( 'NONE',  ( 0.000000000000000000, -0.2334453638558922628, -0.9723699203976798877 ) ) ;
#5548 = ORIENTED_EDGE ( 'NONE', *, *, #53789, .F. ) ;
#5549 =( BOUNDED_CURVE ( )  B_SPLINE_CURVE ( 2, ( #61613, #27010, #21003, #62372, #33389, #10100, #33022 ),
 .UNSPECIFIED., .F., .F. ) 
 B_SPLINE_CURVE_WITH_KNOTS ( ( 3, 2, 2, 3 ),
 ( 0.7083333333333331483, 0.7152777777777775681, 0.7222222222222220989, 0.7291666666666665186 ),
 .UNSPECIFIED. ) 
 CURVE ( )  GEOMETRIC_REPRESENTATION_ITEM ( )  RATIONAL_B_SPLINE_CURVE ( ( 1.000000000000004219, 0.8660254037844343777, 1.000000000000000000, 0.8660254037844387076, 1.000000000000000000, 0.8660254037844408170, 0.9999999999999978906 ) ) 
 REPRESENTATION_ITEM ( '' )  );
#5550 = DIRECTION ( 'NONE',  ( 0.000000000000000000, -0.3090169943749471737, 0.9510565162951537532 ) ) ;
#5551 = DIRECTION ( 'NONE',  ( 0.000000000000000000, 6.938893903907229364E-16, 1.000000000000000000 ) ) ;
#5552 = EDGE_CURVE ( 'NONE', #34058, #11494, #72778, .T. ) ;
#5553 = DIRECTION ( 'NONE',  ( -1.000000000000000000, 0.000000000000000000, -0.000000000000000000 ) ) ;
#5554 = CARTESIAN_POINT ( 'NONE',  ( -92.35000000000000853, -208.4700217866474929, 84.65541666666669585 ) ) ;
#5555 = DIRECTION ( 'NONE',  ( 0.000000000000000000, 0.9876883405951372152, 0.1564344650402346160 ) ) ;
#5556 = ORIENTED_EDGE ( 'NONE', *, *, #2780, .F. ) ;
#5557 = VERTEX_POINT ( 'NONE', #70765 ) ;
#5558 = CARTESIAN_POINT ( 'NONE',  ( 93.84685191531251292, -211.9973110713294489, 86.73239583420048859 ) ) ;
#5559 = EDGE_CURVE ( 'NONE', #38945, #4632, #19266, .T. ) ;
#5560 = CARTESIAN_POINT ( 'NONE',  ( -93.67499999999998295, -207.7050326799711968, 81.61270833506763722 ) ) ;
#5561 = DIRECTION ( 'NONE',  ( 0.000000000000000000, -0.8910065241883722287, 0.4539904997395383668 ) ) ;
#5562 = DIRECTION ( 'NONE',  ( 0.000000000000000000, 0.000000000000000000, 1.000000000000000000 ) ) ;
#5563 =( BOUNDED_CURVE ( )  B_SPLINE_CURVE ( 2, ( #27799, #28531, #74027, #68780, #62411, #63147, #28170 ),
 .UNSPECIFIED., .F., .F. ) 
 B_SPLINE_CURVE_WITH_KNOTS ( ( 3, 2, 2, 3 ),
 ( 0.2708333333333337034, 0.2777777777777781232, 0.2847222222222224874, 0.2916666666666669072 ),
 .UNSPECIFIED. ) 
 CURVE ( )  GEOMETRIC_REPRESENTATION_ITEM ( )  RATIONAL_B_SPLINE_CURVE ( ( 0.9999999999999924505, 0.8660254037844462571, 1.000000000000000000, 0.8660254037844387076, 1.000000000000000000, 0.8660254037844343777, 1.000000000000004219 ) ) 
 REPRESENTATION_ITEM ( '' )  );
#5564 = DIRECTION ( 'NONE',  ( 1.000000000000000000, 0.000000000000000000, 0.000000000000000000 ) ) ;
#5565 = EDGE_CURVE ( 'NONE', #73113, #11201, #5583, .T. ) ;
#5566 = AXIS2_PLACEMENT_3D ( 'NONE', #4303, #5416, #16675 ) ;
#5567 = CARTESIAN_POINT ( 'NONE',  ( 96.32499999999998863, -212.2949673200287179, 82.03604166840096923 ) ) ;
#5568 = CARTESIAN_POINT ( 'NONE',  ( 96.32499999999998863, -212.2949673200287179, 89.57666666666666799 ) ) ;
#5569 = ORIENTED_EDGE ( 'NONE', *, *, #73557, .T. ) ;
#5570 = EDGE_LOOP ( 'NONE', ( #66507, #70540, #51036, #5665 ) ) ;
#5571 = ORIENTED_EDGE ( 'NONE', *, *, #4976, .F. ) ;
#5572 = VERTEX_POINT ( 'NONE', #48219 ) ;
#5573 = LINE ( 'NONE', #39398, #68174 ) ;
#5574 = VECTOR ( 'NONE', #24030, 1000.000000000000000 ) ;
#5575 = CARTESIAN_POINT ( 'NONE',  ( 10.00000000000000000, -37.22597642581161637, 5.202137450156258502 ) ) ;
#5576 = LINE ( 'NONE', #16091, #72540 ) ;
#5577 = CARTESIAN_POINT ( 'NONE',  ( 96.32499999999998863, -212.2949673200287179, 78.22604166840096696 ) ) ;
#5578 = CARTESIAN_POINT ( 'NONE',  ( 97.64999999999997726, 91.52997821335252127, 80.84541666666666515 ) ) ;
#5579 = VERTEX_POINT ( 'NONE', #71130 ) ;
#5580 = DIRECTION ( 'NONE',  ( 0.000000000000000000, 0.000000000000000000, 1.000000000000000000 ) ) ;
#5581 = EDGE_LOOP ( 'NONE', ( #28125, #2649, #2352, #53451 ) ) ;
#5582 = CARTESIAN_POINT ( 'NONE',  ( -6.880223345695647197, -142.5202692415819854, 5.500000000000000000 ) ) ;
#5583 = CIRCLE ( 'NONE', #70366, 77.49899999999999523 ) ;
#5584 = ORIENTED_EDGE ( 'NONE', *, *, #5473, .T. ) ;
#5585 = AXIS2_PLACEMENT_3D ( 'NONE', #73344, #10566, #68475 ) ;
#5586 = CARTESIAN_POINT ( 'NONE',  ( 0.000000000000000000, 16.45098606841126454, 33.79645857604518966 ) ) ;
#5587 = CARTESIAN_POINT ( 'NONE',  ( -92.69370383062504004, 90.00000000000004263, 81.86406250086714920 ) ) ;
#5588 = CARTESIAN_POINT ( 'NONE',  ( 96.15314808468748708, 91.99731107132950569, 76.73114583420047552 ) ) ;
#5589 = ORIENTED_EDGE ( 'NONE', *, *, #60526, .F. ) ;
#5590 = DIRECTION ( 'NONE',  ( -1.000000000000000000, 0.000000000000000000, 0.000000000000000000 ) ) ;
#5591 = FACE_OUTER_BOUND ( 'NONE', #64787, .T. ) ;
#5592 = CARTESIAN_POINT ( 'NONE',  ( 100.0000000000000000, -214.9999999999999716, -90.00000000000000000 ) ) ;
#5593 = DIRECTION ( 'NONE',  ( -1.000000000000000000, -0.000000000000000000, -0.000000000000000000 ) ) ;
#5594 = EDGE_LOOP ( 'NONE', ( #14899, #42394, #34769, #46058 ) ) ;
#5595 = FACE_OUTER_BOUND ( 'NONE', #69437, .T. ) ;
#5596 = CARTESIAN_POINT ( 'NONE',  ( -93.84685191531248449, -208.0026889286704943, 78.63614583420047666 ) ) ;
#5597 = EDGE_LOOP ( 'NONE', ( #33846, #52334, #14884, #54547 ) ) ;
#5598 = MECHANICAL_DESIGN_GEOMETRIC_PRESENTATION_REPRESENTATION (  '', ( #65580 ), #70381 ) ;
#5599 = ORIENTED_EDGE ( 'NONE', *, *, #20574, .T. ) ;
#5600 = CARTESIAN_POINT ( 'NONE',  ( -97.65000000000001990, 90.00000000000004263, 90.00000000000000000 ) ) ;
#5601 = EDGE_LOOP ( 'NONE', ( #12654, #65551, #24404, #58922 ) ) ;
#5602 = CARTESIAN_POINT ( 'NONE',  ( 0.000000000000000000, -71.21200624218825226, 40.65526001592589722 ) ) ;
#5603 = CARTESIAN_POINT ( 'NONE',  ( 0.000000000000000000, 33.79645857604513992, 16.45098606841138178 ) ) ;
#5604 = EDGE_LOOP ( 'NONE', ( #33258, #63531, #38590, #6918 ) ) ;
#5605 = CARTESIAN_POINT ( 'NONE',  ( -96.15314808468745866, -211.9973110713294489, 77.68364583420047609 ) ) ;
#5606 = ORIENTED_EDGE ( 'NONE', *, *, #73133, .T. ) ;
#5607 = LINE ( 'NONE', #51441, #21851 ) ;
#5608 = DIRECTION ( 'NONE',  ( 0.000000000000000000, 0.000000000000000000, 1.000000000000000000 ) ) ;
#5609 = CARTESIAN_POINT ( 'NONE',  ( 1.692257445284848207E-12, 0.000000000000000000, -65.00000000000000000 ) ) ;
#5610 = DIRECTION ( 'NONE',  ( 0.000000000000000000, 0.000000000000000000, 1.000000000000000000 ) ) ;
#5611 = CARTESIAN_POINT ( 'NONE',  ( -96.32500000000001705, 87.70503267997129626, 81.21583333333333599 ) ) ;
#5612 = EDGE_CURVE ( 'NONE', #64620, #51781, #64388, .T. ) ;
#5613 = CARTESIAN_POINT ( 'NONE',  ( 10.00000000000000000, 34.44570377933598593, 69.42325613327452061 ) ) ;
#5614 = CARTESIAN_POINT ( 'NONE',  ( 93.84685191531248449, 91.99731107132950569, 84.45697916753380241 ) ) ;
#5615 = CARTESIAN_POINT ( 'NONE',  ( -12.49999999999999645, 0.000000000000000000, 125.0000000000000000 ) ) ;
#5616 = CARTESIAN_POINT ( 'NONE',  ( -92.35000000000003695, 90.00000000000004263, 88.41249999999999432 ) ) ;
#5617 = ADVANCED_FACE ( 'NONE', ( #14372 ), #36929, .F. ) ;
#5618 = CARTESIAN_POINT ( 'NONE',  ( 0.000000000000000000, 0.000000000000000000, 0.000000000000000000 ) ) ;
#5619 = DIRECTION ( 'NONE',  ( 2.603472992746261562E-14, 2.546204323184492723E-14, -1.000000000000000000 ) ) ;
#5620 = DIRECTION ( 'NONE',  ( -1.000000000000000000, -9.814797785686868941E-17, 0.000000000000000000 ) ) ;
#5621 = EDGE_CURVE ( 'NONE', #64515, #2735, #47583, .T. ) ;
#5622 = LINE ( 'NONE', #51835, #49122 ) ;
#5623 = DIRECTION ( 'NONE',  ( 1.000000000000000000, 0.000000000000000000, 0.000000000000000000 ) ) ;
#5624 = CARTESIAN_POINT ( 'NONE',  ( -93.67500000000003979, 92.29496732002878900, 75.81833333333332803 ) ) ;
#5625 = AXIS2_PLACEMENT_3D ( 'NONE', #18427, #63572, #63942 ) ;
#5626 = CARTESIAN_POINT ( 'NONE',  ( 11.99999999999999822, -49.70050353004846500, -59.46389618802017907 ) ) ;
#5627 = EDGE_CURVE ( 'NONE', #55850, #68978, #21476, .T. ) ;
#5628 = CARTESIAN_POINT ( 'NONE',  ( 10.00000000000000000, 59.46389618802034960, -49.70050353004825894 ) ) ;
#5629 = DIRECTION ( 'NONE',  ( -0.5200609990132993854, -0.8541291221503274356, 0.000000000000000000 ) ) ;
#5630 = CARTESIAN_POINT ( 'NONE',  ( 11.99999999999999822, 2.956366410621684260, -75.11725578898465017 ) ) ;
#5631 = VECTOR ( 'NONE', #35443, 1000.000000000000000 ) ;
#5632 = CARTESIAN_POINT ( 'NONE',  ( -96.32499999999996021, -207.7050326799711968, 82.27416666666665890 ) ) ;
#5633 = CIRCLE ( 'NONE', #34369, 82.00000000000000000 ) ;
#5634 = CARTESIAN_POINT ( 'NONE',  ( 92.35000000000000853, -209.9999999999999716, 89.44437500173430067 ) ) ;
#5635 = AXIS2_PLACEMENT_3D ( 'NONE', #60893, #9378, #32296 ) ;
#5636 = EDGE_CURVE ( 'NONE', #55462, #1624, #68483, .T. ) ;
#5637 = EDGE_LOOP ( 'NONE', ( #34303, #46688, #56962, #69376 ) ) ;
#5638 = CARTESIAN_POINT ( 'NONE',  ( -97.65000000000000568, 91.52997821335254969, 77.24708333333332178 ) ) ;
#5639 = EDGE_CURVE ( 'NONE', #5801, #42810, #34541, .T. ) ;
#5640 = EDGE_CURVE ( 'NONE', #26437, #55546, #13967, .T. ) ;
#5641 = DIRECTION ( 'NONE',  ( 0.000000000000000000, -0.5000000000000011102, -0.8660254037844380415 ) ) ;
#5642 = DIRECTION ( 'NONE',  ( 0.8225049752423776450, 0.5687579148473765889, 0.000000000000000000 ) ) ;
#5643 = LINE ( 'NONE', #22930, #53416 ) ;
#5644 = EDGE_CURVE ( 'NONE', #24488, #40794, #9465, .T. ) ;
#5645 = CARTESIAN_POINT ( 'NONE',  ( 95.00000000000000000, -207.3369185715606307, 86.46781250086716852 ) ) ;
#5646 = AXIS2_PLACEMENT_3D ( 'NONE', #13104, #1873, #7839 ) ;
#5647 = VERTEX_POINT ( 'NONE', #16218 ) ;
#5648 = ORIENTED_EDGE ( 'NONE', *, *, #69208, .F. ) ;
#5649 = AXIS2_PLACEMENT_3D ( 'NONE', #5375, #57609, #33917 ) ;
#5650 = EDGE_CURVE ( 'NONE', #58605, #55390, #56076, .T. ) ;
#5651 = LINE ( 'NONE', #5281, #46409 ) ;
#5652 = ORIENTED_EDGE ( 'NONE', *, *, #64410, .T. ) ;
#5653 = CARTESIAN_POINT ( 'NONE',  ( 11.34017801569539685, -96.04900080221412395, -2.500000000000000000 ) ) ;
#5654 = CARTESIAN_POINT ( 'NONE',  ( 92.69370383062501162, -211.3315407142195852, 78.90072916753381094 ) ) ;
#5655 = EDGE_LOOP ( 'NONE', ( #59713, #37490, #46615, #34093 ) ) ;
#5656 = CARTESIAN_POINT ( 'NONE',  ( 97.30629616937498838, -211.3315407142195852, 81.81114583420048803 ) ) ;
#5657 = ORIENTED_EDGE ( 'NONE', *, *, #43327, .F. ) ;
#5658 = DIRECTION ( 'NONE',  ( 1.000000000000000000, 0.000000000000000000, -0.000000000000000000 ) ) ;
#5659 = ORIENTED_EDGE ( 'NONE', *, *, #29268, .F. ) ;
#5660 = ORIENTED_EDGE ( 'NONE', *, *, #66600, .F. ) ;
#5661 = DIRECTION ( 'NONE',  ( -1.000000000000000000, 0.000000000000000000, -0.000000000000000000 ) ) ;
#5662 = ORIENTED_EDGE ( 'NONE', *, *, #24333, .T. ) ;
#5663 = CARTESIAN_POINT ( 'NONE',  ( 0.000000000000000000, 10.74501242461282757, 35.92658777277515014 ) ) ;
#5664 = CARTESIAN_POINT ( 'NONE',  ( 93.67500000000001137, -207.7050326799711968, 87.43354166840096298 ) ) ;
#5665 = ORIENTED_EDGE ( 'NONE', *, *, #64179, .F. ) ;
#5666 = DIRECTION ( 'NONE',  ( 0.000000000000000000, 0.000000000000000000, -1.000000000000000000 ) ) ;
#5667 = ORIENTED_EDGE ( 'NONE', *, *, #10518, .F. ) ;
#5668 = CARTESIAN_POINT ( 'NONE',  ( 5.000000000000000000, -0.6964580643377611402, -0.6026403643956901313 ) ) ;
#5669 = ORIENTED_EDGE ( 'NONE', *, *, #22611, .T. ) ;
#5670 = VERTEX_POINT ( 'NONE', #39533 ) ;
#5671 = ORIENTED_EDGE ( 'NONE', *, *, #32218, .T. ) ;
#5672 = CARTESIAN_POINT ( 'NONE',  ( -97.64999999996638280, -210.0000076551254722, 78.01464417100379478 ) ) ;
#5673 = CARTESIAN_POINT ( 'NONE',  ( -97.65000000000001990, 90.00000000000004263, 78.57000000000000739 ) ) ;
#5674 = ORIENTED_EDGE ( 'NONE', *, *, #5179, .T. ) ;
#5675 = ORIENTED_EDGE ( 'NONE', *, *, #66295, .F. ) ;
#5676 = AXIS2_PLACEMENT_3D ( 'NONE', #21848, #71854, #61710 ) ;
#5677 = ORIENTED_EDGE ( 'NONE', *, *, #55930, .F. ) ;
#5678 = AXIS2_PLACEMENT_3D ( 'NONE', #58444, #70087, #1361 ) ;
#5679 = DIRECTION ( 'NONE',  ( -1.000000000000000000, 0.000000000000000000, -0.000000000000000000 ) ) ;
#5680 =( BOUNDED_CURVE ( )  B_SPLINE_CURVE ( 2, ( #72344, #43438, #59596, #8828, #71593, #66715, #31005 ),
 .UNSPECIFIED., .F., .F. ) 
 B_SPLINE_CURVE_WITH_KNOTS ( ( 3, 2, 2, 3 ),
 ( 0.3541666666666665741, 0.3611111111111109939, 0.3680555555555554137, 0.3749999999999998335 ),
 .UNSPECIFIED. ) 
 CURVE ( )  GEOMETRIC_REPRESENTATION_ITEM ( )  RATIONAL_B_SPLINE_CURVE ( ( 1.000000000000002220, 0.8660254037844365982, 1.000000000000000000, 0.8660254037844387076, 1.000000000000000000, 0.8660254037844419273, 0.9999999999999967804 ) ) 
 REPRESENTATION_ITEM ( '' )  );
#5681 = DIRECTION ( 'NONE',  ( -2.628368902995175337E-16, -1.000000000000000000, 0.000000000000000000 ) ) ;
#5682 = CARTESIAN_POINT ( 'NONE',  ( -92.35000000000005116, 88.47002178664754979, 87.08958333333333712 ) ) ;
#5683 = ORIENTED_EDGE ( 'NONE', *, *, #38523, .T. ) ;
#5684 = CARTESIAN_POINT ( 'NONE',  ( 10.00000000000000000, -55.16347631943084195, 60.67117009219116852 ) ) ;
#5685 = AXIS2_PLACEMENT_3D ( 'NONE', #35734, #52670, #70310 ) ;
#5686 = EDGE_LOOP ( 'NONE', ( #29391, #17111, #23076, #28497 ) ) ;
#5687 = DIRECTION ( 'NONE',  ( -0.000000000000000000, -0.000000000000000000, -1.000000000000000000 ) ) ;
#5688 = CARTESIAN_POINT ( 'NONE',  ( -97.30629616937495996, -209.9999999999999716, 87.10281250086714522 ) ) ;
#5689 = ORIENTED_EDGE ( 'NONE', *, *, #22921, .T. ) ;
#5690 = PLANE ( 'NONE',  #1457 ) ;
#5691 = DIRECTION ( 'NONE',  ( -1.000000000000000000, 0.000000000000000000, 0.000000000000000000 ) ) ;
#5692 = CYLINDRICAL_SURFACE ( 'NONE', #56103, 42.00000000000000000 ) ;
#5693 = CARTESIAN_POINT ( 'NONE',  ( -92.69370383062498320, -211.3315407142195852, 76.57239583420046358 ) ) ;
#5694 = ADVANCED_FACE ( 'NONE', ( #55332 ), #27495, .T. ) ;
#5695 = CARTESIAN_POINT ( 'NONE',  ( 62.50000000000000000, 0.000000000000000000, -184.9999999999999432 ) ) ;
#5696 = DIRECTION ( 'NONE',  ( 0.000000000000000000, 0.000000000000000000, 1.000000000000000000 ) ) ;
#5697 = ADVANCED_FACE ( 'NONE', ( #9840 ), #50431, .F. ) ;
#5698 = AXIS2_PLACEMENT_3D ( 'NONE', #11176, #33349, #63079 ) ;
#5699 = DIRECTION ( 'NONE',  ( -1.000000000000000000, -0.000000000000000000, -0.000000000000000000 ) ) ;
#5700 = EDGE_CURVE ( 'NONE', #39132, #24073, #44805, .T. ) ;
#5701 = LINE ( 'NONE', #34998, #15913 ) ;
#5702 = AXIS2_PLACEMENT_3D ( 'NONE', #22111, #39409, #63101 ) ;
#5703 = DIRECTION ( 'NONE',  ( 1.000000000000000000, 0.000000000000000000, 0.000000000000000000 ) ) ;
#5704 = CARTESIAN_POINT ( 'NONE',  ( -97.30629616937501680, 91.33154071421968467, 77.52489583420046415 ) ) ;
#5705 = CARTESIAN_POINT ( 'NONE',  ( -3.000000000000000000, -13.04903810567675038, 19.60159698893425428 ) ) ;
#5706 = FACE_OUTER_BOUND ( 'NONE', #38771, .T. ) ;
#5707 = EDGE_CURVE ( 'NONE', #26180, #9139, #33883, .T. ) ;
#5708 = ORIENTED_EDGE ( 'NONE', *, *, #50132, .T. ) ;
#5709 = CARTESIAN_POINT ( 'NONE',  ( 96.32499999999998863, 87.70503267997126784, 79.49604166840096298 ) ) ;
#5710 = EDGE_CURVE ( 'NONE', #359, #24340, #22610, .T. ) ;
#5711 = CARTESIAN_POINT ( 'NONE',  ( 97.64999999999999147, -210.0000217321284879, 89.12687425009498554 ) ) ;
#5712 = CARTESIAN_POINT ( 'NONE',  ( -5.000000000000000000, 2.886751345948126879, -6.000000000000000000 ) ) ;
#5713 = CARTESIAN_POINT ( 'NONE',  ( 0.000000000000000000, -21.40280677340398086, 36.13751322684410638 ) ) ;
#5714 = DIRECTION ( 'NONE',  ( -8.783410004945701396E-16, -1.065814103640131188E-14, -1.000000000000000000 ) ) ;
#5715 = CARTESIAN_POINT ( 'NONE',  ( -20.63749999999999574, -2.946905753440916183E-14, -1.643265707205091412E-14 ) ) ;
#5716 = CARTESIAN_POINT ( 'NONE',  ( -97.30629616937495996, -209.9999999999999716, 78.37156250086715659 ) ) ;
#5717 = CARTESIAN_POINT ( 'NONE',  ( 0.000000000000000000, 0.000000000000000000, -20.00000000000000000 ) ) ;
#5718 = APPLICATION_CONTEXT ( 'automotive_design' ) ;
#5719 = ORIENTED_EDGE ( 'NONE', *, *, #72608, .T. ) ;
#5720 = VECTOR ( 'NONE', #18384, 1000.000000000000000 ) ;
#5721 = FACE_OUTER_BOUND ( 'NONE', #29762, .T. ) ;
#5722 = EDGE_CURVE ( 'NONE', #12189, #59848, #69430, .T. ) ;
#5723 = CARTESIAN_POINT ( 'NONE',  ( 10.00000000000000000, -76.66974797899830207, -11.30684508768422170 ) ) ;
#5724 = DIRECTION ( 'NONE',  ( -1.000000000000000000, -0.000000000000000000, 0.000000000000000000 ) ) ;
#5725 = VECTOR ( 'NONE', #34971, 1000.000000000000000 ) ;
#5726 = DIRECTION ( 'NONE',  ( 2.603472992746261562E-14, 2.546204323184492723E-14, -1.000000000000000000 ) ) ;
#5727 = EDGE_CURVE ( 'NONE', #71661, #63816, #833, .T. ) ;
#5728 = EDGE_CURVE ( 'NONE', #13415, #59025, #57195, .T. ) ;
#5729 = VECTOR ( 'NONE', #45834, 1000.000000000000000 ) ;
#5730 = VECTOR ( 'NONE', #65164, 1000.000000000000227 ) ;
#5731 = FACE_OUTER_BOUND ( 'NONE', #45906, .T. ) ;
#5732 = VERTEX_POINT ( 'NONE', #23715 ) ;
#5733 = LINE ( 'NONE', #29370, #66072 ) ;
#5734 = EDGE_CURVE ( 'NONE', #66703, #56916, #40268, .T. ) ;
#5735 = CARTESIAN_POINT ( 'NONE',  ( 92.35000000000000853, -209.9999999999999716, 79.83999999999998920 ) ) ;
#5736 = EDGE_LOOP ( 'NONE', ( #72619, #72189, #1969, #38688 ) ) ;
#5737 = DIRECTION ( 'NONE',  ( -0.7071067811865479058, 8.659560562354930393E-17, -0.7071067811865472397 ) ) ;
#5738 = ORIENTED_EDGE ( 'NONE', *, *, #35004, .F. ) ;
#5739 = DIRECTION ( 'NONE',  ( -1.000000000000000000, -0.000000000000000000, -0.000000000000000000 ) ) ;
#5740 = VERTEX_POINT ( 'NONE', #1206 ) ;
#5741 = CARTESIAN_POINT ( 'NONE',  ( 0.000000000000000000, 0.000000000000000000, 0.000000000000000000 ) ) ;
#5742 = VERTEX_POINT ( 'NONE', #22989 ) ;
#5743 = CARTESIAN_POINT ( 'NONE',  ( 2.426025403784448642, 2.655529440325959183E-32, -2.168404344971008868E-16 ) ) ;
#5744 = AXIS2_PLACEMENT_3D ( 'NONE', #37905, #60835, #9317 ) ;
#5745 = VERTEX_POINT ( 'NONE', #1569 ) ;
#5746 = LINE ( 'NONE', #51954, #4517 ) ;
#5747 = VERTEX_POINT ( 'NONE', #23355 ) ;
#5748 = ORIENTED_EDGE ( 'NONE', *, *, #17800, .T. ) ;
#5749 = FACE_OUTER_BOUND ( 'NONE', #52429, .T. ) ;
#5750 = VECTOR ( 'NONE', #38051, 1000.000000000000000 ) ;
#5751 = EDGE_LOOP ( 'NONE', ( #16213, #49673, #409, #17324 ) ) ;
#5752 = ORIENTED_EDGE ( 'NONE', *, *, #7489, .F. ) ;
#5753 = VECTOR ( 'NONE', #28626, 999.9999999999998863 ) ;
#5754 = LINE ( 'NONE', #39215, #37181 ) ;
#5755 = CARTESIAN_POINT ( 'NONE',  ( 0.000000000000000000, -26.02418014898260878, -70.52718814184285634 ) ) ;
#5756 = ORIENTED_EDGE ( 'NONE', *, *, #32942, .T. ) ;
#5757 = ORIENTED_EDGE ( 'NONE', *, *, #9397, .T. ) ;
#5758 = CARTESIAN_POINT ( 'NONE',  ( 92.69370383062498320, 88.66845928578037217, 85.88572916753382458 ) ) ;
#5759 = ORIENTED_EDGE ( 'NONE', *, *, #56951, .F. ) ;
#5760 = CARTESIAN_POINT ( 'NONE',  ( 97.30629616937498838, -208.6684592857803011, 80.48822916753383083 ) ) ;
#5761 = SHAPE_DEFINITION_REPRESENTATION ( #4397, #42128 ) ;
#5762 = CARTESIAN_POINT ( 'NONE',  ( -92.35000000000003695, -208.4700217866474077, 76.40041666666667197 ) ) ;
#5763 = CARTESIAN_POINT ( 'NONE',  ( -97.64999999999999147, 88.47002178664753558, 84.33791666666667197 ) ) ;
#5764 = DIRECTION ( 'NONE',  ( -1.000000000000000000, 0.000000000000000000, 0.000000000000000000 ) ) ;
#5765 = CARTESIAN_POINT ( 'NONE',  ( 1.560000000000000053, 0.000000000000000000, 2.999999999999998668 ) ) ;
#5766 = CARTESIAN_POINT ( 'NONE',  ( 11.99999999999999822, 51.03279382321088065, 55.19960302592086521 ) ) ;
#5767 = CARTESIAN_POINT ( 'NONE',  ( 10.00000000000000000, 80.28980883073757013, 16.65972982744963460 ) ) ;
#5768 = CARTESIAN_POINT ( 'NONE',  ( -92.69370383062498320, -209.9999999999999716, 89.32531250086714181 ) ) ;
#5769 = CARTESIAN_POINT ( 'NONE',  ( -92.69370383062504004, 90.00000000000004263, 86.94406250086716170 ) ) ;
#5770 = VERTEX_POINT ( 'NONE', #28601 ) ;
#5772 = CARTESIAN_POINT ( 'NONE',  ( -95.00000000000002842, 92.66308142843932671, 86.30906250086715659 ) ) ;
#5771 = CARTESIAN_POINT ( 'NONE',  ( 97.30629616937498838, 90.00000000000002842, 85.51531250086713953 ) ) ;
#5773 =( BOUNDED_CURVE ( )  B_SPLINE_CURVE ( 2, ( #2076, #24958, #3903, #19314, #8422, #13675, #26804 ),
 .UNSPECIFIED., .F., .F. ) 
 B_SPLINE_CURVE_WITH_KNOTS ( ( 3, 2, 2, 3 ),
 ( 0.02116741234828206988, 0.02822306216352941585, 0.03527882770441186089, 0.04233441017594471306 ),
 .UNSPECIFIED. ) 
 CURVE ( )  GEOMETRIC_REPRESENTATION_ITEM ( )  RATIONAL_B_SPLINE_CURVE ( ( 0.9999956052845440091, 0.8660276011782074290, 1.000000000000000000, 0.8660254037844387076, 1.000000000000000000, 0.8660288798979868252, 0.9999930479532868066 ) ) 
 REPRESENTATION_ITEM ( '' )  );
#5774 = ORIENTED_EDGE ( 'NONE', *, *, #38944, .F. ) ;
#5775 = CARTESIAN_POINT ( 'NONE',  ( 10.00000000000000000, -33.00180498840035170, -17.80606268964575278 ) ) ;
#5776 = AXIS2_PLACEMENT_3D ( 'NONE', #52600, #24773, #70615 ) ;
#5777 = CARTESIAN_POINT ( 'NONE',  ( 10.00000000000000000, -21.32104025579135964, 30.84782396557210760 ) ) ;
#5778 = LINE ( 'NONE', #40346, #48742 ) ;
#5779 = DIRECTION ( 'NONE',  ( 0.000000000000000000, 0.2079116908177664758, -0.9781476007338042455 ) ) ;
#5780 = CARTESIAN_POINT ( 'NONE',  ( -97.30629616937495996, -209.9999999999999716, 87.10281250086714522 ) ) ;
#5781 = AXIS2_PLACEMENT_3D ( 'NONE', #63399, #27694, #50618 ) ;
#5782 = VECTOR ( 'NONE', #56283, 1000.000000000000000 ) ;
#5783 = DIRECTION ( 'NONE',  ( -0.000000000000000000, -0.000000000000000000, 1.000000000000000000 ) ) ;
#5784 = CARTESIAN_POINT ( 'NONE',  ( -95.00000000000002842, 86.94004357329504273, 88.96812500173430749 ) ) ;
#5785 = B_SPLINE_CURVE_WITH_KNOTS ( 'NONE', 3,
 ( #57282, #6523, #28701, #69299, #17428, #63302, #51996, #52371, #63679, #20387, #19268, #54241, #71501, #7623, #65519, #43342, #37687, #2768, #13991, #37321, #42958, #14375, #24911, #25294 ),
 .UNSPECIFIED., .F., .F.,
 ( 4, 2, 2, 2, 2, 2, 2, 2, 2, 2, 2, 4 ),
 ( -0.009991285189197379041, -0.009254074025163634351, -0.008516862861129889661, -0.007779651697096144104, -0.007411046115079250943, -0.007042440533062358649, -0.006673834951045466354, -0.006305229369028574060, -0.005568018204994787737, -0.004830807040961002281, -0.004462201458944102181, -0.004093595876927202080 ),
 .UNSPECIFIED. ) ;
#5786 = CARTESIAN_POINT ( 'NONE',  ( 10.00000000000000000, 0.000000000000000000, 0.000000000000000000 ) ) ;
#5787 = LINE ( 'NONE', #28691, #35863 ) ;
#5788 = ORIENTED_EDGE ( 'NONE', *, *, #65963, .F. ) ;
#5789 = EDGE_CURVE ( 'NONE', #37324, #18341, #52284, .T. ) ;
#5790 = ORIENTED_EDGE ( 'NONE', *, *, #56082, .F. ) ;
#5791 = AXIS2_PLACEMENT_3D ( 'NONE', #53865, #60984, #3865 ) ;
#5792 = EDGE_CURVE ( 'NONE', #67138, #14148, #11319, .T. ) ;
#5793 = CARTESIAN_POINT ( 'NONE',  ( -97.65000000000001990, 88.47002178664754979, 79.25791666666665947 ) ) ;
#5794 = CARTESIAN_POINT ( 'NONE',  ( 10.00000000000000000, 0.000000000000000000, 0.000000000000000000 ) ) ;
#5795 = DIRECTION ( 'NONE',  ( 1.000000000000000000, -0.000000000000000000, 0.000000000000000000 ) ) ;
#5796 = CARTESIAN_POINT ( 'NONE',  ( 15.00000000000000000, -13.04903810567646971, 19.60159698893442481 ) ) ;
#5797 = CYLINDRICAL_SURFACE ( 'NONE', #398, 42.00000000000000000 ) ;
#5798 = CARTESIAN_POINT ( 'NONE',  ( 15.00000000000000000, 26.50000000000000355, -1.500000000000000000 ) ) ;
#5799 = DIRECTION ( 'NONE',  ( -1.000000000000000000, -0.000000000000000000, 0.000000000000000000 ) ) ;
#5800 = EDGE_CURVE ( 'NONE', #54047, #56693, #34250, .T. ) ;
#5801 = VERTEX_POINT ( 'NONE', #12428 ) ;
#5802 = CARTESIAN_POINT ( 'NONE',  ( -93.84685191531252713, 88.00268892867056536, 77.15447916753380753 ) ) ;
#5803 = CARTESIAN_POINT ( 'NONE',  ( 0.000000000000000000, 23.59884966291538433, -12.14883922797231719 ) ) ;
#5804 = CARTESIAN_POINT ( 'NONE',  ( 0.000000000000000000, 68.55367621811204515, -44.99326035065983120 ) ) ;
#5805 = VECTOR ( 'NONE', #17560, 1000.000000000000000 ) ;
#5806 = DIRECTION ( 'NONE',  ( 0.000000000000000000, 0.000000000000000000, 1.000000000000000000 ) ) ;
#5807 = DIRECTION ( 'NONE',  ( 0.000000000000000000, 0.000000000000000000, 1.000000000000000000 ) ) ;
#5808 = CARTESIAN_POINT ( 'NONE',  ( -3.000000000000000000, 22.07842321921481243, 8.187992925817422218 ) ) ;
#5809 = CARTESIAN_POINT ( 'NONE',  ( -97.30629616937495996, -209.9999999999999716, 89.16656250086715829 ) ) ;
#5810 = EDGE_CURVE ( 'NONE', #12127, #28753, #63220, .T. ) ;
#5811 = AXIS2_PLACEMENT_3D ( 'NONE', #35728, #70303, #42138 ) ;
#5812 = EDGE_CURVE ( 'NONE', #2580, #30548, #56001, .T. ) ;
#5813 = CARTESIAN_POINT ( 'NONE',  ( 97.30629616937498838, 90.00000000000002842, 76.78406250086715090 ) ) ;
#5814 = CARTESIAN_POINT ( 'NONE',  ( -97.30629616937497417, -211.3315407142195852, 80.96447916753382401 ) ) ;
#5815 = DIRECTION ( 'NONE',  ( 0.000000000000000000, 0.9723699203976756689, 0.2334453638559095268 ) ) ;
#5816 = VERTEX_POINT ( 'NONE', #45924 ) ;
#5817 = CARTESIAN_POINT ( 'NONE',  ( 11.99999999999999822, -30.41916302227062019, -71.27951684758059514 ) ) ;
#5818 = DIRECTION ( 'NONE',  ( 0.000000000000000000, 0.4539904997395413644, 0.8910065241883706744 ) ) ;
#5819 = CARTESIAN_POINT ( 'NONE',  ( -12.50000000000000000, -107.5000000000000000, 40.00000000000000000 ) ) ;
#5820 = EDGE_CURVE ( 'NONE', #17228, #10249, #30755, .T. ) ;
#5821 = ADVANCED_FACE ( 'NONE', ( #68852 ), #40639, .T. ) ;
#5822 = CARTESIAN_POINT ( 'NONE',  ( 10.00000000000000000, -35.38097989696503021, -12.42422080174676147 ) ) ;
#5823 = CARTESIAN_POINT ( 'NONE',  ( 92.69370383062501162, -211.3315407142195852, 79.53572916753380184 ) ) ;
#5824 = ORIENTED_EDGE ( 'NONE', *, *, #72222, .T. ) ;
#5825 = CARTESIAN_POINT ( 'NONE',  ( -96.32500000000001705, 92.29496732002878900, 75.28916666666665947 ) ) ;
#5826 = ORIENTED_EDGE ( 'NONE', *, *, #18491, .F. ) ;
#5827 = AXIS2_PLACEMENT_3D ( 'NONE', #24687, #47998, #65296 ) ;
#5828 = CARTESIAN_POINT ( 'NONE',  ( 92.35000000019411459, 89.99998015682159291, 84.36502760998348549 ) ) ;
#5829 = ORIENTED_EDGE ( 'NONE', *, *, #9776, .T. ) ;
#5830 = CIRCLE ( 'NONE', #74228, 31.99999999999998579 ) ;
#5831 = CIRCLE ( 'NONE', #65879, 31.99999999999998579 ) ;
#5832 = DIRECTION ( 'NONE',  ( 0.000000000000000000, -1.000000000000000000, -1.301042606982602560E-15 ) ) ;
#5833 = VECTOR ( 'NONE', #37229, 1000.000000000000000 ) ;
#5834 = ORIENTED_EDGE ( 'NONE', *, *, #70421, .T. ) ;
#5835 = VERTEX_POINT ( 'NONE', #18437 ) ;
#5836 = CIRCLE ( 'NONE', #57456, 77.49900000000002365 ) ;
#5837 = ORIENTED_EDGE ( 'NONE', *, *, #8050, .F. ) ;
#5838 = DIRECTION ( 'NONE',  ( -1.000000000000000000, 0.000000000000000000, 0.000000000000000000 ) ) ;
#5839 = ORIENTED_EDGE ( 'NONE', *, *, #60838, .T. ) ;
#5840 = ORIENTED_EDGE ( 'NONE', *, *, #47459, .T. ) ;
#5841 = CARTESIAN_POINT ( 'NONE',  ( 96.15314808468748708, 88.00268892867053694, 84.29822916753381890 ) ) ;
#5842 = CARTESIAN_POINT ( 'NONE',  ( 92.35000000000000853, -209.9999999999999716, 77.29999999999999716 ) ) ;
#5843 = ORIENTED_EDGE ( 'NONE', *, *, #67054, .T. ) ;
#5844 = ORIENTED_EDGE ( 'NONE', *, *, #37965, .T. ) ;
#5845 = VERTEX_POINT ( 'NONE', #30088 ) ;
#5846 = ORIENTED_EDGE ( 'NONE', *, *, #42374, .F. ) ;
#5847 = DIRECTION ( 'NONE',  ( -1.000000000000000000, 0.000000000000000000, -0.000000000000000000 ) ) ;
#5848 = CIRCLE ( 'NONE', #19021, 31.99999999999998934 ) ;
#5849 = PRESENTATION_STYLE_ASSIGNMENT (( #35512 ) ) ;
#5850 = CARTESIAN_POINT ( 'NONE',  ( 0.000000000000000000, -51.03279382321125723, 55.19960302592048862 ) ) ;
#5851 = LINE ( 'NONE', #12938, #60296 ) ;
#5852 = DIRECTION ( 'NONE',  ( -0.000000000000000000, -0.000000000000000000, 1.000000000000000000 ) ) ;
#5853 = CARTESIAN_POINT ( 'NONE',  ( 97.64999999999999147, -209.9999999999999716, 87.22187500173430408 ) ) ;
#5854 = DIRECTION ( 'NONE',  ( 0.000000000000000000, 0.000000000000000000, -1.000000000000000000 ) ) ;
#5855 = CIRCLE ( 'NONE', #67066, 82.00000000000000000 ) ;
#5856 = DIRECTION ( 'NONE',  ( -1.000000000000000000, 0.000000000000000000, 0.000000000000000000 ) ) ;
#5857 = AXIS2_PLACEMENT_3D ( 'NONE', #46657, #29713, #16426 ) ;
#5858 = ORIENTED_EDGE ( 'NONE', *, *, #65443, .T. ) ;
#5859 = CARTESIAN_POINT ( 'NONE',  ( -96.32499999999996021, -207.7050326799711968, 83.62354166840097491 ) ) ;
#5860 = ORIENTED_EDGE ( 'NONE', *, *, #50226, .F. ) ;
#5861 = CYLINDRICAL_SURFACE ( 'NONE', #67441, 37.49900000000000233 ) ;
#5862 = ORIENTED_EDGE ( 'NONE', *, *, #65859, .T. ) ;
#5864 = CARTESIAN_POINT ( 'NONE',  ( -97.65000000000001990, 91.52997821335253548, 77.96145833506763267 ) ) ;
#5863 = CARTESIAN_POINT ( 'NONE',  ( 93.67499999999999716, 87.70503267997126784, 79.39020833506762642 ) ) ;
#5865 = AXIS2_PLACEMENT_3D ( 'NONE', #51849, #63887, #34934 ) ;
#5866 = VERTEX_POINT ( 'NONE', #828 ) ;
#5867 = CARTESIAN_POINT ( 'NONE',  ( 97.30629616937498838, 91.33154071421968467, 81.28197916753381946 ) ) ;
#5868 = CARTESIAN_POINT ( 'NONE',  ( -3.000000000000000000, 5.835314593368477354, 22.81335362449854642 ) ) ;
#5869 = PRODUCT_DEFINITION ( 'UNKNOWN', '', #69968, #2599 ) ;
#5870 = DIRECTION ( 'NONE',  ( -1.000000000000000000, -0.000000000000000000, -0.000000000000000000 ) ) ;
#5871 = ADVANCED_FACE ( 'NONE', ( #12793 ), #57935, .T. ) ;
#5872 = CARTESIAN_POINT ( 'NONE',  ( -1.200000000000000030E-05, 0.9569279952884607310, 2.500000000000015543 ) ) ;
#5873 = LINE ( 'NONE', #40433, #3067 ) ;
#5874 = ORIENTED_EDGE ( 'NONE', *, *, #62309, .T. ) ;
#5875 = DIRECTION ( 'NONE',  ( -0.000000000000000000, -0.000000000000000000, 1.000000000000000000 ) ) ;
#5876 = DIRECTION ( 'NONE',  ( 0.9918136447140100120, -0.1276937514489704939, 0.000000000000000000 ) ) ;
#5877 = CARTESIAN_POINT ( 'NONE',  ( 10.00000000000000000, 37.22597642581158084, -5.202137450156524068 ) ) ;
#5878 = ORIENTED_EDGE ( 'NONE', *, *, #14323, .F. ) ;
#5879 = EDGE_CURVE ( 'NONE', #8621, #51903, #2724, .T. ) ;
#5880 = ORIENTED_EDGE ( 'NONE', *, *, #301, .T. ) ;
#5881 = EDGE_CURVE ( 'NONE', #2902, #43742, #53033, .T. ) ;
#5882 = VECTOR ( 'NONE', #16289, 1000.000000000000000 ) ;
#5883 = CYLINDRICAL_SURFACE ( 'NONE', #15596, 2.650000000000540812 ) ;
#5884 = FACE_OUTER_BOUND ( 'NONE', #17690, .T. ) ;
#5885 = CYLINDRICAL_SURFACE ( 'NONE', #38911, 2.649999999999985700 ) ;
#5886 = CARTESIAN_POINT ( 'NONE',  ( -92.69370383062498320, -208.6684592857803011, 80.64697916753382856 ) ) ;
#5887 = EDGE_CURVE ( 'NONE', #40700, #59084, #59613, .T. ) ;
#5888 = CIRCLE ( 'NONE', #59917, 31.99999999999999289 ) ;
#5889 = VERTEX_POINT ( 'NONE', #36106 ) ;
#5890 = VECTOR ( 'NONE', #47492, 1000.000000000000000 ) ;
#5891 = CARTESIAN_POINT ( 'NONE',  ( 10.00000000000000000, -44.88180994100421373, 63.18004540533011948 ) ) ;
#5892 = DIRECTION ( 'NONE',  ( -0.9730327541852497042, 0.2306669878475623159, 0.000000000000000000 ) ) ;
#5893 = AXIS2_PLACEMENT_3D ( 'NONE', #69937, #11679, #831 ) ;
#5894 = DIRECTION ( 'NONE',  ( -1.000000000000000000, 0.000000000000000000, -0.000000000000000000 ) ) ;
#5895 = CARTESIAN_POINT ( 'NONE',  ( 97.30629616937498838, 90.00000000000002842, 75.99031250086714806 ) ) ;
#5896 = VECTOR ( 'NONE', #50448, 1000.000000000000000 ) ;
#5897 = CARTESIAN_POINT ( 'NONE',  ( 0.000000000000000000, 51.03279382321088065, 55.19960302592086521 ) ) ;
#5898 = DIRECTION ( 'NONE',  ( 0.000000000000000000, 0.000000000000000000, 1.000000000000000000 ) ) ;
#5899 = CARTESIAN_POINT ( 'NONE',  ( 0.000000000000000000, -4.992566952385247170, 37.16516213103275845 ) ) ;
#5900 = CARTESIAN_POINT ( 'NONE',  ( 7.103376864691351012E-17, -120.0000000000000000, -64.00000000000000000 ) ) ;
#5901 = DIRECTION ( 'NONE',  ( 0.000000000000000000, -0.9876883405951358830, -0.1564344650402420822 ) ) ;
#5902 = EDGE_CURVE ( 'NONE', #23253, #37124, #24823, .T. ) ;
#5903 = DIRECTION ( 'NONE',  ( 0.000000000000000000, -0.9510565162951499785, -0.3090169943749582204 ) ) ;
#5904 = EDGE_CURVE ( 'NONE', #27052, #22824, #42800, .T. ) ;
#5905 = CARTESIAN_POINT ( 'NONE',  ( 96.15314808468748708, 88.00268892867053694, 88.10822916753382117 ) ) ;
#5906 = AXIS2_PLACEMENT_3D ( 'NONE', #20376, #38035, #19626 ) ;
#5907 = FACE_OUTER_BOUND ( 'NONE', #21100, .T. ) ;
#5908 = DIRECTION ( 'NONE',  ( 1.000000000000000000, 0.000000000000000000, 0.000000000000000000 ) ) ;
#5909 = AXIS2_PLACEMENT_3D ( 'NONE', #41722, #64664, #63935 ) ;
#5910 = ORIENTED_EDGE ( 'NONE', *, *, #73650, .F. ) ;
#5911 = DIRECTION ( 'NONE',  ( -1.000000000000000000, 0.000000000000000000, 0.000000000000000000 ) ) ;
#5912 = CARTESIAN_POINT ( 'NONE',  ( -97.30629616937501680, 88.66845928578038638, 80.80572916753379786 ) ) ;
#5913 = AXIS2_PLACEMENT_3D ( 'NONE', #70534, #20538, #66412 ) ;
#5914 = AXIS2_PLACEMENT_3D ( 'NONE', #72472, #61583, #21719 ) ;
#5915 = CARTESIAN_POINT ( 'NONE',  ( 10.00000000000000000, 0.000000000000000000, 0.000000000000000000 ) ) ;
#5916 = ORIENTED_EDGE ( 'NONE', *, *, #36345, .F. ) ;
#5917 = CIRCLE ( 'NONE', #47917, 42.00000000000000000 ) ;
#5918 = DIRECTION ( 'NONE',  ( -1.000000000000000000, 0.000000000000000000, 0.000000000000000000 ) ) ;
#5919 = FACE_OUTER_BOUND ( 'NONE', #16578, .T. ) ;
#5920 = DIRECTION ( 'NONE',  ( 0.000000000000000000, -0.5877852522924689183, -0.8090169943749504489 ) ) ;
#5921 = CARTESIAN_POINT ( 'NONE',  ( 0.000000000000000000, 0.000000000000000000, 0.000000000000000000 ) ) ;
#5922 = CARTESIAN_POINT ( 'NONE',  ( 96.15314808468748708, -208.0026889286704943, 76.88989583420048746 ) ) ;
#5923 = CARTESIAN_POINT ( 'NONE',  ( 5.999999999999999112, 2.543863470248399761, 81.96053171279903893 ) ) ;
#5924 = ORIENTED_EDGE ( 'NONE', *, *, #73686, .T. ) ;
#5925 = ORIENTED_EDGE ( 'NONE', *, *, #55880, .F. ) ;
#5926 = VECTOR ( 'NONE', #28580, 1000.000000000000000 ) ;
#5927 = CARTESIAN_POINT ( 'NONE',  ( 95.00000000000000000, -212.6630814284392557, 84.24531250086717193 ) ) ;
#5928 = CARTESIAN_POINT ( 'NONE',  ( 10.00000000000000000, 0.000000000000000000, 0.000000000000000000 ) ) ;
#5929 = CARTESIAN_POINT ( 'NONE',  ( -62.50000000000000000, 7.654042494670957804E-15, -270.0000000000000000 ) ) ;
#5930 = CARTESIAN_POINT ( 'NONE',  ( 97.65000000000003411, 91.52997821335250705, 82.75041666666666629 ) ) ;
#5931 = DIRECTION ( 'NONE',  ( -0.000000000000000000, 0.1045284632676569680, 0.9945218953682730678 ) ) ;
#5932 = VECTOR ( 'NONE', #15839, 1000.000000000000000 ) ;
#5933 = DIRECTION ( 'NONE',  ( -1.000000000000000000, -0.000000000000000000, 0.000000000000000000 ) ) ;
#5934 = CARTESIAN_POINT ( 'NONE',  ( 92.35000000000002274, -208.4700217866474645, 88.04208333333332348 ) ) ;
#5935 = AXIS2_PLACEMENT_3D ( 'NONE', #24851, #31229, #53429 ) ;
#5936 = EDGE_CURVE ( 'NONE', #26543, #32443, #52400, .T. ) ;
#5937 = ORIENTED_EDGE ( 'NONE', *, *, #59928, .F. ) ;
#5938 = ORIENTED_EDGE ( 'NONE', *, *, #61140, .F. ) ;
#5939 = AXIS2_PLACEMENT_3D ( 'NONE', #8152, #26555, #65679 ) ;
#5940 = ORIENTED_EDGE ( 'NONE', *, *, #8821, .F. ) ;
#5941 = ORIENTED_EDGE ( 'NONE', *, *, #61992, .T. ) ;
#5942 = AXIS2_PLACEMENT_3D ( 'NONE', #15017, #55618, #27790 ) ;
#5943 = SURFACE_STYLE_USAGE ( .BOTH. , #40137 ) ;
#5944 = CARTESIAN_POINT ( 'NONE',  ( -92.69370383062502583, 88.66845928578038638, 87.52614583420049144 ) ) ;
#5945 = DIRECTION ( 'NONE',  ( -1.000000000000000000, 0.000000000000000000, 0.000000000000000000 ) ) ;
#5946 = AXIS2_PLACEMENT_3D ( 'NONE', #11992, #34933, #52213 ) ;
#5947 = EDGE_CURVE ( 'NONE', #68980, #27978, #25200, .T. ) ;
#5948 = CARTESIAN_POINT ( 'NONE',  ( 10.00000000000000000, 0.000000000000000000, 0.000000000000000000 ) ) ;
#5949 = CARTESIAN_POINT ( 'NONE',  ( 95.00000000000000000, -206.9400435732949575, 75.95062500173428077 ) ) ;
#5950 = CARTESIAN_POINT ( 'NONE',  ( 92.34999999999999432, 88.47002178664753558, 78.62291666666668277 ) ) ;
#5951 = EDGE_CURVE ( 'NONE', #17707, #62900, #53398, .T. ) ;
#5952 = VERTEX_POINT ( 'NONE', #7897 ) ;
#5953 = CARTESIAN_POINT ( 'NONE',  ( 10.00000000000000000, 2.956366410620650420, 75.11725578898469280 ) ) ;
#5954 = ORIENTED_EDGE ( 'NONE', *, *, #56561, .T. ) ;
#5955 = CYLINDRICAL_SURFACE ( 'NONE', #24245, 2.649999999999985700 ) ;
#5956 = ORIENTED_EDGE ( 'NONE', *, *, #21030, .F. ) ;
#5957 = DIRECTION ( 'NONE',  ( -1.000000000000000000, -0.000000000000000000, 0.000000000000000000 ) ) ;
#5958 = CARTESIAN_POINT ( 'NONE',  ( -96.15314808468751551, 88.00268892867056536, 81.01739583420049939 ) ) ;
#5959 = CARTESIAN_POINT ( 'NONE',  ( 93.84685191531248449, 91.99731107132950569, 74.93197916753379673 ) ) ;
#5960 = VERTEX_POINT ( 'NONE', #59048 ) ;
#5961 = DIRECTION ( 'NONE',  ( -1.000000000000000000, 0.000000000000000000, -0.000000000000000000 ) ) ;
#5962 = EDGE_CURVE ( 'NONE', #4841, #69024, #40677, .T. ) ;
#5963 = FACE_OUTER_BOUND ( 'NONE', #2498, .T. ) ;
#5964 = AXIS2_PLACEMENT_3D ( 'NONE', #1918, #47007, #58648 ) ;
#5965 = CYLINDRICAL_SURFACE ( 'NONE', #11352, 77.49899999999999523 ) ;
#5966 = CARTESIAN_POINT ( 'NONE',  ( 95.00000000002596323, -209.9999999999999147, -74.99999999999349143 ) ) ;
#5967 = ORIENTED_EDGE ( 'NONE', *, *, #54804, .F. ) ;
#5968 = CARTESIAN_POINT ( 'NONE',  ( 12.00000000000000000, 16.61724383029390140, 20.69703378468902955 ) ) ;
#5969 = CIRCLE ( 'NONE', #44364, 31.99999999999999645 ) ;
#5971 = CARTESIAN_POINT ( 'NONE',  ( -96.15314808468747287, -208.0026889286704943, 78.10697916753380809 ) ) ;
#5970 = AXIS2_PLACEMENT_3D ( 'NONE', #54397, #21272, #10013 ) ;
#5972 = VERTEX_POINT ( 'NONE', #30816 ) ;
#5973 = VERTEX_POINT ( 'NONE', #70663 ) ;
#5974 = CARTESIAN_POINT ( 'NONE',  ( 12.00000000000000000, 0.000000000000000000, 0.000000000000000000 ) ) ;
#5975 = AXIS2_PLACEMENT_3D ( 'NONE', #43004, #65571, #2811 ) ;
#5976 = CIRCLE ( 'NONE', #73114, 77.49900000000000944 ) ;
#5977 = EDGE_LOOP ( 'NONE', ( #69618, #51795, #56041, #23463 ) ) ;
#5978 = LINE ( 'NONE', #34897, #56394 ) ;
#5979 = FACE_OUTER_BOUND ( 'NONE', #25092, .T. ) ;
#5980 = ORIENTED_EDGE ( 'NONE', *, *, #27683, .F. ) ;
#5981 = CARTESIAN_POINT ( 'NONE',  ( -97.30629616937497417, -208.6684592857803011, 76.25489583420049655 ) ) ;
#5982 = VERTEX_POINT ( 'NONE', #71778 ) ;
#5984 = EDGE_CURVE ( 'NONE', #11648, #29034, #52453, .T. ) ;
#5983 = DIRECTION ( 'NONE',  ( 0.000000000000000000, 0.000000000000000000, 1.000000000000000000 ) ) ;
#5985 = FACE_OUTER_BOUND ( 'NONE', #7155, .T. ) ;
#5986 = FACE_OUTER_BOUND ( 'NONE', #954, .T. ) ;
#5987 = ORIENTED_EDGE ( 'NONE', *, *, #8309, .F. ) ;
#5988 = FACE_OUTER_BOUND ( 'NONE', #39421, .T. ) ;
#5989 = CARTESIAN_POINT ( 'NONE',  ( 97.30629616937498838, 91.33154071421968467, 86.20322916753380582 ) ) ;
#5990 = CARTESIAN_POINT ( 'NONE',  ( -96.32499999999996021, -212.2949673200287179, 83.75583333333332803 ) ) ;
#5991 = CARTESIAN_POINT ( 'NONE',  ( -96.32500000000001705, 87.70503267997129626, 88.20083333333332121 ) ) ;
#5992 = CARTESIAN_POINT ( 'NONE',  ( 96.32499999999998863, -207.7050326799711968, 86.61333333333332973 ) ) ;
#5993 = CARTESIAN_POINT ( 'NONE',  ( 0.000000000000000000, 0.000000000000000000, 0.000000000000000000 ) ) ;
#5994 = DIRECTION ( 'NONE',  ( -1.000000000000000000, 0.000000000000000000, -0.000000000000000000 ) ) ;
#5995 = ADVANCED_FACE ( 'NONE', ( #13168 ), #2677, .T. ) ;
#5996 = CARTESIAN_POINT ( 'NONE',  ( 92.35000000030107969, -209.9999754409356854, 87.53856274002261273 ) ) ;
#5997 = LINE ( 'NONE', #39828, #39906 ) ;
#5998 = ADVANCED_FACE ( 'NONE', ( #65064 ), #36465, .T. ) ;
#5999 =( BOUNDED_CURVE ( )  B_SPLINE_CURVE ( 2, ( #28432, #17164, #67929, #34443, #10783, #40097, #44636 ),
 .UNSPECIFIED., .F., .F. ) 
 B_SPLINE_CURVE_WITH_KNOTS ( ( 3, 2, 2, 3 ),
 ( 0.8466920362409167122, 0.8537476304509593605, 0.8608033959918763856, 0.8678591737257297378 ),
 .UNSPECIFIED. ) 
 CURVE ( )  GEOMETRIC_REPRESENTATION_ITEM ( )  RATIONAL_B_SPLINE_CURVE ( ( 0.9999934937103009958, 0.8660286570082842417, 1.000000000000000000, 0.8660254037844387076, 1.000000000000000000, 0.8660254037844387076, 1.000000000000000000 ) ) 
 REPRESENTATION_ITEM ( '' )  );
#6000 = EDGE_CURVE ( 'NONE', #24873, #63128, #57246, .T. ) ;
#6001 = CARTESIAN_POINT ( 'NONE',  ( 12.13205353604972991, -140.1820037904669789, -5.500000000000000000 ) ) ;
#6002 = VECTOR ( 'NONE', #67434, 1000.000000000000000 ) ;
#6003 = CARTESIAN_POINT ( 'NONE',  ( 10.00000000000000000, 0.000000000000000000, 0.000000000000000000 ) ) ;
#6004 = AXIS2_PLACEMENT_3D ( 'NONE', #66961, #26733, #54946 ) ;
#6005 = CARTESIAN_POINT ( 'NONE',  ( -96.15314808468752972, 91.99731107132950569, 88.26697916753380468 ) ) ;
#6006 = CARTESIAN_POINT ( 'NONE',  ( -3.000000000000000000, 6.762365576493310826, 25.66652317338401090 ) ) ;
#6007 = AXIS2_PLACEMENT_3D ( 'NONE', #32849, #55799, #44147 ) ;
#6008 = CARTESIAN_POINT ( 'NONE',  ( 10.00000000000000000, 21.32104025579114648, 30.84782396557224970 ) ) ;
#6009 =( BOUNDED_CURVE ( )  B_SPLINE_CURVE ( 2, ( #66695, #53941, #2479, #36268, #70839, #36632, #43418 ),
 .UNSPECIFIED., .F., .F. ) 
 B_SPLINE_CURVE_WITH_KNOTS ( ( 3, 2, 2, 3 ),
 ( 0.5000000000000000000, 0.5069444444444444198, 0.5138888888888887285, 0.5208333333333332593 ),
 .UNSPECIFIED. ) 
 CURVE ( )  GEOMETRIC_REPRESENTATION_ITEM ( )  RATIONAL_B_SPLINE_CURVE ( ( 1.000000000000000000, 0.8660254037844387076, 1.000000000000000000, 0.8660254037844387076, 1.000000000000000000, 0.8660254037844408170, 0.9999999999999978906 ) ) 
 REPRESENTATION_ITEM ( '' )  );
#6010 = CARTESIAN_POINT ( 'NONE',  ( -96.32500000000001705, 92.29496732002878900, 77.19416666666666060 ) ) ;
#6011 = DIRECTION ( 'NONE',  ( -1.000000000000000000, -0.000000000000000000, -0.000000000000000000 ) ) ;
#6012 = CARTESIAN_POINT ( 'NONE',  ( 15.00000000000000000, -4.261787119644963262, 26.19803753235780164 ) ) ;
#6013 = CYLINDRICAL_SURFACE ( 'NONE', #28351, 77.49899999999999523 ) ;
#6014 = VECTOR ( 'NONE', #65712, 1000.000000000000114 ) ;
#6015 = AXIS2_PLACEMENT_3D ( 'NONE', #61793, #15919, #62159 ) ;
#6016 = AXIS2_PLACEMENT_3D ( 'NONE', #27678, #11131, #4774 ) ;
#6017 = CARTESIAN_POINT ( 'NONE',  ( 96.15314808468748708, -208.0026889286704943, 87.04989583420048405 ) ) ;
#6018 = ORIENTED_EDGE ( 'NONE', *, *, #36475, .T. ) ;
#6019 = VECTOR ( 'NONE', #1258, 1000.000000000000000 ) ;
#6020 = ORIENTED_EDGE ( 'NONE', *, *, #7544, .F. ) ;
#6021 = VECTOR ( 'NONE', #9682, 1000.000000000000114 ) ;
#6022 = DIRECTION ( 'NONE',  ( 1.000000000000000000, 0.000000000000000000, 0.000000000000000000 ) ) ;
#6023 = EDGE_LOOP ( 'NONE', ( #15414, #37830, #40484, #13524 ) ) ;
#6024 = CARTESIAN_POINT ( 'NONE',  ( -3.000000000000000000, 9.615535125379096826, -24.73947219025905042 ) ) ;
#6025 = CARTESIAN_POINT ( 'NONE',  ( 96.48680242707320076, -208.1953243530631994, 74.81083481226637844 ) ) ;
#6026 = ORIENTED_EDGE ( 'NONE', *, *, #50909, .F. ) ;
#6027 = CARTESIAN_POINT ( 'NONE',  ( 97.30629616937498838, -208.6684592857803011, 82.55197916753382970 ) ) ;
#6028 = EDGE_CURVE ( 'NONE', #1496, #49408, #36837, .T. ) ;
#6029 = VERTEX_POINT ( 'NONE', #66174 ) ;
#6030 = CARTESIAN_POINT ( 'NONE',  ( -7.500000000000015987, -76.30000000000001137, -204.9999999999999716 ) ) ;
#6031 = ORIENTED_EDGE ( 'NONE', *, *, #50053, .F. ) ;
#6032 = EDGE_LOOP ( 'NONE', ( #37727, #11218, #1518, #21287, #50002 ) ) ;
#6033 = FACE_OUTER_BOUND ( 'NONE', #25542, .T. ) ;
#6034 = UNCERTAINTY_MEASURE_WITH_UNIT (LENGTH_MEASURE( 1.000000000000000082E-05 ), #60719, 'distance_accuracy_value', 'NONE');
#6035 = DIRECTION ( 'NONE',  ( 0.000000000000000000, 0.000000000000000000, -1.000000000000000000 ) ) ;
#6036 = EDGE_CURVE ( 'NONE', #39875, #73588, #14023, .T. ) ;
#6037 = ORIENTED_EDGE ( 'NONE', *, *, #44770, .F. ) ;
#6038 = CARTESIAN_POINT ( 'NONE',  ( 97.64999999999999147, -209.9999999999999716, 86.58687500173429896 ) ) ;
#6039 = EDGE_CURVE ( 'NONE', #52228, #72105, #30823, .T. ) ;
#6040 = ORIENTED_EDGE ( 'NONE', *, *, #33252, .T. ) ;
#6041 = CARTESIAN_POINT ( 'NONE',  ( 0.000000000000000000, -8.840884882375609877, 74.65374052328647281 ) ) ;
#6042 = EDGE_LOOP ( 'NONE', ( #43040, #37058, #6629, #52785 ) ) ;
#6043 = CARTESIAN_POINT ( 'NONE',  ( 5.000000000000000000, -2.058885705017528878, -1.328630925609301183 ) ) ;
#6044 = CIRCLE ( 'NONE', #51645, 31.99999999999999289 ) ;
#6045 = ORIENTED_EDGE ( 'NONE', *, *, #32015, .T. ) ;
#6046 = EDGE_CURVE ( 'NONE', #32186, #27271, #20016, .T. ) ;
#6047 = VECTOR ( 'NONE', #41113, 1000.000000000000114 ) ;
#6048 = ORIENTED_EDGE ( 'NONE', *, *, #51684, .T. ) ;
#6049 = ORIENTED_EDGE ( 'NONE', *, *, #70578, .T. ) ;
#6050 = DIRECTION ( 'NONE',  ( 0.6862798483830533369, 0.7273375899149812085, 0.000000000000000000 ) ) ;
#6051 = CARTESIAN_POINT ( 'NONE',  ( -10.00000000000000000, 0.000000000000000000, 0.000000000000000000 ) ) ;
#6052 = ORIENTED_EDGE ( 'NONE', *, *, #29797, .F. ) ;
#6053 = ORIENTED_EDGE ( 'NONE', *, *, #51264, .T. ) ;
#6054 = VECTOR ( 'NONE', #48125, 1000.000000000000000 ) ;
#6055 = ORIENTED_EDGE ( 'NONE', *, *, #46328, .F. ) ;
#6056 = CARTESIAN_POINT ( 'NONE',  ( 0.000000000000000000, 36.72794159290334903, -65.59268652807170952 ) ) ;
#6057 = CARTESIAN_POINT ( 'NONE',  ( 11.99999999999999822, 0.000000000000000000, 0.000000000000000000 ) ) ;
#6058 = CARTESIAN_POINT ( 'NONE',  ( -96.32500000000001705, 92.29496732002878900, 86.08416666666666117 ) ) ;
#6059 = VERTEX_POINT ( 'NONE', #33412 ) ;
#6060 = DIRECTION ( 'NONE',  ( -0.000000000000000000, -0.000000000000000000, 1.000000000000000000 ) ) ;
#6061 = VERTEX_POINT ( 'NONE', #21775 ) ;
#6062 = FACE_OUTER_BOUND ( 'NONE', #16947, .T. ) ;
#6063 = CARTESIAN_POINT ( 'NONE',  ( -92.69370383062498320, -208.6684592857803011, 86.83822916753381094 ) ) ;
#6064 = EDGE_LOOP ( 'NONE', ( #1293, #7957, #7204, #69285 ) ) ;
#6066 = EDGE_CURVE ( 'NONE', #53345, #51292, #55616, .T. ) ;
#6065 = FACE_OUTER_BOUND ( 'NONE', #16174, .T. ) ;
#6067 = DIRECTION ( 'NONE',  ( 0.000000000000000000, 0.000000000000000000, 1.000000000000000000 ) ) ;
#6068 = LINE ( 'NONE', #28974, #70469 ) ;
#6069 = CARTESIAN_POINT ( 'NONE',  ( -97.30629616937497417, -211.3315407142195852, 76.36072916753381890 ) ) ;
#6070 = CIRCLE ( 'NONE', #32428, 77.49899999999999523 ) ;
#6071 = CARTESIAN_POINT ( 'NONE',  ( 10.00000000000000000, 0.000000000000000000, 0.000000000000000000 ) ) ;
#6072 = FACE_OUTER_BOUND ( 'NONE', #13134, .T. ) ;
#6073 = CIRCLE ( 'NONE', #15662, 11.59999999999999787 ) ;
#6074 = DIRECTION ( 'NONE',  ( -1.000000000000000000, 0.000000000000000000, -0.000000000000000000 ) ) ;
#6075 = AXIS2_PLACEMENT_3D ( 'NONE', #58626, #34584, #46246 ) ;
#6076 = AXIS2_PLACEMENT_3D ( 'NONE', #52485, #39188, #50824 ) ;
#6077 = CARTESIAN_POINT ( 'NONE',  ( -96.32500000000001705, 92.29496732002878900, 76.55916666666666970 ) ) ;
#6078 = DIRECTION ( 'NONE',  ( -1.000000000000000000, 0.000000000000000000, 0.000000000000000000 ) ) ;
#6079 = EDGE_CURVE ( 'NONE', #46417, #11359, #34428, .T. ) ;
#6080 = CARTESIAN_POINT ( 'NONE',  ( -97.30629616937501680, 91.33154071421968467, 78.15989583420048348 ) ) ;
#6081 = CARTESIAN_POINT ( 'NONE',  ( -10.00000000000000000, 0.000000000000000000, 0.000000000000000000 ) ) ;
#6082 = DIRECTION ( 'NONE',  ( 0.000000000000000000, 0.3090169943749410675, 0.9510565162951556406 ) ) ;
#6083 = EDGE_CURVE ( 'NONE', #70179, #69749, #66839, .T. ) ;
#6084 = ORIENTED_EDGE ( 'NONE', *, *, #55163, .F. ) ;
#6085 = CARTESIAN_POINT ( 'NONE',  ( 94.99999999999998579, 86.94004357329502852, 79.44312500173430180 ) ) ;
#6086 = DIRECTION ( 'NONE',  ( -1.000000000000000000, -0.000000000000000000, -0.000000000000000000 ) ) ;
#6087 = CARTESIAN_POINT ( 'NONE',  ( 97.64999999999999147, -210.0000001051138270, 86.58687499784845443 ) ) ;
#6088 = DIRECTION ( 'NONE',  ( 0.000000000000000000, 0.9135454576426005335, 0.4067366430758010409 ) ) ;
#6089 = DIRECTION ( 'NONE',  ( -1.000000000000000000, -0.000000000000000000, 0.000000000000000000 ) ) ;
#6090 = CARTESIAN_POINT ( 'NONE',  ( -92.35000000000005116, 91.52997821335253548, 85.36979166840096411 ) ) ;
#6091 = CARTESIAN_POINT ( 'NONE',  ( -94.99999999999997158, -207.3369185715606307, 75.67281250086716682 ) ) ;
#6092 = CYLINDRICAL_SURFACE ( 'NONE', #6844, 2.649999999999985700 ) ;
#6093 = ORIENTED_EDGE ( 'NONE', *, *, #48448, .F. ) ;
#6094 = DIRECTION ( 'NONE',  ( -1.000000000000000000, 0.000000000000000000, 0.000000000000000000 ) ) ;
#6095 = CARTESIAN_POINT ( 'NONE',  ( -97.64999999990727986, 90.00001381026693537, 80.55392363656929433 ) ) ;
#6096 = CARTESIAN_POINT ( 'NONE',  ( 0.000000000000000000, 2.935248768560057897, -3.252606517456513302E-15 ) ) ;
#6097 = LINE ( 'NONE', #63612, #28139 ) ;
#6098 = AXIS2_PLACEMENT_3D ( 'NONE', #40549, #28899, #40189 ) ;
#6099 = VECTOR ( 'NONE', #34440, 1000.000000000000114 ) ;
#6100 = AXIS2_PLACEMENT_3D ( 'NONE', #62365, #33015, #28488 ) ;
#6101 = FACE_OUTER_BOUND ( 'NONE', #65148, .T. ) ;
#6102 = ORIENTED_EDGE ( 'NONE', *, *, #47024, .T. ) ;
#6103 = DIRECTION ( 'NONE',  ( -1.000000000000000000, 0.000000000000000000, -0.000000000000000000 ) ) ;
#6104 = DIRECTION ( 'NONE',  ( 0.000000000000000000, 0.4067366430758010409, 0.9135454576426005335 ) ) ;
#6105 = VERTEX_POINT ( 'NONE', #39076 ) ;
#6106 = CARTESIAN_POINT ( 'NONE',  ( 95.00000000000000000, -207.3369185715606307, 88.84906250086713442 ) ) ;
#6107 = DIRECTION ( 'NONE',  ( 0.000000000000000000, 0.000000000000000000, -1.000000000000000000 ) ) ;
#6108 = ORIENTED_EDGE ( 'NONE', *, *, #15242, .F. ) ;
#6109 = EDGE_CURVE ( 'NONE', #51433, #29098, #23645, .T. ) ;
#6110 = CYLINDRICAL_SURFACE ( 'NONE', #58487, 31.99999999999998579 ) ;
#6111 = AXIS2_PLACEMENT_3D ( 'NONE', #23711, #51910, #68097 ) ;
#6112 = ORIENTED_EDGE ( 'NONE', *, *, #73907, .T. ) ;
#6113 = CARTESIAN_POINT ( 'NONE',  ( 4.999999999999999112, 40.68715046381943523, -10.41901085202036370 ) ) ;
#6114 = VERTEX_POINT ( 'NONE', #38704 ) ;
#6115 = AXIS2_PLACEMENT_3D ( 'NONE', #34803, #629, #41547 ) ;
#6116 = DIRECTION ( 'NONE',  ( -1.000000000000000000, -0.000000000000000000, -0.000000000000000000 ) ) ;
#6117 = EDGE_CURVE ( 'NONE', #74276, #31156, #58417, .T. ) ;
#6118 = VECTOR ( 'NONE', #45449, 1000.000000000000114 ) ;
#6119 = EDGE_LOOP ( 'NONE', ( #36901, #50843, #16812, #55753 ) ) ;
#6120 = DIRECTION ( 'NONE',  ( -0.000000000000000000, -0.000000000000000000, 1.000000000000000000 ) ) ;
#6121 = ORIENTED_EDGE ( 'NONE', *, *, #14142, .T. ) ;
#6122 = AXIS2_PLACEMENT_3D ( 'NONE', #64241, #35642, #25115 ) ;
#6123 = EDGE_CURVE ( 'NONE', #62092, #70160, #73637, .T. ) ;
#6124 = VERTEX_POINT ( 'NONE', #22155 ) ;
#6125 = CARTESIAN_POINT ( 'NONE',  ( 11.99999999999999822, 17.28742895386084655, 75.54627589209950145 ) ) ;
#6126 = VERTEX_POINT ( 'NONE', #33044 ) ;
#6127 = ORIENTED_EDGE ( 'NONE', *, *, #14016, .F. ) ;
#6128 = CARTESIAN_POINT ( 'NONE',  ( 92.48632958231164025, 89.99999999999990052, 74.91808492278045151 ) ) ;
#6129 = ORIENTED_EDGE ( 'NONE', *, *, #36563, .T. ) ;
#6130 = ADVANCED_FACE ( 'NONE', ( #45095 ), #4137, .T. ) ;
#6131 = ORIENTED_EDGE ( 'NONE', *, *, #17745, .F. ) ;
#6132 = CARTESIAN_POINT ( 'NONE',  ( 92.69370383062498320, 90.00000000000002842, 83.92781250086714806 ) ) ;
#6133 = ORIENTED_EDGE ( 'NONE', *, *, #21709, .F. ) ;
#6134 = CARTESIAN_POINT ( 'NONE',  ( 93.84685191531249870, -208.0026889286704943, 83.18697916753382060 ) ) ;
#6135 = APPLICATION_PROTOCOL_DEFINITION ( 'draft international standard', 'automotive_design', 1998, #1897 ) ;
#6136 = CARTESIAN_POINT ( 'NONE',  ( -92.35000000000547971, -210.0000054026037049, 81.50687481489497088 ) ) ;
#6137 = CARTESIAN_POINT ( 'NONE',  ( -97.65000000000001990, 90.00000000000004263, 84.28499999999999659 ) ) ;
#6138 = CARTESIAN_POINT ( 'NONE',  ( 0.000000000000000000, 0.000000000000000000, 125.0000000000000000 ) ) ;
#6139 = DIRECTION ( 'NONE',  ( -0.000000000000000000, -0.000000000000000000, 1.000000000000000000 ) ) ;
#6140 = CARTESIAN_POINT ( 'NONE',  ( 3.000000000000000000, 3.673940397442059868E-16, -5.974599999999999689 ) ) ;
#6141 = CARTESIAN_POINT ( 'NONE',  ( 10.00000000000000000, 0.000000000000000000, 0.000000000000000000 ) ) ;
#6142 = CARTESIAN_POINT ( 'NONE',  ( -93.84685191531247028, -211.9973110713294489, 84.77447916753381207 ) ) ;
#6143 = CARTESIAN_POINT ( 'NONE',  ( -92.69370383062502583, 91.33154071421968467, 83.18697916753382060 ) ) ;
#6144 = ORIENTED_EDGE ( 'NONE', *, *, #37130, .T. ) ;
#6145 = EDGE_CURVE ( 'NONE', #73479, #34939, #53643, .T. ) ;
#6147 = CARTESIAN_POINT ( 'NONE',  ( -97.30629616937501680, 88.66845928578038638, 83.98072916753380923 ) ) ;
#6146 = CARTESIAN_POINT ( 'NONE',  ( 92.69370383062498320, 91.33154071421968467, 83.23989583420046756 ) ) ;
#6148 = VERTEX_POINT ( 'NONE', #61267 ) ;
#6149 = CARTESIAN_POINT ( 'NONE',  ( 0.000000000000000000, -41.91543099594816368, -2.663952781846588014 ) ) ;
#6151 = EDGE_CURVE ( 'NONE', #65031, #20728, #33802, .T. ) ;
#6150 = CARTESIAN_POINT ( 'NONE',  ( 92.35000000000000853, -209.9999999999999716, 79.20499999999999829 ) ) ;
#6152 = LINE ( 'NONE', #53108, #25932 ) ;
#6153 = DIRECTION ( 'NONE',  ( 1.000000000000000000, 0.000000000000000000, 0.000000000000000000 ) ) ;
#6154 = CARTESIAN_POINT ( 'NONE',  ( -97.30629616937495996, -209.9999999999999716, 87.73781250086713612 ) ) ;
#6155 = FACE_OUTER_BOUND ( 'NONE', #2168, .T. ) ;
#6156 = CIRCLE ( 'NONE', #13313, 37.49900000000000233 ) ;
#6157 = CARTESIAN_POINT ( 'NONE',  ( 10.00000000000000000, 0.000000000000000000, 0.000000000000000000 ) ) ;
#6158 = CARTESIAN_POINT ( 'NONE',  ( -94.99999999999997158, -209.9999999999999716, 90.00000000000000000 ) ) ;
#6159 = AXIS2_PLACEMENT_3D ( 'NONE', #19725, #26483, #49775 ) ;
#6160 = EDGE_CURVE ( 'NONE', #53009, #64628, #68015, .T. ) ;
#6161 = EDGE_CURVE ( 'NONE', #30392, #55889, #55985, .T. ) ;
#6162 = DIRECTION ( 'NONE',  ( 0.000000000000000000, 0.9510565162951546414, -0.3090169943749442871 ) ) ;
#6163 = ORIENTED_EDGE ( 'NONE', *, *, #71614, .T. ) ;
#6164 = ORIENTED_EDGE ( 'NONE', *, *, #38786, .F. ) ;
#6165 = CARTESIAN_POINT ( 'NONE',  ( -92.35000000000005116, 91.52997821335253548, 79.57541666666665492 ) ) ;
#6166 = CARTESIAN_POINT ( 'NONE',  ( 93.67500000000001137, -212.2949673200287179, 88.83583333333334053 ) ) ;
#6167 = EDGE_CURVE ( 'NONE', #33089, #35131, #8024, .T. ) ;
#6168 = CARTESIAN_POINT ( 'NONE',  ( 0.000000000000000000, 0.000000000000000000, 20.00000000000000000 ) ) ;
#6169 = CARTESIAN_POINT ( 'NONE',  ( 93.67499999999998295, 92.29496732002878900, 76.55916666666666970 ) ) ;
#6170 = DIRECTION ( 'NONE',  ( -1.000000000000000000, 0.000000000000000000, 0.000000000000000000 ) ) ;
#6171 = CARTESIAN_POINT ( 'NONE',  ( -2.500000000000015543, -73.00000000000001421, -204.9999999999999716 ) ) ;
#6172 = ORIENTED_EDGE ( 'NONE', *, *, #4168, .F. ) ;
#6173 = CARTESIAN_POINT ( 'NONE',  ( -92.69370383062502583, 91.33154071421968467, 77.94822916753381037 ) ) ;
#6174 = EDGE_CURVE ( 'NONE', #50325, #12497, #74030, .T. ) ;
#6175 = FACE_OUTER_BOUND ( 'NONE', #34393, .T. ) ;
#6176 = CIRCLE ( 'NONE', #12154, 31.99999999999998579 ) ;
#6177 = CARTESIAN_POINT ( 'NONE',  ( 10.00000000000000000, 0.000000000000000000, 0.000000000000000000 ) ) ;
#6178 = AXIS2_PLACEMENT_3D ( 'NONE', #33588, #39989, #39246 ) ;
#6179 = DIRECTION ( 'NONE',  ( 0.000000000000000000, -0.7071067811865536790, 0.7071067811865414665 ) ) ;
#6180 = CARTESIAN_POINT ( 'NONE',  ( 0.000000000000000000, -120.0000000000000000, -5.500000000000000000 ) ) ;
#6181 = FACE_OUTER_BOUND ( 'NONE', #554, .T. ) ;
#6182 = CARTESIAN_POINT ( 'NONE',  ( -97.30629616937497417, -211.3315407142195852, 86.04447916753382231 ) ) ;
#6183 = VECTOR ( 'NONE', #53050, 1000.000000000000000 ) ;
#6184 = CARTESIAN_POINT ( 'NONE',  ( 96.15314808468748708, 91.99731107132950569, 76.25489583420049655 ) ) ;
#6185 = CARTESIAN_POINT ( 'NONE',  ( -96.15314808468745866, -211.9973110713294489, 79.11239583420048405 ) ) ;
#6186 = CARTESIAN_POINT ( 'NONE',  ( -97.64998927049497013, 91.52998440803517610, 84.94645790656221607 ) ) ;
#6187 = ORIENTED_EDGE ( 'NONE', *, *, #46121, .T. ) ;
#6188 = CARTESIAN_POINT ( 'NONE',  ( 92.34999999999998010, 90.00002803130637119, 87.53937403222812463 ) ) ;
#6189 = CARTESIAN_POINT ( 'NONE',  ( 10.00000000000000000, -26.02418014898359289, 70.52718814184250107 ) ) ;
#6190 = CARTESIAN_POINT ( 'NONE',  ( 10.00000000000000000, 14.66109333815460225, 73.73191006444577056 ) ) ;
#6191 = CARTESIAN_POINT ( 'NONE',  ( -97.30629616937501680, 88.66845928578038638, 75.88447916753382572 ) ) ;
#6192 = CARTESIAN_POINT ( 'NONE',  ( 92.69370383062501162, -208.6684592857803011, 77.52489583420046415 ) ) ;
#6193 = ORIENTED_EDGE ( 'NONE', *, *, #57591, .F. ) ;
#6194 = LINE ( 'NONE', #16347, #44271 ) ;
#6195 = ORIENTED_EDGE ( 'NONE', *, *, #30449, .T. ) ;
#6196 = CARTESIAN_POINT ( 'NONE',  ( 10.00000000000000000, 44.88180994100468268, -63.18004540532978552 ) ) ;
#6197 = ORIENTED_EDGE ( 'NONE', *, *, #7880, .F. ) ;
#6198 = AXIS2_PLACEMENT_3D ( 'NONE', #66606, #66963, #38029 ) ;
#6199 = EDGE_CURVE ( 'NONE', #73126, #5572, #48859, .T. ) ;
#6201 = CIRCLE ( 'NONE', #31343, 82.00000000000000000 ) ;
#6200 = DIRECTION ( 'NONE',  ( -1.000000000000000000, 0.000000000000000000, 0.000000000000000000 ) ) ;
#6202 = EDGE_CURVE ( 'NONE', #19951, #15157, #54815, .T. ) ;
#6203 = CIRCLE ( 'NONE', #2632, 31.99999999999998579 ) ;
#6204 = ORIENTED_EDGE ( 'NONE', *, *, #17311, .T. ) ;
#6205 = VERTEX_POINT ( 'NONE', #67274 ) ;
#6207 = ORIENTED_EDGE ( 'NONE', *, *, #27418, .T. ) ;
#6206 = EDGE_CURVE ( 'NONE', #37368, #3856, #61635, .T. ) ;
#6208 = ADVANCED_FACE ( 'NONE', ( #27405 ), #50340, .T. ) ;
#6209 = CARTESIAN_POINT ( 'NONE',  ( 92.35002740377132113, -208.4700059650727155, 79.86645724064028684 ) ) ;
#6210 = VECTOR ( 'NONE', #10753, 1000.000000000000000 ) ;
#6211 = ORIENTED_EDGE ( 'NONE', *, *, #34277, .F. ) ;
#6212 = ORIENTED_EDGE ( 'NONE', *, *, #16970, .T. ) ;
#6213 =( BOUNDED_CURVE ( )  B_SPLINE_CURVE ( 2, ( #33639, #73481, #56955, #5464, #44935, #67857, #69331, #40390, #68972 ),
 .UNSPECIFIED., .F., .F. ) 
 B_SPLINE_CURVE_WITH_KNOTS ( ( 3, 2, 2, 2, 3 ),
 ( 0.08466915177933910519, 0.08466918649100467487, 0.09172495203192151947, 0.09878071757283837795, 0.1058364832028025337 ),
 .UNSPECIFIED. ) 
 CURVE ( )  GEOMETRIC_REPRESENTATION_ITEM ( )  RATIONAL_B_SPLINE_CURVE ( ( 0.9999986817990271781, 0.9999993408962710717, 1.000000000000000000, 0.8660254037844387076, 1.000000000000000000, 0.8660254037844387076, 1.000000000000000000, 0.8660254037844387076, 1.000000000000000000 ) ) 
 REPRESENTATION_ITEM ( '' )  );
#6214 = CARTESIAN_POINT ( 'NONE',  ( 92.69370383062498320, 90.00000000000002842, 82.18156250086715886 ) ) ;
#6215 = CARTESIAN_POINT ( 'NONE',  ( 93.67500000000001137, -212.2949673200287179, 75.50083333333331836 ) ) ;
#6216 = ORIENTED_EDGE ( 'NONE', *, *, #34103, .T. ) ;
#6217 = ORIENTED_EDGE ( 'NONE', *, *, #15773, .T. ) ;
#6218 = ORIENTED_EDGE ( 'NONE', *, *, #25806, .F. ) ;
#6219 = VERTEX_POINT ( 'NONE', #22909 ) ;
#6220 = LINE ( 'NONE', #29120, #41871 ) ;
#6221 = VECTOR ( 'NONE', #44219, 1000.000000000000000 ) ;
#6222 = DIRECTION ( 'NONE',  ( 0.000000000000000000, 0.000000000000000000, 1.000000000000000000 ) ) ;
#6223 = CARTESIAN_POINT ( 'NONE',  ( -96.32500000000001705, 87.70503267997129626, 87.56583333333333030 ) ) ;
#6224 = CARTESIAN_POINT ( 'NONE',  ( 15.69955575014744831, 0.001194404164628767254, -90.00000000000000000 ) ) ;
#6225 = DIRECTION ( 'NONE',  ( 0.000000000000000000, 0.000000000000000000, 1.000000000000000000 ) ) ;
#6226 = AXIS2_PLACEMENT_3D ( 'NONE', #24655, #47586, #41955 ) ;
#6227 = CARTESIAN_POINT ( 'NONE',  ( 11.99999999999999822, 0.000000000000000000, 0.000000000000000000 ) ) ;
#6228 = CARTESIAN_POINT ( 'NONE',  ( 11.99999999999999822, -8.840884882375609877, 74.65374052328647281 ) ) ;
#6229 = EDGE_CURVE ( 'NONE', #72554, #24755, #46204, .T. ) ;
#6230 = CARTESIAN_POINT ( 'NONE',  ( 97.64999999999999147, 89.99999997442942856, 84.04687500080852658 ) ) ;
#6231 = VERTEX_POINT ( 'NONE', #39825 ) ;
#6232 = CARTESIAN_POINT ( 'NONE',  ( -97.64999999999994884, -211.5299782133524502, 80.60729166840097548 ) ) ;
#6233 = ORIENTED_EDGE ( 'NONE', *, *, #39, .T. ) ;
#6234 = DIRECTION ( 'NONE',  ( -1.000000000000000000, 7.571541139944061634E-15, 2.603472992745718826E-14 ) ) ;
#6235 = EDGE_LOOP ( 'NONE', ( #48527, #66152, #48103, #64168 ) ) ;
#6237 = CARTESIAN_POINT ( 'NONE',  ( -97.65000000000001990, 88.47002178664754979, 79.97229166840095615 ) ) ;
#6236 = CARTESIAN_POINT ( 'NONE',  ( 94.99999999999998579, 86.94004357329500010, 78.80812500173429669 ) ) ;
#6238 = ORIENTED_EDGE ( 'NONE', *, *, #37519, .T. ) ;
#6239 = CARTESIAN_POINT ( 'NONE',  ( 92.69370383062498320, 91.33154071421968467, 81.49364583420047836 ) ) ;
#6240 = CARTESIAN_POINT ( 'NONE',  ( -92.34999999999999432, -209.9999999999999716, 80.79249999999998977 ) ) ;
#6241 = DIRECTION ( 'NONE',  ( -1.000000000000000000, 0.000000000000000000, 0.000000000000000000 ) ) ;
#6242 = CARTESIAN_POINT ( 'NONE',  ( 22.08297821871651934, -111.8242998470044540, 5.500000000000000000 ) ) ;
#6243 = FACE_OUTER_BOUND ( 'NONE', #46420, .T. ) ;
#6244 = EDGE_LOOP ( 'NONE', ( #72557, #32737, #74039, #58146 ) ) ;
#6245 = CARTESIAN_POINT ( 'NONE',  ( -92.35000000000000853, 91.52997821335252127, 80.21041666666666003 ) ) ;
#6246 = FACE_OUTER_BOUND ( 'NONE', #60862, .T. ) ;
#6247 = EDGE_CURVE ( 'NONE', #64554, #53358, #12342, .T. ) ;
#6248 = EDGE_CURVE ( 'NONE', #54778, #36975, #6711, .T. ) ;
#6249 = DIRECTION ( 'NONE',  ( 0.6862798483830534479, 0.7273375899149810975, 0.000000000000000000 ) ) ;
#6250 = ORIENTED_EDGE ( 'NONE', *, *, #6151, .F. ) ;
#6251 = EDGE_LOOP ( 'NONE', ( #47646, #57508, #45544, #63264, #49651, #8413, #41828, #63640, #58565, #38533, #35267, #71307, #3161, #46051, #61590, #59356, #50128, #31007, #69791, #24334, #20566, #25496, #16925, #36521, #71280, #2627, #39672, #33216, #55725, #23896, #71919, #31164, #40056, #24597, #73407, #48906, #62536, #69634, #15059, #61128, #54822, #55603, #73999, #70879, #50272, #23849, #48908, #2259, #4788, #72488 ) ) ;
#6252 = CARTESIAN_POINT ( 'NONE',  ( 23.11608002360578240, -124.4885236261218182, 5.500000000000000000 ) ) ;
#6253 = CARTESIAN_POINT ( 'NONE',  ( 10.00000000000000000, -27.05870788708213226, -26.08949754953053102 ) ) ;
#6254 = CARTESIAN_POINT ( 'NONE',  ( -94.99999999999997158, -206.9400435732949575, 75.87125000000000341 ) ) ;
#6255 = CARTESIAN_POINT ( 'NONE',  ( -97.30629616937495996, -209.9999999999999716, 76.46656250086715545 ) ) ;
#6256 = ORIENTED_EDGE ( 'NONE', *, *, #27249, .T. ) ;
#6257 =( GEOMETRIC_REPRESENTATION_CONTEXT ( 3 ) GLOBAL_UNCERTAINTY_ASSIGNED_CONTEXT ( ( #21885 ) ) GLOBAL_UNIT_ASSIGNED_CONTEXT ( ( #65167, #25668, #59016 ) ) REPRESENTATION_CONTEXT ( 'NONE', 'WORKASPACE' ) );
#6258 = VECTOR ( 'NONE', #50329, 1000.000000000000000 ) ;
#6259 = DIRECTION ( 'NONE',  ( 0.000000000000000000, 0.000000000000000000, 1.000000000000000000 ) ) ;
#6260 = LINE ( 'NONE', #22429, #28685 ) ;
#6261 = AXIS2_PLACEMENT_3D ( 'NONE', #64685, #14648, #60173 ) ;
#6262 = CARTESIAN_POINT ( 'NONE',  ( 11.99999999999999822, -46.54456581323847786, 59.03342792756247093 ) ) ;
#6263 = CARTESIAN_POINT ( 'NONE',  ( 92.69370383062498320, 88.66845928578035796, 75.09072916753380866 ) ) ;
#6264 = CYLINDRICAL_SURFACE ( 'NONE', #66469, 37.49900000000000233 ) ;
#6265 = DIRECTION ( 'NONE',  ( 0.000000000000000000, 0.000000000000000000, 1.000000000000000000 ) ) ;
#6266 = DIRECTION ( 'NONE',  ( -0.8541291221503266584, 0.5200609990133008287, 0.000000000000000000 ) ) ;
#6267 = DIRECTION ( 'NONE',  ( 0.000000000000000000, 0.5877852522924743583, -0.8090169943749465631 ) ) ;
#6268 = CARTESIAN_POINT ( 'NONE',  ( 10.00000000000000000, -35.53030884539094103, 12.26510123303246935 ) ) ;
#6269 = CARTESIAN_POINT ( 'NONE',  ( 0.000000000000000000, 10.96151621346487914, 35.95386929396260456 ) ) ;
#6270 = AXIS2_PLACEMENT_3D ( 'NONE', #15564, #55412, #38864 ) ;
#6271 = CARTESIAN_POINT ( 'NONE',  ( 96.15314808468748708, 91.99731107132950569, 85.77989583420048803 ) ) ;
#6272 = CARTESIAN_POINT ( 'NONE',  ( 10.00000000000000000, 0.000000000000000000, 0.000000000000000000 ) ) ;
#6273 = CARTESIAN_POINT ( 'NONE',  ( -96.32499999999996021, -212.2949673200287179, 75.58020833506763836 ) ) ;
#6274 = ORIENTED_EDGE ( 'NONE', *, *, #60939, .F. ) ;
#6275 = CARTESIAN_POINT ( 'NONE',  ( 97.64999999999999147, -209.9999884513868551, 83.41187540116096955 ) ) ;
#6276 = CARTESIAN_POINT ( 'NONE',  ( -97.30629616937501680, 88.66845928578038638, 80.17072916753380696 ) ) ;
#6277 = AXIS2_PLACEMENT_3D ( 'NONE', #3473, #9830, #32746 ) ;
#6278 = VECTOR ( 'NONE', #30979, 1000.000000000000114 ) ;
#6279 = CARTESIAN_POINT ( 'NONE',  ( 92.69370383062501162, -211.3315407142195852, 86.52072916753381548 ) ) ;
#6280 = ORIENTED_EDGE ( 'NONE', *, *, #71200, .T. ) ;
#6281 = CARTESIAN_POINT ( 'NONE',  ( 97.64999999999999147, -210.0000000983658026, 80.23687499810812085 ) ) ;
#6282 = CYLINDRICAL_SURFACE ( 'NONE', #9649, 31.99999999999998579 ) ;
#6283 = DIRECTION ( 'NONE',  ( 0.000000000000000000, -0.9510565162951506446, -0.3090169943749562775 ) ) ;
#6284 = EDGE_CURVE ( 'NONE', #6672, #60240, #378, .T. ) ;
#6285 = EDGE_CURVE ( 'NONE', #37614, #53249, #70415, .T. ) ;
#6286 = CARTESIAN_POINT ( 'NONE',  ( -0.0004442498525516064278, 0.001194404164626844313, -85.59999999999999432 ) ) ;
#6287 = DIRECTION ( 'NONE',  ( 0.3853207896976533209, -0.9227826878668545785, 0.000000000000000000 ) ) ;
#6288 = EDGE_CURVE ( 'NONE', #71207, #33546, #22529, .T. ) ;
#6289 = ORIENTED_EDGE ( 'NONE', *, *, #15644, .F. ) ;
#6290 = EDGE_LOOP ( 'NONE', ( #58941, #34022, #35259, #48466 ) ) ;
#6291 = EDGE_CURVE ( 'NONE', #20918, #33855, #63501, .T. ) ;
#6292 = CARTESIAN_POINT ( 'NONE',  ( 95.00000000000000000, -207.3369185715606307, 80.11781250086714579 ) ) ;
#6293 = CARTESIAN_POINT ( 'NONE',  ( 10.00000000000000000, -33.80338159004273280, -16.23288003029533044 ) ) ;
#6294 = FACE_OUTER_BOUND ( 'NONE', #28535, .T. ) ;
#6295 = DIRECTION ( 'NONE',  ( -1.000000000000000000, 0.000000000000000000, -0.000000000000000000 ) ) ;
#6296 = DIRECTION ( 'NONE',  ( 0.000000000000000000, 0.000000000000000000, 1.000000000000000000 ) ) ;
#6297 = ADVANCED_FACE ( 'NONE', ( #11593, #45473, #34534 ), #69492, .F. ) ;
#6298 = DIRECTION ( 'NONE',  ( -1.000000000000000000, 0.000000000000000000, 0.000000000000000000 ) ) ;
#6299 = CARTESIAN_POINT ( 'NONE',  ( 95.00000000000000000, -206.9400435732949575, 84.76125000000000398 ) ) ;
#6300 = ORIENTED_EDGE ( 'NONE', *, *, #51850, .F. ) ;
#6301 = ORIENTED_EDGE ( 'NONE', *, *, #63241, .T. ) ;
#6302 = ORIENTED_EDGE ( 'NONE', *, *, #47419, .T. ) ;
#6303 = ORIENTED_EDGE ( 'NONE', *, *, #57680, .T. ) ;
#6304 = CARTESIAN_POINT ( 'NONE',  ( 10.00000000000000000, 77.32052557432849937, -5.256550761632002633 ) ) ;
#6305 = VECTOR ( 'NONE', #12708, 999.9999999999998863 ) ;
#6306 =( NAMED_UNIT ( * ) SI_UNIT ( $, .STERADIAN. ) SOLID_ANGLE_UNIT ( ) );
#6307 = CARTESIAN_POINT ( 'NONE',  ( -95.00000000000002842, 92.66308142843932671, 85.83281250086714920 ) ) ;
#6308 = CARTESIAN_POINT ( 'NONE',  ( 10.00000000000000000, 30.80686688397010542, 21.53537804866092387 ) ) ;
#6309 = LINE ( 'NONE', #29571, #17346 ) ;
#6310 = CARTESIAN_POINT ( 'NONE',  ( 97.64999999999999147, -209.9999999999999716, 78.33187500173430351 ) ) ;
#6311 = CARTESIAN_POINT ( 'NONE',  ( 93.67499999999999716, 87.70503267997126784, 79.94583333333332575 ) ) ;
#6312 = EDGE_CURVE ( 'NONE', #4680, #39290, #17634, .T. ) ;
#6313 = ORIENTED_EDGE ( 'NONE', *, *, #61943, .F. ) ;
#6314 = DIRECTION ( 'NONE',  ( -1.000000000000000000, 0.000000000000000000, -0.000000000000000000 ) ) ;
#6315 = AXIS2_PLACEMENT_3D ( 'NONE', #33790, #5610, #40179 ) ;
#6316 = VERTEX_POINT ( 'NONE', #11238 ) ;
#6317 = EDGE_CURVE ( 'NONE', #73325, #19207, #52564, .T. ) ;
#6318 = DIRECTION ( 'NONE',  ( 0.000000000000000000, 0.000000000000000000, 1.000000000000000000 ) ) ;
#6319 = ORIENTED_EDGE ( 'NONE', *, *, #61190, .F. ) ;
#6320 = CARTESIAN_POINT ( 'NONE',  ( 92.35000000001612364, -210.0000060634596082, 88.17456390440206349 ) ) ;
#6321 = CARTESIAN_POINT ( 'NONE',  ( -92.69370383062505425, 91.33154071421968467, 80.01197916753382344 ) ) ;
#6322 = CARTESIAN_POINT ( 'NONE',  ( 97.30629616937498838, 88.66845928578037217, 75.93739583420047268 ) ) ;
#6323 = ORIENTED_EDGE ( 'NONE', *, *, #32001, .F. ) ;
#6324 = DIRECTION ( 'NONE',  ( 0.000000000000000000, 0.000000000000000000, 1.000000000000000000 ) ) ;
#6325 = CYLINDRICAL_SURFACE ( 'NONE', #35017, 37.49900000000000233 ) ;
#6326 = DIRECTION ( 'NONE',  ( 0.000000000000000000, 0.000000000000000000, 1.000000000000000000 ) ) ;
#6327 = DIRECTION ( 'NONE',  ( 1.000000000000000000, -0.000000000000000000, -0.000000000000000000 ) ) ;
#6328 = ORIENTED_EDGE ( 'NONE', *, *, #42689, .T. ) ;
#6329 = CARTESIAN_POINT ( 'NONE',  ( -35.50000000000000711, -120.0000000000000000, 2.500000000000000000 ) ) ;
#6330 = CIRCLE ( 'NONE', #59130, 42.00000000000000000 ) ;
#6331 = ADVANCED_FACE ( 'NONE', ( #51457 ), #57116, .T. ) ;
#6333 = EDGE_CURVE ( 'NONE', #24241, #7257, #69853, .T. ) ;
#6332 = CIRCLE ( 'NONE', #36306, 37.49900000000000233 ) ;
#6334 = CARTESIAN_POINT ( 'NONE',  ( -96.15314808468745866, -211.9973110713294489, 77.68364583420047609 ) ) ;
#6335 = VERTEX_POINT ( 'NONE', #18349 ) ;
#6336 = ORIENTED_EDGE ( 'NONE', *, *, #19594, .T. ) ;
#6337 = DIRECTION ( 'NONE',  ( 0.000000000000000000, -0.5224985647159559043, 0.8526401643540878483 ) ) ;
#6338 = ORIENTED_EDGE ( 'NONE', *, *, #34386, .T. ) ;
#6339 = LINE ( 'NONE', #16492, #25145 ) ;
#6340 = CARTESIAN_POINT ( 'NONE',  ( 96.32499999999998863, 87.70503267997126784, 80.68666666666665321 ) ) ;
#6341 = EDGE_LOOP ( 'NONE', ( #43867, #69874, #61233, #65500 ) ) ;
#6342 = CARTESIAN_POINT ( 'NONE',  ( -97.30629616937495996, -209.9999999999999716, 87.89656250086714806 ) ) ;
#6343 = ORIENTED_EDGE ( 'NONE', *, *, #73169, .F. ) ;
#6344 = CARTESIAN_POINT ( 'NONE',  ( 97.64999999999999147, 89.99999149135229004, 88.49187470744952577 ) ) ;
#6345 = CYLINDRICAL_SURFACE ( 'NONE', #60879, 10.00000000000000178 ) ;
#6346 = ORIENTED_EDGE ( 'NONE', *, *, #58664, .T. ) ;
#6347 = ORIENTED_EDGE ( 'NONE', *, *, #50689, .F. ) ;
#6348 = DIRECTION ( 'NONE',  ( 1.000000000000000000, -0.000000000000000000, -0.000000000000000000 ) ) ;
#6349 = DIRECTION ( 'NONE',  ( -1.000000000000000000, -0.000000000000000000, -0.000000000000000000 ) ) ;
#6350 = CARTESIAN_POINT ( 'NONE',  ( 93.84685191531248449, 88.00268892867053694, 84.66864583420047552 ) ) ;
#6351 = CARTESIAN_POINT ( 'NONE',  ( 11.99999999999999822, 46.54456581323805153, 59.03342792756280488 ) ) ;
#6352 = CARTESIAN_POINT ( 'NONE',  ( -96.32500000000001705, 87.70503267997129626, 75.50083333333331836 ) ) ;
#6353 = PLANE ( 'NONE',  #26468 ) ;
#6354 = CARTESIAN_POINT ( 'NONE',  ( 0.000000000000000000, -55.20638768913724448, -51.02545421589383068 ) ) ;
#6355 = DIRECTION ( 'NONE',  ( -1.000000000000000000, 0.000000000000000000, 0.000000000000000000 ) ) ;
#6356 = CARTESIAN_POINT ( 'NONE',  ( 11.99999999999999822, 23.16143007188530589, -73.95703589263951017 ) ) ;
#6357 = CARTESIAN_POINT ( 'NONE',  ( 0.000000000000000000, 2.946379043146343246, 75.11764819372150725 ) ) ;
#6358 = DIRECTION ( 'NONE',  ( 0.000000000000000000, 0.000000000000000000, 1.000000000000000000 ) ) ;
#6359 = DIRECTION ( 'NONE',  ( 0.9827303690289279636, 0.1850432970638681840, 0.000000000000000000 ) ) ;
#6360 = CARTESIAN_POINT ( 'NONE',  ( -23.50000000000000355, -120.0000000000000000, -64.00000000000000000 ) ) ;
#6361 = CARTESIAN_POINT ( 'NONE',  ( 15.00000000000000000, -26.23277895567251505, -4.042438405569750870 ) ) ;
#6362 = VECTOR ( 'NONE', #18224, 1000.000000000000000 ) ;
#6363 = EDGE_CURVE ( 'NONE', #27461, #26343, #27222, .T. ) ;
#6364 = ADVANCED_FACE ( 'NONE', ( #52196 ), #57482, .T. ) ;
#6365 = CARTESIAN_POINT ( 'NONE',  ( 10.00000000000000000, 0.8828120875900632436, 37.48860685352291000 ) ) ;
#6366 = EDGE_CURVE ( 'NONE', #31543, #26168, #56056, .T. ) ;
#6367 = EDGE_LOOP ( 'NONE', ( #21007, #30234, #46739, #8667 ) ) ;
#6368 = CIRCLE ( 'NONE', #41194, 31.99999999999999645 ) ;
#6369 = CARTESIAN_POINT ( 'NONE',  ( 10.00000000000000000, -17.67226234102849958, 33.17418723428301774 ) ) ;
#6370 = DIRECTION ( 'NONE',  ( 1.000000000000000000, -0.000000000000000000, -0.000000000000000000 ) ) ;
#6371 = DIRECTION ( 'NONE',  ( -0.000000000000000000, -0.000000000000000000, 1.000000000000000000 ) ) ;
#6372 = EDGE_CURVE ( 'NONE', #48989, #35036, #60832, .T. ) ;
#6373 = DIRECTION ( 'NONE',  ( 0.000000000000000000, 0.000000000000000000, 1.000000000000000000 ) ) ;
#6374 = FACE_OUTER_BOUND ( 'NONE', #17948, .T. ) ;
#6375 = VECTOR ( 'NONE', #54688, 1000.000000000000114 ) ;
#6376 = AXIS2_PLACEMENT_3D ( 'NONE', #58575, #41650, #64591 ) ;
#6377 = CARTESIAN_POINT ( 'NONE',  ( 95.00000000000000000, -207.3369185715606307, 84.56281250086716739 ) ) ;
#6378 = EDGE_CURVE ( 'NONE', #60507, #66693, #45293, .T. ) ;
#6379 = ORIENTED_EDGE ( 'NONE', *, *, #18906, .T. ) ;
#6380 = VERTEX_POINT ( 'NONE', #42040 ) ;
#6381 = CARTESIAN_POINT ( 'NONE',  ( -92.34999999999999432, -209.9999999999999716, 85.87249999999998806 ) ) ;
#6382 = ORIENTED_EDGE ( 'NONE', *, *, #54498, .F. ) ;
#6383 = CYLINDRICAL_SURFACE ( 'NONE', #43794, 37.49900000000000233 ) ;
#6384 = DIRECTION ( 'NONE',  ( -1.000000000000000000, 0.000000000000000000, 0.000000000000000000 ) ) ;
#6385 = EDGE_CURVE ( 'NONE', #20073, #45219, #36014, .T. ) ;
#6386 = ORIENTED_EDGE ( 'NONE', *, *, #11894, .T. ) ;
#6387 = CARTESIAN_POINT ( 'NONE',  ( 97.30629616937498838, -211.3315407142195852, 84.35114583420049428 ) ) ;
#6388 = VERTEX_POINT ( 'NONE', #65707 ) ;
#6389 = CARTESIAN_POINT ( 'NONE',  ( 94.99999999999998579, 93.05995642670504253, 80.39562500173430237 ) ) ;
#6390 = ORIENTED_EDGE ( 'NONE', *, *, #9994, .F. ) ;
#6391 = ORIENTED_EDGE ( 'NONE', *, *, #17836, .F. ) ;
#6392 = DIRECTION ( 'NONE',  ( -1.000000000000000000, 0.000000000000000000, 0.000000000000000000 ) ) ;
#6393 = DIRECTION ( 'NONE',  ( 0.000000000000000000, 0.000000000000000000, 1.000000000000000000 ) ) ;
#6394 = EDGE_LOOP ( 'NONE', ( #46540, #31405, #68145, #19160 ) ) ;
#6395 = CARTESIAN_POINT ( 'NONE',  ( -7.499999999999969802, 73.00000000000001421, -255.0000000000000000 ) ) ;
#6396 = CARTESIAN_POINT ( 'NONE',  ( 96.32499999999998863, -207.7050326799711968, 86.69270833506763552 ) ) ;
#6397 = EDGE_CURVE ( 'NONE', #1496, #27817, #3280, .T. ) ;
#6398 = ORIENTED_EDGE ( 'NONE', *, *, #47397, .F. ) ;
#6399 = FACE_OUTER_BOUND ( 'NONE', #37814, .T. ) ;
#6400 = EDGE_CURVE ( 'NONE', #46991, #57518, #64592, .T. ) ;
#6401 = AXIS2_PLACEMENT_3D ( 'NONE', #6623, #63406, #52471 ) ;
#6402 = VERTEX_POINT ( 'NONE', #47307 ) ;
#6403 = CARTESIAN_POINT ( 'NONE',  ( 11.99999999999999822, -26.02418014898359289, 70.52718814184250107 ) ) ;
#6404 = ORIENTED_EDGE ( 'NONE', *, *, #12033, .F. ) ;
#6405 = CARTESIAN_POINT ( 'NONE',  ( 97.64999999999997726, 88.47002178664753558, 87.16895833506762870 ) ) ;
#6406 = PRODUCT_DEFINITION_FORMATION_WITH_SPECIFIED_SOURCE ( 'ANY', '', #48755, .NOT_KNOWN. ) ;
#6407 = ORIENTED_EDGE ( 'NONE', *, *, #3333, .T. ) ;
#6408 = SURFACE_STYLE_FILL_AREA ( #12028 ) ;
#6409 = ORIENTED_EDGE ( 'NONE', *, *, #46294, .F. ) ;
#6410 = DIRECTION ( 'NONE',  ( -1.000000000000000000, 0.000000000000000000, 0.000000000000000000 ) ) ;
#6411 = CARTESIAN_POINT ( 'NONE',  ( 19.29194287201271862, -133.5026271600380880, 5.500000000000000000 ) ) ;
#6412 = ORIENTED_EDGE ( 'NONE', *, *, #5474, .T. ) ;
#6413 = AXIS2_PLACEMENT_3D ( 'NONE', #50079, #36971, #8404 ) ;
#6414 = EDGE_LOOP ( 'NONE', ( #46005, #25090, #49882, #14494 ) ) ;
#6415 = VERTEX_POINT ( 'NONE', #25108 ) ;
#6416 = DIRECTION ( 'NONE',  ( -0.000000000000000000, -0.9135454576426004225, -0.4067366430758009854 ) ) ;
#6417 = DIRECTION ( 'NONE',  ( -1.000000000000000000, 0.000000000000000000, 0.000000000000000000 ) ) ;
#6418 = CARTESIAN_POINT ( 'NONE',  ( -92.35000000000003695, 90.00000000000004263, 87.14249999999999829 ) ) ;
#6419 = ORIENTED_EDGE ( 'NONE', *, *, #40593, .F. ) ;
#6420 = CARTESIAN_POINT ( 'NONE',  ( 92.35000000000000853, -209.9999999999999716, 90.00000000000000000 ) ) ;
#6421 = AXIS2_PLACEMENT_3D ( 'NONE', #34852, #681, #7396 ) ;
#6422 =( BOUNDED_CURVE ( )  B_SPLINE_CURVE ( 2, ( #49550, #48810, #7852, #71728, #37549, #54826, #42079 ),
 .UNSPECIFIED., .F., .F. ) 
 B_SPLINE_CURVE_WITH_KNOTS ( ( 3, 2, 2, 3 ),
 ( 0.4656806970079900854, 0.4727362912414405649, 0.4797920567823575899, 0.4868478063952913493 ),
 .UNSPECIFIED. ) 
 CURVE ( )  GEOMETRIC_REPRESENTATION_ITEM ( )  RATIONAL_B_SPLINE_CURVE ( ( 0.9999934945991874047, 0.8660286565638194434, 1.000000000000000000, 0.8660254037844387076, 1.000000000000000000, 0.8660254037844387076, 1.000000000000000000 ) ) 
 REPRESENTATION_ITEM ( '' )  );
#6423 = EDGE_LOOP ( 'NONE', ( #62138, #21822, #50264, #72977 ) ) ;
#6424 = DIRECTION ( 'NONE',  ( -1.000000000000000000, -0.000000000000000000, -0.000000000000000000 ) ) ;
#6425 = CARTESIAN_POINT ( 'NONE',  ( -97.30629616937497417, -208.6684592857803011, 85.77989583420048803 ) ) ;
#6426 = ORIENTED_EDGE ( 'NONE', *, *, #32725, .F. ) ;
#6427 = VECTOR ( 'NONE', #7182, 1000.000000000000000 ) ;
#6428 = CARTESIAN_POINT ( 'NONE',  ( -92.34999999999999432, -209.9999998456625860, 79.60187500750915035 ) ) ;
#6429 = DIRECTION ( 'NONE',  ( 0.000000000000000000, 0.000000000000000000, 1.000000000000000000 ) ) ;
#6430 = DIRECTION ( 'NONE',  ( -1.000000000000000000, 0.000000000000000000, 0.000000000000000000 ) ) ;
#6431 = CARTESIAN_POINT ( 'NONE',  ( -94.99999999999997158, -212.6630814284392557, 76.46656250086712703 ) ) ;
#6432 = FACE_OUTER_BOUND ( 'NONE', #56599, .T. ) ;
#6433 = CARTESIAN_POINT ( 'NONE',  ( 10.00000000000000000, 0.000000000000000000, 0.000000000000000000 ) ) ;
#6434 = AXIS2_PLACEMENT_3D ( 'NONE', #41384, #12798, #70300 ) ;
#6435 = VECTOR ( 'NONE', #10581, 1000.000000000000000 ) ;
#6436 = CARTESIAN_POINT ( 'NONE',  ( 0.000000000000000000, 41.19522573413826194, -65.64334221924865176 ) ) ;
#6437 = CARTESIAN_POINT ( 'NONE',  ( 10.00000000000000000, -37.58145647212455032, 0.6853352020789044152 ) ) ;
#6438 = EDGE_CURVE ( 'NONE', #1386, #19207, #68080, .T. ) ;
#6439 = CARTESIAN_POINT ( 'NONE',  ( -96.15314808468751551, 88.00268892867056536, 77.04864583420047097 ) ) ;
#6440 = FACE_OUTER_BOUND ( 'NONE', #66156, .T. ) ;
#6441 = LINE ( 'NONE', #52287, #51855 ) ;
#6442 = ORIENTED_EDGE ( 'NONE', *, *, #47596, .T. ) ;
#6443 = DIRECTION ( 'NONE',  ( 0.000000000000000000, 0.000000000000000000, -1.000000000000000000 ) ) ;
#6444 = DIRECTION ( 'NONE',  ( 0.000000000000000000, -0.7071067811865536790, 0.7071067811865413555 ) ) ;
#6445 = CYLINDRICAL_SURFACE ( 'NONE', #37023, 82.00000000000000000 ) ;
#6446 = DIRECTION ( 'NONE',  ( 1.000000000000000000, 0.000000000000000000, 0.000000000000000000 ) ) ;
#6447 = DIRECTION ( 'NONE',  ( 0.000000000000000000, 0.000000000000000000, 1.000000000000000000 ) ) ;
#6448 = CARTESIAN_POINT ( 'NONE',  ( 11.99999999999999822, 63.18004540533092239, -44.88180994100307686 ) ) ;
#6449 = CARTESIAN_POINT ( 'NONE',  ( -96.15314808468747287, -208.0026889286704943, 77.63072916753381492 ) ) ;
#6450 = EDGE_CURVE ( 'NONE', #11255, #53009, #36376, .T. ) ;
#6451 = EDGE_CURVE ( 'NONE', #73300, #55761, #26046, .T. ) ;
#6452 = LINE ( 'NONE', #34265, #16448 ) ;
#6453 = VECTOR ( 'NONE', #18628, 1000.000000000000000 ) ;
#6454 = ORIENTED_EDGE ( 'NONE', *, *, #73834, .F. ) ;
#6455 = CARTESIAN_POINT ( 'NONE',  ( 0.000000000000000000, 24.81905959214274660, -9.408202855044498492 ) ) ;
#6456 = CYLINDRICAL_SURFACE ( 'NONE', #39475, 82.00000000000000000 ) ;
#6457 = CIRCLE ( 'NONE', #12446, 37.49900000000000944 ) ;
#6458 = ADVANCED_FACE ( 'NONE', ( #65341 ), #37511, .F. ) ;
#6459 = PRODUCT_DEFINITION_FORMATION_WITH_SPECIFIED_SOURCE ( 'ANY', '', #68031, .NOT_KNOWN. ) ;
#6460 = DIRECTION ( 'NONE',  ( -1.000000000000000000, 1.047380211910311281E-14, 2.618450529775778123E-14 ) ) ;
#6461 = EDGE_CURVE ( 'NONE', #20380, #39507, #68579, .T. ) ;
#6462 = CARTESIAN_POINT ( 'NONE',  ( 10.00000000000000000, 0.000000000000000000, 0.000000000000000000 ) ) ;
#6463 = VERTEX_POINT ( 'NONE', #59696 ) ;
#6464 = DIRECTION ( 'NONE',  ( 1.000000000000000000, 0.000000000000000000, 0.000000000000000000 ) ) ;
#6465 = DIRECTION ( 'NONE',  ( 1.000000000000000000, 0.000000000000000000, 0.000000000000000000 ) ) ;
#6466 = EDGE_LOOP ( 'NONE', ( #41428, #10904, #56874, #53023 ) ) ;
#6467 = CIRCLE ( 'NONE', #56925, 82.00000000000000000 ) ;
#6468 = CARTESIAN_POINT ( 'NONE',  ( 97.30629616937498838, -211.3315407142195852, 83.55739583420047722 ) ) ;
#6469 = CARTESIAN_POINT ( 'NONE',  ( -2.500000000000015543, -73.00000000000001421, -251.7000000000000455 ) ) ;
#6470 = CIRCLE ( 'NONE', #70098, 31.99999999999998579 ) ;
#6471 = EDGE_CURVE ( 'NONE', #18143, #56853, #25478, .T. ) ;
#6472 = ORIENTED_EDGE ( 'NONE', *, *, #37086, .T. ) ;
#6473 = CARTESIAN_POINT ( 'NONE',  ( 11.99999999999999822, -75.11725578898470701, 2.956366410620372864 ) ) ;
#6474 = ORIENTED_EDGE ( 'NONE', *, *, #58489, .F. ) ;
#6475 = AXIS2_PLACEMENT_3D ( 'NONE', #28429, #40094, #32948 ) ;
#6476 = LINE ( 'NONE', #29739, #14253 ) ;
#6477 = EDGE_LOOP ( 'NONE', ( #62339, #38164, #59540, #65023 ) ) ;
#6478 = AXIS2_PLACEMENT_3D ( 'NONE', #19915, #31204, #18445 ) ;
#6479 = CARTESIAN_POINT ( 'NONE',  ( -92.69370383062502583, 91.33154071421968467, 79.37697916753381833 ) ) ;
#6480 = ORIENTED_EDGE ( 'NONE', *, *, #51624, .F. ) ;
#6481 = ORIENTED_EDGE ( 'NONE', *, *, #1963, .T. ) ;
#6482 = ORIENTED_EDGE ( 'NONE', *, *, #73234, .F. ) ;
#6483 = CYLINDRICAL_SURFACE ( 'NONE', #11599, 2.649999999999985700 ) ;
#6484 = EDGE_CURVE ( 'NONE', #55201, #43013, #21999, .T. ) ;
#6485 = ADVANCED_FACE ( 'NONE', ( #48041 ), #70955, .T. ) ;
#6486 = ORIENTED_EDGE ( 'NONE', *, *, #22922, .F. ) ;
#6487 = CARTESIAN_POINT ( 'NONE',  ( 10.00000000000000000, -40.65526001592565564, -71.21200624218839437 ) ) ;
#6488 = VERTEX_POINT ( 'NONE', #2951 ) ;
#6489 = CARTESIAN_POINT ( 'NONE',  ( 92.55058773059860755, 89.32071446497070610, 74.93153462041256319 ) ) ;
#6490 = ADVANCED_FACE ( 'NONE', ( #71694 ), #19460, .T. ) ;
#6491 = ORIENTED_EDGE ( 'NONE', *, *, #35957, .F. ) ;
#6492 = AXIS2_PLACEMENT_3D ( 'NONE', #34502, #44310, #16861 ) ;
#6493 = VERTEX_POINT ( 'NONE', #13810 ) ;
#6494 = ORIENTED_EDGE ( 'NONE', *, *, #68058, .T. ) ;
#6495 = CARTESIAN_POINT ( 'NONE',  ( 95.00000000000000000, -207.3369185715606307, 82.49906250086714010 ) ) ;
#6496 = APPLICATION_PROTOCOL_DEFINITION ( 'draft international standard', 'automotive_design', 1998, #50808 ) ;
#6497 = CARTESIAN_POINT ( 'NONE',  ( -92.35000000000003695, 90.00000000000004263, 84.60249999999999204 ) ) ;
#6498 = CARTESIAN_POINT ( 'NONE',  ( 0.000000000000000000, 0.000000000000000000, 0.000000000000000000 ) ) ;
#6499 = CARTESIAN_POINT ( 'NONE',  ( -92.35000000000005116, -208.4700217866474361, 89.10041666666667481 ) ) ;
#6500 = LINE ( 'NONE', #18140, #3659 ) ;
#6501 = LINE ( 'NONE', #12124, #45536 ) ;
#6502 = CARTESIAN_POINT ( 'NONE',  ( -92.69370383062498320, -211.3315407142195852, 83.55739583420047722 ) ) ;
#6503 = CARTESIAN_POINT ( 'NONE',  ( -97.30629616937501680, 88.66845928578038638, 82.86947916753382515 ) ) ;
#6504 = ORIENTED_EDGE ( 'NONE', *, *, #34224, .T. ) ;
#6505 = VECTOR ( 'NONE', #10393, 1000.000000000000114 ) ;
#6506 = CARTESIAN_POINT ( 'NONE',  ( 93.84685191531248449, 88.00268892867053694, 84.03364583420047040 ) ) ;
#6507 = EDGE_LOOP ( 'NONE', ( #42951, #49920, #3347, #49503 ) ) ;
#6508 = DIRECTION ( 'NONE',  ( -1.000000000000000000, -0.000000000000000000, 0.000000000000000000 ) ) ;
#6509 = CARTESIAN_POINT ( 'NONE',  ( 92.35000000000000853, -209.9999999999999716, 76.10937500173430692 ) ) ;
#6510 = DIRECTION ( 'NONE',  ( 0.000000000000000000, 0.000000000000000000, 1.000000000000000000 ) ) ;
#6511 = CARTESIAN_POINT ( 'NONE',  ( 92.35000000000000853, -209.9999999999999716, 90.00000000000000000 ) ) ;
#6512 = CARTESIAN_POINT ( 'NONE',  ( -92.69370383062498320, -208.6684592857803295, 87.47322916753380184 ) ) ;
#6513 = LINE ( 'NONE', #18515, #17475 ) ;
#6514 = FACE_OUTER_BOUND ( 'NONE', #21357, .T. ) ;
#6515 = DIRECTION ( 'NONE',  ( 0.000000000000000000, 1.000000000000000000, 0.000000000000000000 ) ) ;
#6516 = DIRECTION ( 'NONE',  ( 0.000000000000000000, 0.3090169943749442316, 0.9510565162951545304 ) ) ;
#6517 = ORIENTED_EDGE ( 'NONE', *, *, #61564, .T. ) ;
#6518 = AXIS2_PLACEMENT_3D ( 'NONE', #9422, #9054, #54195 ) ;
#6519 = ORIENTED_EDGE ( 'NONE', *, *, #65201, .T. ) ;
#6520 = CARTESIAN_POINT ( 'NONE',  ( -97.65000000000001990, 88.47002178664754979, 76.71791666666666742 ) ) ;
#6521 = CARTESIAN_POINT ( 'NONE',  ( 11.99999999999999822, 76.41127070299290835, -12.93880638057234123 ) ) ;
#6522 = CARTESIAN_POINT ( 'NONE',  ( -96.15314808468751551, 88.00268892867056536, 87.20864583420046756 ) ) ;
#6523 = CARTESIAN_POINT ( 'NONE',  ( -93.41453557521617768, -208.2943803060621519, 74.79912739178799086 ) ) ;
#6524 = CARTESIAN_POINT ( 'NONE',  ( 94.99999999999998579, 93.05995642670504253, 76.50624999999999432 ) ) ;
#6525 = EDGE_CURVE ( 'NONE', #22209, #69025, #1485, .T. ) ;
#6526 = DIRECTION ( 'NONE',  ( 0.000000000000000000, 0.000000000000000000, 1.000000000000000000 ) ) ;
#6527 = AXIS2_PLACEMENT_3D ( 'NONE', #35594, #12663, #42362 ) ;
#6528 = DIRECTION ( 'NONE',  ( 0.000000000000000000, 0.000000000000000000, 1.000000000000000000 ) ) ;
#6529 = AXIS2_PLACEMENT_3D ( 'NONE', #71524, #37711, #65917 ) ;
#6530 = ORIENTED_EDGE ( 'NONE', *, *, #49987, .F. ) ;
#6531 = CARTESIAN_POINT ( 'NONE',  ( -96.15314808468752972, 91.99731107132950569, 76.83697916753381207 ) ) ;
#6532 = AXIS2_PLACEMENT_3D ( 'NONE', #15588, #4327, #61460 ) ;
#6533 = CARTESIAN_POINT ( 'NONE',  ( 0.000000000000000000, -120.0000000000000000, 2.500000000000000000 ) ) ;
#6534 = EDGE_CURVE ( 'NONE', #30413, #23323, #36428, .T. ) ;
#6535 = CARTESIAN_POINT ( 'NONE',  ( 10.00000000000000000, 0.000000000000000000, 0.000000000000000000 ) ) ;
#6536 = CARTESIAN_POINT ( 'NONE',  ( 3.000000000000000000, 0.000000000000000000, 0.000000000000000000 ) ) ;
#6537 = DIRECTION ( 'NONE',  ( 1.000000000000000000, -0.000000000000000000, -0.000000000000000000 ) ) ;
#6538 = CARTESIAN_POINT ( 'NONE',  ( -94.99999999999997158, -212.6630814284392557, 85.51531250086713953 ) ) ;
#6539 = EDGE_CURVE ( 'NONE', #19072, #60775, #60448, .T. ) ;
#6540 = DIRECTION ( 'NONE',  ( 0.000000000000000000, -0.5877852522924689183, -0.8090169943749504489 ) ) ;
#6541 = AXIS2_PLACEMENT_3D ( 'NONE', #13481, #30756, #53705 ) ;
#6542 = CARTESIAN_POINT ( 'NONE',  ( 97.30629616937498838, 90.00000000000002842, 75.51406250086715488 ) ) ;
#6543 = AXIS2_PLACEMENT_3D ( 'NONE', #57637, #18498, #35781 ) ;
#6544 = CARTESIAN_POINT ( 'NONE',  ( -93.84685191531248449, -208.0026889286704943, 75.61989583420049144 ) ) ;
#6545 = CARTESIAN_POINT ( 'NONE',  ( 15.00000000000000000, -18.13022148937242761, 15.02647892043569122 ) ) ;
#6546 = EDGE_LOOP ( 'NONE', ( #5677, #17010, #64304, #65458 ) ) ;
#6547 = EDGE_CURVE ( 'NONE', #3697, #37374, #44255, .T. ) ;
#6548 = CYLINDRICAL_SURFACE ( 'NONE', #30485, 82.00000000000000000 ) ;
#6549 = DIRECTION ( 'NONE',  ( -1.000000000000000000, 0.000000000000000000, -0.000000000000000000 ) ) ;
#6550 = CARTESIAN_POINT ( 'NONE',  ( 0.000000000000000000, 0.000000000000000000, -175.0000000000000000 ) ) ;
#6551 = FACE_OUTER_BOUND ( 'NONE', #26793, .T. ) ;
#6552 = CARTESIAN_POINT ( 'NONE',  ( 96.15314808468748708, -208.0026889286704943, 77.36614583420046642 ) ) ;
#6553 = VERTEX_POINT ( 'NONE', #72796 ) ;
#6554 = VECTOR ( 'NONE', #47935, 1000.000000000000114 ) ;
#6555 = CARTESIAN_POINT ( 'NONE',  ( 0.000000000000000000, 0.000000000000000000, 0.000000000000000000 ) ) ;
#6556 = EDGE_CURVE ( 'NONE', #38932, #25891, #54789, .T. ) ;
#6557 = EDGE_LOOP ( 'NONE', ( #8731, #55011, #39479, #37474 ) ) ;
#6558 = CYLINDRICAL_SURFACE ( 'NONE', #73570, 82.00000000000000000 ) ;
#6559 = ADVANCED_FACE ( 'NONE', ( #32210 ), #20940, .T. ) ;
#6560 = ORIENTED_EDGE ( 'NONE', *, *, #60756, .T. ) ;
#6561 = DIRECTION ( 'NONE',  ( 0.000000000000000000, -0.1564344650402381132, 0.9876883405951365491 ) ) ;
#6562 = EDGE_CURVE ( 'NONE', #6768, #30711, #66814, .T. ) ;
#6563 = AXIS2_PLACEMENT_3D ( 'NONE', #18035, #52989, #30771 ) ;
#6564 = ORIENTED_EDGE ( 'NONE', *, *, #63134, .T. ) ;
#6565 = ORIENTED_EDGE ( 'NONE', *, *, #52349, .T. ) ;
#6566 = EDGE_LOOP ( 'NONE', ( #35494, #23077, #26561, #32988 ) ) ;
#6567 = CARTESIAN_POINT ( 'NONE',  ( 93.67500000000001137, -207.7050326799711968, 79.81354166840095843 ) ) ;
#6568 = ADVANCED_FACE ( 'NONE', ( #38237 ), #27700, .T. ) ;
#6569 = VERTEX_POINT ( 'NONE', #16046 ) ;
#6570 = ORIENTED_EDGE ( 'NONE', *, *, #61234, .T. ) ;
#6571 = CARTESIAN_POINT ( 'NONE',  ( 96.15314808468748708, 88.00268892867053694, 83.66322916753382799 ) ) ;
#6572 = AXIS2_PLACEMENT_3D ( 'NONE', #27684, #16784, #5147 ) ;
#6573 = PLANE ( 'NONE',  #51562 ) ;
#6575 = DIRECTION ( 'NONE',  ( 0.000000000000000000, -0.1564344650402170744, -0.9876883405951398798 ) ) ;
#6574 = CIRCLE ( 'NONE', #48595, 31.99999999999999289 ) ;
#6576 = ORIENTED_EDGE ( 'NONE', *, *, #40768, .F. ) ;
#6577 = ORIENTED_EDGE ( 'NONE', *, *, #5734, .T. ) ;
#6578 = ORIENTED_EDGE ( 'NONE', *, *, #53204, .T. ) ;
#6579 = VERTEX_POINT ( 'NONE', #26946 ) ;
#6580 = DIRECTION ( 'NONE',  ( -1.000000000000000000, 0.000000000000000000, -0.000000000000000000 ) ) ;
#6581 = EDGE_LOOP ( 'NONE', ( #25698, #66222, #32349, #39592 ) ) ;
#6582 = AXIS2_PLACEMENT_3D ( 'NONE', #21883, #33524, #56486 ) ;
#6583 = CARTESIAN_POINT ( 'NONE',  ( 93.67499999999998295, 92.29496732002878900, 84.17916666666666003 ) ) ;
#6584 = FACE_OUTER_BOUND ( 'NONE', #45451, .T. ) ;
#6585 = CARTESIAN_POINT ( 'NONE',  ( 10.00000000000000000, 0.000000000000000000, 0.000000000000000000 ) ) ;
#6586 = CARTESIAN_POINT ( 'NONE',  ( 92.35000000000000853, -211.5299782133524218, 86.95729166840096980 ) ) ;
#6587 = CYLINDRICAL_SURFACE ( 'NONE', #41962, 14.09999999999999964 ) ;
#6588 = CARTESIAN_POINT ( 'NONE',  ( 10.00000000000000000, -27.05870788708250885, 26.08949754953014022 ) ) ;
#6589 = ORIENTED_EDGE ( 'NONE', *, *, #60595, .T. ) ;
#6590 = CARTESIAN_POINT ( 'NONE',  ( -93.67499999999998295, -207.7050326799711968, 78.43770833506764006 ) ) ;
#6591 = VERTEX_POINT ( 'NONE', #8927 ) ;
#6592 = APPLICATION_CONTEXT ( 'automotive_design' ) ;
#6593 = AXIS2_PLACEMENT_3D ( 'NONE', #21543, #67419, #26815 ) ;
#6594 = VERTEX_POINT ( 'NONE', #50624 ) ;
#6596 = CARTESIAN_POINT ( 'NONE',  ( -93.67500000000003979, 92.29496732002878900, 78.43770833506764006 ) ) ;
#6595 = CARTESIAN_POINT ( 'NONE',  ( 93.67499999999998295, 92.29496732002878900, 77.90854166840097150 ) ) ;
#6597 = ORIENTED_EDGE ( 'NONE', *, *, #27035, .T. ) ;
#6598 = CARTESIAN_POINT ( 'NONE',  ( 94.99999999999998579, 87.33691857156068750, 78.53031250086715431 ) ) ;
#6599 = PLANE ( 'NONE',  #40966 ) ;
#6600 = PLANE ( 'NONE',  #55460 ) ;
#6601 = DIRECTION ( 'NONE',  ( 1.000000000000000000, 0.000000000000000000, 0.000000000000000000 ) ) ;
#6602 = ORIENTED_EDGE ( 'NONE', *, *, #68133, .F. ) ;
#6603 = CARTESIAN_POINT ( 'NONE',  ( 12.00000000000000000, -26.23277895567245466, 4.042438405570107030 ) ) ;
#6604 = DIRECTION ( 'NONE',  ( 1.000000000000000000, -7.331661483372147883E-15, -2.618450529775767079E-14 ) ) ;
#6605 = ORIENTED_EDGE ( 'NONE', *, *, #31892, .F. ) ;
#6606 = ORIENTED_EDGE ( 'NONE', *, *, #31120, .F. ) ;
#6607 = LINE ( 'NONE', #8734, #12052 ) ;
#6608 = CARTESIAN_POINT ( 'NONE',  ( -3.447886558751868336, -3.782864459065579776, -0.7348938709837913308 ) ) ;
#6609 = LINE ( 'NONE', #1009, #36124 ) ;
#6610 = CARTESIAN_POINT ( 'NONE',  ( -92.69370383062498320, -209.9999999999999716, 79.32406250086715715 ) ) ;
#6611 = ORIENTED_EDGE ( 'NONE', *, *, #67291, .T. ) ;
#6612 = EDGE_CURVE ( 'NONE', #29293, #4157, #26581, .T. ) ;
#6613 = CARTESIAN_POINT ( 'NONE',  ( 0.000000000000000000, 0.000000000000000000, 0.000000000000000000 ) ) ;
#6614 = CARTESIAN_POINT ( 'NONE',  ( -97.01659045496313638, -211.6055158133294469, 74.95309847082374688 ) ) ;
#6615 = ADVANCED_FACE ( 'NONE', ( #55158 ), #4416, .F. ) ;
#6616 = CARTESIAN_POINT ( 'NONE',  ( 10.00000000000000000, 16.23288003029543347, -33.80338159004267595 ) ) ;
#6617 = DIRECTION ( 'NONE',  ( -1.000000000000000000, 0.000000000000000000, 0.000000000000000000 ) ) ;
#6618 = CARTESIAN_POINT ( 'NONE',  ( -7.469491406282116053, 4.756046723998915482, -45.00000000000000000 ) ) ;
#6619 = CARTESIAN_POINT ( 'NONE',  ( 11.99999999999999822, 0.000000000000000000, 0.000000000000000000 ) ) ;
#6620 = FACE_OUTER_BOUND ( 'NONE', #46634, .T. ) ;
#6621 = CYLINDRICAL_SURFACE ( 'NONE', #18433, 2.649999999999999467 ) ;
#6622 = ADVANCED_FACE ( 'NONE', ( #49515 ), #61181, .T. ) ;
#6623 = CARTESIAN_POINT ( 'NONE',  ( -3.000000000000000000, 14.60985201121729737, -18.46759930825687945 ) ) ;
#6624 = DIRECTION ( 'NONE',  ( -0.000000000000000000, 0.1045284632676548031, 0.9945218953682732899 ) ) ;
#6625 = EDGE_CURVE ( 'NONE', #40077, #71422, #27312, .T. ) ;
#6626 = AXIS2_PLACEMENT_3D ( 'NONE', #32723, #55677, #50014 ) ;
#6627 = CARTESIAN_POINT ( 'NONE',  ( 97.30629616937498838, 91.33154071421968467, 88.26697916753381890 ) ) ;
#6628 = CARTESIAN_POINT ( 'NONE',  ( -96.15314808468747287, -208.0026889286704943, 85.88572916753381037 ) ) ;
#6629 = ORIENTED_EDGE ( 'NONE', *, *, #59881, .F. ) ;
#6630 = CARTESIAN_POINT ( 'NONE',  ( 0.000000000000000000, 0.000000000000000000, -43.79999999999998295 ) ) ;
#6631 = CARTESIAN_POINT ( 'NONE',  ( -92.69370383062505425, 91.33154071421968467, 77.31322916753380525 ) ) ;
#6632 = AXIS2_PLACEMENT_3D ( 'NONE', #40474, #63424, #16434 ) ;
#6633 = AXIS2_PLACEMENT_3D ( 'NONE', #30357, #53302, #68759 ) ;
#6634 = CARTESIAN_POINT ( 'NONE',  ( 96.15314808468750130, -211.9973110713294489, 88.58447916753381435 ) ) ;
#6635 = VERTEX_POINT ( 'NONE', #43536 ) ;
#6636 =( BOUNDED_CURVE ( )  B_SPLINE_CURVE ( 2, ( #17610, #11962, #13349, #36279, #71963, #20091, #48675, #26103, #14078 ),
 .UNSPECIFIED., .F., .F. ) 
 B_SPLINE_CURVE_WITH_KNOTS ( ( 3, 2, 2, 2, 3 ),
 ( 0.2116728463006670724, 0.2116729662264710543, 0.2187287317673534404, 0.2257844973082357709, 0.2328402629019979686 ),
 .UNSPECIFIED. ) 
 CURVE ( )  GEOMETRIC_REPRESENTATION_ITEM ( )  RATIONAL_B_SPLINE_CURVE ( ( 0.9999954457845905420, 0.9999977228535908980, 1.000000000000000000, 0.8660254037844387076, 1.000000000000000000, 0.8660254037844387076, 1.000000000000000000, 0.8660254037844387076, 1.000000000000000000 ) ) 
 REPRESENTATION_ITEM ( '' )  );
#6637 = FACE_OUTER_BOUND ( 'NONE', #63194, .T. ) ;
#6638 = AXIS2_PLACEMENT_3D ( 'NONE', #32924, #55874, #4387 ) ;
#6639 = ORIENTED_EDGE ( 'NONE', *, *, #43425, .T. ) ;
#6640 = CARTESIAN_POINT ( 'NONE',  ( 10.00000000000000000, 46.54456581323888997, -59.03342792756214408 ) ) ;
#6641 = ADVANCED_FACE ( 'NONE', ( #72072, #33318, #39359 ), #21297, .T. ) ;
#6642 = EDGE_CURVE ( 'NONE', #37989, #63739, #38617, .T. ) ;
#6643 = CARTESIAN_POINT ( 'NONE',  ( 0.000000000000000000, 4.992566952384984269, 37.16516213103279398 ) ) ;
#6644 = CIRCLE ( 'NONE', #676, 31.99999999999999289 ) ;
#6645 = ORIENTED_EDGE ( 'NONE', *, *, #24062, .T. ) ;
#6646 = ORIENTED_EDGE ( 'NONE', *, *, #2025, .T. ) ;
#6647 = CARTESIAN_POINT ( 'NONE',  ( 95.00000000000000000, -207.3369185715606307, 82.02281250086714692 ) ) ;
#6648 = DIRECTION ( 'NONE',  ( 0.000000000000000000, -0.9510565162951565288, 0.3090169943749382919 ) ) ;
#6649 = EDGE_CURVE ( 'NONE', #24509, #58812, #13627, .T. ) ;
#6650 = CARTESIAN_POINT ( 'NONE',  ( -2.499999999999997780, 8.494897427831771708, -19.01812422950394676 ) ) ;
#6651 = AXIS2_PLACEMENT_3D ( 'NONE', #60094, #49156, #55545 ) ;
#6652 = CARTESIAN_POINT ( 'NONE',  ( 0.000000000000000000, -0.8828120875903202602, 37.48860685352291000 ) ) ;
#6653 = DIRECTION ( 'NONE',  ( 0.000000000000000000, 0.000000000000000000, 1.000000000000000000 ) ) ;
#6654 = DIRECTION ( 'NONE',  ( -0.000000000000000000, -0.000000000000000000, 1.000000000000000000 ) ) ;
#6655 = CARTESIAN_POINT ( 'NONE',  ( 92.35000000000000853, -209.9999999999999716, 83.65000000000000568 ) ) ;
#6656 = EDGE_LOOP ( 'NONE', ( #66016, #59299, #19386, #34193 ) ) ;
#6657 = EDGE_LOOP ( 'NONE', ( #60966, #45718, #50373, #12816 ) ) ;
#6658 = ORIENTED_EDGE ( 'NONE', *, *, #74103, .T. ) ;
#6659 = ORIENTED_EDGE ( 'NONE', *, *, #49055, .T. ) ;
#6660 = DIRECTION ( 'NONE',  ( -0.000000000000000000, -0.000000000000000000, -1.000000000000000000 ) ) ;
#6661 = AXIS2_PLACEMENT_3D ( 'NONE', #60681, #53928, #64842 ) ;
#6662 = SURFACE_STYLE_USAGE ( .BOTH. , #692 ) ;
#6663 = CARTESIAN_POINT ( 'NONE',  ( -93.84685191531252713, 88.00268892867056536, 87.47322916753381605 ) ) ;
#6664 = CYLINDRICAL_SURFACE ( 'NONE', #49752, 77.49899999999999523 ) ;
#6665 = CYLINDRICAL_SURFACE ( 'NONE', #12611, 2.649999999999985700 ) ;
#6666 = CARTESIAN_POINT ( 'NONE',  ( 93.67500000000001137, -207.7050326799711968, 77.90854166840097150 ) ) ;
#6667 = CARTESIAN_POINT ( 'NONE',  ( 94.99999999999998579, 86.94004357329500010, 77.45874999999999488 ) ) ;
#6668 = VERTEX_POINT ( 'NONE', #44637 ) ;
#6669 = CARTESIAN_POINT ( 'NONE',  ( -96.32499999999996021, -212.2949673200287179, 88.91520833506763211 ) ) ;
#6670 = ORIENTED_EDGE ( 'NONE', *, *, #21705, .F. ) ;
#6671 = DIRECTION ( 'NONE',  ( 0.000000000000000000, 0.3826834323650841752, 0.9238795325112891810 ) ) ;
#6672 = VERTEX_POINT ( 'NONE', #38988 ) ;
#6673 = DIRECTION ( 'NONE',  ( -0.000000000000000000, -0.000000000000000000, 1.000000000000000000 ) ) ;
#6674 = CARTESIAN_POINT ( 'NONE',  ( -96.15314808468751551, 88.00268892867056536, 82.28739583420048120 ) ) ;
#6675 = CARTESIAN_POINT ( 'NONE',  ( 97.30629616937498838, 91.33154071421968467, 74.77322916753379900 ) ) ;
#6676 = VECTOR ( 'NONE', #3201, 1000.000000000000000 ) ;
#6677 = ORIENTED_EDGE ( 'NONE', *, *, #34922, .T. ) ;
#6678 = FACE_OUTER_BOUND ( 'NONE', #19337, .T. ) ;
#6679 = LINE ( 'NONE', #17957, #1413 ) ;
#6680 = LINE ( 'NONE', #12678, #4188 ) ;
#6681 = CARTESIAN_POINT ( 'NONE',  ( -97.64999999999996305, -208.4700217866474645, 86.21645833506764234 ) ) ;
#6682 = VERTEX_POINT ( 'NONE', #61925 ) ;
#6683 = DIRECTION ( 'NONE',  ( 0.000000000000000000, -0.8090169943749504489, -0.5877852522924689183 ) ) ;
#6684 = CIRCLE ( 'NONE', #35493, 82.00000000000000000 ) ;
#6685 = CARTESIAN_POINT ( 'NONE',  ( -11.59999999999999964, -0.8299999999999986278, -1.199999999999999956 ) ) ;
#6686 = VERTEX_POINT ( 'NONE', #10407 ) ;
#6687 = VERTEX_POINT ( 'NONE', #4800 ) ;
#6689 = FACE_BOUND ( 'NONE', #1320, .T. ) ;
#6688 = VECTOR ( 'NONE', #64497, 999.9999999999998863 ) ;
#6690 = ORIENTED_EDGE ( 'NONE', *, *, #25117, .F. ) ;
#6691 = DIRECTION ( 'NONE',  ( 0.000000000000000000, 0.000000000000000000, 1.000000000000000000 ) ) ;
#6692 = VECTOR ( 'NONE', #61445, 1000.000000000000114 ) ;
#6693 = CIRCLE ( 'NONE', #11515, 31.99999999999998934 ) ;
#6694 = CARTESIAN_POINT ( 'NONE',  ( 0.000000000000000000, -120.0000000000000000, 2.500000000000000000 ) ) ;
#6695 = VERTEX_POINT ( 'NONE', #45004 ) ;
#6696 = CARTESIAN_POINT ( 'NONE',  ( -92.69370383062498320, -209.9999999999999716, 87.57906250086715261 ) ) ;
#6697 = ORIENTED_EDGE ( 'NONE', *, *, #33338, .T. ) ;
#6698 = DIRECTION ( 'NONE',  ( -1.000000000000000000, 0.000000000000000000, 0.000000000000000000 ) ) ;
#6699 = DIRECTION ( 'NONE',  ( -1.000000000000000000, 0.000000000000000000, 0.000000000000000000 ) ) ;
#6700 = VERTEX_POINT ( 'NONE', #67930 ) ;
#6701 = ORIENTED_EDGE ( 'NONE', *, *, #39986, .T. ) ;
#6702 = CARTESIAN_POINT ( 'NONE',  ( -96.32500000000001705, 92.29496732002878900, 83.62354166840097491 ) ) ;
#6703 = EDGE_CURVE ( 'NONE', #73508, #42429, #46110, .T. ) ;
#6704 = AXIS2_PLACEMENT_3D ( 'NONE', #35844, #7296, #30211 ) ;
#6705 = CARTESIAN_POINT ( 'NONE',  ( 10.00000000000000000, -35.53030884539094103, 12.26510123303246935 ) ) ;
#6706 = CARTESIAN_POINT ( 'NONE',  ( 97.30629616937498838, 90.00000000000002842, 82.34031250086714238 ) ) ;
#6707 = CYLINDRICAL_SURFACE ( 'NONE', #72415, 82.00000000000000000 ) ;
#6708 = CARTESIAN_POINT ( 'NONE',  ( -93.67500000000003979, 92.29496732002878900, 80.34270833506762699 ) ) ;
#6709 = CARTESIAN_POINT ( 'NONE',  ( -99.99999999999997158, -214.9999999999999716, 90.00000000000000000 ) ) ;
#6710 = CARTESIAN_POINT ( 'NONE',  ( 15.00000000000000000, -3.948201729842032215, 23.21447184625297666 ) ) ;
#6712 = ADVANCED_FACE ( 'NONE', ( #40848 ), #23915, .F. ) ;
#6711 = LINE ( 'NONE', #68767, #68032 ) ;
#6713 = DIRECTION ( 'NONE',  ( -0.000000000000000000, -0.4067366430757898277, -0.9135454576426055295 ) ) ;
#6714 = DIRECTION ( 'NONE',  ( -1.000000000000000000, -0.000000000000000000, -0.000000000000000000 ) ) ;
#6715 = EDGE_CURVE ( 'NONE', #69906, #41007, #22437, .T. ) ;
#6716 = DIRECTION ( 'NONE',  ( -1.000000000000000000, -0.000000000000000000, 0.000000000000000000 ) ) ;
#6717 = CARTESIAN_POINT ( 'NONE',  ( -10.00000000000000000, 0.000000000000000000, 0.000000000000000000 ) ) ;
#6718 = CARTESIAN_POINT ( 'NONE',  ( -92.69370383062505425, 88.66845928578038638, 89.27239583420048064 ) ) ;
#6719 = DIRECTION ( 'NONE',  ( -0.000000000000000000, -0.3090169943749573878, 0.9510565162951503115 ) ) ;
#6720 = EDGE_CURVE ( 'NONE', #24697, #9702, #28001, .T. ) ;
#6721 = CARTESIAN_POINT ( 'NONE',  ( 2.750000000000000000, 0.000000000000000000, 2.699999999999999734 ) ) ;
#6722 = EDGE_CURVE ( 'NONE', #48440, #44941, #29532, .T. ) ;
#6723 = VERTEX_POINT ( 'NONE', #28433 ) ;
#6724 = CYLINDRICAL_SURFACE ( 'NONE', #53421, 77.49899999999999523 ) ;
#6725 = CARTESIAN_POINT ( 'NONE',  ( 92.35000000000003695, 91.52997821335253548, 85.50208333333331723 ) ) ;
#6726 = CIRCLE ( 'NONE', #24749, 77.49900000000000944 ) ;
#6727 = CARTESIAN_POINT ( 'NONE',  ( -10.00000000000000000, 0.000000000000000000, 0.000000000000000000 ) ) ;
#6728 = FACE_OUTER_BOUND ( 'NONE', #64089, .T. ) ;
#6729 = CARTESIAN_POINT ( 'NONE',  ( 10.00000000000000000, 0.6853352020790449695, 37.58145647212454321 ) ) ;
#6730 = CIRCLE ( 'NONE', #18576, 26.50000000000000355 ) ;
#6731 = EDGE_CURVE ( 'NONE', #14085, #4461, #58020, .T. ) ;
#6732 = EDGE_CURVE ( 'NONE', #63525, #40273, #649, .T. ) ;
#6733 = CARTESIAN_POINT ( 'NONE',  ( 97.30629616937498838, -211.3315407142195852, 81.17614583420048291 ) ) ;
#6734 = ORIENTED_EDGE ( 'NONE', *, *, #46028, .T. ) ;
#6735 = VECTOR ( 'NONE', #70862, 1000.000000000000000 ) ;
#6736 = EDGE_LOOP ( 'NONE', ( #25794, #68132, #53568, #74156 ) ) ;
#6737 = DIRECTION ( 'NONE',  ( -1.000000000000000000, -0.000000000000000000, -0.000000000000000000 ) ) ;
#6738 = ORIENTED_EDGE ( 'NONE', *, *, #17747, .F. ) ;
#6739 = AXIS2_PLACEMENT_3D ( 'NONE', #10957, #3849, #28233 ) ;
#6740 = DIRECTION ( 'NONE',  ( -1.427937372958396981E-15, 1.000000000000000000, -1.053567635648657358E-14 ) ) ;
#6741 = AXIS2_PLACEMENT_3D ( 'NONE', #9368, #48121, #71037 ) ;
#6742 = CARTESIAN_POINT ( 'NONE',  ( 95.00000000000000000, -207.3369185715606307, 75.51406250086714067 ) ) ;
#6743 = EDGE_LOOP ( 'NONE', ( #46150, #36857 ) ) ;
#6744 = CARTESIAN_POINT ( 'NONE',  ( 92.69370383062501162, -211.3315407142195852, 78.42447916753380355 ) ) ;
#6745 = ORIENTED_EDGE ( 'NONE', *, *, #62075, .F. ) ;
#6746 = DIRECTION ( 'NONE',  ( 0.000000000000000000, 0.000000000000000000, 1.000000000000000000 ) ) ;
#6747 = ORIENTED_EDGE ( 'NONE', *, *, #29457, .T. ) ;
#6748 = ORIENTED_EDGE ( 'NONE', *, *, #72073, .T. ) ;
#6749 = FACE_OUTER_BOUND ( 'NONE', #3462, .T. ) ;
#6750 = DIRECTION ( 'NONE',  ( -0.000000000000000000, -0.000000000000000000, -1.000000000000000000 ) ) ;
#6751 = ORIENTED_EDGE ( 'NONE', *, *, #69035, .F. ) ;
#6752 = LINE ( 'NONE', #40601, #19747 ) ;
#6753 = CARTESIAN_POINT ( 'NONE',  ( 97.64999999999997726, -211.5299782133524502, 85.89895833506764689 ) ) ;
#6754 = CARTESIAN_POINT ( 'NONE',  ( 94.99999999999998579, 86.94004357329500010, 88.25374999999999659 ) ) ;
#6755 = VERTEX_POINT ( 'NONE', #34829 ) ;
#6756 = DIRECTION ( 'NONE',  ( -1.000000000000000000, 0.000000000000000000, 0.000000000000000000 ) ) ;
#6757 = ORIENTED_EDGE ( 'NONE', *, *, #43843, .F. ) ;
#6758 = ORIENTED_EDGE ( 'NONE', *, *, #54065, .F. ) ;
#6759 = CYLINDRICAL_SURFACE ( 'NONE', #19297, 77.49899999999999523 ) ;
#6760 = ORIENTED_EDGE ( 'NONE', *, *, #52004, .F. ) ;
#6761 = CARTESIAN_POINT ( 'NONE',  ( 97.64999999999997726, 88.47002178664753558, 85.26395833506762756 ) ) ;
#6762 = ORIENTED_EDGE ( 'NONE', *, *, #44931, .F. ) ;
#6763 = ORIENTED_EDGE ( 'NONE', *, *, #46124, .T. ) ;
#6764 = LINE ( 'NONE', #46253, #50066 ) ;
#6765 = CARTESIAN_POINT ( 'NONE',  ( 10.00000000000000000, -10.74501242461258244, -35.92658777277521409 ) ) ;
#6766 = VERTEX_POINT ( 'NONE', #1022 ) ;
#6767 = ORIENTED_EDGE ( 'NONE', *, *, #11183, .F. ) ;
#6768 = VERTEX_POINT ( 'NONE', #22819 ) ;
#6769 = LINE ( 'NONE', #65040, #38457 ) ;
#6770 = DIRECTION ( 'NONE',  ( -1.000000000000000000, 0.000000000000000000, -0.000000000000000000 ) ) ;
#6771 = EDGE_CURVE ( 'NONE', #12946, #3354, #71195, .T. ) ;
#6772 = CARTESIAN_POINT ( 'NONE',  ( -92.35000000000005116, 88.47002178664754979, 88.99458333333333826 ) ) ;
#6773 = VERTEX_POINT ( 'NONE', #18266 ) ;
#6774 = EDGE_CURVE ( 'NONE', #35754, #26913, #35200, .T. ) ;
#6775 = CARTESIAN_POINT ( 'NONE',  ( -3.000000000000000000, 22.07842321921481243, 8.187992925817422218 ) ) ;
#6776 = ORIENTED_EDGE ( 'NONE', *, *, #2584, .F. ) ;
#6777 = CARTESIAN_POINT ( 'NONE',  ( -92.69370383062498320, -211.3315407142195852, 81.65239583420049030 ) ) ;
#6778 = ORIENTED_EDGE ( 'NONE', *, *, #59612, .T. ) ;
#6779 = DIRECTION ( 'NONE',  ( -1.000000000000000000, 0.000000000000000000, -0.000000000000000000 ) ) ;
#6780 = AXIS2_PLACEMENT_3D ( 'NONE', #73711, #9824, #22223 ) ;
#6781 = CARTESIAN_POINT ( 'NONE',  ( 10.00000000000000000, -72.35160999960831418, 20.41045688087797672 ) ) ;
#6782 = CARTESIAN_POINT ( 'NONE',  ( 92.34999999999999432, 91.52997821335252127, 89.39145833506763950 ) ) ;
#6783 = CARTESIAN_POINT ( 'NONE',  ( -94.99999999999997158, -207.3369185715606307, 77.41906250086714181 ) ) ;
#6784 = PRODUCT_DEFINITION ( 'UNKNOWN', '', #32838, #71699 ) ;
#6785 = EDGE_CURVE ( 'NONE', #28639, #34509, #17165, .T. ) ;
#6786 = CARTESIAN_POINT ( 'NONE',  ( 0.000000000000000000, 17.80606268964585226, -33.00180498840028775 ) ) ;
#6787 = CIRCLE ( 'NONE', #11549, 14.09999999999999964 ) ;
#6788 = ADVANCED_FACE ( 'NONE', ( #23542 ), #62297, .T. ) ;
#6789 = CARTESIAN_POINT ( 'NONE',  ( 11.99999999999999822, 72.35432306680485226, -20.40083707022909110 ) ) ;
#6790 = CARTESIAN_POINT ( 'NONE',  ( 10.00000000000000000, 22.48208911017500355, 35.47612816024531668 ) ) ;
#6791 = AXIS2_PLACEMENT_3D ( 'NONE', #62253, #40053, #253 ) ;
#6792 = LINE ( 'NONE', #8266, #45936 ) ;
#6793 = CARTESIAN_POINT ( 'NONE',  ( 0.000000000000000000, 0.000000000000000000, 0.000000000000000000 ) ) ;
#6794 = CARTESIAN_POINT ( 'NONE',  ( -92.69370383062502583, 91.33154071421968467, 77.31322916753380525 ) ) ;
#6795 = FACE_OUTER_BOUND ( 'NONE', #46601, .T. ) ;
#6796 = FACE_OUTER_BOUND ( 'NONE', #5373, .T. ) ;
#6797 = VECTOR ( 'NONE', #69934, 1000.000000000000000 ) ;
#6798 = EDGE_CURVE ( 'NONE', #52133, #14126, #31591, .T. ) ;
#6799 = ORIENTED_EDGE ( 'NONE', *, *, #63586, .T. ) ;
#6800 = FACE_OUTER_BOUND ( 'NONE', #19750, .T. ) ;
#6801 = DIRECTION ( 'NONE',  ( 1.000000000000000000, 0.000000000000000000, 0.000000000000000000 ) ) ;
#6802 = DIRECTION ( 'NONE',  ( -1.000000000000000000, -0.000000000000000000, 0.000000000000000000 ) ) ;
#6803 = CARTESIAN_POINT ( 'NONE',  ( 10.00000000000000000, 50.95692526931328104, 58.39081064771769292 ) ) ;
#6804 = FACE_OUTER_BOUND ( 'NONE', #71179, .T. ) ;
#6805 = LINE ( 'NONE', #6448, #68837 ) ;
#6806 = CARTESIAN_POINT ( 'NONE',  ( -92.69370383062498320, -209.9999999999999716, 76.14906250086716000 ) ) ;
#6807 = EDGE_CURVE ( 'NONE', #5113, #61245, #8803, .T. ) ;
#6808 = CARTESIAN_POINT ( 'NONE',  ( 10.00000000000000000, -36.88895765772637247, 6.736453364083436313 ) ) ;
#6809 = EDGE_CURVE ( 'NONE', #10929, #31307, #10786, .T. ) ;
#6810 = ORIENTED_EDGE ( 'NONE', *, *, #72124, .T. ) ;
#6811 = CARTESIAN_POINT ( 'NONE',  ( 10.00000000000000000, 0.000000000000000000, 0.000000000000000000 ) ) ;
#6812 = DIRECTION ( 'NONE',  ( -7.959965316982041921E-16, -1.065814103640131188E-14, -1.000000000000000000 ) ) ;
#6813 = LINE ( 'NONE', #1227, #65845 ) ;
#6814 = CARTESIAN_POINT ( 'NONE',  ( 5.999999999999999112, -27.74655509720617630, -77.16300072079690153 ) ) ;
#6815 = AXIS2_PLACEMENT_3D ( 'NONE', #29220, #40150, #62736 ) ;
#6816 = DIRECTION ( 'NONE',  ( 0.000000000000000000, 0.000000000000000000, -1.000000000000000000 ) ) ;
#6817 = ORIENTED_EDGE ( 'NONE', *, *, #10021, .T. ) ;
#6818 = DIRECTION ( 'NONE',  ( -1.000000000000000000, 0.000000000000000000, 0.000000000000000000 ) ) ;
#6819 = CARTESIAN_POINT ( 'NONE',  ( 11.99999999999999822, 8.840884882376133902, -74.65374052328640175 ) ) ;
#6820 = ORIENTED_EDGE ( 'NONE', *, *, #57955, .T. ) ;
#6821 = CARTESIAN_POINT ( 'NONE',  ( 97.30629616937498838, -211.3315407142195852, 86.73239583420047438 ) ) ;
#6822 = CARTESIAN_POINT ( 'NONE',  ( 0.000000000000000000, -37.22597642581153821, -5.202137450156795850 ) ) ;
#6823 = VECTOR ( 'NONE', #40176, 1000.000000000000000 ) ;
#6824 = ORIENTED_EDGE ( 'NONE', *, *, #61288, .F. ) ;
#6825 = CARTESIAN_POINT ( 'NONE',  ( 97.30629616937498838, -208.6684592857803011, 89.53697916753382913 ) ) ;
#6826 = AXIS2_PLACEMENT_3D ( 'NONE', #10165, #33457, #45136 ) ;
#6827 = ORIENTED_EDGE ( 'NONE', *, *, #66744, .F. ) ;
#6828 = CARTESIAN_POINT ( 'NONE',  ( 0.000000000000000000, 38.55633173627034438, -16.65560815589369881 ) ) ;
#6829 = VERTEX_POINT ( 'NONE', #52109 ) ;
#6830 = CARTESIAN_POINT ( 'NONE',  ( -96.15314808468751551, 88.00268892867056536, 80.38239583420048007 ) ) ;
#6831 = ORIENTED_EDGE ( 'NONE', *, *, #16640, .T. ) ;
#6832 = VECTOR ( 'NONE', #20872, 1000.000000000000000 ) ;
#6833 = ORIENTED_EDGE ( 'NONE', *, *, #53751, .T. ) ;
#6834 = CARTESIAN_POINT ( 'NONE',  ( 12.49999999999999645, 1.530808498934191127E-15, 53.20000000000001705 ) ) ;
#6835 = VECTOR ( 'NONE', #70865, 1000.000000000000000 ) ;
#6836 = ORIENTED_EDGE ( 'NONE', *, *, #43544, .T. ) ;
#6837 = DIRECTION ( 'NONE',  ( -1.000000000000000000, -0.000000000000000000, 0.000000000000000000 ) ) ;
#6838 = CARTESIAN_POINT ( 'NONE',  ( 97.64999999999999147, -209.9999999999999716, 79.52249999999999375 ) ) ;
#6839 = ADVANCED_FACE ( 'NONE', ( #35191 ), #33708, .T. ) ;
#6840 = ORIENTED_EDGE ( 'NONE', *, *, #68105, .F. ) ;
#6842 = DIRECTION ( 'NONE',  ( 1.000000000000000000, 0.000000000000000000, 0.000000000000000000 ) ) ;
#6841 = PRODUCT_DEFINITION_SHAPE ( 'NONE', 'NONE',  #74354 ) ;
#6843 = AXIS2_PLACEMENT_3D ( 'NONE', #30451, #53763, #42493 ) ;
#6844 = AXIS2_PLACEMENT_3D ( 'NONE', #62874, #57949, #45574 ) ;
#6845 = EDGE_LOOP ( 'NONE', ( #46434, #7193 ) ) ;
#6846 =( BOUNDED_CURVE ( )  B_SPLINE_CURVE ( 2, ( #34877, #39782, #33368, #39406, #39033, #22488, #28111, #34493, #10835 ),
 .UNSPECIFIED., .F., .F. ) 
 B_SPLINE_CURVE_WITH_KNOTS ( ( 3, 2, 2, 2, 3 ),
 ( 0.9313609857393206903, 0.9313610513964741822, 0.9384168169373561241, 0.9454725824782379551, 0.9525283480321509177 ),
 .UNSPECIFIED. ) 
 CURVE ( )  GEOMETRIC_REPRESENTATION_ITEM ( )  RATIONAL_B_SPLINE_CURVE ( ( 0.9999975066323494310, 0.9999987533045736621, 1.000000000000000000, 0.8660254037844387076, 1.000000000000000000, 0.8660254037844387076, 1.000000000000000000, 0.8660254037844387076, 1.000000000000000000 ) ) 
 REPRESENTATION_ITEM ( '' )  );
#6847 = CARTESIAN_POINT ( 'NONE',  ( 97.64999999999999147, -210.0000000207152198, 80.87187500099602744 ) ) ;
#6848 = EDGE_LOOP ( 'NONE', ( #34742, #64084, #4073, #36549 ) ) ;
#6849 = ORIENTED_EDGE ( 'NONE', *, *, #61978, .F. ) ;
#6850 = ORIENTED_EDGE ( 'NONE', *, *, #46524, .F. ) ;
#6851 = CARTESIAN_POINT ( 'NONE',  ( 95.00000000000000000, -212.6630814284392557, 80.91156250086714863 ) ) ;
#6852 = APPLICATION_PROTOCOL_DEFINITION ( 'draft international standard', 'automotive_design', 1998, #16238 ) ;
#6853 = CARTESIAN_POINT ( 'NONE',  ( -92.34999999999999432, -211.5299782133524218, 81.45395833506763950 ) ) ;
#6854 = AXIS2_PLACEMENT_3D ( 'NONE', #28837, #23210, #52884 ) ;
#6855 = CARTESIAN_POINT ( 'NONE',  ( 10.00000000000000000, 17.28742895386191236, -75.54627589209927407 ) ) ;
#6856 = CARTESIAN_POINT ( 'NONE',  ( 92.34999999999999432, 90.00000000000002842, 84.92000000000000171 ) ) ;
#6857 = FACE_OUTER_BOUND ( 'NONE', #28370, .T. ) ;
#6858 = EDGE_CURVE ( 'NONE', #16851, #32740, #40098, .T. ) ;
#6859 = DIRECTION ( 'NONE',  ( -1.000000000000000000, 0.000000000000000000, 0.000000000000000000 ) ) ;
#6860 = DIRECTION ( 'NONE',  ( -1.000000000000000000, 0.000000000000000000, 0.000000000000000000 ) ) ;
#6861 = CARTESIAN_POINT ( 'NONE',  ( -97.30629616937495996, -209.9999999999999716, 84.56281250086713897 ) ) ;
#6862 = EDGE_CURVE ( 'NONE', #50810, #42112, #26823, .T. ) ;
#6863 = CARTESIAN_POINT ( 'NONE',  ( -96.15314808468751551, 88.00268892867056536, 81.65239583420049030 ) ) ;
#6864 = ORIENTED_EDGE ( 'NONE', *, *, #31795, .F. ) ;
#6865 = CARTESIAN_POINT ( 'NONE',  ( 92.69370383062498320, 91.33154071421968467, 83.87489583420047268 ) ) ;
#6866 = VERTEX_POINT ( 'NONE', #69044 ) ;
#6867 = DIRECTION ( 'NONE',  ( -1.000000000000000000, -0.000000000000000000, -0.000000000000000000 ) ) ;
#6868 = CARTESIAN_POINT ( 'NONE',  ( -10.00000000000000000, 0.000000000000000000, 0.000000000000000000 ) ) ;
#6869 = DIRECTION ( 'NONE',  ( 0.000000000000000000, 0.000000000000000000, 1.000000000000000000 ) ) ;
#6870 = CARTESIAN_POINT ( 'NONE',  ( 0.000000000000000000, 0.000000000000000000, 0.000000000000000000 ) ) ;
#6871 = DIRECTION ( 'NONE',  ( -0.000000000000000000, -0.000000000000000000, -1.000000000000000000 ) ) ;
#6872 = CARTESIAN_POINT ( 'NONE',  ( -92.69370383062498320, -211.3315407142195852, 85.46239583420044994 ) ) ;
#6873 = DIRECTION ( 'NONE',  ( 1.000000000000000000, 0.000000000000000000, 0.000000000000000000 ) ) ;
#6874 = ADVANCED_FACE ( 'NONE', ( #71233 ), #31016, .T. ) ;
#6875 = FACE_OUTER_BOUND ( 'NONE', #39427, .T. ) ;
#6876 = DIRECTION ( 'NONE',  ( -1.000000000000000000, -0.000000000000000000, 0.000000000000000000 ) ) ;
#6877 = CARTESIAN_POINT ( 'NONE',  ( 12.49999999999999645, 1.530808498934191127E-15, 125.0000000000000000 ) ) ;
#6878 = ORIENTED_EDGE ( 'NONE', *, *, #18069, .T. ) ;
#6879 = ORIENTED_EDGE ( 'NONE', *, *, #28754, .F. ) ;
#6880 = CARTESIAN_POINT ( 'NONE',  ( -92.35000000000003695, 90.00000000000004263, 77.61749999999999261 ) ) ;
#6881 = CARTESIAN_POINT ( 'NONE',  ( 11.99999999999999822, 74.65374052328660071, -8.840884882374309583 ) ) ;
#6882 = DIRECTION ( 'NONE',  ( -0.000000000000000000, -0.000000000000000000, -1.000000000000000000 ) ) ;
#6883 = CARTESIAN_POINT ( 'NONE',  ( 6.000000000000000000, 74.18225833017937987, -34.94270380257559339 ) ) ;
#6884 = DIRECTION ( 'NONE',  ( 0.000000000000000000, -0.8660254037844363761, 0.5000000000000038858 ) ) ;
#6885 = CARTESIAN_POINT ( 'NONE',  ( 11.99999999999999822, 74.65491531819118620, -8.830959090342659579 ) ) ;
#6886 = CARTESIAN_POINT ( 'NONE',  ( 0.000000000000000000, 46.11716303203188261, 67.80270845531904911 ) ) ;
#6887 = EDGE_CURVE ( 'NONE', #14607, #38641, #46052, .T. ) ;
#6888 = EDGE_LOOP ( 'NONE', ( #49753, #7608, #30221, #14110 ) ) ;
#6889 = CARTESIAN_POINT ( 'NONE',  ( -92.69370383062502583, 88.66845928578038638, 75.93739583420047268 ) ) ;
#6890 = CIRCLE ( 'NONE', #40478, 77.49899999999999523 ) ;
#6891 = CARTESIAN_POINT ( 'NONE',  ( -2.499999999999971578, 69.70000000000003126, -255.0000000000000000 ) ) ;
#6892 = DIRECTION ( 'NONE',  ( 1.000000000000000000, 0.000000000000000000, 0.000000000000000000 ) ) ;
#6893 = CARTESIAN_POINT ( 'NONE',  ( 12.74955575014744547, 0.001194404164628405998, 127.4927882439603195 ) ) ;
#6894 = CIRCLE ( 'NONE', #20086, 31.99999999999999645 ) ;
#6895 = CARTESIAN_POINT ( 'NONE',  ( 12.00000000000000000, 8.688484142253932063, -21.88630264137371029 ) ) ;
#6896 = CARTESIAN_POINT ( 'NONE',  ( 7.999999999999991118, 2.252361157298889269E-13, 20.20000000000000995 ) ) ;
#6897 = CARTESIAN_POINT ( 'NONE',  ( -97.30629616937497417, -208.6684592857803011, 84.66864583420047552 ) ) ;
#6898 = CIRCLE ( 'NONE', #48899, 16.00000000000000000 ) ;
#6899 = ADVANCED_FACE ( 'NONE', ( #1761 ), #59237, .F. ) ;
#6900 = DIRECTION ( 'NONE',  ( 0.9227826878668550226, 0.3853207896976523772, -0.000000000000000000 ) ) ;
#6901 = ADVANCED_FACE ( 'NONE', ( #70872 ), #61617, .T. ) ;
#6902 = ADVANCED_FACE ( 'NONE', ( #2513 ), #24290, .T. ) ;
#6903 = CARTESIAN_POINT ( 'NONE',  ( 96.15314808468748708, 88.00268892867053694, 78.58322916753382970 ) ) ;
#6904 = CARTESIAN_POINT ( 'NONE',  ( -92.69370383062498320, -209.9999999999999716, 75.51406250086715488 ) ) ;
#6905 = CARTESIAN_POINT ( 'NONE',  ( 97.64999999999999147, 90.00000000000002842, 88.41249999999999432 ) ) ;
#6906 = EDGE_LOOP ( 'NONE', ( #63747, #29710, #40514, #15687 ) ) ;
#6907 = CARTESIAN_POINT ( 'NONE',  ( 11.99999999999999822, 18.89407956138362010, -75.16055320797013906 ) ) ;
#6908 = CYLINDRICAL_SURFACE ( 'NONE', #32267, 2.649999999999985700 ) ;
#6909 = CARTESIAN_POINT ( 'NONE',  ( 0.000000000000000000, 27.13269053701096922, 25.88420570971410228 ) ) ;
#6910 = CARTESIAN_POINT ( 'NONE',  ( -95.00000000000002842, 92.66308142843932671, 75.67281250086715261 ) ) ;
#6911 = CARTESIAN_POINT ( 'NONE',  ( 92.69370383062501162, -211.3315407142195852, 77.63072916753380071 ) ) ;
#6912 = EDGE_LOOP ( 'NONE', ( #43721, #32938, #12694, #4735 ) ) ;
#6913 = FACE_OUTER_BOUND ( 'NONE', #64183, .T. ) ;
#6914 = EDGE_LOOP ( 'NONE', ( #17202, #9152, #57698, #31329 ) ) ;
#6915 = DIRECTION ( 'NONE',  ( 0.000000000000000000, 0.000000000000000000, 1.000000000000000000 ) ) ;
#6916 = VERTEX_POINT ( 'NONE', #19736 ) ;
#6917 = DIRECTION ( 'NONE',  ( -1.000000000000000000, 0.000000000000000000, 0.000000000000000000 ) ) ;
#6918 = ORIENTED_EDGE ( 'NONE', *, *, #61542, .T. ) ;
#6919 = ORIENTED_EDGE ( 'NONE', *, *, #72571, .T. ) ;
#6920 = ORIENTED_EDGE ( 'NONE', *, *, #40087, .T. ) ;
#6921 = CARTESIAN_POINT ( 'NONE',  ( -12.50000000000000000, -132.5000000000000000, 40.00000000000000000 ) ) ;
#6922 = EDGE_LOOP ( 'NONE', ( #39250, #7519, #61602, #500 ) ) ;
#6923 = ORIENTED_EDGE ( 'NONE', *, *, #25705, .T. ) ;
#6924 = CARTESIAN_POINT ( 'NONE',  ( 97.30629616937498838, 91.33154071421968467, 81.91697916753381037 ) ) ;
#6925 = CARTESIAN_POINT ( 'NONE',  ( 4.999999999999999112, 40.68715046381927891, 10.41901085202092858 ) ) ;
#6926 = CARTESIAN_POINT ( 'NONE',  ( -9.937067298023318784, 7.583184918921300088, 125.0000000000000000 ) ) ;
#6927 = AXIS2_PLACEMENT_3D ( 'NONE', #67549, #34437, #22813 ) ;
#6928 = ORIENTED_EDGE ( 'NONE', *, *, #65558, .T. ) ;
#6929 = ORIENTED_EDGE ( 'NONE', *, *, #15217, .F. ) ;
#6930 = ADVANCED_FACE ( 'NONE', ( #42683 ), #35922, .T. ) ;
#6931 = VERTEX_POINT ( 'NONE', #41567 ) ;
#6932 = CARTESIAN_POINT ( 'NONE',  ( 0.000000000000000000, 40.68715046381927891, 10.41901085202092858 ) ) ;
#6933 = EDGE_LOOP ( 'NONE', ( #44905, #10621, #14116, #51379, #39222 ) ) ;
#6934 = DIRECTION ( 'NONE',  ( 0.000000000000000000, -0.5224985647159380298, -0.8526401643540988395 ) ) ;
#6935 = AXIS2_PLACEMENT_3D ( 'NONE', #4127, #72512, #71766 ) ;
#6936 = CARTESIAN_POINT ( 'NONE',  ( 6.782329983125270800, 10.49999999999999467, -20.00000000000000000 ) ) ;
#6937 = DIRECTION ( 'NONE',  ( 0.000000000000000000, 0.000000000000000000, 1.000000000000000000 ) ) ;
#6938 = CIRCLE ( 'NONE', #50129, 77.49899999999999523 ) ;
#6939 = CARTESIAN_POINT ( 'NONE',  ( 92.35000000000000853, -209.9999999999999716, 82.45937500173430124 ) ) ;
#6940 = EDGE_CURVE ( 'NONE', #39621, #7767, #66587, .T. ) ;
#6941 = FACE_OUTER_BOUND ( 'NONE', #22281, .T. ) ;
#6942 = DIRECTION ( 'NONE',  ( 0.000000000000000000, 0.000000000000000000, 1.000000000000000000 ) ) ;
#6943 = CARTESIAN_POINT ( 'NONE',  ( -92.34999999999999432, -208.4700217866474645, 79.01979166840095559 ) ) ;
#6944 = ORIENTED_EDGE ( 'NONE', *, *, #69129, .T. ) ;
#6945 = EDGE_CURVE ( 'NONE', #27925, #50886, #4692, .T. ) ;
#6946 = DIRECTION ( 'NONE',  ( 1.000000000000000000, 1.427937372958405461E-15, 7.962523111839130290E-16 ) ) ;
#6947 = ORIENTED_EDGE ( 'NONE', *, *, #15118, .T. ) ;
#6949 = CARTESIAN_POINT ( 'NONE',  ( -97.65000000000001990, 91.52997821335253548, 76.05645833506761733 ) ) ;
#6948 = CARTESIAN_POINT ( 'NONE',  ( 92.34999999999999432, 90.00000000000002842, 80.55437500173430010 ) ) ;
#6950 = ORIENTED_EDGE ( 'NONE', *, *, #13215, .F. ) ;
#6951 = CARTESIAN_POINT ( 'NONE',  ( 97.30629616937498838, 90.00000000000002842, 80.59406250086715318 ) ) ;
#6952 = CARTESIAN_POINT ( 'NONE',  ( 10.00000000000000000, 0.000000000000000000, 0.000000000000000000 ) ) ;
#6953 = DIRECTION ( 'NONE',  ( 0.000000000000000000, 0.000000000000000000, 1.000000000000000000 ) ) ;
#6954 = DIRECTION ( 'NONE',  ( -0.000000000000000000, -0.000000000000000000, 1.000000000000000000 ) ) ;
#6955 = CYLINDRICAL_SURFACE ( 'NONE', #51023, 42.00000000000000000 ) ;
#6956 = EDGE_CURVE ( 'NONE', #1870, #975, #52046, .T. ) ;
#6957 = ORIENTED_EDGE ( 'NONE', *, *, #59238, .T. ) ;
#6958 = CARTESIAN_POINT ( 'NONE',  ( 0.000000000000000000, -22.90783923731575200, -78.73519480814978522 ) ) ;
#6959 = CARTESIAN_POINT ( 'NONE',  ( 1.648146632868999539, 4.821944789745367110, -6.000000000000003553 ) ) ;
#6960 = ORIENTED_EDGE ( 'NONE', *, *, #51937, .T. ) ;
#6961 = AXIS2_PLACEMENT_3D ( 'NONE', #15987, #28005, #39680 ) ;
#6962 = EDGE_LOOP ( 'NONE', ( #20044, #40146, #30752, #10339 ) ) ;
#6963 = CIRCLE ( 'NONE', #65787, 2.541999999999999815 ) ;
#6964 = AXIS2_PLACEMENT_3D ( 'NONE', #16438, #15702, #45025 ) ;
#6965 = AXIS2_PLACEMENT_3D ( 'NONE', #34726, #52007, #197 ) ;
#6966 = FACE_BOUND ( 'NONE', #58248, .T. ) ;
#6967 = EDGE_CURVE ( 'NONE', #40320, #37554, #13363, .T. ) ;
#6968 = CARTESIAN_POINT ( 'NONE',  ( -2.008727693139930270, -4.613763217533273675, -0.5592653008974395323 ) ) ;
#6969 = DIRECTION ( 'NONE',  ( 1.000000000000000000, 0.000000000000000000, 0.000000000000000000 ) ) ;
#6970 = CARTESIAN_POINT ( 'NONE',  ( -92.69370383062498320, -211.3315407142195852, 79.27114583420048177 ) ) ;
#6971 = AXIS2_PLACEMENT_3D ( 'NONE', #24476, #35022, #18820 ) ;
#6972 = EDGE_CURVE ( 'NONE', #16649, #25971, #31389, .T. ) ;
#6973 = ORIENTED_EDGE ( 'NONE', *, *, #51766, .T. ) ;
#6974 = DIRECTION ( 'NONE',  ( 0.000000000000000000, 0.000000000000000000, 1.000000000000000000 ) ) ;
#6975 = CARTESIAN_POINT ( 'NONE',  ( 97.64999999999999147, 90.00000000000002842, 82.06250000000000000 ) ) ;
#6976 = DIRECTION ( 'NONE',  ( -1.000000000000000000, 0.000000000000000000, 0.000000000000000000 ) ) ;
#6977 = CYLINDRICAL_SURFACE ( 'NONE', #40073, 16.00000000000000000 ) ;
#6978 = CARTESIAN_POINT ( 'NONE',  ( -26.50000000000000355, -120.0000000000000000, -64.00000000000000000 ) ) ;
#6979 = DIRECTION ( 'NONE',  ( 0.000000000000000000, 0.8526401643540935105, -0.5224985647159468005 ) ) ;
#6980 = FACE_OUTER_BOUND ( 'NONE', #1959, .T. ) ;
#6981 = CARTESIAN_POINT ( 'NONE',  ( -92.34999999999993747, -211.5299782133523934, 76.29458333333333542 ) ) ;
#6982 = LINE ( 'NONE', #41209, #70562 ) ;
#6983 = EDGE_CURVE ( 'NONE', #64759, #64357, #35556, .T. ) ;
#6984 = ADVANCED_FACE ( 'NONE', ( #36293 ), #64508, .T. ) ;
#6985 =( GEOMETRIC_REPRESENTATION_CONTEXT ( 3 ) GLOBAL_UNCERTAINTY_ASSIGNED_CONTEXT ( ( #42869 ) ) GLOBAL_UNIT_ASSIGNED_CONTEXT ( ( #15634, #241, #11822 ) ) REPRESENTATION_CONTEXT ( 'NONE', 'WORKASPACE' ) );
#6986 = CARTESIAN_POINT ( 'NONE',  ( 92.69370383062498320, 91.33154071421968467, 87.84364583420048689 ) ) ;
#6987 = VECTOR ( 'NONE', #72351, 1000.000000000000227 ) ;
#6988 = CARTESIAN_POINT ( 'NONE',  ( -94.99999999999997158, -207.3369185715606307, 85.19781250086714408 ) ) ;
#6989 = FACE_OUTER_BOUND ( 'NONE', #5098, .T. ) ;
#6990 = ORIENTED_EDGE ( 'NONE', *, *, #51705, .T. ) ;
#6991 = CARTESIAN_POINT ( 'NONE',  ( -92.35000000000003695, 90.00000000000004263, 81.42749999999999488 ) ) ;
#6992 = CARTESIAN_POINT ( 'NONE',  ( -97.64999999999994884, -208.4700217866474645, 79.78708333333332803 ) ) ;
#6993 = CARTESIAN_POINT ( 'NONE',  ( -92.69370383062504004, 90.00000000000004263, 77.89531250086714920 ) ) ;
#6994 = VECTOR ( 'NONE', #10304, 1000.000000000000000 ) ;
#6995 = VECTOR ( 'NONE', #21302, 1000.000000000000114 ) ;
#6996 = CARTESIAN_POINT ( 'NONE',  ( 97.30629616937498838, -209.9999999999999716, 88.69031250086715090 ) ) ;
#6997 = ORIENTED_EDGE ( 'NONE', *, *, #46879, .F. ) ;
#6998 = EDGE_LOOP ( 'NONE', ( #30721, #64306, #50564, #51435 ) ) ;
#6999 = ORIENTED_EDGE ( 'NONE', *, *, #44465, .F. ) ;
#7000 = CIRCLE ( 'NONE', #21419, 82.00000000000000000 ) ;
#7001 = CYLINDRICAL_SURFACE ( 'NONE', #27515, 31.99999999999999289 ) ;
#7002 = FACE_OUTER_BOUND ( 'NONE', #16624, .T. ) ;
#7003 = CIRCLE ( 'NONE', #41845, 31.99999999999998934 ) ;
#7004 = VERTEX_POINT ( 'NONE', #73083 ) ;
#7005 = ORIENTED_EDGE ( 'NONE', *, *, #49496, .F. ) ;
#7006 = VECTOR ( 'NONE', #54632, 1000.000000000000000 ) ;
#7007 = VECTOR ( 'NONE', #13642, 1000.000000000000114 ) ;
#7008 = CARTESIAN_POINT ( 'NONE',  ( 92.69370383062501162, -211.3315407142195852, 81.59947916753382913 ) ) ;
#7009 = CARTESIAN_POINT ( 'NONE',  ( 20.85212586905262100, -130.9402397935870965, 5.500000000000000000 ) ) ;
#7010 = LINE ( 'NONE', #1429, #47202 ) ;
#7011 =( GEOMETRIC_REPRESENTATION_CONTEXT ( 3 ) GLOBAL_UNCERTAINTY_ASSIGNED_CONTEXT ( ( #19549 ) ) GLOBAL_UNIT_ASSIGNED_CONTEXT ( ( #25581, #48514, #8671 ) ) REPRESENTATION_CONTEXT ( 'NONE', 'WORKASPACE' ) );
#7012 = CARTESIAN_POINT ( 'NONE',  ( 4.999999999999999112, 0.2838785441256751474, -0.5080592402122395823 ) ) ;
#7013 = CARTESIAN_POINT ( 'NONE',  ( 92.35000000000000853, -209.9999999999999716, 76.66499999999999204 ) ) ;
#7014 = CARTESIAN_POINT ( 'NONE',  ( 11.99999999999999822, -66.50666863321974631, -39.78640506895675344 ) ) ;
#7015 = CARTESIAN_POINT ( 'NONE',  ( 97.64999999999999147, -209.9999999999999716, 83.96750000000000114 ) ) ;
#7016 = EDGE_CURVE ( 'NONE', #60338, #26546, #11266, .T. ) ;
#7017 = ORIENTED_EDGE ( 'NONE', *, *, #55835, .T. ) ;
#7018 = ORIENTED_EDGE ( 'NONE', *, *, #69502, .F. ) ;
#7019 = ORIENTED_EDGE ( 'NONE', *, *, #13477, .T. ) ;
#7020 = ORIENTED_EDGE ( 'NONE', *, *, #3994, .T. ) ;
#7021 = FACE_OUTER_BOUND ( 'NONE', #53424, .T. ) ;
#7022 = ADVANCED_FACE ( 'NONE', ( #21210 ), #61662, .T. ) ;
#7023 = CARTESIAN_POINT ( 'NONE',  ( -95.00000000000002842, 87.33691857156074434, 86.15031250086714465 ) ) ;
#7024 = LINE ( 'NONE', #29950, #30545 ) ;
#7025 = EDGE_CURVE ( 'NONE', #26361, #63641, #27221, .T. ) ;
#7026 = DIRECTION ( 'NONE',  ( -0.000000000000000000, -0.000000000000000000, 1.000000000000000000 ) ) ;
#7027 = CARTESIAN_POINT ( 'NONE',  ( 97.30629616937498838, -211.3315407142195852, 88.00239583420047040 ) ) ;
#7028 = ADVANCED_FACE ( 'NONE', ( #14847 ), #61083, .T. ) ;
#7029 = CARTESIAN_POINT ( 'NONE',  ( 96.32499999999998863, 87.70503267997126784, 78.14666666666667538 ) ) ;
#7030 = ORIENTED_EDGE ( 'NONE', *, *, #65481, .T. ) ;
#7031 = LINE ( 'NONE', #30328, #70757 ) ;
#7032 = VERTEX_POINT ( 'NONE', #32123 ) ;
#7033 = VERTEX_POINT ( 'NONE', #9581 ) ;
#7034 = CARTESIAN_POINT ( 'NONE',  ( -95.00000000000002842, 93.05995642670501411, 87.38062500173430180 ) ) ;
#7035 = AXIS2_PLACEMENT_3D ( 'NONE', #62553, #11036, #26462 ) ;
#7036 = CARTESIAN_POINT ( 'NONE',  ( 97.30629616937498838, 90.00000000000002842, 75.99031250086714806 ) ) ;
#7037 = EDGE_LOOP ( 'NONE', ( #6207, #35670, #34432, #6379 ) ) ;
#7038 = LINE ( 'NONE', #40519, #23756 ) ;
#7039 = AXIS2_PLACEMENT_3D ( 'NONE', #6535, #42589, #20756 ) ;
#7040 = AXIS2_PLACEMENT_3D ( 'NONE', #10969, #4977, #71982 ) ;
#7041 = LINE ( 'NONE', #18323, #33781 ) ;
#7042 = CARTESIAN_POINT ( 'NONE',  ( 10.00000000000000000, -26.08949754953044220, 27.05870788708222818 ) ) ;
#7043 = ADVANCED_FACE ( 'NONE', ( #9205 ), #20107, .F. ) ;
#7044 = DIRECTION ( 'NONE',  ( -0.000000000000000000, -0.000000000000000000, 1.000000000000000000 ) ) ;
#7045 = VERTEX_POINT ( 'NONE', #60724 ) ;
#7046 = CARTESIAN_POINT ( 'NONE',  ( 10.00000000000000000, 55.19960302592066625, 51.03279382321107249 ) ) ;
#7047 = DIRECTION ( 'NONE',  ( -0.000000000000000000, -0.000000000000000000, -1.000000000000000000 ) ) ;
#7048 = ORIENTED_EDGE ( 'NONE', *, *, #11978, .F. ) ;
#7049 = VECTOR ( 'NONE', #32393, 1000.000000000000000 ) ;
#7050 = VERTEX_POINT ( 'NONE', #55815 ) ;
#7051 = CONICAL_SURFACE ( 'NONE', #13055, 17.30399999999999849, 0.2094395102393129815 ) ;
#7052 = CYLINDRICAL_SURFACE ( 'NONE', #1420, 42.00000000000000000 ) ;
#7053 = CARTESIAN_POINT ( 'NONE',  ( 10.00000000000000000, -33.79645857604525361, 16.45098606841114730 ) ) ;
#7054 = EDGE_CURVE ( 'NONE', #26436, #35888, #55643, .T. ) ;
#7055 = CARTESIAN_POINT ( 'NONE',  ( 92.35000000000000853, -209.9999999999999716, 87.45999999999999375 ) ) ;
#7056 = VERTEX_POINT ( 'NONE', #49053 ) ;
#7057 = CARTESIAN_POINT ( 'NONE',  ( -96.15314808468745866, -211.9973110713294489, 86.73239583420048859 ) ) ;
#7058 = ORIENTED_EDGE ( 'NONE', *, *, #58375, .T. ) ;
#7059 =( NAMED_UNIT ( * ) PLANE_ANGLE_UNIT ( ) SI_UNIT ( $, .RADIAN. ) );
#7060 = EDGE_CURVE ( 'NONE', #1094, #43028, #54701, .T. ) ;
#7061 = ORIENTED_EDGE ( 'NONE', *, *, #48033, .T. ) ;
#7062 = VECTOR ( 'NONE', #11047, 1000.000000000000000 ) ;
#7063 = AXIS2_PLACEMENT_3D ( 'NONE', #43363, #8392, #60644 ) ;
#7064 = ORIENTED_EDGE ( 'NONE', *, *, #32233, .F. ) ;
#7065 = CARTESIAN_POINT ( 'NONE',  ( 21.07894319797337701, -103.8699611390234878, 5.500000000000000000 ) ) ;
#7066 = EDGE_CURVE ( 'NONE', #3169, #65641, #61463, .T. ) ;
#7067 = EDGE_CURVE ( 'NONE', #4558, #6335, #3598, .T. ) ;
#7068 = AXIS2_PLACEMENT_3D ( 'NONE', #32258, #48818, #60491 ) ;
#7069 = CARTESIAN_POINT ( 'NONE',  ( 0.000000000000000000, 2.935248768560057897, -3.252606517456513302E-15 ) ) ;
#7070 = CARTESIAN_POINT ( 'NONE',  ( 97.30629616937498838, 88.66845928578035796, 82.92239583420045790 ) ) ;
#7071 = DIRECTION ( 'NONE',  ( -1.000000000000000000, -0.000000000000000000, -0.000000000000000000 ) ) ;
#7072 = DIRECTION ( 'NONE',  ( -7.685483754327489091E-16, -1.065814103640131188E-14, -1.000000000000000000 ) ) ;
#7073 = CARTESIAN_POINT ( 'NONE',  ( -93.67500000000003979, 92.29496732002878900, 80.89833333333332632 ) ) ;
#7074 = CIRCLE ( 'NONE', #55046, 16.00000000000000000 ) ;
#7075 = DIRECTION ( 'NONE',  ( 0.000000000000000000, -0.4539904997395351471, -0.8910065241883737830 ) ) ;
#7076 = DIRECTION ( 'NONE',  ( -1.000000000000000000, -0.000000000000000000, 0.000000000000000000 ) ) ;
#7077 = CARTESIAN_POINT ( 'NONE',  ( 11.99999999999999822, 0.000000000000000000, 0.000000000000000000 ) ) ;
#7078 = CARTESIAN_POINT ( 'NONE',  ( 0.000000000000000000, -29.81001611430991360, -22.74946021919165418 ) ) ;
#7079 = ADVANCED_FACE ( 'NONE', ( #4329 ), #44162, .F. ) ;
#7080 = AXIS2_PLACEMENT_3D ( 'NONE', #27236, #14487, #67481 ) ;
#7081 =( BOUNDED_CURVE ( )  B_SPLINE_CURVE ( 2, ( #23908, #59602, #35547, #18988, #13357, #46847, #7360 ),
 .UNSPECIFIED., .F., .F. ) 
 B_SPLINE_CURVE_WITH_KNOTS ( ( 3, 2, 2, 3 ),
 ( 0.2328402629019979686, 0.2398960283900005708, 0.2469517939308829568, 0.2540073681283125939 ),
 .UNSPECIFIED. ) 
 CURVE ( )  GEOMETRIC_REPRESENTATION_ITEM ( )  RATIONAL_B_SPLINE_CURVE ( ( 1.000000000000000000, 0.8660254037844387076, 1.000000000000000000, 0.8660254037844387076, 1.000000000000000000, 0.8660290370063296050, 0.9999927337532750204 ) ) 
 REPRESENTATION_ITEM ( '' )  );
#7082 = CARTESIAN_POINT ( 'NONE',  ( 10.00000000000000000, 17.80606268964585226, -33.00180498840028775 ) ) ;
#7083 = EDGE_CURVE ( 'NONE', #48585, #10371, #8842, .T. ) ;
#7084 = DIRECTION ( 'NONE',  ( -1.000000000000000000, -0.000000000000000000, 0.000000000000000000 ) ) ;
#7085 = CARTESIAN_POINT ( 'NONE',  ( -95.00000000000002842, 92.66308142843932671, 85.03906250086714635 ) ) ;
#7086 = CARTESIAN_POINT ( 'NONE',  ( 97.64999999999999147, 90.00000000000002842, 83.33250000000001023 ) ) ;
#7087 = AXIS2_PLACEMENT_3D ( 'NONE', #41807, #35065, #6860 ) ;
#7088 = DIRECTION ( 'NONE',  ( 0.000000000000000000, 0.000000000000000000, 1.000000000000000000 ) ) ;
#7089 = ORIENTED_EDGE ( 'NONE', *, *, #55487, .T. ) ;
#7091 = DIRECTION ( 'NONE',  ( -0.000000000000000000, -0.000000000000000000, -1.000000000000000000 ) ) ;
#7090 = AXIS2_PLACEMENT_3D ( 'NONE', #36538, #70746, #20366 ) ;
#7092 = CARTESIAN_POINT ( 'NONE',  ( 97.64999999999821512, -209.9999969335172807, 75.79187510780352000 ) ) ;
#7093 = DIRECTION ( 'NONE',  ( 0.000000000000000000, -0.1564344650402380854, 0.9876883405951365491 ) ) ;
#7094 = CIRCLE ( 'NONE', #21512, 82.00000000000000000 ) ;
#7095 = CIRCLE ( 'NONE', #23904, 3.299999999999983391 ) ;
#7096 = CARTESIAN_POINT ( 'NONE',  ( 4.999999999999999112, -40.98264845739755202, 9.188173127307159405 ) ) ;
#7097 = CARTESIAN_POINT ( 'NONE',  ( 97.30629616937498838, -211.3315407142195852, 83.71614583420050337 ) ) ;
#7098 = CIRCLE ( 'NONE', #62225, 77.49899999999999523 ) ;
#7099 = AXIS2_PLACEMENT_3D ( 'NONE', #64251, #36030, #51848 ) ;
#7100 = ORIENTED_EDGE ( 'NONE', *, *, #14155, .F. ) ;
#7101 = VERTEX_POINT ( 'NONE', #20497 ) ;
#7102 =( NAMED_UNIT ( * ) SI_UNIT ( $, .STERADIAN. ) SOLID_ANGLE_UNIT ( ) );
#7103 = ORIENTED_EDGE ( 'NONE', *, *, #6363, .F. ) ;
#7104 = CARTESIAN_POINT ( 'NONE',  ( 97.65000000000004832, -208.4700217866474929, 88.46541666666664128 ) ) ;
#7105 = CARTESIAN_POINT ( 'NONE',  ( 93.84685191531249870, -208.0026889286704943, 75.56697916753381605 ) ) ;
#7106 = ORIENTED_EDGE ( 'NONE', *, *, #37091, .F. ) ;
#7107 = CARTESIAN_POINT ( 'NONE',  ( 93.84685191531249870, -208.0026889286704943, 80.17072916753382117 ) ) ;
#7108 = VECTOR ( 'NONE', #72787, 1000.000000000000000 ) ;
#7109 = VECTOR ( 'NONE', #36447, 1000.000000000000000 ) ;
#7110 = ORIENTED_EDGE ( 'NONE', *, *, #37391, .F. ) ;
#7111 = ADVANCED_FACE ( 'NONE', ( #72356 ), #15591, .T. ) ;
#7112 = CARTESIAN_POINT ( 'NONE',  ( 11.99999999999999822, -68.26794271651239399, -31.47745569255214093 ) ) ;
#7113 = EDGE_LOOP ( 'NONE', ( #6102, #61489, #13011, #14790 ) ) ;
#7114 = ORIENTED_EDGE ( 'NONE', *, *, #25956, .T. ) ;
#7115 = CARTESIAN_POINT ( 'NONE',  ( 10.00000000000000000, 41.76937507738875155, -62.50329211542393892 ) ) ;
#7116 = VECTOR ( 'NONE', #65821, 1000.000000000000000 ) ;
#7117 = CIRCLE ( 'NONE', #10716, 82.00000000000000000 ) ;
#7118 = EDGE_CURVE ( 'NONE', #36401, #37377, #20869, .T. ) ;
#7119 = FILL_AREA_STYLE ('',( #65015 ) ) ;
#7120 = DIRECTION ( 'NONE',  ( -1.000000000000000000, 0.000000000000000000, 0.000000000000000000 ) ) ;
#7121 = VECTOR ( 'NONE', #5658, 1000.000000000000000 ) ;
#7122 = VERTEX_POINT ( 'NONE', #30876 ) ;
#7123 = CARTESIAN_POINT ( 'NONE',  ( -92.35000000000012221, 91.52997821335257811, 84.02041666666666231 ) ) ;
#7124 = CARTESIAN_POINT ( 'NONE',  ( 95.00000000000000000, -213.0599564267049857, 84.52312500173428589 ) ) ;
#7125 = ADVANCED_FACE ( 'NONE', ( #30509 ), #3092, .T. ) ;
#7127 = AXIS2_PLACEMENT_3D ( 'NONE', #39842, #393, #11608 ) ;
#7126 = CARTESIAN_POINT ( 'NONE',  ( 92.34999999999999432, 90.00000000000002842, 89.36499999999999488 ) ) ;
#7128 = EDGE_CURVE ( 'NONE', #30173, #51588, #37289, .T. ) ;
#7129 = ORIENTED_EDGE ( 'NONE', *, *, #4336, .T. ) ;
#7130 = CARTESIAN_POINT ( 'NONE',  ( 0.000000000000000000, 0.000000000000000000, 0.000000000000000000 ) ) ;
#7131 = DIRECTION ( 'NONE',  ( -1.000000000000000000, -0.000000000000000000, 0.000000000000000000 ) ) ;
#7132 =( REPRESENTATION_RELATIONSHIP ('NONE','NONE', #31117, #10045 ) REPRESENTATION_RELATIONSHIP_WITH_TRANSFORMATION ( #16560 )SHAPE_REPRESENTATION_RELATIONSHIP( ) );
#7133 = ORIENTED_EDGE ( 'NONE', *, *, #68282, .T. ) ;
#7134 = ORIENTED_EDGE ( 'NONE', *, *, #4707, .F. ) ;
#7135 = CARTESIAN_POINT ( 'NONE',  ( 5.000000000000000000, -1.096207231254244352, -0.7463930790433302986 ) ) ;
#7136 = ORIENTED_EDGE ( 'NONE', *, *, #35084, .T. ) ;
#7137 = CARTESIAN_POINT ( 'NONE',  ( 97.64999999999999147, 90.00000000000002842, 86.58687500173429896 ) ) ;
#7138 = VERTEX_POINT ( 'NONE', #36895 ) ;
#7139 = ORIENTED_EDGE ( 'NONE', *, *, #8845, .T. ) ;
#7140 = CARTESIAN_POINT ( 'NONE',  ( 0.000000000000000000, 55.38113227695783536, 54.21277698773694453 ) ) ;
#7141 = LINE ( 'NONE', #70266, #58244 ) ;
#7142 = EDGE_LOOP ( 'NONE', ( #68629, #17378, #59631, #4786 ) ) ;
#7143 = ORIENTED_EDGE ( 'NONE', *, *, #72075, .T. ) ;
#7144 = EDGE_LOOP ( 'NONE', ( #45827, #45959, #17104, #11694 ) ) ;
#7145 = CARTESIAN_POINT ( 'NONE',  ( 10.00000000000000000, -8.966570791701267140, 81.50828551894223040 ) ) ;
#7146 = LINE ( 'NONE', #64299, #69748 ) ;
#7147 = EDGE_CURVE ( 'NONE', #34118, #41638, #25984, .T. ) ;
#7148 = CARTESIAN_POINT ( 'NONE',  ( -96.32500000000001705, 92.29496732002878900, 87.35416666666665719 ) ) ;
#7149 = ORIENTED_EDGE ( 'NONE', *, *, #66707, .T. ) ;
#7150 = CARTESIAN_POINT ( 'NONE',  ( 0.000000000000000000, 56.15606465355042332, -59.75363087400017292 ) ) ;
#7151 = DIRECTION ( 'NONE',  ( -1.000000000000000000, -0.000000000000000000, -0.000000000000000000 ) ) ;
#7152 = VERTEX_POINT ( 'NONE', #1629 ) ;
#7153 = DIRECTION ( 'NONE',  ( 0.000000000000000000, -0.9510565162951543083, 0.3090169943749449533 ) ) ;
#7154 = CARTESIAN_POINT ( 'NONE',  ( -96.15314808468747287, -208.0026889286704943, 82.55197916753380127 ) ) ;
#7155 = EDGE_LOOP ( 'NONE', ( #8988, #13476, #18055, #42338 ) ) ;
#7156 = AXIS2_PLACEMENT_3D ( 'NONE', #70281, #13881, #36820 ) ;
#7157 = FACE_OUTER_BOUND ( 'NONE', #57507, .T. ) ;
#7158 = LINE ( 'NONE', #25548, #34412 ) ;
#7159 = CARTESIAN_POINT ( 'NONE',  ( -97.64999999954989107, -210.0000310946949753, 88.81037122969127040 ) ) ;
#7160 = CARTESIAN_POINT ( 'NONE',  ( 10.00000000000000000, -54.21277698773715059, 55.38113227695762930 ) ) ;
#7161 = AXIS2_PLACEMENT_3D ( 'NONE', #73193, #26956, #72082 ) ;
#7162 = AXIS2_PLACEMENT_3D ( 'NONE', #7610, #47463, #52733 ) ;
#7163 = DIRECTION ( 'NONE',  ( 0.000000000000000000, -0.3090169943749349057, -0.9510565162951576390 ) ) ;
#7164 = EDGE_CURVE ( 'NONE', #73338, #3737, #71394, .T. ) ;
#7165 = EDGE_CURVE ( 'NONE', #52760, #33517, #70068, .T. ) ;
#7166 =( LENGTH_UNIT ( ) NAMED_UNIT ( * ) SI_UNIT ( .MILLI., .METRE. ) );
#7168 = AXIS2_PLACEMENT_3D ( 'NONE', #61939, #57042, #15316 ) ;
#7167 = DIRECTION ( 'NONE',  ( -1.000000000000000000, -0.000000000000000000, -0.000000000000000000 ) ) ;
#7169 = CARTESIAN_POINT ( 'NONE',  ( 2.459674775249762302, 3.512261536898573354E-15, 1.958521724562357923E-15 ) ) ;
#7170 = DIRECTION ( 'NONE',  ( -1.000000000000000000, -0.000000000000000000, -0.000000000000000000 ) ) ;
#7171 = DIRECTION ( 'NONE',  ( -1.000000000000000000, 0.000000000000000000, 0.000000000000000000 ) ) ;
#7172 = CARTESIAN_POINT ( 'NONE',  ( -93.84685191531252713, 88.00268892867056536, 77.78947916753381264 ) ) ;
#7173 = LINE ( 'NONE', #54149, #38278 ) ;
#7174 = CARTESIAN_POINT ( 'NONE',  ( 97.64999999999999147, 90.00000000000002842, 76.34749999999999659 ) ) ;
#7175 = DIRECTION ( 'NONE',  ( -0.000000000000000000, -0.000000000000000000, 1.000000000000000000 ) ) ;
#7176 = CIRCLE ( 'NONE', #62471, 31.99999999999998579 ) ;
#7177 = CARTESIAN_POINT ( 'NONE',  ( 10.00000000000000000, 30.41916302227113178, 71.27951684758036777 ) ) ;
#7179 = CARTESIAN_POINT ( 'NONE',  ( 2.949999999999999734, 3.061616997868382648E-16, -2.499999999999999556 ) ) ;
#7178 = CIRCLE ( 'NONE', #68421, 82.00000000000000000 ) ;
#7180 = DIRECTION ( 'NONE',  ( 0.000000000000000000, 0.000000000000000000, 1.000000000000000000 ) ) ;
#7181 = CARTESIAN_POINT ( 'NONE',  ( -10.00000000000000000, 0.000000000000000000, 0.000000000000000000 ) ) ;
#7182 = DIRECTION ( 'NONE',  ( 1.000000000000000000, -0.000000000000000000, -0.000000000000000000 ) ) ;
#7183 = CARTESIAN_POINT ( 'NONE',  ( -92.69370383062498320, -208.6684592857803011, 74.93197916753381094 ) ) ;
#7184 = AXIS2_PLACEMENT_3D ( 'NONE', #22474, #23856, #56695 ) ;
#7185 = VECTOR ( 'NONE', #757, 1000.000000000000000 ) ;
#7186 = PLANE ( 'NONE',  #48860 ) ;
#7187 = ORIENTED_EDGE ( 'NONE', *, *, #53215, .T. ) ;
#7188 = DIRECTION ( 'NONE',  ( -1.000000000000000000, 0.000000000000000000, 0.000000000000000000 ) ) ;
#7189 = CARTESIAN_POINT ( 'NONE',  ( 6.250000000000005329, 3.673940397442060854E-16, -3.000000000000000888 ) ) ;
#7190 = DIRECTION ( 'NONE',  ( 0.000000000000000000, 0.7071067811865437980, 0.7071067811865512365 ) ) ;
#7191 = DIRECTION ( 'NONE',  ( 0.6691306063588671194, -0.7431448254773862505, 0.000000000000000000 ) ) ;
#7192 = FACE_OUTER_BOUND ( 'NONE', #30183, .T. ) ;
#7193 = ORIENTED_EDGE ( 'NONE', *, *, #65149, .F. ) ;
#7194 = CARTESIAN_POINT ( 'NONE',  ( 0.000000000000000000, -29.01471420065507090, -76.69515212746047439 ) ) ;
#7195 = CARTESIAN_POINT ( 'NONE',  ( 114.1267819554180392, -82.91796067500511924, -5.500000000000000000 ) ) ;
#7196 = EDGE_LOOP ( 'NONE', ( #71586, #7875, #7693, #18483 ) ) ;
#7197 = VECTOR ( 'NONE', #16634, 1000.000000000000114 ) ;
#7198 = CARTESIAN_POINT ( 'NONE',  ( 96.15314808468750130, -211.9973110713294489, 83.50447916753381605 ) ) ;
#7199 = CARTESIAN_POINT ( 'NONE',  ( 93.84685191531251292, -211.9973110713294489, 88.63739583420048973 ) ) ;
#7200 = ORIENTED_EDGE ( 'NONE', *, *, #11598, .F. ) ;
#7201 = EDGE_CURVE ( 'NONE', #49855, #24962, #71465, .T. ) ;
#7202 = CARTESIAN_POINT ( 'NONE',  ( 96.15314808468750130, -211.9973110713294489, 88.74322916753382628 ) ) ;
#7203 = AXIS2_PLACEMENT_3D ( 'NONE', #27596, #44151, #49776 ) ;
#7204 = ORIENTED_EDGE ( 'NONE', *, *, #70697, .F. ) ;
#7205 = DIRECTION ( 'NONE',  ( 0.000000000000000000, 0.000000000000000000, 1.000000000000000000 ) ) ;
#7206 = ORIENTED_EDGE ( 'NONE', *, *, #25740, .T. ) ;
#7207 = CARTESIAN_POINT ( 'NONE',  ( -95.00000000000002842, 92.66308142843932671, 80.75281250086715090 ) ) ;
#7208 = EDGE_LOOP ( 'NONE', ( #56918, #29271, #51051, #8144 ) ) ;
#7209 = ADVANCED_FACE ( 'NONE', ( #36524 ), #24880, .T. ) ;
#7210 = ORIENTED_EDGE ( 'NONE', *, *, #19751, .F. ) ;
#7211 = AXIS2_PLACEMENT_3D ( 'NONE', #13163, #30812, #47388 ) ;
#7212 = CARTESIAN_POINT ( 'NONE',  ( 11.99999999999999822, 0.000000000000000000, 0.000000000000000000 ) ) ;
#7213 = VERTEX_POINT ( 'NONE', #19602 ) ;
#7214 = CARTESIAN_POINT ( 'NONE',  ( 11.99999999999999822, -76.41127070299280888, 12.93880638057290788 ) ) ;
#7215 = LINE ( 'NONE', #6125, #22456 ) ;
#7216 = EDGE_CURVE ( 'NONE', #73668, #50254, #41800, .T. ) ;
#7217 = ORIENTED_EDGE ( 'NONE', *, *, #43833, .F. ) ;
#7218 = LINE ( 'NONE', #36885, #22634 ) ;
#7219 = EDGE_LOOP ( 'NONE', ( #70030, #19350, #25331, #71093 ) ) ;
#7220 = DIRECTION ( 'NONE',  ( 0.000000000000000000, 0.000000000000000000, 1.000000000000000000 ) ) ;
#7221 = ADVANCED_FACE ( 'NONE', ( #2369 ), #13230, .F. ) ;
#7222 = ORIENTED_EDGE ( 'NONE', *, *, #57036, .F. ) ;
#7223 = AXIS2_PLACEMENT_3D ( 'NONE', #73533, #22043, #10017 ) ;
#7224 = ORIENTED_EDGE ( 'NONE', *, *, #15730, .T. ) ;
#7225 = ORIENTED_EDGE ( 'NONE', *, *, #13560, .T. ) ;
#7226 = CIRCLE ( 'NONE', #16837, 23.50000000000041922 ) ;
#7227 = CARTESIAN_POINT ( 'NONE',  ( 97.30629616937498838, -208.6684592857803011, 82.39322916753381776 ) ) ;
#7228 = AXIS2_PLACEMENT_3D ( 'NONE', #55026, #43766, #66686 ) ;
#7229 = CARTESIAN_POINT ( 'NONE',  ( -22.67106064244953245, -113.6342314410295842, 5.500000000000000000 ) ) ;
#7230 = AXIS2_PLACEMENT_3D ( 'NONE', #19717, #25374, #42663 ) ;
#7231 = SHAPE_DEFINITION_REPRESENTATION ( #15150, #27826 ) ;
#7232 = CARTESIAN_POINT ( 'NONE',  ( -92.35000000000000853, 88.47002178664756400, 82.00958333333333883 ) ) ;
#7233 = CARTESIAN_POINT ( 'NONE',  ( -97.64999999999996305, -209.9999999999999716, 78.64937500173429896 ) ) ;
#7234 = CARTESIAN_POINT ( 'NONE',  ( 92.34999999999998010, -208.4700217866475214, 79.15208333333333712 ) ) ;
#7235 = CARTESIAN_POINT ( 'NONE',  ( -96.32499999999996021, -212.2949673200287179, 75.50083333333331836 ) ) ;
#7236 = CYLINDRICAL_SURFACE ( 'NONE', #18073, 82.00000000000000000 ) ;
#7237 = CIRCLE ( 'NONE', #69644, 14.53333333333331545 ) ;
#7238 = CARTESIAN_POINT ( 'NONE',  ( 0.000000000000000000, 33.80338159004307386, -16.23288003029461279 ) ) ;
#7239 = CIRCLE ( 'NONE', #14415, 37.49900000000000944 ) ;
#7240 = CARTESIAN_POINT ( 'NONE',  ( -96.15314808468747287, -208.0026889286704943, 83.18697916753382060 ) ) ;
#7241 = ADVANCED_FACE ( 'NONE', ( #42547 ), #59105, .T. ) ;
#7242 = CARTESIAN_POINT ( 'NONE',  ( -95.00000000000002842, 87.33691857156074434, 83.61031250086716682 ) ) ;
#7243 = ADVANCED_FACE ( 'NONE', ( #13952 ), #59846, .F. ) ;
#7244 = VERTEX_POINT ( 'NONE', #65852 ) ;
#7245 = CARTESIAN_POINT ( 'NONE',  ( 92.69370383062498320, 88.66845928578037217, 80.80572916753382628 ) ) ;
#7246 = ORIENTED_EDGE ( 'NONE', *, *, #40752, .F. ) ;
#7247 = DIRECTION ( 'NONE',  ( 0.000000000000000000, 0.000000000000000000, -1.000000000000000000 ) ) ;
#7248 = FACE_OUTER_BOUND ( 'NONE', #34337, .T. ) ;
#7249 = LINE ( 'NONE', #63290, #13371 ) ;
#7250 = DIRECTION ( 'NONE',  ( -1.000000000000000000, 0.000000000000000000, 0.000000000000000000 ) ) ;
#7251 = CARTESIAN_POINT ( 'NONE',  ( 10.00000000000000000, 35.91791733033475253, 68.67312586195009771 ) ) ;
#7252 = CARTESIAN_POINT ( 'NONE',  ( -93.84685191531247028, -211.9973110713294489, 85.40947916753380298 ) ) ;
#7253 = DIRECTION ( 'NONE',  ( -1.000000000000000000, -0.000000000000000000, -0.000000000000000000 ) ) ;
#7254 = CARTESIAN_POINT ( 'NONE',  ( 22.75000000000000000, 0.000000000000000000, 0.000000000000000000 ) ) ;
#7255 = CARTESIAN_POINT ( 'NONE',  ( 11.99999999999999822, 46.53671651294032330, -59.03961581697353012 ) ) ;
#7256 = CARTESIAN_POINT ( 'NONE',  ( 11.99999999999999822, -62.50329211542407393, -41.76937507738853839 ) ) ;
#7257 = VERTEX_POINT ( 'NONE', #60227 ) ;
#7258 = ADVANCED_FACE ( 'NONE', ( #14340 ), #43308, .F. ) ;
#7259 = EDGE_CURVE ( 'NONE', #28369, #26699, #58065, .T. ) ;
#7260 = EDGE_LOOP ( 'NONE', ( #38681, #28136, #67593, #54277 ) ) ;
#7261 = LINE ( 'NONE', #70763, #68691 ) ;
#7262 = DIRECTION ( 'NONE',  ( 1.000000000000000000, 0.000000000000000000, 0.000000000000000000 ) ) ;
#7263 = CARTESIAN_POINT ( 'NONE',  ( -96.15314808468752972, 91.99731107132950569, 89.53697916753381492 ) ) ;
#7264 = CARTESIAN_POINT ( 'NONE',  ( 0.000000000000000000, -65.64334221924939072, 41.19522573413710376 ) ) ;
#7265 = CARTESIAN_POINT ( 'NONE',  ( 97.64999999999993463, 91.52997821335253548, 76.40041666666667197 ) ) ;
#7266 = CARTESIAN_POINT ( 'NONE',  ( 10.00000000000000000, 0.000000000000000000, 0.000000000000000000 ) ) ;
#7267 = CARTESIAN_POINT ( 'NONE',  ( 11.99999999999999822, 0.000000000000000000, 0.000000000000000000 ) ) ;
#7268 = ORIENTED_EDGE ( 'NONE', *, *, #23172, .T. ) ;
#7269 = CYLINDRICAL_SURFACE ( 'NONE', #22448, 77.49899999999999523 ) ;
#7270 = VECTOR ( 'NONE', #31289, 1000.000000000000000 ) ;
#7271 = VECTOR ( 'NONE', #62294, 1000.000000000000000 ) ;
#7272 = CARTESIAN_POINT ( 'NONE',  ( 11.99999999999999822, 74.65491531819118620, 23.16904090965732621 ) ) ;
#7273 = CARTESIAN_POINT ( 'NONE',  ( -12.49999999999999645, 0.000000000000000000, 125.0000000000000000 ) ) ;
#7274 = CARTESIAN_POINT ( 'NONE',  ( 92.35000000019411459, -210.0000198431783929, 84.36502760998391182 ) ) ;
#7275 = AXIS2_PLACEMENT_3D ( 'NONE', #54031, #14534, #49488 ) ;
#7276 = DIRECTION ( 'NONE',  ( 0.000000000000000000, -0.9135454576426005335, -0.4067366430758010409 ) ) ;
#7277 = CARTESIAN_POINT ( 'NONE',  ( -92.69370383062498320, -209.9999999999999716, 86.30906250086715659 ) ) ;
#7278 = DIRECTION ( 'NONE',  ( 0.000000000000000000, 0.000000000000000000, 1.000000000000000000 ) ) ;
#7279 = CYLINDRICAL_SURFACE ( 'NONE', #49032, 82.00000000000000000 ) ;
#7280 = EDGE_CURVE ( 'NONE', #44409, #59589, #57838, .T. ) ;
#7281 = CARTESIAN_POINT ( 'NONE',  ( -92.69370383062496899, -210.9303121318039871, 74.84209103131394158 ) ) ;
#7282 = DIRECTION ( 'NONE',  ( 0.000000000000000000, 0.000000000000000000, 1.000000000000000000 ) ) ;
#7283 = AXIS2_PLACEMENT_3D ( 'NONE', #60970, #33494, #43696 ) ;
#7284 = VERTEX_POINT ( 'NONE', #73996 ) ;
#7285 = DIRECTION ( 'NONE',  ( -1.000000000000000000, 0.000000000000000000, -0.000000000000000000 ) ) ;
#7286 = CARTESIAN_POINT ( 'NONE',  ( 94.99999999999998579, 93.05995642670504253, 75.87125000000000341 ) ) ;
#7287 = CARTESIAN_POINT ( 'NONE',  ( -92.35000000005469190, 89.99998298270445218, 88.49187441316097136 ) ) ;
#7288 = VECTOR ( 'NONE', #6416, 1000.000000000000114 ) ;
#7289 = VECTOR ( 'NONE', #46261, 1000.000000000000000 ) ;
#7290 = EDGE_CURVE ( 'NONE', #30489, #63633, #66157, .T. ) ;
#7291 = VECTOR ( 'NONE', #10130, 1000.000000000000000 ) ;
#7292 = CARTESIAN_POINT ( 'NONE',  ( 0.000000000000000000, -70.53064760720297954, -26.01480285779911839 ) ) ;
#7293 = CARTESIAN_POINT ( 'NONE',  ( 93.84685191531249870, -208.0026889286704943, 75.56697916753381605 ) ) ;
#7294 = ORIENTED_EDGE ( 'NONE', *, *, #21569, .T. ) ;
#7295 = EDGE_CURVE ( 'NONE', #64863, #59272, #35263, .T. ) ;
#7296 = DIRECTION ( 'NONE',  ( -1.000000000000000000, 0.000000000000000000, -0.000000000000000000 ) ) ;
#7297 = ORIENTED_EDGE ( 'NONE', *, *, #71036, .F. ) ;
#7298 =( BOUNDED_CURVE ( )  B_SPLINE_CURVE ( 2, ( #8283, #3048, #24833, #71419, #20300, #19557, #42502 ),
 .UNSPECIFIED., .F., .F. ) 
 B_SPLINE_CURVE_WITH_KNOTS ( ( 3, 2, 2, 3 ),
 ( 0.9101937466091534201, 0.9172495203147085219, 0.9243052858555914630, 0.9313609857393204683 ),
 .UNSPECIFIED. ) 
 CURVE ( )  GEOMETRIC_REPRESENTATION_ITEM ( )  RATIONAL_B_SPLINE_CURVE ( ( 1.000000000000000000, 0.8660254037844387076, 1.000000000000000000, 0.8660254037844387076, 1.000000000000000000, 0.8660266504798714848, 0.9999975066323365525 ) ) 
 REPRESENTATION_ITEM ( '' )  );
#7299 = CARTESIAN_POINT ( 'NONE',  ( 10.00000000000000000, -17.28742895386031719, -75.54627589209962935 ) ) ;
#7300 = ORIENTED_EDGE ( 'NONE', *, *, #67968, .T. ) ;
#7301 = ADVANCED_FACE ( 'NONE', ( #22510 ), #45076, .T. ) ;
#7302 = CYLINDRICAL_SURFACE ( 'NONE', #57413, 77.49899999999999523 ) ;
#7303 = ORIENTED_EDGE ( 'NONE', *, *, #6397, .T. ) ;
#7304 = ORIENTED_EDGE ( 'NONE', *, *, #26905, .T. ) ;
#7305 = VERTEX_POINT ( 'NONE', #17603 ) ;
#7306 = DIRECTION ( 'NONE',  ( -1.000000000000000000, 3.552713678800500929E-15, 0.000000000000000000 ) ) ;
#7307 = ORIENTED_EDGE ( 'NONE', *, *, #3695, .T. ) ;
#7308 = VERTEX_POINT ( 'NONE', #67998 ) ;
#7309 = CARTESIAN_POINT ( 'NONE',  ( 94.99999999999998579, 87.33691857156068750, 80.43531250086715545 ) ) ;
#7310 = CARTESIAN_POINT ( 'NONE',  ( 11.99999999999999822, -15.33399622253425321, -80.55351364060605590 ) ) ;
#7311 = EDGE_CURVE ( 'NONE', #31915, #45341, #39804, .T. ) ;
#7312 = CARTESIAN_POINT ( 'NONE',  ( 96.32499999999998863, -212.2949673200287179, 75.60666666666665492 ) ) ;
#7313 = ORIENTED_EDGE ( 'NONE', *, *, #56458, .F. ) ;
#7314 = ORIENTED_EDGE ( 'NONE', *, *, #40834, .T. ) ;
#7315 = VECTOR ( 'NONE', #52856, 1000.000000000000000 ) ;
#7316 = CIRCLE ( 'NONE', #64964, 82.00000000000000000 ) ;
#7317 = EDGE_LOOP ( 'NONE', ( #70092, #57940, #29661, #57874 ) ) ;
#7318 = CARTESIAN_POINT ( 'NONE',  ( 0.000000000000000000, 39.04073710021344112, 15.48615015657596672 ) ) ;
#7319 = AXIS2_PLACEMENT_3D ( 'NONE', #38510, #39629, #4319 ) ;
#7320 = VERTEX_POINT ( 'NONE', #68385 ) ;
#7321 = DIRECTION ( 'NONE',  ( 1.000000000000000000, 0.000000000000000000, 0.000000000000000000 ) ) ;
#7322 = DIRECTION ( 'NONE',  ( 0.000000000000000000, 0.3826834323650841752, 0.9238795325112891810 ) ) ;
#7323 = DIRECTION ( 'NONE',  ( 0.000000000000000000, 1.000000000000000000, 0.000000000000000000 ) ) ;
#7324 = FACE_OUTER_BOUND ( 'NONE', #39487, .T. ) ;
#7325 = CARTESIAN_POINT ( 'NONE',  ( 92.35000000003287823, -209.9999916080746516, 86.90410584365268676 ) ) ;
#7326 = CARTESIAN_POINT ( 'NONE',  ( 0.000000000000000000, -73.73191006444561424, -14.66109333815538918 ) ) ;
#7327 = CARTESIAN_POINT ( 'NONE',  ( 0.000000000000000000, -6.736453364083290651, -36.88895765772640090 ) ) ;
#7328 = CARTESIAN_POINT ( 'NONE',  ( -94.99999999999997158, -206.9400435732949575, 80.39562500173431658 ) ) ;
#7329 = ADVANCED_FACE ( 'NONE', ( #5979 ), #10855, .F. ) ;
#7330 = CARTESIAN_POINT ( 'NONE',  ( 4.348517481000897078, -143.0941636721797465, -2.500000000000000000 ) ) ;
#7331 = EDGE_CURVE ( 'NONE', #58186, #73677, #73621, .T. ) ;
#7332 = ORIENTED_EDGE ( 'NONE', *, *, #36488, .T. ) ;
#7334 = CARTESIAN_POINT ( 'NONE',  ( -96.32500000000001705, 87.70503267997129626, 77.48520833506763950 ) ) ;
#7333 = CARTESIAN_POINT ( 'NONE',  ( 93.67499999999998295, 92.29496732002878900, 77.27354166840096639 ) ) ;
#7336 = EDGE_CURVE ( 'NONE', #6388, #32813, #66499, .T. ) ;
#7335 = VERTEX_POINT ( 'NONE', #33783 ) ;
#7337 = CARTESIAN_POINT ( 'NONE',  ( 94.99999999999998579, 92.66308142843935514, 80.11781250086714579 ) ) ;
#7338 = CARTESIAN_POINT ( 'NONE',  ( 0.000000000000000000, -59.75363087400035056, -56.15606465355020305 ) ) ;
#7339 = DIRECTION ( 'NONE',  ( 0.9997280174009348652, -0.02332147558787931590, 0.000000000000000000 ) ) ;
#7340 = CARTESIAN_POINT ( 'NONE',  ( 10.00000000000000000, 37.22597642581158084, -5.202137450156524068 ) ) ;
#7341 = PLANE ( 'NONE',  #55403 ) ;
#7342 = AXIS2_PLACEMENT_3D ( 'NONE', #18794, #12787, #60164 ) ;
#7343 = CARTESIAN_POINT ( 'NONE',  ( 0.000000000000000000, -75.54627589209955829, 17.28742895386058009 ) ) ;
#7344 = ORIENTED_EDGE ( 'NONE', *, *, #3250, .F. ) ;
#7345 = CYLINDRICAL_SURFACE ( 'NONE', #67324, 77.49899999999999523 ) ;
#7346 = VECTOR ( 'NONE', #67906, 1000.000000000000114 ) ;
#7347 = CARTESIAN_POINT ( 'NONE',  ( 1.301042606982605321E-15, 5.773502691896264416, -5.553418012614792509 ) ) ;
#7348 = VERTEX_POINT ( 'NONE', #4871 ) ;
#7349 = CIRCLE ( 'NONE', #49345, 31.99999999999998579 ) ;
#7350 = ORIENTED_EDGE ( 'NONE', *, *, #36099, .F. ) ;
#7351 = VECTOR ( 'NONE', #22916, 1000.000000000000000 ) ;
#7352 = FACE_BOUND ( 'NONE', #46868, .T. ) ;
#7353 = DIRECTION ( 'NONE',  ( 1.000000000000000000, -0.000000000000000000, -0.000000000000000000 ) ) ;
#7354 = DIRECTION ( 'NONE',  ( 0.000000000000000000, 0.2334453638559058908, -0.9723699203976764460 ) ) ;
#7355 = CARTESIAN_POINT ( 'NONE',  ( 10.00000000000000000, 16.23288003029497162, 33.80338159004289622 ) ) ;
#7356 = CARTESIAN_POINT ( 'NONE',  ( -94.99999999999997158, -212.6630814284392557, 77.89531250086714920 ) ) ;
#7357 = ORIENTED_EDGE ( 'NONE', *, *, #59523, .T. ) ;
#7358 = CARTESIAN_POINT ( 'NONE',  ( -95.00000000000002842, 90.00000000000004263, 90.00000000000000000 ) ) ;
#7359 = CARTESIAN_POINT ( 'NONE',  ( 92.34999999999999432, 90.00000000000002842, 77.29999999999999716 ) ) ;
#7360 = CARTESIAN_POINT ( 'NONE',  ( 92.35000000049295465, 89.99996796756887818, 85.63541623677173220 ) ) ;
#7361 = FACE_OUTER_BOUND ( 'NONE', #66051, .T. ) ;
#7362 = DIRECTION ( 'NONE',  ( 0.000000000000000000, 0.000000000000000000, -1.000000000000000000 ) ) ;
#7363 = CARTESIAN_POINT ( 'NONE',  ( 0.000000000000000000, 0.000000000000000000, 42.00000000000001421 ) ) ;
#7364 = DIRECTION ( 'NONE',  ( -1.000000000000000000, 0.000000000000000000, -0.000000000000000000 ) ) ;
#7365 = DIRECTION ( 'NONE',  ( -0.000000000000000000, -0.000000000000000000, 1.000000000000000000 ) ) ;
#7366 = CARTESIAN_POINT ( 'NONE',  ( 10.00000000000000000, 26.02418014898407961, -70.52718814184231633 ) ) ;
#7367 = CARTESIAN_POINT ( 'NONE',  ( 11.99999999999999822, 68.26794271651262136, 31.47745569255165066 ) ) ;
#7368 = CARTESIAN_POINT ( 'NONE',  ( 94.99999999999998579, 87.33691857156068750, 84.88031250086713442 ) ) ;
#7369 = CARTESIAN_POINT ( 'NONE',  ( -94.99999999999997158, -207.3369185715606307, 87.73781250086715033 ) ) ;
#7370 = DIRECTION ( 'NONE',  ( -0.8541291221503266584, 0.5200609990133008287, 0.000000000000000000 ) ) ;
#7371 = VERTEX_POINT ( 'NONE', #63479 ) ;
#7372 =( GEOMETRIC_REPRESENTATION_CONTEXT ( 3 ) GLOBAL_UNCERTAINTY_ASSIGNED_CONTEXT ( ( #66335 ) ) GLOBAL_UNIT_ASSIGNED_CONTEXT ( ( #47497, #41124, #23821 ) ) REPRESENTATION_CONTEXT ( 'NONE', 'WORKASPACE' ) );
#7373 = DIRECTION ( 'NONE',  ( 0.000000000000000000, 0.9723699203976756689, 0.2334453638559094157 ) ) ;
#7374 = CARTESIAN_POINT ( 'NONE',  ( -96.32499999999996021, -212.2949673200287179, 81.21583333333333599 ) ) ;
#7375 = DIRECTION ( 'NONE',  ( -1.000000000000000000, 0.000000000000000000, 0.000000000000000000 ) ) ;
#7376 = AXIS2_PLACEMENT_3D ( 'NONE', #68012, #40931, #22906 ) ;
#7377 = AXIS2_PLACEMENT_3D ( 'NONE', #2028, #26394, #66263 ) ;
#7378 = EDGE_CURVE ( 'NONE', #61574, #5475, #43702, .T. ) ;
#7379 = CARTESIAN_POINT ( 'NONE',  ( 96.15314808468750130, -211.9973110713294489, 87.31447916753380412 ) ) ;
#7380 = ORIENTED_EDGE ( 'NONE', *, *, #48377, .F. ) ;
#7381 = EDGE_CURVE ( 'NONE', #50810, #28846, #34080, .T. ) ;
#7382 = VECTOR ( 'NONE', #70925, 1000.000000000000000 ) ;
#7383 = ORIENTED_EDGE ( 'NONE', *, *, #50570, .F. ) ;
#7384 = ORIENTED_EDGE ( 'NONE', *, *, #31300, .F. ) ;
#7385 = EDGE_CURVE ( 'NONE', #14108, #68714, #30465, .T. ) ;
#7386 = EDGE_CURVE ( 'NONE', #33091, #15908, #10370, .T. ) ;
#7387 = VECTOR ( 'NONE', #2015, 1000.000000000000000 ) ;
#7388 = CARTESIAN_POINT ( 'NONE',  ( 11.99999999999999822, -70.52718814184277107, 26.02418014898285037 ) ) ;
#7389 = CARTESIAN_POINT ( 'NONE',  ( 11.99999999999999822, -68.67312586194971402, -35.91791733033549860 ) ) ;
#7390 = ORIENTED_EDGE ( 'NONE', *, *, #37935, .T. ) ;
#7391 = CIRCLE ( 'NONE', #33797, 16.00000000000000355 ) ;
#7392 = VERTEX_POINT ( 'NONE', #17238 ) ;
#7393 = DIRECTION ( 'NONE',  ( 1.000000000000000000, 0.000000000000000000, 0.000000000000000000 ) ) ;
#7394 = CARTESIAN_POINT ( 'NONE',  ( 92.69370383062501162, -209.9999999999999716, 81.54656250086715374 ) ) ;
#7395 = CARTESIAN_POINT ( 'NONE',  ( 0.000000000000000000, 0.000000000000000000, 4.700000000000000178 ) ) ;
#7396 = DIRECTION ( 'NONE',  ( 1.000000000000000000, 0.000000000000000000, 0.000000000000000000 ) ) ;
#7397 = DIRECTION ( 'NONE',  ( 0.000000000000000000, -0.8660254037844363761, -0.5000000000000039968 ) ) ;
#7398 = LINE ( 'NONE', #20521, #53114 ) ;
#7399 = ADVANCED_FACE ( 'NONE', ( #34898 ), #40170, .T. ) ;
#7400 = DIRECTION ( 'NONE',  ( 0.000000000000000000, 0.8526401643540897357, 0.5224985647159527957 ) ) ;
#7401 = CARTESIAN_POINT ( 'NONE',  ( 97.64999999999997726, -211.5299782133524502, 86.45458333333333201 ) ) ;
#7402 = ORIENTED_EDGE ( 'NONE', *, *, #64604, .T. ) ;
#7403 = ORIENTED_EDGE ( 'NONE', *, *, #16049, .T. ) ;
#7404 = ORIENTED_EDGE ( 'NONE', *, *, #4948, .F. ) ;
#7405 = ORIENTED_EDGE ( 'NONE', *, *, #34886, .T. ) ;
#7406 = PRESENTATION_STYLE_ASSIGNMENT (( #35962 ) ) ;
#7407 = CARTESIAN_POINT ( 'NONE',  ( -96.15314808468752972, 91.99731107132950569, 86.52072916753382970 ) ) ;
#7408 = DIRECTION ( 'NONE',  ( -1.000000000000000000, 0.000000000000000000, -0.000000000000000000 ) ) ;
#7409 = FACE_OUTER_BOUND ( 'NONE', #16121, .T. ) ;
#7410 = CARTESIAN_POINT ( 'NONE',  ( 97.30629616937498838, -209.9999999999999716, 87.42031250086714067 ) ) ;
#7411 = CARTESIAN_POINT ( 'NONE',  ( 92.34999999999999432, 91.52997821335252127, 77.24708333333332178 ) ) ;
#7412 = EDGE_LOOP ( 'NONE', ( #69840, #40993, #1827, #3512 ) ) ;
#7413 = CARTESIAN_POINT ( 'NONE',  ( -92.34999999999999432, -211.5299782133524502, 87.80395833506763381 ) ) ;
#7415 = ORIENTED_EDGE ( 'NONE', *, *, #4032, .F. ) ;
#7414 = EDGE_CURVE ( 'NONE', #49091, #67107, #23299, .T. ) ;
#7416 = ADVANCED_FACE ( 'NONE', ( #35264 ), #18700, .F. ) ;
#7417 = CARTESIAN_POINT ( 'NONE',  ( -97.64999999990727986, 90.00001381026693537, 80.55392363656929433 ) ) ;
#7418 = EDGE_CURVE ( 'NONE', #71534, #62834, #24524, .T. ) ;
#7419 = VERTEX_POINT ( 'NONE', #29984 ) ;
#7420 = CARTESIAN_POINT ( 'NONE',  ( -97.65000000000001990, 90.00000000000004263, 87.53937500173429953 ) ) ;
#7421 = CARTESIAN_POINT ( 'NONE',  ( 92.69370383062498320, 91.33154071421968467, 89.74864583420048803 ) ) ;
#7422 = EDGE_LOOP ( 'NONE', ( #49213, #71459, #35668, #9922 ) ) ;
#7423 = LINE ( 'NONE', #29224, #30936 ) ;
#7424 = DIRECTION ( 'NONE',  ( 0.000000000000000000, -0.07845909572785234043, 0.9969173337331274087 ) ) ;
#7425 = DIRECTION ( 'NONE',  ( -0.000000000000000000, -0.000000000000000000, -1.000000000000000000 ) ) ;
#7426 = PRESENTATION_LAYER_ASSIGNMENT (  '', '', ( #35052 ) ) ;
#7427 = AXIS2_PLACEMENT_3D ( 'NONE', #42846, #30437, #42117 ) ;
#7428 = CARTESIAN_POINT ( 'NONE',  ( -94.99999999999997158, -206.9400435732949575, 86.11062500173430578 ) ) ;
#7429 = VERTEX_POINT ( 'NONE', #48026 ) ;
#7430 = LINE ( 'NONE', #70185, #35120 ) ;
#7431 = CARTESIAN_POINT ( 'NONE',  ( -92.69370383062498320, -208.6684592857803011, 75.40822916753381833 ) ) ;
#7432 = VERTEX_POINT ( 'NONE', #58557 ) ;
#7433 = ORIENTED_EDGE ( 'NONE', *, *, #23785, .T. ) ;
#7434 = CARTESIAN_POINT ( 'NONE',  ( 10.00000000000000000, 65.59268652807263322, -36.72794159290169347 ) ) ;
#7435 = AXIS2_PLACEMENT_3D ( 'NONE', #8067, #14816, #37763 ) ;
#7436 = DIRECTION ( 'NONE',  ( -1.000000000000000000, -0.000000000000000000, -0.000000000000000000 ) ) ;
#7437 = CARTESIAN_POINT ( 'NONE',  ( 0.000000000000000000, -74.65374052328654386, 8.840884882374837161 ) ) ;
#7438 = CARTESIAN_POINT ( 'NONE',  ( -92.69370383062498320, -211.3315407142195852, 86.89114583420050053 ) ) ;
#7439 = VERTEX_POINT ( 'NONE', #52541 ) ;
#7440 = VERTEX_POINT ( 'NONE', #13060 ) ;
#7441 = ORIENTED_EDGE ( 'NONE', *, *, #42983, .F. ) ;
#7442 = DIRECTION ( 'NONE',  ( 0.000000000000000000, 0.8526401643540897357, 0.5224985647159527957 ) ) ;
#7443 = AXIS2_PLACEMENT_3D ( 'NONE', #38948, #51326, #50964 ) ;
#7444 = DIRECTION ( 'NONE',  ( 0.000000000000000000, 0.000000000000000000, 1.000000000000000000 ) ) ;
#7445 = FACE_OUTER_BOUND ( 'NONE', #18948, .T. ) ;
#7446 = CARTESIAN_POINT ( 'NONE',  ( 92.69370383062498320, 88.66845928578035796, 80.80572916753379786 ) ) ;
#7447 = FACE_OUTER_BOUND ( 'NONE', #56263, .T. ) ;
#7448 = DIRECTION ( 'NONE',  ( 1.000000000000000000, 0.000000000000000000, 0.000000000000000000 ) ) ;
#7449 = DIRECTION ( 'NONE',  ( 1.000000000000000000, -3.061616997868382648E-16, -0.000000000000000000 ) ) ;
#7450 = PLANE ( 'NONE',  #49602 ) ;
#7451 = DIRECTION ( 'NONE',  ( -1.000000000000000000, -0.000000000000000000, -0.000000000000000000 ) ) ;
#7452 = DIRECTION ( 'NONE',  ( -1.000000000000000000, -0.000000000000000000, -0.000000000000000000 ) ) ;
#7453 = CYLINDRICAL_SURFACE ( 'NONE', #68721, 2.649999999999985700 ) ;
#7454 = EDGE_CURVE ( 'NONE', #45911, #54824, #40915, .T. ) ;
#7455 = CARTESIAN_POINT ( 'NONE',  ( 0.000000000000000000, 78.73519480814955784, 22.90783923731656557 ) ) ;
#7456 = EDGE_CURVE ( 'NONE', #1351, #26686, #58945, .T. ) ;
#7457 = CARTESIAN_POINT ( 'NONE',  ( 11.99999999999999822, -68.27212725128254078, -31.46837873495049465 ) ) ;
#7458 = CARTESIAN_POINT ( 'NONE',  ( -95.00000000000002842, 87.33691857156074434, 85.99156250086714692 ) ) ;
#7459 = CARTESIAN_POINT ( 'NONE',  ( 26.49955575014745079, 0.001194404164630089764, -80.00000000000000000 ) ) ;
#7460 = EDGE_CURVE ( 'NONE', #61671, #26809, #62981, .T. ) ;
#7461 = ADVANCED_FACE ( 'NONE', ( #46545 ), #58191, .T. ) ;
#7462 = LINE ( 'NONE', #30376, #72064 ) ;
#7463 = PRODUCT_DEFINITION_SHAPE ( 'NONE', 'NONE',  #74362 ) ;
#7464 = ORIENTED_EDGE ( 'NONE', *, *, #752, .F. ) ;
#7465 = CARTESIAN_POINT ( 'NONE',  ( 11.99999999999999822, -62.20884554313985149, -46.21855187248698371 ) ) ;
#7466 = CARTESIAN_POINT ( 'NONE',  ( 3.469446951953614189E-15, 12.79999999999999893, 0.000000000000000000 ) ) ;
#7467 = DIRECTION ( 'NONE',  ( -1.000000000000000000, 0.000000000000000000, 0.000000000000000000 ) ) ;
#7468 = EDGE_CURVE ( 'NONE', #56318, #9063, #47331, .T. ) ;
#7469 = CIRCLE ( 'NONE', #49487, 42.00000000000000000 ) ;
#7470 = CARTESIAN_POINT ( 'NONE',  ( -10.00000000000000000, 0.000000000000000000, 0.000000000000000000 ) ) ;
#7471 = CARTESIAN_POINT ( 'NONE',  ( 92.69370383062501162, -208.6684592857803011, 82.12864583420048348 ) ) ;
#7472 = CIRCLE ( 'NONE', #66300, 31.99999999999998579 ) ;
#7473 = EDGE_LOOP ( 'NONE', ( #72656, #46595, #46048, #10734 ) ) ;
#7474 = VERTEX_POINT ( 'NONE', #7055 ) ;
#7475 = AXIS2_PLACEMENT_3D ( 'NONE', #72341, #15195, #53955 ) ;
#7476 = CARTESIAN_POINT ( 'NONE',  ( 10.00000000000000000, 35.95386929396256903, -10.96151621346501237 ) ) ;
#7477 = ORIENTED_EDGE ( 'NONE', *, *, #67667, .T. ) ;
#7478 = EDGE_CURVE ( 'NONE', #8315, #32534, #31089, .T. ) ;
#7479 = LINE ( 'NONE', #42070, #16142 ) ;
#7480 = AXIS2_PLACEMENT_3D ( 'NONE', #40524, #57089, #69464 ) ;
#7481 = LINE ( 'NONE', #41684, #18410 ) ;
#7483 = VERTEX_POINT ( 'NONE', #23993 ) ;
#7482 = ADVANCED_FACE ( 'NONE', ( #29600 ), #35312, .T. ) ;
#7484 = CARTESIAN_POINT ( 'NONE',  ( 97.30629616937498838, -209.9999999999999716, 80.59406250086715318 ) ) ;
#7485 = ORIENTED_EDGE ( 'NONE', *, *, #46101, .F. ) ;
#7486 = FACE_OUTER_BOUND ( 'NONE', #35227, .T. ) ;
#7487 = VERTEX_POINT ( 'NONE', #65326 ) ;
#7488 = AXIS2_PLACEMENT_3D ( 'NONE', #42669, #30266, #53209 ) ;
#7489 = EDGE_CURVE ( 'NONE', #13137, #46053, #50924, .T. ) ;
#7490 = ORIENTED_EDGE ( 'NONE', *, *, #40224, .F. ) ;
#7491 = CARTESIAN_POINT ( 'NONE',  ( 92.35001072511524001, -208.4700155944993014, 86.85145790673756494 ) ) ;
#7492 = AXIS2_PLACEMENT_3D ( 'NONE', #56989, #34406, #16381 ) ;
#7493 = CARTESIAN_POINT ( 'NONE',  ( 11.99999999999999822, -62.50884508063395373, -41.76106447765554464 ) ) ;
#7494 = ORIENTED_EDGE ( 'NONE', *, *, #12997, .T. ) ;
#7495 = CARTESIAN_POINT ( 'NONE',  ( 10.00000000000000000, 29.81001611431041098, -22.74946021919100403 ) ) ;
#7496 = CARTESIAN_POINT ( 'NONE',  ( 96.32499999999998863, -212.2949673200287179, 85.21104166840096639 ) ) ;
#7497 = CARTESIAN_POINT ( 'NONE',  ( 93.67499999999998295, 92.29496732002878900, 88.62416666666665321 ) ) ;
#7498 = ORIENTED_EDGE ( 'NONE', *, *, #53702, .F. ) ;
#7499 = CARTESIAN_POINT ( 'NONE',  ( 6.000000000000000000, -81.34940948281328588, -10.30890764327469000 ) ) ;
#7500 = ADVANCED_FACE ( 'NONE', ( #64956 ), #52926, .F. ) ;
#7501 = CYLINDRICAL_SURFACE ( 'NONE', #8096, 42.00000000000000000 ) ;
#7502 = VERTEX_POINT ( 'NONE', #47290 ) ;
#7503 = EDGE_LOOP ( 'NONE', ( #53823, #1874, #37109, #39941 ) ) ;
#7504 = CARTESIAN_POINT ( 'NONE',  ( -97.30629616937501680, 88.66845928578038638, 86.67947916753382742 ) ) ;
#7505 = CARTESIAN_POINT ( 'NONE',  ( 94.99999999999998579, 92.66308142843935514, 84.40406250086712703 ) ) ;
#7506 = ORIENTED_EDGE ( 'NONE', *, *, #39463, .T. ) ;
#7507 = CARTESIAN_POINT ( 'NONE',  ( 92.34999999999999432, 88.47002178664753558, 84.41729166840097776 ) ) ;
#7508 = EDGE_CURVE ( 'NONE', #18650, #39686, #36363, .T. ) ;
#7509 = B_SPLINE_CURVE_WITH_KNOTS ( 'NONE', 1,
 ( #16012, #10374 ),
 .UNSPECIFIED., .F., .F.,
 ( 2, 2 ),
 ( 0.000000000000000000, 1.000000000000000000 ),
 .UNSPECIFIED. ) ;
#7510 = ORIENTED_EDGE ( 'NONE', *, *, #72462, .F. ) ;
#7511 = FACE_BOUND ( 'NONE', #59973, .T. ) ;
#7512 = DIRECTION ( 'NONE',  ( 0.000000000000000000, 0.8660254037844374864, -0.5000000000000019984 ) ) ;
#7513 = ORIENTED_EDGE ( 'NONE', *, *, #67295, .T. ) ;
#7514 = ORIENTED_EDGE ( 'NONE', *, *, #9602, .F. ) ;
#7515 = ORIENTED_EDGE ( 'NONE', *, *, #38555, .T. ) ;
#7516 = CARTESIAN_POINT ( 'NONE',  ( -99.99999999999998579, -116.0000000000000000, -40.00000000000002132 ) ) ;
#7517 = DIRECTION ( 'NONE',  ( 1.000000000000000000, 0.000000000000000000, 0.000000000000000000 ) ) ;
#7518 = CARTESIAN_POINT ( 'NONE',  ( -92.35000000000005116, 88.47002178664754979, 85.81958333333331268 ) ) ;
#7519 = ORIENTED_EDGE ( 'NONE', *, *, #6774, .T. ) ;
#7520 = DIRECTION ( 'NONE',  ( 1.000000000000000000, -0.000000000000000000, -0.000000000000000000 ) ) ;
#7521 = CARTESIAN_POINT ( 'NONE',  ( 0.000000000000000000, -73.95703589263990807, 23.16143007188399139 ) ) ;
#7522 = EDGE_LOOP ( 'NONE', ( #7619, #37907 ) ) ;
#7523 =( BOUNDED_CURVE ( )  B_SPLINE_CURVE ( 2, ( #67629, #10108, #62000, #9363, #43603, #37946, #38316 ),
 .UNSPECIFIED., .F., .F. ) 
 B_SPLINE_CURVE_WITH_KNOTS ( ( 3, 2, 2, 3 ),
 ( 0.2291666666666663521, 0.2361111111111107719, 0.2430555555555551639, 0.2499999999999995837 ),
 .UNSPECIFIED. ) 
 CURVE ( )  GEOMETRIC_REPRESENTATION_ITEM ( )  RATIONAL_B_SPLINE_CURVE ( ( 1.000000000000005995, 0.8660254037844328234, 1.000000000000000000, 0.8660254037844387076, 1.000000000000000000, 0.8660254037844467012, 0.9999999999999920064 ) ) 
 REPRESENTATION_ITEM ( '' )  );
#7524 = CARTESIAN_POINT ( 'NONE',  ( 0.000000000000000000, 20.41045688087930898, -72.35160999960793049 ) ) ;
#7525 = CARTESIAN_POINT ( 'NONE',  ( -96.15314808468745866, -211.9973110713294489, 84.03364583420047040 ) ) ;
#7526 = ORIENTED_EDGE ( 'NONE', *, *, #21115, .F. ) ;
#7527 = CARTESIAN_POINT ( 'NONE',  ( 4.999999999999999112, 21.40280677340371795, 36.13751322684426270 ) ) ;
#7528 = CARTESIAN_POINT ( 'NONE',  ( 10.00000000000000000, -26.08949754953005495, -27.05870788708258701 ) ) ;
#7529 = DIRECTION ( 'NONE',  ( 1.000000000000000000, 0.000000000000000000, 0.000000000000000000 ) ) ;
#7530 = DIRECTION ( 'NONE',  ( -0.4279312458752990711, -0.9038112904824846527, 0.000000000000000000 ) ) ;
#7531 = CARTESIAN_POINT ( 'NONE',  ( 11.99999999999999822, 17.28742895386084655, 75.54627589209950145 ) ) ;
#7532 = AXIS2_PLACEMENT_3D ( 'NONE', #42642, #59948, #36252 ) ;
#7533 = CARTESIAN_POINT ( 'NONE',  ( 0.000000000000000000, 35.91791733033570466, -68.67312586194960033 ) ) ;
#7534 = CARTESIAN_POINT ( 'NONE',  ( -92.34999999999999432, -209.9999999999999716, 83.96750000000000114 ) ) ;
#7535 = CARTESIAN_POINT ( 'NONE',  ( 50.00005079999999680, 2.571758278209441661E-15, -21.00000000000000000 ) ) ;
#7536 = CARTESIAN_POINT ( 'NONE',  ( -10.00000000000000000, 0.000000000000000000, 0.000000000000000000 ) ) ;
#7537 = DIRECTION ( 'NONE',  ( 1.000000000000000000, 0.000000000000000000, 0.000000000000000000 ) ) ;
#7538 = VECTOR ( 'NONE', #64409, 1000.000000000000000 ) ;
#7539 = CARTESIAN_POINT ( 'NONE',  ( -92.69370383062502583, 91.33154071421968467, 89.53697916753382913 ) ) ;
#7540 = FACE_OUTER_BOUND ( 'NONE', #18123, .T. ) ;
#7541 = DIRECTION ( 'NONE',  ( 0.000000000000000000, 0.000000000000000000, 1.000000000000000000 ) ) ;
#7542 = CIRCLE ( 'NONE', #32735, 16.00000000000000355 ) ;
#7543 = CARTESIAN_POINT ( 'NONE',  ( -97.65000000000001990, 90.00000000000004263, 89.90078125043358170 ) ) ;
#7544 = EDGE_CURVE ( 'NONE', #36799, #5972, #43546, .T. ) ;
#7545 = CIRCLE ( 'NONE', #8729, 31.99999999999998579 ) ;
#7546 = PLANE ( 'NONE',  #36504 ) ;
#7547 = CARTESIAN_POINT ( 'NONE',  ( 15.00000000000000000, 24.81905959214260804, -9.408202855044828894 ) ) ;
#7548 = AXIS2_PLACEMENT_3D ( 'NONE', #30815, #30087, #1568 ) ;
#7549 = CARTESIAN_POINT ( 'NONE',  ( 96.32499999999998863, -212.2949673200287179, 77.51166666666665606 ) ) ;
#7550 = EDGE_CURVE ( 'NONE', #17105, #26000, #10018, .T. ) ;
#7551 = CARTESIAN_POINT ( 'NONE',  ( 0.000000000000000000, 0.000000000000000000, 0.000000000000000000 ) ) ;
#7552 = CARTESIAN_POINT ( 'NONE',  ( 10.00000000000000000, 0.000000000000000000, 0.000000000000000000 ) ) ;
#7553 = CARTESIAN_POINT ( 'NONE',  ( -97.30629616937497417, -208.6684592857803011, 75.14364583420049826 ) ) ;
#7554 = ADVANCED_FACE ( 'NONE', ( #60794 ), #60428, .F. ) ;
#7555 = ADVANCED_FACE ( 'NONE', ( #26932 ), #14917, .T. ) ;
#7556 = DIRECTION ( 'NONE',  ( 0.000000000000000000, 0.000000000000000000, -1.000000000000000000 ) ) ;
#7557 = EDGE_LOOP ( 'NONE', ( #51494, #51711, #31987, #43694 ) ) ;
#7558 = CYLINDRICAL_SURFACE ( 'NONE', #25107, 16.00000000000000000 ) ;
#7559 = CARTESIAN_POINT ( 'NONE',  ( 11.99999999999999822, -55.16347631942997509, -60.67117009219195722 ) ) ;
#7560 = CARTESIAN_POINT ( 'NONE',  ( 6.000000000000000000, -8.966570791700160470, -81.50828551894237251 ) ) ;
#7561 = CARTESIAN_POINT ( 'NONE',  ( -24.50849501662245800, -109.8101191361138831, 5.500000000000000000 ) ) ;
#7562 = EDGE_CURVE ( 'NONE', #51749, #37374, #44932, .T. ) ;
#7563 = CARTESIAN_POINT ( 'NONE',  ( 11.99999999999999822, 78.73519480814954363, 22.90783923731657268 ) ) ;
#7564 = EDGE_CURVE ( 'NONE', #5745, #9042, #43875, .T. ) ;
#7565 = ORIENTED_EDGE ( 'NONE', *, *, #35091, .T. ) ;
#7566 = DIRECTION ( 'NONE',  ( 0.000000000000000000, 0.000000000000000000, 1.000000000000000000 ) ) ;
#7567 = EDGE_LOOP ( 'NONE', ( #30297, #72474, #11493, #56517 ) ) ;
#7568 = CARTESIAN_POINT ( 'NONE',  ( 92.69370383062501162, -211.3315407142195852, 85.88572916753381037 ) ) ;
#7569 = CARTESIAN_POINT ( 'NONE',  ( 92.69370383062501162, -209.9999999999999716, 89.16656250086715829 ) ) ;
#7570 = ORIENTED_EDGE ( 'NONE', *, *, #722, .T. ) ;
#7571 = CARTESIAN_POINT ( 'NONE',  ( 97.30629616937498838, -209.9999999999999716, 88.21406250086714351 ) ) ;
#7572 = ORIENTED_EDGE ( 'NONE', *, *, #44389, .T. ) ;
#7573 = DIRECTION ( 'NONE',  ( -1.000000000000000000, -0.000000000000000000, -0.000000000000000000 ) ) ;
#7574 = ORIENTED_EDGE ( 'NONE', *, *, #26619, .T. ) ;
#7575 = EDGE_CURVE ( 'NONE', #6594, #7502, #20564, .T. ) ;
#7576 = EDGE_CURVE ( 'NONE', #25675, #7033, #55518, .T. ) ;
#7577 = CARTESIAN_POINT ( 'NONE',  ( -97.30629616937501680, 91.33154071421968467, 79.58864583420047722 ) ) ;
#7578 = ORIENTED_EDGE ( 'NONE', *, *, #10674, .T. ) ;
#7579 = VERTEX_POINT ( 'NONE', #38219 ) ;
#7580 = CARTESIAN_POINT ( 'NONE',  ( -2.499999999999970690, 73.00000000000001421, -255.0000000000000000 ) ) ;
#7581 = EDGE_LOOP ( 'NONE', ( #66657, #40869, #58158, #72769 ) ) ;
#7582 = CARTESIAN_POINT ( 'NONE',  ( 92.35001072950502987, -208.4700155919648807, 84.94645790656225870 ) ) ;
#7583 = FILL_AREA_STYLE ('',( #31607 ) ) ;
#7584 = VERTEX_POINT ( 'NONE', #55139 ) ;
#7585 = PLANE ( 'NONE',  #28630 ) ;
#7586 = EDGE_CURVE ( 'NONE', #16851, #19930, #50760, .T. ) ;
#7587 = CIRCLE ( 'NONE', #55620, 31.99999999999999289 ) ;
#7588 = ORIENTED_EDGE ( 'NONE', *, *, #52692, .F. ) ;
#7589 = AXIS2_PLACEMENT_3D ( 'NONE', #13636, #8380, #25666 ) ;
#7590 = ORIENTED_EDGE ( 'NONE', *, *, #38810, .T. ) ;
#7591 = ORIENTED_EDGE ( 'NONE', *, *, #51886, .F. ) ;
#7592 = AXIS2_PLACEMENT_3D ( 'NONE', #68395, #10488, #17251 ) ;
#7593 = ORIENTED_EDGE ( 'NONE', *, *, #11299, .T. ) ;
#7594 = CARTESIAN_POINT ( 'NONE',  ( 96.15314808468750130, -211.9973110713294489, 79.69447916753379957 ) ) ;
#7595 = AXIS2_PLACEMENT_3D ( 'NONE', #15863, #38794, #61729 ) ;
#7596 = CARTESIAN_POINT ( 'NONE',  ( 5.000000000000000000, -32.34446384429989507, 26.79245525562703278 ) ) ;
#7597 = AXIS2_PLACEMENT_3D ( 'NONE', #1484, #47306, #54056 ) ;
#7598 = LINE ( 'NONE', #2371, #24593 ) ;
#7599 = DIRECTION ( 'NONE',  ( -1.000000000000000000, 0.000000000000000000, 0.000000000000000000 ) ) ;
#7600 = DIRECTION ( 'NONE',  ( 0.000000000000000000, 0.000000000000000000, -1.000000000000000000 ) ) ;
#7601 = LINE ( 'NONE', #42929, #57191 ) ;
#7602 = FACE_OUTER_BOUND ( 'NONE', #26247, .T. ) ;
#7603 = CARTESIAN_POINT ( 'NONE',  ( 89.17737905728634473, -39.70432723693593857, 5.500000000000000000 ) ) ;
#7604 = CARTESIAN_POINT ( 'NONE',  ( -97.30629616937495996, -209.9999999999999716, 85.19781250086714408 ) ) ;
#7605 = CARTESIAN_POINT ( 'NONE',  ( -96.15314808468752972, 91.99731107132950569, 83.34572916753383254 ) ) ;
#7606 = ORIENTED_EDGE ( 'NONE', *, *, #45768, .T. ) ;
#7607 = CARTESIAN_POINT ( 'NONE',  ( 94.99999999999998579, 87.33691857156068750, 79.64156250086713840 ) ) ;
#7608 = ORIENTED_EDGE ( 'NONE', *, *, #60041, .T. ) ;
#7609 = CARTESIAN_POINT ( 'NONE',  ( -12.00000000000000000, 0.000000000000000000, 0.000000000000000000 ) ) ;
#7610 = CARTESIAN_POINT ( 'NONE',  ( 0.000000000000000000, 0.000000000000000000, 0.000000000000000000 ) ) ;
#7611 = DIRECTION ( 'NONE',  ( 0.000000000000000000, 0.5224985647159500202, -0.8526401643540915121 ) ) ;
#7612 = DIRECTION ( 'NONE',  ( 0.8191520442889917986, 0.000000000000000000, 0.5735764363510460484 ) ) ;
#7613 = CYLINDRICAL_SURFACE ( 'NONE', #14017, 31.99999999999998579 ) ;
#7614 = CARTESIAN_POINT ( 'NONE',  ( -97.30629616937497417, -208.6684592857803295, 83.23989583420048177 ) ) ;
#7615 = CARTESIAN_POINT ( 'NONE',  ( 10.00000000000000000, -37.48860685352290290, -0.8828120875904512665 ) ) ;
#7616 = PLANE ( 'NONE',  #70312 ) ;
#7617 = CARTESIAN_POINT ( 'NONE',  ( -3.000000000000000000, 5.835314593368477354, 22.81335362449854642 ) ) ;
#7618 = VERTEX_POINT ( 'NONE', #9276 ) ;
#7619 = ORIENTED_EDGE ( 'NONE', *, *, #20014, .F. ) ;
#7620 = CARTESIAN_POINT ( 'NONE',  ( -93.67500000000003979, 92.29496732002878900, 75.81833333333332803 ) ) ;
#7621 = CARTESIAN_POINT ( 'NONE',  ( -93.67500000000003979, 87.70503267997129626, 84.57604166840096127 ) ) ;
#7622 = CARTESIAN_POINT ( 'NONE',  ( 10.00000000000000000, 33.79645857604513992, -16.45098606841138178 ) ) ;
#7623 = CARTESIAN_POINT ( 'NONE',  ( -96.34407192492896854, -207.9734350352809429, 74.86703477254887673 ) ) ;
#7624 = DIRECTION ( 'NONE',  ( -1.000000000000000000, -0.000000000000000000, -0.000000000000000000 ) ) ;
#7625 = AXIS2_PLACEMENT_3D ( 'NONE', #17529, #56663, #57024 ) ;
#7626 = CYLINDRICAL_SURFACE ( 'NONE', #65010, 16.00000000000000000 ) ;
#7627 = DIRECTION ( 'NONE',  ( -0.000000000000000000, -0.000000000000000000, -1.000000000000000000 ) ) ;
#7628 = ORIENTED_EDGE ( 'NONE', *, *, #64087, .T. ) ;
#7629 = CARTESIAN_POINT ( 'NONE',  ( -92.69370383062504004, 90.00000000000004263, 75.35531250086714294 ) ) ;
#7630 = PRODUCT_DEFINITION_FORMATION_WITH_SPECIFIED_SOURCE ( 'ANY', '', #9766, .NOT_KNOWN. ) ;
#7631 = ADVANCED_FACE ( 'NONE', ( #4036 ), #37120, .F. ) ;
#7632 = LINE ( 'NONE', #64789, #16569 ) ;
#7633 = DIRECTION ( 'NONE',  ( -1.000000000000000000, 0.000000000000000000, 0.000000000000000000 ) ) ;
#7634 = EDGE_CURVE ( 'NONE', #60432, #36593, #61166, .T. ) ;
#7635 = CARTESIAN_POINT ( 'NONE',  ( 92.35000000000000853, -209.9999999999999716, 84.36437500173430237 ) ) ;
#7636 = LINE ( 'NONE', #26027, #7750 ) ;
#7637 = CARTESIAN_POINT ( 'NONE',  ( -96.15314808468745866, -211.9973110713294489, 86.73239583420048859 ) ) ;
#7638 = ADVANCED_FACE ( 'NONE', ( #48388 ), #49128, .T. ) ;
#7639 = CARTESIAN_POINT ( 'NONE',  ( 5.000000000000002665, 74.18225833017888249, 34.94270380257665209 ) ) ;
#7640 = AXIS2_PLACEMENT_3D ( 'NONE', #16175, #68439, #6035 ) ;
#7641 = EDGE_CURVE ( 'NONE', #14148, #1244, #66436, .T. ) ;
#7642 = VECTOR ( 'NONE', #36477, 1000.000000000000000 ) ;
#7643 = CYLINDRICAL_SURFACE ( 'NONE', #24997, 42.00000000000000000 ) ;
#7644 = CARTESIAN_POINT ( 'NONE',  ( -92.69370383062498320, -209.9999999999999716, 77.41906250086715602 ) ) ;
#7645 = CARTESIAN_POINT ( 'NONE',  ( 0.000000000000000000, -55.19960302592104284, 51.03279382321070301 ) ) ;
#7646 = ORIENTED_EDGE ( 'NONE', *, *, #35330, .F. ) ;
#7647 = CARTESIAN_POINT ( 'NONE',  ( -92.35000000045951651, -209.9999506483816560, 87.22187670868756015 ) ) ;
#7648 = DIRECTION ( 'NONE',  ( 1.000000000000000000, 0.000000000000000000, 0.000000000000000000 ) ) ;
#7649 = CARTESIAN_POINT ( 'NONE',  ( -21.67772167707813935, -110.8034581014852762, 5.500000000000000000 ) ) ;
#7650 = CIRCLE ( 'NONE', #46087, 31.99999999999999289 ) ;
#7651 = CIRCLE ( 'NONE', #64071, 12.49999999999999822 ) ;
#7652 = DIRECTION ( 'NONE',  ( 0.000000000000000000, 0.8090169943749486725, -0.5877852522924713607 ) ) ;
#7654 = EDGE_CURVE ( 'NONE', #21827, #54492, #41320, .T. ) ;
#7653 = CARTESIAN_POINT ( 'NONE',  ( 93.84685191531249870, -208.0026889286704943, 78.10697916753380809 ) ) ;
#7655 = VERTEX_POINT ( 'NONE', #43521 ) ;
#7656 = EDGE_CURVE ( 'NONE', #10101, #14764, #26564, .T. ) ;
#7657 = FACE_OUTER_BOUND ( 'NONE', #18701, .T. ) ;
#7658 = FACE_OUTER_BOUND ( 'NONE', #65763, .T. ) ;
#7659 = ORIENTED_EDGE ( 'NONE', *, *, #45769, .T. ) ;
#7660 = FACE_OUTER_BOUND ( 'NONE', #66386, .T. ) ;
#7661 = ORIENTED_EDGE ( 'NONE', *, *, #34461, .T. ) ;
#7662 = DIRECTION ( 'NONE',  ( 0.000000000000000000, 0.000000000000000000, 1.000000000000000000 ) ) ;
#7663 = EDGE_CURVE ( 'NONE', #44464, #59117, #65325, .T. ) ;
#7664 = EDGE_CURVE ( 'NONE', #1704, #54121, #8547, .T. ) ;
#7665 = ORIENTED_EDGE ( 'NONE', *, *, #30644, .F. ) ;
#7666 = EDGE_LOOP ( 'NONE', ( #5210, #34211, #33527, #21898 ) ) ;
#7667 = ORIENTED_EDGE ( 'NONE', *, *, #23459, .T. ) ;
#7668 = DIRECTION ( 'NONE',  ( 2.603472992746261562E-14, 2.546204323184492723E-14, -1.000000000000000000 ) ) ;
#7669 = ORIENTED_EDGE ( 'NONE', *, *, #56882, .T. ) ;
#7670 = AXIS2_PLACEMENT_3D ( 'NONE', #56735, #28499, #22134 ) ;
#7671 = EDGE_LOOP ( 'NONE', ( #23753, #58367, #22947, #15159 ) ) ;
#7672 = CARTESIAN_POINT ( 'NONE',  ( 92.69370383062498320, 90.00000000000002842, 80.27656250086714351 ) ) ;
#7673 = CARTESIAN_POINT ( 'NONE',  ( 10.00000000000000000, -5.256550761632340141, -77.32052557432847095 ) ) ;
#7674 = CARTESIAN_POINT ( 'NONE',  ( 10.00000000000000000, 55.38113227695782115, 54.21277698773695164 ) ) ;
#7675 = ORIENTED_EDGE ( 'NONE', *, *, #18570, .T. ) ;
#7676 = AXIS2_PLACEMENT_3D ( 'NONE', #60275, #48604, #13639 ) ;
#7677 = VERTEX_POINT ( 'NONE', #68662 ) ;
#7678 = EDGE_LOOP ( 'NONE', ( #62460, #33822, #31770, #62441 ) ) ;
#7679 = LINE ( 'NONE', #53542, #74290 ) ;
#7680 = VERTEX_POINT ( 'NONE', #57011 ) ;
#7681 = VECTOR ( 'NONE', #42912, 1000.000000000000000 ) ;
#7682 = CARTESIAN_POINT ( 'NONE',  ( -13.50000000000001954, -72.99999999999998579, -255.0000000000000000 ) ) ;
#7683 = CARTESIAN_POINT ( 'NONE',  ( -97.64999999999996305, -209.9999999999999716, 77.29999999999999716 ) ) ;
#7684 = CARTESIAN_POINT ( 'NONE',  ( 0.000000000000000000, 0.000000000000000000, 0.000000000000000000 ) ) ;
#7685 = CARTESIAN_POINT ( 'NONE',  ( 15.00000000000000000, 16.61724383029390140, 20.69703378468902955 ) ) ;
#7686 = DIRECTION ( 'NONE',  ( -1.000000000000000000, 0.000000000000000000, 0.000000000000000000 ) ) ;
#7687 = CARTESIAN_POINT ( 'NONE',  ( 0.000000000000000000, 0.000000000000000000, 42.00000000000001421 ) ) ;
#7688 = DIRECTION ( 'NONE',  ( 0.000000000000000000, 0.000000000000000000, 1.000000000000000000 ) ) ;
#7689 = CARTESIAN_POINT ( 'NONE',  ( -96.32499999999996021, -207.7050326799711968, 77.90854166840097150 ) ) ;
#7690 = LINE ( 'NONE', #70091, #54295 ) ;
#7692 = CARTESIAN_POINT ( 'NONE',  ( -97.65000000000001990, 91.52997821335253548, 75.42145833506764063 ) ) ;
#7691 = CARTESIAN_POINT ( 'NONE',  ( 93.67499999999999716, 87.70503267997126784, 76.85020833506763438 ) ) ;
#7693 = ORIENTED_EDGE ( 'NONE', *, *, #20646, .T. ) ;
#7694 = CARTESIAN_POINT ( 'NONE',  ( 92.69370383062498320, 91.33154071421968467, 78.31864583420050963 ) ) ;
#7695 = CIRCLE ( 'NONE', #49693, 42.00000000000000000 ) ;
#7696 = DIRECTION ( 'NONE',  ( -0.000000000000000000, -0.000000000000000000, 1.000000000000000000 ) ) ;
#7697 = DIRECTION ( 'NONE',  ( -1.000000000000000000, 0.000000000000000000, 0.000000000000000000 ) ) ;
#7698 = LINE ( 'NONE', #37011, #39634 ) ;
#7699 = DIRECTION ( 'NONE',  ( -0.000000000000000000, -0.000000000000000000, 1.000000000000000000 ) ) ;
#7700 = CARTESIAN_POINT ( 'NONE',  ( 10.00000000000000000, -73.95703589263990807, 23.16143007188399139 ) ) ;
#7701 = ADVANCED_BREP_SHAPE_REPRESENTATION ( '', ( #36653, #43395 ), #21791 ) ;
#7702 = ORIENTED_EDGE ( 'NONE', *, *, #36649, .T. ) ;
#7704 = DIRECTION ( 'NONE',  ( 0.000000000000000000, -0.5224985647159379187, -0.8526401643540989506 ) ) ;
#7703 = CIRCLE ( 'NONE', #34100, 2.650000000000540812 ) ;
#7705 = CIRCLE ( 'NONE', #54501, 31.99999999999998934 ) ;
#7706 = CARTESIAN_POINT ( 'NONE',  ( -2.074714256722481664, 4.575665857285980742, -5.989444439476608650 ) ) ;
#7707 = VERTEX_POINT ( 'NONE', #73535 ) ;
#7708 = VERTEX_POINT ( 'NONE', #39346 ) ;
#7709 = EDGE_CURVE ( 'NONE', #34044, #57844, #49724, .T. ) ;
#7710 = ADVANCED_FACE ( 'NONE', ( #50229 ), #34066, .F. ) ;
#7711 = CARTESIAN_POINT ( 'NONE',  ( 95.00000000000000000, -206.9400435732949575, 82.85625000000000284 ) ) ;
#7712 = CARTESIAN_POINT ( 'NONE',  ( 0.000000000000000000, 36.88895765772642221, -6.736453364083161865 ) ) ;
#7713 = AXIS2_PLACEMENT_3D ( 'NONE', #49761, #48296, #48667 ) ;
#7714 = EDGE_CURVE ( 'NONE', #11647, #47006, #71302, .T. ) ;
#7715 = CARTESIAN_POINT ( 'NONE',  ( 10.00000000000000000, -59.03961581697432592, 46.53671651293927880 ) ) ;
#7716 = LINE ( 'NONE', #13351, #29345 ) ;
#7717 = CARTESIAN_POINT ( 'NONE',  ( -92.69370383062498320, -211.3315407142195852, 77.36614583420048064 ) ) ;
#7718 = ORIENTED_EDGE ( 'NONE', *, *, #69780, .F. ) ;
#7719 = VECTOR ( 'NONE', #5764, 1000.000000000000000 ) ;
#7720 = ADVANCED_FACE ( 'NONE', ( #5516 ), #4402, .T. ) ;
#7721 = CARTESIAN_POINT ( 'NONE',  ( 95.00000000000000000, -209.9999999999999716, 90.00000000000000000 ) ) ;
#7722 = LINE ( 'NONE', #37036, #3076 ) ;
#7723 = DIRECTION ( 'NONE',  ( -1.000000000000000000, -0.000000000000000000, 0.000000000000000000 ) ) ;
#7724 = ADVANCED_FACE ( 'NONE', ( #40446 ), #28419, .F. ) ;
#7725 = LINE ( 'NONE', #70123, #62071 ) ;
#7726 = DIRECTION ( 'NONE',  ( -1.000000000000000000, 0.000000000000000000, 0.000000000000000000 ) ) ;
#7727 = DIRECTION ( 'NONE',  ( 0.000000000000000000, 0.000000000000000000, 1.000000000000000000 ) ) ;
#7728 = DIRECTION ( 'NONE',  ( -1.000000000000000000, 0.000000000000000000, 0.000000000000000000 ) ) ;
#7729 = DIRECTION ( 'NONE',  ( 0.000000000000000000, 0.3090169943749480619, -0.9510565162951533091 ) ) ;
#7730 = AXIS2_PLACEMENT_3D ( 'NONE', #63125, #34513, #23252 ) ;
#7731 =( BOUNDED_CURVE ( )  B_SPLINE_CURVE ( 2, ( #39624, #68194, #50520, #44898, #21572, #15572, #27957 ),
 .UNSPECIFIED., .F., .F. ) 
 B_SPLINE_CURVE_WITH_KNOTS ( ( 3, 2, 2, 3 ),
 ( 0.7291666666666665186, 0.7361111111111109384, 0.7430555555555553582, 0.7499999999999996669 ),
 .UNSPECIFIED. ) 
 CURVE ( )  GEOMETRIC_REPRESENTATION_ITEM ( )  RATIONAL_B_SPLINE_CURVE ( ( 1.000000000000002220, 0.8660254037844365982, 1.000000000000000000, 0.8660254037844387076, 1.000000000000000000, 0.8660254037844451469, 0.9999999999999935607 ) ) 
 REPRESENTATION_ITEM ( '' )  );
#7732 = EDGE_CURVE ( 'NONE', #56025, #57064, #56646, .T. ) ;
#7733 = CARTESIAN_POINT ( 'NONE',  ( 96.15314808468748708, 91.99731107132950569, 83.87489583420048689 ) ) ;
#7734 = CARTESIAN_POINT ( 'NONE',  ( -92.69370383062498320, -211.3315407142195852, 84.98614583420047097 ) ) ;
#7735 = DIRECTION ( 'NONE',  ( 0.000000000000000000, 0.4539904997395479702, -0.8910065241883673437 ) ) ;
#7736 = ORIENTED_EDGE ( 'NONE', *, *, #55840, .F. ) ;
#7737 = DIRECTION ( 'NONE',  ( 0.000000000000000000, 0.000000000000000000, -1.000000000000000000 ) ) ;
#7738 = CARTESIAN_POINT ( 'NONE',  ( -93.67499999999998295, -207.7050326799711968, 79.62833333333333030 ) ) ;
#7739 = CARTESIAN_POINT ( 'NONE',  ( -96.15314808468751551, 88.00268892867056536, 77.04864583420047097 ) ) ;
#7740 = AXIS2_PLACEMENT_3D ( 'NONE', #22105, #38659, #67598 ) ;
#7742 = ADVANCED_FACE ( 'NONE', ( #276 ), #73910, .F. ) ;
#7741 = CARTESIAN_POINT ( 'NONE',  ( 93.84685191531249870, -208.0026889286704943, 88.26697916753380468 ) ) ;
#7743 = ORIENTED_EDGE ( 'NONE', *, *, #6556, .F. ) ;
#7744 = EDGE_CURVE ( 'NONE', #32195, #17108, #22805, .T. ) ;
#7745 = DIRECTION ( 'NONE',  ( -1.000000000000000000, 0.000000000000000000, 0.000000000000000000 ) ) ;
#7746 = ORIENTED_EDGE ( 'NONE', *, *, #17336, .T. ) ;
#7747 = AXIS2_PLACEMENT_3D ( 'NONE', #1442, #58917, #53267 ) ;
#7748 = VECTOR ( 'NONE', #42150, 1000.000000000000000 ) ;
#7749 = ORIENTED_EDGE ( 'NONE', *, *, #72728, .T. ) ;
#7750 = VECTOR ( 'NONE', #71142, 1000.000000000000000 ) ;
#7751 = CARTESIAN_POINT ( 'NONE',  ( 97.64999999999999147, -209.9999999999999716, 75.71250000000000568 ) ) ;
#7752 = AXIS2_PLACEMENT_3D ( 'NONE', #15600, #26508, #49438 ) ;
#7753 = CARTESIAN_POINT ( 'NONE',  ( 10.00000000000000000, 30.84782396557218931, 21.32104025579126017 ) ) ;
#7754 = VERTEX_POINT ( 'NONE', #40082 ) ;
#7755 = ORIENTED_EDGE ( 'NONE', *, *, #65848, .F. ) ;
#7756 = CIRCLE ( 'NONE', #66579, 15.99999999999999645 ) ;
#7757 = CARTESIAN_POINT ( 'NONE',  ( 0.000000000000000000, 0.000000000000000000, 0.000000000000000000 ) ) ;
#7758 = CARTESIAN_POINT ( 'NONE',  ( 95.00000000000000000, -212.6630814284392557, 81.70531250086715147 ) ) ;
#7759 = DIRECTION ( 'NONE',  ( 1.000000000000000000, 0.000000000000000000, 0.000000000000000000 ) ) ;
#7761 = LINE ( 'NONE', #47243, #65241 ) ;
#7760 = VECTOR ( 'NONE', #39856, 1000.000000000000000 ) ;
#7762 = DIRECTION ( 'NONE',  ( 0.000000000000000000, 0.4539904997395476927, -0.8910065241883674547 ) ) ;
#7763 = DIRECTION ( 'NONE',  ( 0.000000000000000000, 0.000000000000000000, -1.000000000000000000 ) ) ;
#7764 = DIRECTION ( 'NONE',  ( -1.000000000000000000, -0.000000000000000000, 0.000000000000000000 ) ) ;
#7765 = CARTESIAN_POINT ( 'NONE',  ( 96.32499999999998863, -212.2949673200287179, 83.22666666666665947 ) ) ;
#7766 = CIRCLE ( 'NONE', #1797, 82.00000000000000000 ) ;
#7767 = VERTEX_POINT ( 'NONE', #44621 ) ;
#7768 = ORIENTED_EDGE ( 'NONE', *, *, #55280, .F. ) ;
#7769 = EDGE_LOOP ( 'NONE', ( #58424, #55135, #31790, #7675 ) ) ;
#7770 = ORIENTED_EDGE ( 'NONE', *, *, #49901, .F. ) ;
#7771 = CARTESIAN_POINT ( 'NONE',  ( -95.00000000000002842, 87.33691857156074434, 85.51531250086713953 ) ) ;
#7772 = CYLINDRICAL_SURFACE ( 'NONE', #36557, 16.00000000000000000 ) ;
#7773 = FACE_OUTER_BOUND ( 'NONE', #9270, .T. ) ;
#7774 = CARTESIAN_POINT ( 'NONE',  ( 93.84685191531249870, -208.0026889286704943, 86.99697916753380866 ) ) ;
#7775 = DIRECTION ( 'NONE',  ( -0.3853207896976523772, 0.9227826878668550226, 0.000000000000000000 ) ) ;
#7776 = ORIENTED_EDGE ( 'NONE', *, *, #9834, .F. ) ;
#7777 = CARTESIAN_POINT ( 'NONE',  ( 93.67499999999998295, 92.29496732002878900, 79.73416666666666686 ) ) ;
#7778 = EDGE_CURVE ( 'NONE', #56779, #27169, #34430, .T. ) ;
#7779 = ORIENTED_EDGE ( 'NONE', *, *, #16014, .T. ) ;
#7780 = LINE ( 'NONE', #24335, #30187 ) ;
#7781 = ORIENTED_EDGE ( 'NONE', *, *, #29769, .T. ) ;
#7782 = CARTESIAN_POINT ( 'NONE',  ( -95.00000000000002842, 93.05995642670501411, 84.84062500173429555 ) ) ;
#7783 = CARTESIAN_POINT ( 'NONE',  ( 93.84685191531248449, 91.99731107132950569, 86.52072916753382970 ) ) ;
#7784 = CYLINDRICAL_SURFACE ( 'NONE', #64603, 42.00000000000000000 ) ;
#7785 = CARTESIAN_POINT ( 'NONE',  ( 4.999999999999999112, 21.40280677340371795, 36.13751322684426270 ) ) ;
#7786 = CARTESIAN_POINT ( 'NONE',  ( 0.000000000000000000, 0.000000000000000000, 0.000000000000000000 ) ) ;
#7787 = CARTESIAN_POINT ( 'NONE',  ( 0.000000000000000000, 0.000000000000000000, -2.500000000000000000 ) ) ;
#7788 = ORIENTED_EDGE ( 'NONE', *, *, #14651, .F. ) ;
#7789 = CARTESIAN_POINT ( 'NONE',  ( 0.000000000000000000, 5.835314593368477354, 22.81335362449854642 ) ) ;
#7790 = CARTESIAN_POINT ( 'NONE',  ( -93.84685191531247028, -211.9973110713294489, 75.88447916753381151 ) ) ;
#7791 = ORIENTED_EDGE ( 'NONE', *, *, #61728, .T. ) ;
#7792 = EDGE_LOOP ( 'NONE', ( #61292, #32926, #66037, #71907 ) ) ;
#7793 = EDGE_CURVE ( 'NONE', #31889, #25853, #38973, .T. ) ;
#7794 = FACE_OUTER_BOUND ( 'NONE', #47633, .T. ) ;
#7795 = EDGE_CURVE ( 'NONE', #8585, #39671, #23359, .T. ) ;
#7796 = DIRECTION ( 'NONE',  ( 0.000000000000000000, 0.000000000000000000, 1.000000000000000000 ) ) ;
#7797 = CARTESIAN_POINT ( 'NONE',  ( -7.500000000000016875, -80.00000000000001421, -189.9999999999999147 ) ) ;
#7798 = CARTESIAN_POINT ( 'NONE',  ( -97.30629616937495996, -209.9999999999999716, 88.53156250086716739 ) ) ;
#7799 = ORIENTED_EDGE ( 'NONE', *, *, #64674, .F. ) ;
#7800 = AXIS2_PLACEMENT_3D ( 'NONE', #72174, #9394, #16525 ) ;
#7801 = CARTESIAN_POINT ( 'NONE',  ( -97.64999999999996305, -209.9999999999999716, 82.37999999999999545 ) ) ;
#7802 = AXIS2_PLACEMENT_3D ( 'NONE', #72937, #44405, #28571 ) ;
#7803 = ORIENTED_EDGE ( 'NONE', *, *, #13085, .F. ) ;
#7804 = ADVANCED_FACE ( 'NONE', ( #63393 ), #5885, .F. ) ;
#7805 = EDGE_CURVE ( 'NONE', #57727, #62061, #25699, .T. ) ;
#7806 = ORIENTED_EDGE ( 'NONE', *, *, #69005, .F. ) ;
#7807 = CYLINDRICAL_SURFACE ( 'NONE', #35496, 82.00000000000000000 ) ;
#7808 = CARTESIAN_POINT ( 'NONE',  ( 11.59999999999999787, 1.420590287010929336E-15, 53.20000000000001705 ) ) ;
#7809 = LINE ( 'NONE', #53671, #9745 ) ;
#7810 = CARTESIAN_POINT ( 'NONE',  ( 93.84685191531248449, 91.99731107132950569, 81.28197916753380525 ) ) ;
#7811 = CARTESIAN_POINT ( 'NONE',  ( -97.64999999999996305, -209.9999999999999716, 83.65000000000000568 ) ) ;
#7812 = CYLINDRICAL_SURFACE ( 'NONE', #1409, 16.00000000000000000 ) ;
#7813 = VECTOR ( 'NONE', #54781, 1000.000000000000000 ) ;
#7814 = CARTESIAN_POINT ( 'NONE',  ( 6.782329983125270800, 10.49999999999999467, -145.0000000000000000 ) ) ;
#7815 = LINE ( 'NONE', #29996, #19554 ) ;
#7816 = DIRECTION ( 'NONE',  ( 0.000000000000000000, 0.000000000000000000, 1.000000000000000000 ) ) ;
#7817 = DIRECTION ( 'NONE',  ( -0.000000000000000000, -0.000000000000000000, -1.000000000000000000 ) ) ;
#7818 = CARTESIAN_POINT ( 'NONE',  ( 94.99999999999998579, 86.94004357329502852, 83.80875000000000341 ) ) ;
#7819 = EDGE_CURVE ( 'NONE', #48253, #38472, #55887, .T. ) ;
#7820 = FACE_OUTER_BOUND ( 'NONE', #33123, .T. ) ;
#7821 = VECTOR ( 'NONE', #35894, 1000.000000000000114 ) ;
#7822 = DIRECTION ( 'NONE',  ( 0.000000000000000000, 0.000000000000000000, 1.000000000000000000 ) ) ;
#7823 = ORIENTED_EDGE ( 'NONE', *, *, #3907, .T. ) ;
#7824 = CARTESIAN_POINT ( 'NONE',  ( -92.69370383062504004, 90.00000000000004263, 88.05531250086713158 ) ) ;
#7825 = LINE ( 'NONE', #52953, #44351 ) ;
#7826 = AXIS2_PLACEMENT_3D ( 'NONE', #6533, #27966, #57674 ) ;
#7828 = EDGE_CURVE ( 'NONE', #51811, #44034, #33305, .T. ) ;
#7827 = CARTESIAN_POINT ( 'NONE',  ( 10.00000000000000000, -33.79645857604501913, -16.45098606841161626 ) ) ;
#7829 = EDGE_LOOP ( 'NONE', ( #47522, #18086, #61325, #71625 ) ) ;
#7830 = CARTESIAN_POINT ( 'NONE',  ( -6.170112525937308412, 10.87104923258428890, 42.00000000000001421 ) ) ;
#7831 = EDGE_CURVE ( 'NONE', #50886, #4344, #56035, .T. ) ;
#7832 = DIRECTION ( 'NONE',  ( 0.000000000000000000, 0.000000000000000000, -1.000000000000000000 ) ) ;
#7833 = FACE_OUTER_BOUND ( 'NONE', #4363, .T. ) ;
#7834 = DIRECTION ( 'NONE',  ( 1.000000000000000000, 0.000000000000000000, -0.000000000000000000 ) ) ;
#7835 = VECTOR ( 'NONE', #71938, 1000.000000000000000 ) ;
#7836 = CARTESIAN_POINT ( 'NONE',  ( 97.30629616937498838, -208.6684592857803011, 81.91697916753381037 ) ) ;
#7837 = EDGE_LOOP ( 'NONE', ( #56875, #59750, #57543, #29754, #19291, #40900 ) ) ;
#7838 = ORIENTED_EDGE ( 'NONE', *, *, #37171, .T. ) ;
#7839 = DIRECTION ( 'NONE',  ( -1.000000000000000000, 0.000000000000000000, 0.000000000000000000 ) ) ;
#7840 = ORIENTED_EDGE ( 'NONE', *, *, #5233, .T. ) ;
#7841 = DIRECTION ( 'NONE',  ( -0.000000000000000000, 0.8660254037844368202, 0.5000000000000031086 ) ) ;
#7842 = CARTESIAN_POINT ( 'NONE',  ( 11.99999999999999822, -59.03342792756297541, 46.54456581323783126 ) ) ;
#7843 = VECTOR ( 'NONE', #30301, 1000.000000000000000 ) ;
#7844 = ORIENTED_EDGE ( 'NONE', *, *, #17000, .T. ) ;
#7845 = AXIS2_PLACEMENT_3D ( 'NONE', #34413, #39330, #11122 ) ;
#7846 = CARTESIAN_POINT ( 'NONE',  ( 93.84685191531251292, -211.9973110713294489, 79.74739583420048916 ) ) ;
#7847 = EDGE_LOOP ( 'NONE', ( #20526, #60945, #45325, #63356 ) ) ;
#7848 = CYLINDRICAL_SURFACE ( 'NONE', #65959, 37.49900000000000233 ) ;
#7849 = ORIENTED_EDGE ( 'NONE', *, *, #24936, .T. ) ;
#7850 = VECTOR ( 'NONE', #52960, 1000.000000000000000 ) ;
#7851 = ORIENTED_EDGE ( 'NONE', *, *, #4072, .F. ) ;
#7852 = CARTESIAN_POINT ( 'NONE',  ( -96.32499999999996021, -207.7050326799711968, 82.35354166840096468 ) ) ;
#7853 = CARTESIAN_POINT ( 'NONE',  ( 97.64999999946594755, 90.00005320149050192, 78.96687695417308817 ) ) ;
#7854 = AXIS2_PLACEMENT_3D ( 'NONE', #6613, #11866, #641 ) ;
#7855 = ORIENTED_EDGE ( 'NONE', *, *, #49320, .T. ) ;
#7856 = LINE ( 'NONE', #12750, #24479 ) ;
#7857 = CARTESIAN_POINT ( 'NONE',  ( 97.64999999999997726, -208.4700217866474645, 83.46479166840096298 ) ) ;
#7858 = CARTESIAN_POINT ( 'NONE',  ( 92.34999999999999432, 91.52997821335252127, 84.23208333333333542 ) ) ;
#7859 = EDGE_LOOP ( 'NONE', ( #46539, #69107, #56585, #11654 ) ) ;
#7860 = CARTESIAN_POINT ( 'NONE',  ( -25.50183398199384754, -112.6408924756582053, 2.500000000000000000 ) ) ;
#7861 = DIRECTION ( 'NONE',  ( 0.000000000000000000, 0.000000000000000000, -1.000000000000000000 ) ) ;
#7862 = VERTEX_POINT ( 'NONE', #69755 ) ;
#7863 = EDGE_LOOP ( 'NONE', ( #49210, #51401, #64566, #45309 ) ) ;
#7864 = CARTESIAN_POINT ( 'NONE',  ( -97.30629616937501680, 88.66845928578038638, 87.94947916753382344 ) ) ;
#7865 = CARTESIAN_POINT ( 'NONE',  ( 93.84685191531248449, 88.00268892867053694, 85.93864583420048575 ) ) ;
#7866 = ORIENTED_EDGE ( 'NONE', *, *, #54328, .F. ) ;
#7867 = CIRCLE ( 'NONE', #19879, 77.49900000000000944 ) ;
#7868 = CARTESIAN_POINT ( 'NONE',  ( 93.67499999999998295, 92.29496732002878900, 85.52854166840096184 ) ) ;
#7869 = EDGE_CURVE ( 'NONE', #44533, #54089, #47568, .T. ) ;
#7870 = ORIENTED_EDGE ( 'NONE', *, *, #51256, .T. ) ;
#7871 = FACE_BOUND ( 'NONE', #10810, .T. ) ;
#7872 = ORIENTED_EDGE ( 'NONE', *, *, #68849, .T. ) ;
#7873 = ORIENTED_EDGE ( 'NONE', *, *, #23283, .F. ) ;
#7874 = VECTOR ( 'NONE', #37720, 1000.000000000000227 ) ;
#7875 = ORIENTED_EDGE ( 'NONE', *, *, #55617, .T. ) ;
#7876 = CARTESIAN_POINT ( 'NONE',  ( -95.00000000000002842, 93.05995642670504253, 86.03125000000000000 ) ) ;
#7877 = EDGE_CURVE ( 'NONE', #72240, #48807, #637, .T. ) ;
#7878 = DIRECTION ( 'NONE',  ( 0.000000000000000000, 0.1564344650402244019, 0.9876883405951387696 ) ) ;
#7879 = CARTESIAN_POINT ( 'NONE',  ( -96.32500000000001705, 92.29496732002878900, 84.81416666666666515 ) ) ;
#7880 = EDGE_CURVE ( 'NONE', #19238, #67909, #52456, .T. ) ;
#7881 = EDGE_LOOP ( 'NONE', ( #66131, #49749, #72498, #39701 ) ) ;
#7882 = CARTESIAN_POINT ( 'NONE',  ( 93.67499999999999716, 87.70503267997126784, 81.85083333333332689 ) ) ;
#7883 = DIRECTION ( 'NONE',  ( -0.000000000000000000, -0.000000000000000000, 1.000000000000000000 ) ) ;
#7884 = ORIENTED_EDGE ( 'NONE', *, *, #2505, .F. ) ;
#7885 = DIRECTION ( 'NONE',  ( -1.000000000000000000, -0.000000000000000000, 0.000000000000000000 ) ) ;
#7886 = CARTESIAN_POINT ( 'NONE',  ( -94.99999999999997158, -212.6630814284392557, 82.81656250086713555 ) ) ;
#7887 = ORIENTED_EDGE ( 'NONE', *, *, #28259, .F. ) ;
#7888 = CYLINDRICAL_SURFACE ( 'NONE', #8658, 31.99999999999999289 ) ;
#7889 = PLANE ( 'NONE',  #33224 ) ;
#7890 = DIRECTION ( 'NONE',  ( -1.000000000000000000, 0.000000000000000000, 0.000000000000000000 ) ) ;
#7891 = CARTESIAN_POINT ( 'NONE',  ( -3.000000000000000000, 20.85821328998756385, -10.92862929874494959 ) ) ;
#7892 = EDGE_CURVE ( 'NONE', #53084, #44533, #59219, .T. ) ;
#7893 = DIRECTION ( 'NONE',  ( -0.08130631524010117905, 0.9966891607226784355, 0.000000000000000000 ) ) ;
#7894 = PLANE ( 'NONE',  #18115 ) ;
#7895 = CARTESIAN_POINT ( 'NONE',  ( 0.000000000000000000, 55.19960302592066625, 51.03279382321107249 ) ) ;
#7896 = CARTESIAN_POINT ( 'NONE',  ( 93.67499999999998295, 92.29496732002878900, 82.98854166840096980 ) ) ;
#7897 = CARTESIAN_POINT ( 'NONE',  ( 97.30629616937500259, 90.00000000000002842, 74.79348190356851944 ) ) ;
#7898 = CARTESIAN_POINT ( 'NONE',  ( -93.84685191531252713, 88.00268892867056536, 89.37822916753381719 ) ) ;
#7899 = LINE ( 'NONE', #53765, #73097 ) ;
#7900 = DIRECTION ( 'NONE',  ( -0.000000000000000000, -0.000000000000000000, -1.000000000000000000 ) ) ;
#7901 = EDGE_CURVE ( 'NONE', #46053, #71434, #19739, .T. ) ;
#7902 = EDGE_CURVE ( 'NONE', #26184, #70313, #29154, .T. ) ;
#7903 = AXIS2_PLACEMENT_3D ( 'NONE', #905, #60606, #43328 ) ;
#7904 = DIRECTION ( 'NONE',  ( 0.000000000000000000, 0.000000000000000000, 1.000000000000000000 ) ) ;
#7905 = EDGE_CURVE ( 'NONE', #58612, #16918, #24275, .T. ) ;
#7906 = EDGE_CURVE ( 'NONE', #39489, #42628, #60348, .T. ) ;
#7908 = CARTESIAN_POINT ( 'NONE',  ( 90.00000000000000000, 95.00000000000002842, 90.00000000000000000 ) ) ;
#7907 = VECTOR ( 'NONE', #47538, 1000.000000000000000 ) ;
#7909 = LINE ( 'NONE', #47400, #50201 ) ;
#7910 = CARTESIAN_POINT ( 'NONE',  ( 95.73997229764715655, 87.43182282693489071, 75.00000000000000000 ) ) ;
#7911 = CYLINDRICAL_SURFACE ( 'NONE', #29795, 26.50000000000000355 ) ;
#7912 = VECTOR ( 'NONE', #56680, 1000.000000000000000 ) ;
#7913 = CYLINDRICAL_SURFACE ( 'NONE', #48422, 2.649999999999985700 ) ;
#7914 = CARTESIAN_POINT ( 'NONE',  ( -97.64999999999994884, -208.4700217866474645, 86.77208333333334167 ) ) ;
#7915 = AXIS2_PLACEMENT_3D ( 'NONE', #4141, #43978, #43619 ) ;
#7916 = CARTESIAN_POINT ( 'NONE',  ( 0.000000000000000000, 44.88180994100468268, -63.18004540532978552 ) ) ;
#7917 = EDGE_CURVE ( 'NONE', #32536, #16853, #16154, .T. ) ;
#7918 = CIRCLE ( 'NONE', #15106, 12.75000000000000000 ) ;
#7919 = ORIENTED_EDGE ( 'NONE', *, *, #22703, .F. ) ;
#7920 = DIRECTION ( 'NONE',  ( 2.603472992746261562E-14, 2.546204323184492723E-14, -1.000000000000000000 ) ) ;
#7921 = LINE ( 'NONE', #26681, #52669 ) ;
#7922 = SURFACE_STYLE_USAGE ( .BOTH. , #37249 ) ;
#7923 = FACE_OUTER_BOUND ( 'NONE', #3663, .T. ) ;
#7924 = PRESENTATION_LAYER_ASSIGNMENT (  '', '', ( #65580 ) ) ;
#7925 = VERTEX_POINT ( 'NONE', #57750 ) ;
#7926 = CARTESIAN_POINT ( 'NONE',  ( -12.40464318976452596, 10.41032311384371489, 52.00000000000002132 ) ) ;
#7927 = DIRECTION ( 'NONE',  ( 0.000000000000000000, 0.000000000000000000, 1.000000000000000000 ) ) ;
#7928 = EDGE_LOOP ( 'NONE', ( #4269, #36616, #16259, #51125 ) ) ;
#7929 =( BOUNDED_CURVE ( )  B_SPLINE_CURVE ( 2, ( #59769, #48480, #41367, #64666, #19161, #71395, #42843 ),
 .UNSPECIFIED., .F., .F. ) 
 B_SPLINE_CURVE_WITH_KNOTS ( ( 3, 2, 2, 3 ),
 ( 0.3125000000000001665, 0.3194444444444445308, 0.3263888888888890061, 0.3333333333333333703 ),
 .UNSPECIFIED. ) 
 CURVE ( )  GEOMETRIC_REPRESENTATION_ITEM ( )  RATIONAL_B_SPLINE_CURVE ( ( 0.9999999999999967804, 0.8660254037844419273, 1.000000000000000000, 0.8660254037844387076, 1.000000000000000000, 0.8660254037844375974, 1.000000000000001110 ) ) 
 REPRESENTATION_ITEM ( '' )  );
#7930 = CARTESIAN_POINT ( 'NONE',  ( 93.84685191531251292, -211.9973110713294489, 84.03364583420047040 ) ) ;
#7931 = CARTESIAN_POINT ( 'NONE',  ( 93.84685191531249870, -208.0026889286704943, 88.42572916753381662 ) ) ;
#7932 = ORIENTED_EDGE ( 'NONE', *, *, #2305, .F. ) ;
#7933 = CARTESIAN_POINT ( 'NONE',  ( 97.30629616937498838, -211.3315407142195852, 89.43114583420049257 ) ) ;
#7934 = ORIENTED_EDGE ( 'NONE', *, *, #546, .F. ) ;
#7935 = DIRECTION ( 'NONE',  ( 0.9966891607226785466, 0.08130631524009969413, -0.000000000000000000 ) ) ;
#7936 = ORIENTED_EDGE ( 'NONE', *, *, #24354, .T. ) ;
#7937 = CARTESIAN_POINT ( 'NONE',  ( -96.15314808468751551, 88.00268892867056536, 79.74739583420048916 ) ) ;
#7938 = EDGE_LOOP ( 'NONE', ( #34410, #30228, #72645, #8142 ) ) ;
#7939 = ORIENTED_EDGE ( 'NONE', *, *, #55262, .F. ) ;
#7940 = CARTESIAN_POINT ( 'NONE',  ( -96.32499999999996021, -212.2949673200287179, 87.64520833506762187 ) ) ;
#7941 = ORIENTED_EDGE ( 'NONE', *, *, #43110, .T. ) ;
#7942 = DIRECTION ( 'NONE',  ( 0.000000000000000000, 0.000000000000000000, 1.000000000000000000 ) ) ;
#7943 = CARTESIAN_POINT ( 'NONE',  ( 10.00000000000000000, 0.000000000000000000, 0.000000000000000000 ) ) ;
#7944 = ORIENTED_EDGE ( 'NONE', *, *, #5513, .F. ) ;
#7945 = CARTESIAN_POINT ( 'NONE',  ( 0.000000000000000000, 68.55367621811141987, 44.99326035066078333 ) ) ;
#7946 = ORIENTED_EDGE ( 'NONE', *, *, #33077, .T. ) ;
#7947 =( BOUNDED_CURVE ( )  B_SPLINE_CURVE ( 2, ( #27316, #56284, #50249, #58033, #73187, #21685, #61928 ),
 .UNSPECIFIED., .F., .F. ) 
 B_SPLINE_CURVE_WITH_KNOTS ( ( 3, 2, 2, 3 ),
 ( 0.4374999999999994449, 0.4444444444444441422, 0.4513888888888888951, 0.4583333333333335924 ),
 .UNSPECIFIED. ) 
 CURVE ( )  GEOMETRIC_REPRESENTATION_ITEM ( )  RATIONAL_B_SPLINE_CURVE ( ( 1.000000000000010658, 0.8660254037844280495, 1.000000000000000000, 0.8660254037844387076, 1.000000000000000000, 0.8660254037844333785, 1.000000000000005329 ) ) 
 REPRESENTATION_ITEM ( '' )  );
#7948 = CARTESIAN_POINT ( 'NONE',  ( 92.35000000000000853, -209.9999999999999716, 90.00000000000000000 ) ) ;
#7949 = AXIS2_PLACEMENT_3D ( 'NONE', #26004, #48575, #36918 ) ;
#7950 = ORIENTED_EDGE ( 'NONE', *, *, #27324, .F. ) ;
#7951 = EDGE_CURVE ( 'NONE', #65031, #27079, #7716, .T. ) ;
#7952 = VERTEX_POINT ( 'NONE', #36281 ) ;
#7953 = ORIENTED_EDGE ( 'NONE', *, *, #58135, .T. ) ;
#7954 = CARTESIAN_POINT ( 'NONE',  ( 92.69370383062501162, -208.6684592857803011, 76.88989583420047325 ) ) ;
#7955 = CARTESIAN_POINT ( 'NONE',  ( -95.00000000000002842, 93.05995642670504253, 83.49125000000000796 ) ) ;
#7956 = CARTESIAN_POINT ( 'NONE',  ( 10.00000000000000000, -68.55367621811173251, 44.99326035066030016 ) ) ;
#7958 = EDGE_CURVE ( 'NONE', #57048, #66402, #52157, .T. ) ;
#7957 = ORIENTED_EDGE ( 'NONE', *, *, #1091, .T. ) ;
#7959 = LINE ( 'NONE', #70354, #14850 ) ;
#7960 = AXIS2_PLACEMENT_3D ( 'NONE', #54212, #65126, #30151 ) ;
#7961 = DIRECTION ( 'NONE',  ( 0.000000000000000000, 0.000000000000000000, 1.000000000000000000 ) ) ;
#7962 = EDGE_CURVE ( 'NONE', #5557, #26897, #29890, .T. ) ;
#7963 = LINE ( 'NONE', #24517, #71600 ) ;
#7964 = VECTOR ( 'NONE', #4372, 1000.000000000000114 ) ;
#7965 = FACE_OUTER_BOUND ( 'NONE', #338, .T. ) ;
#7966 = EDGE_CURVE ( 'NONE', #63936, #44444, #42153, .T. ) ;
#7967 = CARTESIAN_POINT ( 'NONE',  ( -235.0000123116479926, -123.0000000000000284, 2.500000000000000000 ) ) ;
#7968 = CARTESIAN_POINT ( 'NONE',  ( -97.30629616937495996, -209.9999999999999716, 80.75281250086715090 ) ) ;
#7969 = CARTESIAN_POINT ( 'NONE',  ( -95.00000000000002842, 92.66308142843932671, 77.57781250086715374 ) ) ;
#7970 = ORIENTED_EDGE ( 'NONE', *, *, #38696, .F. ) ;
#7971 = AXIS2_PLACEMENT_3D ( 'NONE', #58298, #69578, #100 ) ;
#7972 = CARTESIAN_POINT ( 'NONE',  ( 92.69370383062498320, 90.00000000000002842, 82.65781250086713783 ) ) ;
#7973 = AXIS2_PLACEMENT_3D ( 'NONE', #17331, #21467, #4584 ) ;
#7974 = EDGE_CURVE ( 'NONE', #2269, #44809, #15742, .T. ) ;
#7975 = VERTEX_POINT ( 'NONE', #18616 ) ;
#7976 = CARTESIAN_POINT ( 'NONE',  ( 92.35000000010803944, 90.00001510551041406, 78.64888723592453346 ) ) ;
#7977 = DIRECTION ( 'NONE',  ( -1.000000000000000000, -0.000000000000000000, -0.000000000000000000 ) ) ;
#7978 = CARTESIAN_POINT ( 'NONE',  ( -97.64995971452495382, -211.5300014721822208, 83.14729327728629471 ) ) ;
#7979 = LINE ( 'NONE', #9085, #22346 ) ;
#7980 = DIRECTION ( 'NONE',  ( -1.000000000000000000, -0.000000000000000000, -0.000000000000000000 ) ) ;
#7981 = CARTESIAN_POINT ( 'NONE',  ( -97.30629616937497417, -211.3315407142195852, 84.61572916753380014 ) ) ;
#7982 = EDGE_CURVE ( 'NONE', #58170, #37734, #6609, .T. ) ;
#7983 = LINE ( 'NONE', #7615, #56673 ) ;
#7984 = CARTESIAN_POINT ( 'NONE',  ( 5.000000000000000000, -15.48615015657610705, 39.04073710021338428 ) ) ;
#7985 = CARTESIAN_POINT ( 'NONE',  ( 10.00000000000000000, -12.26510123303284594, 35.53030884539080603 ) ) ;
#7986 = VERTEX_POINT ( 'NONE', #12969 ) ;
#7987 = CIRCLE ( 'NONE', #38037, 82.00000000000000000 ) ;
#7988 = VERTEX_POINT ( 'NONE', #46839 ) ;
#7989 = CARTESIAN_POINT ( 'NONE',  ( -11.70000000000000107, 2.137572712735109784E-15, -17.45460580326810174 ) ) ;
#7990 = CARTESIAN_POINT ( 'NONE',  ( 92.34999999999999432, 90.00000000000002842, 84.92000000000000171 ) ) ;
#7991 = DIRECTION ( 'NONE',  ( -1.000000000000000000, 0.000000000000000000, 0.000000000000000000 ) ) ;
#7992 = CARTESIAN_POINT ( 'NONE',  ( -96.15314808468751551, 88.00268892867056536, 85.30364583420046642 ) ) ;
#7993 = DIRECTION ( 'NONE',  ( -1.000000000000000000, 0.000000000000000000, -0.000000000000000000 ) ) ;
#7994 = CARTESIAN_POINT ( 'NONE',  ( -20.63750000000001705, -1.978676859095576340E-13, -15.80000000000029914 ) ) ;
#7995 = CARTESIAN_POINT ( 'NONE',  ( -97.65000000000001990, 90.00000000000004263, 83.65000000000000568 ) ) ;
#7996 = EDGE_LOOP ( 'NONE', ( #12479, #33784, #4745, #12957 ) ) ;
#7997 = EDGE_CURVE ( 'NONE', #26343, #18301, #35906, .T. ) ;
#7998 = CARTESIAN_POINT ( 'NONE',  ( -97.30629616937501680, 88.66845928578038638, 76.36072916753381890 ) ) ;
#7999 = ADVANCED_FACE ( 'NONE', ( #53210 ), #24634, .T. ) ;
#8000 = EDGE_CURVE ( 'NONE', #2885, #34381, #31294, .T. ) ;
#8001 = DIRECTION ( 'NONE',  ( 2.603472992746261562E-14, 2.546204323184492723E-14, -1.000000000000000000 ) ) ;
#8002 = PLANE ( 'NONE',  #22666 ) ;
#8003 = CARTESIAN_POINT ( 'NONE',  ( -93.07557990970624928, -211.8218417373838065, 75.00000000000000000 ) ) ;
#8004 = FACE_OUTER_BOUND ( 'NONE', #22549, .T. ) ;
#8005 = CARTESIAN_POINT ( 'NONE',  ( 0.000000000000000000, 39.47590169984846398, 71.87247863392428826 ) ) ;
#8006 = CARTESIAN_POINT ( 'NONE',  ( -92.69370383062498320, -209.9999999999999716, 82.49906250086715431 ) ) ;
#8007 = SHAPE_REPRESENTATION_RELATIONSHIP ( 'NONE' , 'NONE' ,  #54059, #64162 ) ;
#8008 = DIRECTION ( 'NONE',  ( -1.000000000000000000, 0.000000000000000000, 0.000000000000000000 ) ) ;
#8009 = EDGE_CURVE ( 'NONE', #43566, #69008, #14492, .T. ) ;
#8010 = AXIS2_PLACEMENT_3D ( 'NONE', #27479, #49665, #72589 ) ;
#8011 = LINE ( 'NONE', #59150, #34599 ) ;
#8012 = CARTESIAN_POINT ( 'NONE',  ( -94.99999999999997158, -212.6630814284392557, 77.89531250086714920 ) ) ;
#8013 = CYLINDRICAL_SURFACE ( 'NONE', #62202, 32.00000000000000000 ) ;
#8014 = COLOUR_RGB ( '', 0.08235294, 0.09019608, 0.10196078) ;
#8015 = ORIENTED_EDGE ( 'NONE', *, *, #17175, .F. ) ;
#8016 = CARTESIAN_POINT ( 'NONE',  ( 0.000000000000000000, 12.93880638057426502, -76.41127070299258150 ) ) ;
#8017 = CARTESIAN_POINT ( 'NONE',  ( 100.0000000000000000, -214.9999999999999716, 90.00000000000000000 ) ) ;
#8018 = LINE ( 'NONE', #7649, #32962 ) ;
#8019 = AXIS2_PLACEMENT_3D ( 'NONE', #45717, #5856, #28765 ) ;
#8020 = CYLINDRICAL_SURFACE ( 'NONE', #72095, 82.00000000000000000 ) ;
#8021 = CARTESIAN_POINT ( 'NONE',  ( 97.30629616937498838, -208.6684592857803011, 74.77322916753379900 ) ) ;
#8022 = ORIENTED_EDGE ( 'NONE', *, *, #48358, .F. ) ;
#8023 = CARTESIAN_POINT ( 'NONE',  ( 10.00000000000000000, -9.188173127307003085, -40.98264845739760176 ) ) ;
#8024 = CIRCLE ( 'NONE', #5635, 31.99999999999998579 ) ;
#8025 = CARTESIAN_POINT ( 'NONE',  ( 10.00000000000000000, 41.19522573413731692, 65.64334221924924861 ) ) ;
#8026 = SURFACE_SIDE_STYLE ('',( #1692 ) ) ;
#8027 = ORIENTED_EDGE ( 'NONE', *, *, #50735, .T. ) ;
#8028 = DIRECTION ( 'NONE',  ( 0.000000000000000000, 0.000000000000000000, 1.000000000000000000 ) ) ;
#8029 = CIRCLE ( 'NONE', #63267, 31.99999999999999289 ) ;
#8030 = ORIENTED_EDGE ( 'NONE', *, *, #58555, .T. ) ;
#8031 = DIRECTION ( 'NONE',  ( -1.000000000000000000, 0.000000000000000000, -0.000000000000000000 ) ) ;
#8032 = AXIS2_PLACEMENT_3D ( 'NONE', #25424, #48714, #71258 ) ;
#8033 = VERTEX_POINT ( 'NONE', #55052 ) ;
#8034 = ORIENTED_EDGE ( 'NONE', *, *, #62481, .F. ) ;
#8035 = ORIENTED_EDGE ( 'NONE', *, *, #15515, .T. ) ;
#8036 = DIRECTION ( 'NONE',  ( -1.000000000000000000, -0.000000000000000000, -0.000000000000000000 ) ) ;
#8037 = AXIS2_PLACEMENT_3D ( 'NONE', #58333, #54183, #31232 ) ;
#8038 = ORIENTED_EDGE ( 'NONE', *, *, #53131, .T. ) ;
#8039 = ORIENTED_EDGE ( 'NONE', *, *, #9754, .F. ) ;
#8040 = CARTESIAN_POINT ( 'NONE',  ( 92.69370383062498320, 88.66845928578037217, 81.59947916753381492 ) ) ;
#8041 = DIRECTION ( 'NONE',  ( 0.000000000000000000, 0.000000000000000000, 1.000000000000000000 ) ) ;
#8042 = DIRECTION ( 'NONE',  ( -1.000000000000000000, 0.000000000000000000, 0.000000000000000000 ) ) ;
#8043 = ORIENTED_EDGE ( 'NONE', *, *, #8147, .T. ) ;
#8044 = ORIENTED_EDGE ( 'NONE', *, *, #16366, .F. ) ;
#8045 = ORIENTED_EDGE ( 'NONE', *, *, #70967, .F. ) ;
#8046 = CARTESIAN_POINT ( 'NONE',  ( 0.000000000000000000, -0.8299999999999999600, -1.199999999999999956 ) ) ;
#8047 = ORIENTED_EDGE ( 'NONE', *, *, #40923, .F. ) ;
#8048 = DIRECTION ( 'NONE',  ( 0.000000000000000000, 0.000000000000000000, 1.000000000000000000 ) ) ;
#8049 = LINE ( 'NONE', #53925, #5522 ) ;
#8050 = EDGE_CURVE ( 'NONE', #22100, #25604, #71592, .T. ) ;
#8051 = CARTESIAN_POINT ( 'NONE',  ( -96.01774234934310925, 92.19538700400588027, 74.85985921673510290 ) ) ;
#8052 = LINE ( 'NONE', #43764, #35302 ) ;
#8053 = CARTESIAN_POINT ( 'NONE',  ( 12.00000000000000000, -23.29833615347109088, -3.418703333116486665 ) ) ;
#8054 = EDGE_CURVE ( 'NONE', #42911, #12729, #57773, .T. ) ;
#8055 = LINE ( 'NONE', #52428, #42858 ) ;
#8056 = EDGE_CURVE ( 'NONE', #67503, #58433, #22451, .T. ) ;
#8057 = CARTESIAN_POINT ( 'NONE',  ( -97.64999999999996305, -209.9999999999999716, 75.47437500173430180 ) ) ;
#8058 = CARTESIAN_POINT ( 'NONE',  ( -96.15314808468752972, 91.99731107132950569, 87.79072916753381151 ) ) ;
#8060 = CARTESIAN_POINT ( 'NONE',  ( -92.35000000000003695, 90.00000000000004263, 75.15687500173430635 ) ) ;
#8059 = CARTESIAN_POINT ( 'NONE',  ( 93.67499999999999716, 87.70503267997126784, 76.21520833506762926 ) ) ;
#8061 = ORIENTED_EDGE ( 'NONE', *, *, #27146, .T. ) ;
#8062 = CARTESIAN_POINT ( 'NONE',  ( 93.84685191531248449, 91.99731107132950569, 77.63072916753381492 ) ) ;
#8063 = AXIS2_PLACEMENT_3D ( 'NONE', #67630, #4126, #39064 ) ;
#8064 = CARTESIAN_POINT ( 'NONE',  ( 5.999999999999999112, -40.65526001592663619, 71.21200624218782593 ) ) ;
#8065 = LINE ( 'NONE', #70840, #47513 ) ;
#8066 = CARTESIAN_POINT ( 'NONE',  ( 92.35000000046409241, -210.0000309672231253, 77.38038495127494798 ) ) ;
#8067 = CARTESIAN_POINT ( 'NONE',  ( -18.12185313557660038, -104.9634299478706794, 5.500000000000000000 ) ) ;
#8068 = AXIS2_PLACEMENT_3D ( 'NONE', #4109, #20637, #3738 ) ;
#8069 = LINE ( 'NONE', #70102, #7821 ) ;
#8070 = ORIENTED_EDGE ( 'NONE', *, *, #23754, .F. ) ;
#8071 = CARTESIAN_POINT ( 'NONE',  ( 5.999999999999999112, -74.74816331893404708, -33.71516098798818462 ) ) ;
#8072 = DIRECTION ( 'NONE',  ( 0.000000000000000000, 0.000000000000000000, 1.000000000000000000 ) ) ;
#8073 = EDGE_LOOP ( 'NONE', ( #2381, #39893, #39237, #7294 ) ) ;
#8074 = ORIENTED_EDGE ( 'NONE', *, *, #1235, .T. ) ;
#8075 = AXIS2_PLACEMENT_3D ( 'NONE', #6180, #70394, #29438 ) ;
#8076 = EDGE_CURVE ( 'NONE', #3438, #39181, #72131, .T. ) ;
#8077 = DIRECTION ( 'NONE',  ( -0.000000000000000000, -0.000000000000000000, 1.000000000000000000 ) ) ;
#8078 = PRODUCT_DEFINITION_SHAPE ( 'NONE', 'NONE',  #74378 ) ;
#8079 = DIRECTION ( 'NONE',  ( -0.000000000000000000, -0.000000000000000000, 1.000000000000000000 ) ) ;
#8080 = CARTESIAN_POINT ( 'NONE',  ( 11.99999999999999822, 15.33399622253482342, 80.55351364060595643 ) ) ;
#8081 = VECTOR ( 'NONE', #52300, 1000.000000000000000 ) ;
#8082 = DIRECTION ( 'NONE',  ( -0.000000000000000000, -0.000000000000000000, 1.000000000000000000 ) ) ;
#8083 = DIRECTION ( 'NONE',  ( 0.000000000000000000, 0.000000000000000000, 1.000000000000000000 ) ) ;
#8084 = CYLINDRICAL_SURFACE ( 'NONE', #38383, 31.99999999999998579 ) ;
#8085 = ORIENTED_EDGE ( 'NONE', *, *, #10342, .T. ) ;
#8086 = CARTESIAN_POINT ( 'NONE',  ( 0.000000000000000000, -33.00180498840060039, 17.80606268964528027 ) ) ;
#8087 = ADVANCED_FACE ( 'NONE', ( #8464 ), #31004, .T. ) ;
#8088 = EDGE_CURVE ( 'NONE', #29971, #48817, #43348, .T. ) ;
#8089 = PLANE ( 'NONE',  #1861 ) ;
#8090 = AXIS2_PLACEMENT_3D ( 'NONE', #67119, #62904, #11361 ) ;
#8091 = CARTESIAN_POINT ( 'NONE',  ( 10.00000000000000000, 0.000000000000000000, 0.000000000000000000 ) ) ;
#8092 = CARTESIAN_POINT ( 'NONE',  ( -94.99999999999997158, -209.9999999999999716, 90.00000000000000000 ) ) ;
#8093 = CARTESIAN_POINT ( 'NONE',  ( 0.000000000000000000, 60.67117009219216328, -55.16347631942977614 ) ) ;
#8094 = DIRECTION ( 'NONE',  ( 0.000000000000000000, 0.000000000000000000, 1.000000000000000000 ) ) ;
#8095 = CARTESIAN_POINT ( 'NONE',  ( -97.64999999996638280, -210.0000076551254722, 78.01464417100379478 ) ) ;
#8096 = AXIS2_PLACEMENT_3D ( 'NONE', #42087, #28655, #25520 ) ;
#8097 = DIRECTION ( 'NONE',  ( 0.000000000000000000, -0.000000000000000000, -1.000000000000000000 ) ) ;
#8098 = CARTESIAN_POINT ( 'NONE',  ( 93.84685191531248449, 88.00268892867053694, 85.46239583420047836 ) ) ;
#8099 = CARTESIAN_POINT ( 'NONE',  ( -97.30629616937497417, -211.3315407142195852, 86.67947916753382742 ) ) ;
#8100 = LINE ( 'NONE', #12625, #29004 ) ;
#8101 = ORIENTED_EDGE ( 'NONE', *, *, #19284, .T. ) ;
#8102 = DIRECTION ( 'NONE',  ( 1.000000000000000000, 0.000000000000000000, 0.000000000000000000 ) ) ;
#8103 = CARTESIAN_POINT ( 'NONE',  ( -97.64999999999994884, -211.5299782133524502, 81.16291666666666060 ) ) ;
#8104 = CARTESIAN_POINT ( 'NONE',  ( -96.15314808468752972, 91.99731107132950569, 74.93197916753379673 ) ) ;
#8105 = CARTESIAN_POINT ( 'NONE',  ( 93.84685191531251292, -211.9973110713294489, 85.30364583420046642 ) ) ;
#8106 = ORIENTED_EDGE ( 'NONE', *, *, #58163, .F. ) ;
#8107 = ORIENTED_EDGE ( 'NONE', *, *, #169, .F. ) ;
#8108 = AXIS2_PLACEMENT_3D ( 'NONE', #49502, #66079, #20929 ) ;
#8109 = ORIENTED_EDGE ( 'NONE', *, *, #65150, .F. ) ;
#8110 = VECTOR ( 'NONE', #62290, 1000.000000000000000 ) ;
#8111 = CARTESIAN_POINT ( 'NONE',  ( 10.00000000000000000, 0.000000000000000000, 0.000000000000000000 ) ) ;
#8112 = FACE_OUTER_BOUND ( 'NONE', #56803, .T. ) ;
#8113 = AXIS2_PLACEMENT_3D ( 'NONE', #58853, #45083, #30264 ) ;
#8114 = AXIS2_PLACEMENT_3D ( 'NONE', #7551, #46296, #69949 ) ;
#8115 = ORIENTED_EDGE ( 'NONE', *, *, #3410, .F. ) ;
#8116 = CYLINDRICAL_SURFACE ( 'NONE', #2420, 16.00000000000000000 ) ;
#8117 = CARTESIAN_POINT ( 'NONE',  ( 92.69370383062501162, -208.6684592857803295, 78.95364583420045790 ) ) ;
#8118 = CARTESIAN_POINT ( 'NONE',  ( 11.99999999999999822, -41.19522573413689059, -65.64334221924951862 ) ) ;
#8119 = LINE ( 'NONE', #25786, #66420 ) ;
#8120 = CARTESIAN_POINT ( 'NONE',  ( 6.000000000000000000, -2.543863470247820224, -81.96053171279903893 ) ) ;
#8121 = DIRECTION ( 'NONE',  ( 1.000000000000000000, 0.000000000000000000, 0.000000000000000000 ) ) ;
#8122 = DIRECTION ( 'NONE',  ( -0.000000000000000000, -0.000000000000000000, 1.000000000000000000 ) ) ;
#8123 = CARTESIAN_POINT ( 'NONE',  ( 93.67500000000001137, -212.2949673200287179, 82.48583333333333201 ) ) ;
#8124 = PRODUCT_DEFINITION ( 'UNKNOWN', '', #25592, #42407 ) ;
#8125 = EDGE_CURVE ( 'NONE', #39121, #67207, #54689, .T. ) ;
#8126 = ORIENTED_EDGE ( 'NONE', *, *, #35656, .T. ) ;
#8127 = VERTEX_POINT ( 'NONE', #15197 ) ;
#8128 = ORIENTED_EDGE ( 'NONE', *, *, #54812, .T. ) ;
#8129 = VERTEX_POINT ( 'NONE', #3215 ) ;
#8130 = CARTESIAN_POINT ( 'NONE',  ( 10.00000000000000000, -10.74501242461308159, 35.92658777277507909 ) ) ;
#8131 = AXIS2_PLACEMENT_3D ( 'NONE', #40494, #1057, #40876 ) ;
#8132 = CARTESIAN_POINT ( 'NONE',  ( -92.69370383062504004, 90.00000000000004263, 84.40406250086715545 ) ) ;
#8133 = EDGE_CURVE ( 'NONE', #10016, #42721, #4921, .T. ) ;
#8134 = CARTESIAN_POINT ( 'NONE',  ( 97.64999017507810208, 88.47001611422622602, 88.43895794268868826 ) ) ;
#8135 = AXIS2_PLACEMENT_3D ( 'NONE', #57445, #68737, #16860 ) ;
#8136 = DIRECTION ( 'NONE',  ( 0.000000000000000000, 0.000000000000000000, 1.000000000000000000 ) ) ;
#8137 = CARTESIAN_POINT ( 'NONE',  ( 92.34999999999999432, 88.47002178664753558, 75.44791666666667140 ) ) ;
#8138 = AXIS2_PLACEMENT_3D ( 'NONE', #16732, #10336, #33255 ) ;
#8140 = ORIENTED_EDGE ( 'NONE', *, *, #49494, .F. ) ;
#8139 = EDGE_CURVE ( 'NONE', #42336, #55165, #10912, .T. ) ;
#8141 = CARTESIAN_POINT ( 'NONE',  ( -93.67499999999998295, -207.7050326799711968, 87.32770833506762642 ) ) ;
#8142 = ORIENTED_EDGE ( 'NONE', *, *, #16455, .T. ) ;
#8143 = CARTESIAN_POINT ( 'NONE',  ( -3.000000000000000000, 22.07842321921492612, -8.187992925817130896 ) ) ;
#8144 = ORIENTED_EDGE ( 'NONE', *, *, #24462, .T. ) ;
#8145 = CARTESIAN_POINT ( 'NONE',  ( -95.00000000000002842, 86.94004357329504273, 86.42812500173430124 ) ) ;
#8146 = CIRCLE ( 'NONE', #26172, 16.00000000000000355 ) ;
#8147 = EDGE_CURVE ( 'NONE', #12223, #6773, #38134, .T. ) ;
#8148 = CARTESIAN_POINT ( 'NONE',  ( 93.84685191531248449, 88.00268892867053694, 88.00239583420048461 ) ) ;
#8149 = CARTESIAN_POINT ( 'NONE',  ( -1.459549131277904976, -119.6539995182286304, -2.500000000000000000 ) ) ;
#8150 = CARTESIAN_POINT ( 'NONE',  ( -95.00000000000002842, 90.00000000000004263, 90.00000000000000000 ) ) ;
#8151 = CARTESIAN_POINT ( 'NONE',  ( -3.360000000000002096, 0.000000000000000000, 0.000000000000000000 ) ) ;
#8152 = CARTESIAN_POINT ( 'NONE',  ( 22.94323693612312809, -114.6983135802921083, 5.500000000000000000 ) ) ;
#8153 = ORIENTED_EDGE ( 'NONE', *, *, #73381, .F. ) ;
#8154 = LINE ( 'NONE', #54033, #9886 ) ;
#8155 = CARTESIAN_POINT ( 'NONE',  ( -97.30629616937495996, -209.9999999999999716, 75.67281250086713840 ) ) ;
#8156 = ORIENTED_EDGE ( 'NONE', *, *, #46962, .F. ) ;
#8157 = VERTEX_POINT ( 'NONE', #20841 ) ;
#8158 = LINE ( 'NONE', #31087, #54189 ) ;
#8159 = EDGE_CURVE ( 'NONE', #64024, #20082, #24123, .T. ) ;
#8160 = ADVANCED_FACE ( 'NONE', ( #66354 ), #65240, .T. ) ;
#8161 = CARTESIAN_POINT ( 'NONE',  ( 10.00000000000000000, -39.04073710021356192, 15.48615015657568250 ) ) ;
#8162 = DIRECTION ( 'NONE',  ( -0.000000000000000000, -0.000000000000000000, -1.000000000000000000 ) ) ;
#8163 =( BOUNDED_CURVE ( )  B_SPLINE_CURVE ( 2, ( #74048, #57152, #68436, #6389, #52597, #16926, #1151 ),
 .UNSPECIFIED., .F., .F. ) 
 B_SPLINE_CURVE_WITH_KNOTS ( ( 3, 2, 2, 3 ),
 ( 0.5926843883797353607, 0.5997400709749998171, 0.6067958365158829803, 0.6138516023186938453 ),
 .UNSPECIFIED. ) 
 CURVE ( )  GEOMETRIC_REPRESENTATION_ITEM ( )  RATIONAL_B_SPLINE_CURVE ( ( 0.9999968501007930888, 0.8660269787525570750, 1.000000000000000000, 0.8660254037844387076, 1.000000000000000000, 0.8660254037844387076, 1.000000000000000000 ) ) 
 REPRESENTATION_ITEM ( '' )  );
#8164 = CARTESIAN_POINT ( 'NONE',  ( -97.30629616937497417, -208.6684592857803011, 84.03364583420049883 ) ) ;
#8165 = VERTEX_POINT ( 'NONE', #55429 ) ;
#8166 = CIRCLE ( 'NONE', #9338, 12.49999999999999645 ) ;
#8167 = ORIENTED_EDGE ( 'NONE', *, *, #19948, .F. ) ;
#8168 = AXIS2_PLACEMENT_3D ( 'NONE', #56179, #21585, #67833 ) ;
#8169 = ORIENTED_EDGE ( 'NONE', *, *, #34640, .T. ) ;
#8170 = DIRECTION ( 'NONE',  ( -1.000000000000000000, -0.000000000000000000, 0.000000000000000000 ) ) ;
#8171 = CARTESIAN_POINT ( 'NONE',  ( 97.30629616937498838, 88.66845928578037217, 88.79614583420050167 ) ) ;
#8172 = AXIS2_PLACEMENT_3D ( 'NONE', #54600, #7993, #8371 ) ;
#8173 = CARTESIAN_POINT ( 'NONE',  ( 0.000000000000000000, -75.11764819372145041, -2.946379043147127064 ) ) ;
#8174 = CARTESIAN_POINT ( 'NONE',  ( 92.69370383062498320, 91.33154071421968467, 81.33489583420048064 ) ) ;
#8175 = CIRCLE ( 'NONE', #23803, 16.00000000000000000 ) ;
#8176 = CARTESIAN_POINT ( 'NONE',  ( -31.74999999999995737, 3.673940397442060854E-16, -3.000000000000000888 ) ) ;
#8177 = DIRECTION ( 'NONE',  ( 1.000000000000000000, 0.000000000000000000, 0.000000000000000000 ) ) ;
#8178 = CARTESIAN_POINT ( 'NONE',  ( 0.000000000000000000, 0.000000000000000000, 0.000000000000000000 ) ) ;
#8179 = DIRECTION ( 'NONE',  ( -1.000000000000000000, 0.000000000000000000, -0.000000000000000000 ) ) ;
#8180 = CARTESIAN_POINT ( 'NONE',  ( -96.32500000000001705, 87.70503267997129626, 76.85020833506763438 ) ) ;
#8181 = DIRECTION ( 'NONE',  ( 0.9781476007338070211, 2.546183866652749098E-17, 0.2079116908177526257 ) ) ;
#8182 = CARTESIAN_POINT ( 'NONE',  ( -93.07889023459847522, -208.6943671794269335, 74.79348190356851944 ) ) ;
#8183 = CARTESIAN_POINT ( 'NONE',  ( 12.50000000000000000, -107.5000000000000000, -40.00000000000000000 ) ) ;
#8184 = ORIENTED_EDGE ( 'NONE', *, *, #25650, .F. ) ;
#8185 = CARTESIAN_POINT ( 'NONE',  ( -97.30629616937501680, 90.00000000000004263, 86.46781250086714010 ) ) ;
#8186 = CARTESIAN_POINT ( 'NONE',  ( 10.00000000000000000, 11.30684508768339569, 76.66974797899841576 ) ) ;
#8187 = VECTOR ( 'NONE', #67317, 1000.000000000000000 ) ;
#8188 = VECTOR ( 'NONE', #27281, 1000.000000000000000 ) ;
#8189 = AXIS2_PLACEMENT_3D ( 'NONE', #59544, #8031, #30949 ) ;
#8190 = DIRECTION ( 'NONE',  ( -0.000000000000000000, -0.000000000000000000, 1.000000000000000000 ) ) ;
#8191 = ORIENTED_EDGE ( 'NONE', *, *, #33334, .T. ) ;
#8192 = VECTOR ( 'NONE', #19752, 1000.000000000000000 ) ;
#8193 = CARTESIAN_POINT ( 'NONE',  ( 92.35000000000000853, -209.9999999999999716, 83.65000000000000568 ) ) ;
#8194 = LINE ( 'NONE', #24026, #21549 ) ;
#8195 = DIRECTION ( 'NONE',  ( 0.000000000000000000, -0.8090169943749530024, 0.5877852522924653655 ) ) ;
#8196 = EDGE_CURVE ( 'NONE', #27575, #37462, #19322, .T. ) ;
#8197 = CARTESIAN_POINT ( 'NONE',  ( 92.69370383062501162, -211.3315407142195852, 81.59947916753381492 ) ) ;
#8198 = ORIENTED_EDGE ( 'NONE', *, *, #23597, .F. ) ;
#8199 = EDGE_CURVE ( 'NONE', #42329, #53520, #21956, .T. ) ;
#8200 = ORIENTED_EDGE ( 'NONE', *, *, #25986, .F. ) ;
#8201 = EDGE_CURVE ( 'NONE', #46993, #40794, #62187, .T. ) ;
#8202 = CARTESIAN_POINT ( 'NONE',  ( 95.00000000000000000, -209.9999999999999716, 90.00000000000000000 ) ) ;
#8203 = VERTEX_POINT ( 'NONE', #39998 ) ;
#8204 = DIRECTION ( 'NONE',  ( -1.000000000000000000, -0.000000000000000000, 0.000000000000000000 ) ) ;
#8205 = DIRECTION ( 'NONE',  ( 1.000000000000000000, 0.000000000000000000, 0.000000000000000000 ) ) ;
#8206 = MECHANICAL_DESIGN_GEOMETRIC_PRESENTATION_REPRESENTATION (  '', ( #28606 ), #6985 ) ;
#8207 = ORIENTED_EDGE ( 'NONE', *, *, #60885, .T. ) ;
#8208 = PLANE ( 'NONE',  #47744 ) ;
#8209 = CARTESIAN_POINT ( 'NONE',  ( 93.84685191531251292, -211.9973110713294489, 75.93739583420048689 ) ) ;
#8210 = AXIS2_PLACEMENT_3D ( 'NONE', #64055, #18900, #41846 ) ;
#8211 = AXIS2_PLACEMENT_3D ( 'NONE', #63966, #35380, #22622 ) ;
#8212 = EDGE_CURVE ( 'NONE', #42545, #51073, #21576, .T. ) ;
#8213 = VERTEX_POINT ( 'NONE', #45276 ) ;
#8214 = CARTESIAN_POINT ( 'NONE',  ( 6.000000000000000000, 15.33399622253601002, -80.55351364060572905 ) ) ;
#8215 = ORIENTED_EDGE ( 'NONE', *, *, #31126, .T. ) ;
#8216 = VERTEX_POINT ( 'NONE', #27595 ) ;
#8217 = FACE_OUTER_BOUND ( 'NONE', #586, .T. ) ;
#8218 = AXIS2_PLACEMENT_3D ( 'NONE', #5705, #41020, #40641 ) ;
#8219 = CARTESIAN_POINT ( 'NONE',  ( 10.00000000000000000, -77.32052557432845674, 5.256550761632577284 ) ) ;
#8220 = VECTOR ( 'NONE', #116, 1000.000000000000000 ) ;
#8221 = ORIENTED_EDGE ( 'NONE', *, *, #35465, .F. ) ;
#8222 = DIRECTION ( 'NONE',  ( 0.000000000000000000, -0.9876883405951393247, 0.1564344650402204329 ) ) ;
#8223 = CARTESIAN_POINT ( 'NONE',  ( 95.00000000000000000, -213.0599564267049857, 83.25312500173430408 ) ) ;
#8224 = CARTESIAN_POINT ( 'NONE',  ( 94.99999999999998579, 86.94004357329500010, 85.71374999999997613 ) ) ;
#8225 = ORIENTED_EDGE ( 'NONE', *, *, #32602, .T. ) ;
#8226 = DIRECTION ( 'NONE',  ( -1.000000000000000000, 0.000000000000000000, 0.000000000000000000 ) ) ;
#8227 = DIRECTION ( 'NONE',  ( -1.000000000000000000, 0.000000000000000000, -0.000000000000000000 ) ) ;
#8228 = ORIENTED_EDGE ( 'NONE', *, *, #43906, .T. ) ;
#8229 = ORIENTED_EDGE ( 'NONE', *, *, #54100, .F. ) ;
#8230 = CARTESIAN_POINT ( 'NONE',  ( -92.69370383062505425, 88.66845928578038638, 88.79614583420048746 ) ) ;
#8231 = ADVANCED_FACE ( 'NONE', ( #44531 ), #22715, .T. ) ;
#8232 = CARTESIAN_POINT ( 'NONE',  ( 96.15314808468748708, 88.00268892867053694, 80.32947916753380468 ) ) ;
#8233 = VERTEX_POINT ( 'NONE', #51262 ) ;
#8234 = CARTESIAN_POINT ( 'NONE',  ( 93.67499999999998295, 92.29496732002878900, 82.35354166840096468 ) ) ;
#8235 = CIRCLE ( 'NONE', #70634, 31.99999999999999645 ) ;
#8236 = PLANE ( 'NONE',  #73264 ) ;
#8237 = ORIENTED_EDGE ( 'NONE', *, *, #10674, .F. ) ;
#8238 = FACE_BOUND ( 'NONE', #3264, .T. ) ;
#8239 = ORIENTED_EDGE ( 'NONE', *, *, #11386, .T. ) ;
#8240 = ORIENTED_EDGE ( 'NONE', *, *, #9193, .T. ) ;
#8241 = ORIENTED_EDGE ( 'NONE', *, *, #72901, .T. ) ;
#8242 = CARTESIAN_POINT ( 'NONE',  ( -0.0004442498525516064278, 0.001194404164626844313, -85.60000000000000853 ) ) ;
#8243 = FACE_OUTER_BOUND ( 'NONE', #4184, .T. ) ;
#8244 = CIRCLE ( 'NONE', #21427, 3.300000000000000711 ) ;
#8245 = CIRCLE ( 'NONE', #43094, 15.70000000000326956 ) ;
#8246 = CARTESIAN_POINT ( 'NONE',  ( -92.35000000000005116, 88.47002178664754979, 83.27958333333333485 ) ) ;
#8247 = EDGE_CURVE ( 'NONE', #61501, #52056, #28937, .T. ) ;
#8248 = VERTEX_POINT ( 'NONE', #62955 ) ;
#8249 = EDGE_CURVE ( 'NONE', #48511, #46834, #32968, .T. ) ;
#8250 = DIRECTION ( 'NONE',  ( -1.000000000000000000, 0.000000000000000000, 0.000000000000000000 ) ) ;
#8251 = AXIS2_PLACEMENT_3D ( 'NONE', #51672, #52032, #51294 ) ;
#8252 = CARTESIAN_POINT ( 'NONE',  ( 0.000000000000000000, 0.000000000000000000, 0.000000000000000000 ) ) ;
#8253 = ORIENTED_EDGE ( 'NONE', *, *, #9944, .F. ) ;
#8254 = CARTESIAN_POINT ( 'NONE',  ( 10.00000000000000000, 24.73286445877808148, -73.44644590900034586 ) ) ;
#8255 = CARTESIAN_POINT ( 'NONE',  ( -93.84685191531247028, -211.9973110713294489, 82.23447916753380582 ) ) ;
#8256 = VERTEX_POINT ( 'NONE', #5798 ) ;
#8257 = EDGE_CURVE ( 'NONE', #17105, #23233, #2533, .T. ) ;
#8258 = CARTESIAN_POINT ( 'NONE',  ( 10.00000000000000000, -10.96151621346514382, 35.95386929396252640 ) ) ;
#8259 = CARTESIAN_POINT ( 'NONE',  ( 10.00000000000000000, -73.72996012237449293, 14.67089635893687571 ) ) ;
#8260 = LINE ( 'NONE', #36826, #74126 ) ;
#8261 = CARTESIAN_POINT ( 'NONE',  ( 10.00000000000000000, -74.74816331893404708, -33.71516098798818462 ) ) ;
#8262 = FACE_OUTER_BOUND ( 'NONE', #72015, .T. ) ;
#8263 = LINE ( 'NONE', #25553, #33730 ) ;
#8264 = FACE_OUTER_BOUND ( 'NONE', #41793, .T. ) ;
#8265 = CARTESIAN_POINT ( 'NONE',  ( -11.59517495878806947, -96.12423995607481686, 5.500000000000000000 ) ) ;
#8266 = CARTESIAN_POINT ( 'NONE',  ( 10.00000000000000000, 6.736453364083557105, 36.88895765772635826 ) ) ;
#8267 = DIRECTION ( 'NONE',  ( -1.000000000000000000, 0.000000000000000000, 0.000000000000000000 ) ) ;
#8268 = AXIS2_PLACEMENT_3D ( 'NONE', #31630, #67334, #50403 ) ;
#8269 = CARTESIAN_POINT ( 'NONE',  ( -93.84685191531254134, 91.99731107132950569, 74.82614583420047438 ) ) ;
#8270 = CARTESIAN_POINT ( 'NONE',  ( 10.00000000000000000, -31.47745569255092235, -68.26794271651296242 ) ) ;
#8271 = CARTESIAN_POINT ( 'NONE',  ( -1.499592026101402853, -119.9650177866181764, 2.500000000000000000 ) ) ;
#8272 = DIRECTION ( 'NONE',  ( 1.000000000000000000, 7.705842312278612278E-15, -2.603472992745757322E-14 ) ) ;
#8273 = UNCERTAINTY_MEASURE_WITH_UNIT (LENGTH_MEASURE( 1.000000000000000082E-05 ), #17270, 'distance_accuracy_value', 'NONE');
#8274 = VECTOR ( 'NONE', #74247, 1000.000000000000114 ) ;
#8275 = CARTESIAN_POINT ( 'NONE',  ( 10.00000000000000000, 46.53671651294032330, -59.03961581697353012 ) ) ;
#8276 = AXIS2_PLACEMENT_3D ( 'NONE', #29470, #958, #58427 ) ;
#8277 = CIRCLE ( 'NONE', #34675, 82.00000000000000000 ) ;
#8278 = DIRECTION ( 'NONE',  ( 0.7950889364178788110, -0.6064928550163524168, 0.000000000000000000 ) ) ;
#8279 = DIRECTION ( 'NONE',  ( -0.5200609990133016058, -0.8541291221503261033, 0.000000000000000000 ) ) ;
#8281 = CIRCLE ( 'NONE', #46716, 2.650000000000540812 ) ;
#8280 = DIRECTION ( 'NONE',  ( -1.000000000000000000, 0.000000000000000000, 0.000000000000000000 ) ) ;
#8282 = DIRECTION ( 'NONE',  ( -1.000000000000000000, 0.000000000000000000, 0.000000000000000000 ) ) ;
#8283 = CARTESIAN_POINT ( 'NONE',  ( 97.64999999999821512, 90.00000306648260562, 75.79187510780352000 ) ) ;
#8284 = CARTESIAN_POINT ( 'NONE',  ( -97.64999999999994884, -211.5299782133524502, 89.41791666666667027 ) ) ;
#8285 = AXIS2_PLACEMENT_3D ( 'NONE', #22170, #73285, #56004 ) ;
#8286 = DIRECTION ( 'NONE',  ( 0.000000000000000000, 0.000000000000000000, 1.000000000000000000 ) ) ;
#8287 = VERTEX_POINT ( 'NONE', #39259 ) ;
#8288 = DIRECTION ( 'NONE',  ( -0.000000000000000000, -0.000000000000000000, 1.000000000000000000 ) ) ;
#8289 = DIRECTION ( 'NONE',  ( 0.5687579148473765889, -0.8225049752423776450, 0.000000000000000000 ) ) ;
#8291 = DIRECTION ( 'NONE',  ( 1.000000000000000000, 1.427937372958405461E-15, 7.962523111839130290E-16 ) ) ;
#8290 = CIRCLE ( 'NONE', #14298, 77.49899999999999523 ) ;
#8292 = DIRECTION ( 'NONE',  ( 0.000000000000000000, -0.4999999999999920064, -0.8660254037844432595 ) ) ;
#8293 = CIRCLE ( 'NONE', #26260, 3.000000000000000000 ) ;
#8294 = EDGE_CURVE ( 'NONE', #38969, #45116, #50524, .T. ) ;
#8295 = CIRCLE ( 'NONE', #28693, 77.49899999999999523 ) ;
#8296 = AXIS2_PLACEMENT_3D ( 'NONE', #54037, #2571, #25454 ) ;
#8297 = ADVANCED_FACE ( 'NONE', ( #33600 ), #57284, .T. ) ;
#8298 = VERTEX_POINT ( 'NONE', #28704 ) ;
#8299 = AXIS2_PLACEMENT_3D ( 'NONE', #57497, #33815, #22544 ) ;
#8301 = ADVANCED_FACE ( 'NONE', ( #67824, #11057 ), #56559, .T. ) ;
#8300 = DIRECTION ( 'NONE',  ( 0.000000000000000000, 0.000000000000000000, -1.000000000000000000 ) ) ;
#8302 = CARTESIAN_POINT ( 'NONE',  ( 0.000000000000000000, 62.20884554314020676, 46.21855187248652896 ) ) ;
#8303 = ORIENTED_EDGE ( 'NONE', *, *, #13057, .T. ) ;
#8304 = CIRCLE ( 'NONE', #29748, 77.49899999999999523 ) ;
#8305 = CARTESIAN_POINT ( 'NONE',  ( 95.00000000000000000, -207.3369185715606307, 81.22906250086714408 ) ) ;
#8306 = CARTESIAN_POINT ( 'NONE',  ( 97.30629616937498838, -211.3315407142195852, 86.89114583420048632 ) ) ;
#8307 = EDGE_LOOP ( 'NONE', ( #58591, #40606, #46771, #46162 ) ) ;
#8308 = CARTESIAN_POINT ( 'NONE',  ( -92.35000000000003695, 90.00000000000004263, 79.52249999999999375 ) ) ;
#8309 = EDGE_CURVE ( 'NONE', #51433, #55666, #51642, .T. ) ;
#8310 = ORIENTED_EDGE ( 'NONE', *, *, #60357, .T. ) ;
#8311 = FACE_BOUND ( 'NONE', #11345, .T. ) ;
#8312 = ORIENTED_EDGE ( 'NONE', *, *, #10796, .T. ) ;
#8313 = CARTESIAN_POINT ( 'NONE',  ( -96.15314808468752972, 91.99731107132950569, 75.72572916753382799 ) ) ;
#8314 = ORIENTED_EDGE ( 'NONE', *, *, #54736, .T. ) ;
#8315 = VERTEX_POINT ( 'NONE', #22333 ) ;
#8316 = CARTESIAN_POINT ( 'NONE',  ( -94.99999999999997158, -213.0599564267049857, 87.69812500173429726 ) ) ;
#8317 = ORIENTED_EDGE ( 'NONE', *, *, #71639, .T. ) ;
#8318 = CARTESIAN_POINT ( 'NONE',  ( 10.00000000000000000, 0.000000000000000000, 0.000000000000000000 ) ) ;
#8319 = DIRECTION ( 'NONE',  ( 0.000000000000000000, -0.9510565162951500895, -0.3090169943749583314 ) ) ;
#8320 = EDGE_LOOP ( 'NONE', ( #61757, #32515, #16543, #19046 ) ) ;
#8321 = FACE_OUTER_BOUND ( 'NONE', #28925, .T. ) ;
#8322 = ORIENTED_EDGE ( 'NONE', *, *, #10250, .T. ) ;
#8323 = CARTESIAN_POINT ( 'NONE',  ( 95.00000000000000000, -213.0599564267049857, 86.34874999999999545 ) ) ;
#8324 = VECTOR ( 'NONE', #53837, 1000.000000000000114 ) ;
#8325 = EDGE_CURVE ( 'NONE', #31594, #25082, #1353, .T. ) ;
#8326 = AXIS2_PLACEMENT_3D ( 'NONE', #66665, #62139, #44487 ) ;
#8327 = VERTEX_POINT ( 'NONE', #192 ) ;
#8328 = VECTOR ( 'NONE', #4058, 1000.000000000000000 ) ;
#8329 = CIRCLE ( 'NONE', #24017, 31.99999999999998934 ) ;
#8330 = ORIENTED_EDGE ( 'NONE', *, *, #16530, .F. ) ;
#8331 = ORIENTED_EDGE ( 'NONE', *, *, #55262, .T. ) ;
#8332 = CARTESIAN_POINT ( 'NONE',  ( 97.30629616937498838, -211.3315407142195852, 79.74739583420047495 ) ) ;
#8333 = CARTESIAN_POINT ( 'NONE',  ( -7.670864526094549163, -97.73662565058241114, 5.500000000000000000 ) ) ;
#8334 = CONTEXT_DEPENDENT_SHAPE_REPRESENTATION ( #23933, #19926 ) ;
#8335 = DIRECTION ( 'NONE',  ( 0.000000000000000000, -0.9510565162951566398, 0.3090169943749381809 ) ) ;
#8336 = VERTEX_POINT ( 'NONE', #27204 ) ;
#8337 = CARTESIAN_POINT ( 'NONE',  ( 92.35000000000000853, -209.9999999999999716, 90.00000000000000000 ) ) ;
#8338 = ORIENTED_EDGE ( 'NONE', *, *, #66073, .T. ) ;
#8339 = CARTESIAN_POINT ( 'NONE',  ( 10.00000000000000000, 0.000000000000000000, 0.000000000000000000 ) ) ;
#8340 = CARTESIAN_POINT ( 'NONE',  ( 0.000000000000000000, 71.87247863392471459, -39.47590169984770370 ) ) ;
#8341 = DIRECTION ( 'NONE',  ( 0.000000000000000000, 0.9876883405951372152, 0.1564344650402347547 ) ) ;
#8342 = DIRECTION ( 'NONE',  ( -1.000000000000000000, 0.000000000000000000, 0.000000000000000000 ) ) ;
#8343 = CARTESIAN_POINT ( 'NONE',  ( -93.84685191531248449, -208.0026889286704943, 80.54114583420046358 ) ) ;
#8344 = CARTESIAN_POINT ( 'NONE',  ( -92.69370383062502583, 88.66845928578038638, 78.00114583420049996 ) ) ;
#8345 = EDGE_CURVE ( 'NONE', #12034, #17937, #50513, .T. ) ;
#8346 = EDGE_LOOP ( 'NONE', ( #14630, #70144 ) ) ;
#8347 = EDGE_CURVE ( 'NONE', #27953, #70455, #53190, .T. ) ;
#8348 = CARTESIAN_POINT ( 'NONE',  ( 93.84685191531248449, 91.99731107132950569, 80.64697916753381435 ) ) ;
#8349 = VERTEX_POINT ( 'NONE', #13265 ) ;
#8350 = PLANE ( 'NONE',  #7090 ) ;
#8351 = CARTESIAN_POINT ( 'NONE',  ( -11.99999999999999645, 0.000000000000000000, 0.000000000000000000 ) ) ;
#8352 = CARTESIAN_POINT ( 'NONE',  ( 10.00000000000000000, 27.05870788708231700, 26.08949754953034272 ) ) ;
#8353 = FACE_OUTER_BOUND ( 'NONE', #22657, .T. ) ;
#8354 = CARTESIAN_POINT ( 'NONE',  ( 0.000000000000000000, -23.29833615347109443, 3.418703333116492438 ) ) ;
#8355 = CARTESIAN_POINT ( 'NONE',  ( -93.84685191531247028, -211.9973110713294489, 82.23447916753380582 ) ) ;
#8356 = AXIS2_PLACEMENT_3D ( 'NONE', #46183, #45828, #57837 ) ;
#8357 = B_SPLINE_CURVE_WITH_KNOTS ( 'NONE', 3,
 ( #73987, #45819, #68742, #18327, #354, #23245 ),
 .UNSPECIFIED., .F., .F.,
 ( 4, 2, 4 ),
 ( 0.005150343764683549923, 0.006610526168996381374, 0.008070708573309213693 ),
 .UNSPECIFIED. ) ;
#8358 = CARTESIAN_POINT ( 'NONE',  ( 96.32499999999998863, 87.70503267997126784, 87.03666666666666174 ) ) ;
#8359 = DIRECTION ( 'NONE',  ( -1.000000000000000000, 0.000000000000000000, -0.000000000000000000 ) ) ;
#8360 = DIRECTION ( 'NONE',  ( -1.000000000000000000, -0.000000000000000000, 0.000000000000000000 ) ) ;
#8361 = EDGE_LOOP ( 'NONE', ( #56133, #2202, #35775, #25883 ) ) ;
#8362 = AXIS2_PLACEMENT_3D ( 'NONE', #23872, #63737, #5854 ) ;
#8363 = CIRCLE ( 'NONE', #40838, 2.649999999999985700 ) ;
#8364 = ORIENTED_EDGE ( 'NONE', *, *, #3862, .T. ) ;
#8365 = DIRECTION ( 'NONE',  ( 1.000000000000000000, 0.000000000000000000, 0.000000000000000000 ) ) ;
#8366 = CIRCLE ( 'NONE', #41964, 82.00000000000000000 ) ;
#8367 = VECTOR ( 'NONE', #47323, 1000.000000000000000 ) ;
#8368 = CARTESIAN_POINT ( 'NONE',  ( -95.00000000000002842, 93.05995642670501411, 75.87125000000000341 ) ) ;
#8369 = DIRECTION ( 'NONE',  ( 0.000000000000000000, 0.000000000000000000, -1.000000000000000000 ) ) ;
#8370 = CARTESIAN_POINT ( 'NONE',  ( -95.00000000000002842, 92.66308142843932671, 85.67406250086715147 ) ) ;
#8371 = DIRECTION ( 'NONE',  ( 0.000000000000000000, 0.9510565162951544194, -0.3090169943749446757 ) ) ;
#8372 = DIRECTION ( 'NONE',  ( 0.000000000000000000, -0.07845909572785234043, 0.9969173337331274087 ) ) ;
#8373 = CARTESIAN_POINT ( 'NONE',  ( 15.00000000000000000, 18.84667830672605859, 18.68964196561243796 ) ) ;
#8374 = VERTEX_POINT ( 'NONE', #57664 ) ;
#8375 = CARTESIAN_POINT ( 'NONE',  ( 11.99999999999999822, -63.18004540532995605, -44.88180994100445531 ) ) ;
#8376 = DIRECTION ( 'NONE',  ( 0.000000000000000000, 0.000000000000000000, 1.000000000000000000 ) ) ;
#8377 = CARTESIAN_POINT ( 'NONE',  ( 0.000000000000000000, -89.50000000000000000, 5.500000000000000000 ) ) ;
#8378 = DIRECTION ( 'NONE',  ( -0.000000000000000000, -0.000000000000000000, 1.000000000000000000 ) ) ;
#8379 = LINE ( 'NONE', #4896, #3764 ) ;
#8380 = DIRECTION ( 'NONE',  ( -1.000000000000000000, 0.000000000000000000, -0.000000000000000000 ) ) ;
#8381 = CARTESIAN_POINT ( 'NONE',  ( -93.84685191531248449, -208.0026889286704943, 81.33489583420049485 ) ) ;
#8382 = DIRECTION ( 'NONE',  ( 0.000000000000000000, 0.000000000000000000, 1.000000000000000000 ) ) ;
#8383 = ADVANCED_FACE ( 'NONE', ( #41837 ), #29803, .T. ) ;
#8384 =( BOUNDED_CURVE ( )  B_SPLINE_CURVE ( 2, ( #17450, #67847, #17088, #40378, #63330, #11792, #29088, #73096, #38905, #61842, #10325 ),
 .UNSPECIFIED., .F., .F. ) 
 B_SPLINE_CURVE_WITH_KNOTS ( ( 3, 2, 2, 2, 2, 3 ),
 ( 0.6985206468843491168, 0.6985207885473545542, 0.7055765540882368292, 0.7126323196291192152, 0.7196880851700017123, 0.7196881748034549275 ),
 .UNSPECIFIED. ) 
 CURVE ( )  GEOMETRIC_REPRESENTATION_ITEM ( )  RATIONAL_B_SPLINE_CURVE ( ( 0.9999946203249591159, 0.9999973101084729254, 1.000000000000000000, 0.8660254037844387076, 1.000000000000000000, 0.8660254037844387076, 1.000000000000000000, 0.8660254037844387076, 1.000000000000000000, 0.9999982980435457858, 0.9999965961303334261 ) ) 
 REPRESENTATION_ITEM ( '' )  );
#8385 = FACE_OUTER_BOUND ( 'NONE', #41620, .T. ) ;
#8386 = CIRCLE ( 'NONE', #19169, 31.99999999999998224 ) ;
#8387 = EDGE_CURVE ( 'NONE', #305, #11760, #53492, .T. ) ;
#8388 = CARTESIAN_POINT ( 'NONE',  ( 10.00000000000000000, 33.79645857604513992, 16.45098606841138178 ) ) ;
#8389 = CARTESIAN_POINT ( 'NONE',  ( -92.35000000000003695, 90.00000000000004263, 89.04749999999999943 ) ) ;
#8390 = ORIENTED_EDGE ( 'NONE', *, *, #30286, .F. ) ;
#8391 = CARTESIAN_POINT ( 'NONE',  ( -97.64999999996715019, 90.00000839192523472, 86.90410584365564262 ) ) ;
#8392 = DIRECTION ( 'NONE',  ( 1.000000000000000000, 0.000000000000000000, 0.000000000000000000 ) ) ;
#8393 = CIRCLE ( 'NONE', #50392, 13.10000000000023590 ) ;
#8394 = CARTESIAN_POINT ( 'NONE',  ( 10.00000000000000000, -68.26794271651286294, 31.47745569255117104 ) ) ;
#8395 = EDGE_CURVE ( 'NONE', #17551, #40700, #70026, .T. ) ;
#8396 = AXIS2_PLACEMENT_3D ( 'NONE', #44658, #9684, #67573 ) ;
#8397 = EDGE_CURVE ( 'NONE', #70426, #43951, #68567, .T. ) ;
#8398 = CYLINDRICAL_SURFACE ( 'NONE', #10889, 77.49899999999999523 ) ;
#8399 = CARTESIAN_POINT ( 'NONE',  ( 97.30629616937498838, -209.9999999999999716, 89.48406250086715374 ) ) ;
#8400 = ORIENTED_EDGE ( 'NONE', *, *, #43161, .F. ) ;
#8401 = CARTESIAN_POINT ( 'NONE',  ( 10.00000000000000000, 0.000000000000000000, 0.000000000000000000 ) ) ;
#8402 = ORIENTED_EDGE ( 'NONE', *, *, #12589, .T. ) ;
#8403 =( BOUNDED_CURVE ( )  B_SPLINE_CURVE ( 2, ( #71852, #43326, #14721 ),
 .UNSPECIFIED., .F., .F. ) 
 B_SPLINE_CURVE_WITH_KNOTS ( ( 3, 3 ),
 ( 0.000000000000000000, 2.334341054542201936E-05 ),
 .UNSPECIFIED. ) 
 CURVE ( )  GEOMETRIC_REPRESENTATION_ITEM ( )  RATIONAL_B_SPLINE_CURVE ( ( 0.9459494467533910989, 0.9464399322878964682, 0.9469490141588171594 ) ) 
 REPRESENTATION_ITEM ( '' )  );
#8404 = DIRECTION ( 'NONE',  ( 0.000000000000000000, -0.9238795325112906243, 0.3826834323650805114 ) ) ;
#8405 = VERTEX_POINT ( 'NONE', #17431 ) ;
#8406 = AXIS2_PLACEMENT_3D ( 'NONE', #2575, #43520, #21280 ) ;
#8407 = EDGE_CURVE ( 'NONE', #57603, #54442, #41112, .T. ) ;
#8408 = FACE_BOUND ( 'NONE', #72335, .T. ) ;
#8409 = AXIS2_PLACEMENT_3D ( 'NONE', #1120, #19097, #42044 ) ;
#8410 = AXIS2_PLACEMENT_3D ( 'NONE', #40710, #68912, #52346 ) ;
#8411 = VECTOR ( 'NONE', #6249, 1000.000000000000114 ) ;
#8412 = ORIENTED_EDGE ( 'NONE', *, *, #62038, .T. ) ;
#8413 = ORIENTED_EDGE ( 'NONE', *, *, #46782, .T. ) ;
#8414 = AXIS2_PLACEMENT_3D ( 'NONE', #45973, #41795, #7220 ) ;
#8415 = VERTEX_POINT ( 'NONE', #23809 ) ;
#8416 = AXIS2_PLACEMENT_3D ( 'NONE', #10988, #45587, #62886 ) ;
#8417 = CARTESIAN_POINT ( 'NONE',  ( -12.40464318976452596, 10.41032311384371489, 32.98187577049606745 ) ) ;
#8418 = ORIENTED_EDGE ( 'NONE', *, *, #21972, .T. ) ;
#8419 = EDGE_CURVE ( 'NONE', #11350, #38975, #12519, .T. ) ;
#8420 = ORIENTED_EDGE ( 'NONE', *, *, #68442, .F. ) ;
#8421 = CARTESIAN_POINT ( 'NONE',  ( 97.30629616937498838, 91.33154071421968467, 80.64697916753382856 ) ) ;
#8422 = CARTESIAN_POINT ( 'NONE',  ( 93.67500000000001137, -212.2949673200287179, 88.91520833506763211 ) ) ;
#8423 = ADVANCED_FACE ( 'NONE', ( #63305 ), #34720, .T. ) ;
#8424 = CARTESIAN_POINT ( 'NONE',  ( -95.00000000000002842, 93.05995642670504253, 88.01562500173432113 ) ) ;
#8425 = EDGE_LOOP ( 'NONE', ( #34483, #3066 ) ) ;
#8426 = ORIENTED_EDGE ( 'NONE', *, *, #4591, .F. ) ;
#8427 = VERTEX_POINT ( 'NONE', #1300 ) ;
#8428 = DIRECTION ( 'NONE',  ( 1.000000000000000000, 0.000000000000000000, 0.000000000000000000 ) ) ;
#8429 = CIRCLE ( 'NONE', #30035, 31.99999999999998579 ) ;
#8431 = ORIENTED_EDGE ( 'NONE', *, *, #57077, .F. ) ;
#8430 = EDGE_CURVE ( 'NONE', #71727, #69710, #69671, .T. ) ;
#8432 = ADVANCED_FACE ( 'NONE', ( #59139 ), #7626, .T. ) ;
#8433 = DIRECTION ( 'NONE',  ( 1.000000000000000000, 0.000000000000000000, 0.000000000000000000 ) ) ;
#8434 = CYLINDRICAL_SURFACE ( 'NONE', #763, 82.00000000000000000 ) ;
#8435 = DIRECTION ( 'NONE',  ( 0.000000000000000000, -0.9876883405951359940, -0.1564344650402420822 ) ) ;
#8436 = CARTESIAN_POINT ( 'NONE',  ( 97.64999999999996305, 90.00000034979572661, 77.69687501385438111 ) ) ;
#8437 = DIRECTION ( 'NONE',  ( -1.000000000000000000, -0.000000000000000000, -0.000000000000000000 ) ) ;
#8438 = CARTESIAN_POINT ( 'NONE',  ( 10.00000000000000000, -12.26510123303234501, -35.53030884539098366 ) ) ;
#8439 = FACE_OUTER_BOUND ( 'NONE', #58268, .T. ) ;
#8440 = CARTESIAN_POINT ( 'NONE',  ( -92.34999999999999432, -208.4700217866474645, 75.84479166840098685 ) ) ;
#8441 = DIRECTION ( 'NONE',  ( -1.000000000000000000, 0.000000000000000000, -0.000000000000000000 ) ) ;
#8442 = EDGE_CURVE ( 'NONE', #1463, #63017, #29072, .T. ) ;
#8444 = CARTESIAN_POINT ( 'NONE',  ( -95.00000000000002842, 93.05995642670501411, 77.85562500173429612 ) ) ;
#8443 = CARTESIAN_POINT ( 'NONE',  ( 92.34999999999999432, 91.52997821335252127, 76.69145833506763665 ) ) ;
#8445 = ORIENTED_EDGE ( 'NONE', *, *, #9436, .T. ) ;
#8446 = CARTESIAN_POINT ( 'NONE',  ( 93.84685191531248449, 91.99731107132950569, 76.99572916753382401 ) ) ;
#8447 = DIRECTION ( 'NONE',  ( 1.000000000000000000, 0.000000000000000000, 0.000000000000000000 ) ) ;
#8448 = CARTESIAN_POINT ( 'NONE',  ( 10.00000000000000000, 46.11716303203188261, 67.80270845531904911 ) ) ;
#8449 = CARTESIAN_POINT ( 'NONE',  ( 10.00000000000000000, 35.38097989696528600, -12.42422080174602605 ) ) ;
#8450 = EDGE_CURVE ( 'NONE', #9220, #61985, #17789, .T. ) ;
#8451 = CYLINDRICAL_SURFACE ( 'NONE', #66698, 82.00000000000000000 ) ;
#8452 = AXIS2_PLACEMENT_3D ( 'NONE', #63138, #51089, #11236 ) ;
#8453 = ORIENTED_EDGE ( 'NONE', *, *, #49611, .F. ) ;
#8454 = LINE ( 'NONE', #13704, #45777 ) ;
#8455 = AXIS2_PLACEMENT_3D ( 'NONE', #13724, #70482, #29904 ) ;
#8456 = DIRECTION ( 'NONE',  ( 0.000000000000000000, 0.3090169943749560555, 0.9510565162951506446 ) ) ;
#8457 = VERTEX_POINT ( 'NONE', #69301 ) ;
#8458 = EDGE_LOOP ( 'NONE', ( #46686, #65680, #11942, #3063 ) ) ;
#8459 = VECTOR ( 'NONE', #53395, 1000.000000000000000 ) ;
#8460 = LINE ( 'NONE', #60708, #13470 ) ;
#8461 = LINE ( 'NONE', #19355, #18951 ) ;
#8462 = CARTESIAN_POINT ( 'NONE',  ( 96.32499999999998863, -207.7050326799711968, 87.96270833506763154 ) ) ;
#8463 = CARTESIAN_POINT ( 'NONE',  ( 16.84844760790522855, -103.5491698323862124, 5.500000000000000000 ) ) ;
#8464 = FACE_OUTER_BOUND ( 'NONE', #71168, .T. ) ;
#8465 = CARTESIAN_POINT ( 'NONE',  ( -92.69370383062498320, -209.9999999999999716, 75.51406250086715488 ) ) ;
#8466 = ORIENTED_EDGE ( 'NONE', *, *, #70241, .F. ) ;
#8467 = PLANE ( 'NONE',  #73965 ) ;
#8468 = VECTOR ( 'NONE', #48920, 1000.000000000000114 ) ;
#8469 = CARTESIAN_POINT ( 'NONE',  ( -2.503857664561936813E-16, -5.773502691896267081, -6.000000000000000000 ) ) ;
#8470 = CARTESIAN_POINT ( 'NONE',  ( -93.67500000000003979, 92.29496732002878900, 78.99333333333332519 ) ) ;
#8471 = CARTESIAN_POINT ( 'NONE',  ( 11.99999999999999822, 0.000000000000000000, 0.000000000000000000 ) ) ;
#8472 = CARTESIAN_POINT ( 'NONE',  ( 11.99999999999999822, -0.8261519478436571973, 77.49459641780886443 ) ) ;
#8473 = DIRECTION ( 'NONE',  ( -1.000000000000000000, -0.000000000000000000, -0.000000000000000000 ) ) ;
#8474 = UNCERTAINTY_MEASURE_WITH_UNIT (LENGTH_MEASURE( 1.000000000000000082E-05 ), #32161, 'distance_accuracy_value', 'NONE');
#8475 =( NAMED_UNIT ( * ) PLANE_ANGLE_UNIT ( ) SI_UNIT ( $, .RADIAN. ) );
#8476 = CIRCLE ( 'NONE', #18078, 13.10000000000023590 ) ;
#8477 = DIRECTION ( 'NONE',  ( -0.5687579148473752566, 0.8225049752423786442, 0.000000000000000000 ) ) ;
#8478 = DIRECTION ( 'NONE',  ( 0.000000000000000000, 0.9238795325112877377, -0.3826834323650873948 ) ) ;
#8479 = CARTESIAN_POINT ( 'NONE',  ( 92.69370383062498320, 88.66845928578035796, 84.77447916753381207 ) ) ;
#8480 = CARTESIAN_POINT ( 'NONE',  ( -92.69370383062498320, -208.6684592857803295, 84.45697916753383083 ) ) ;
#8481 = DIRECTION ( 'NONE',  ( 0.6862798483830554463, 0.7273375899149793211, -0.000000000000000000 ) ) ;
#8482 = ORIENTED_EDGE ( 'NONE', *, *, #37794, .F. ) ;
#8483 = FACE_BOUND ( 'NONE', #18030, .T. ) ;
#8484 = CARTESIAN_POINT ( 'NONE',  ( -97.64999999999994884, -208.4700217866474645, 77.88208333333332689 ) ) ;
#8485 = ADVANCED_FACE ( 'NONE', ( #1664, #40738 ), #12883, .T. ) ;
#8486 = CARTESIAN_POINT ( 'NONE',  ( 0.000000000000000000, 0.000000000000000000, 0.000000000000000000 ) ) ;
#8487 = ADVANCED_FACE ( 'NONE', ( #64411 ), #35814, .T. ) ;
#8488 = EDGE_CURVE ( 'NONE', #35321, #37581, #20662, .T. ) ;
#8489 = ADVANCED_FACE ( 'NONE', ( #31932 ), #60891, .F. ) ;
#8490 = CARTESIAN_POINT ( 'NONE',  ( 95.00000000000000000, -207.3369185715606307, 83.13406250086714522 ) ) ;
#8491 = ORIENTED_EDGE ( 'NONE', *, *, #44074, .F. ) ;
#8492 = DIRECTION ( 'NONE',  ( -7.962523111839282146E-16, 1.065814103640130873E-14, 1.000000000000000000 ) ) ;
#8493 = EDGE_LOOP ( 'NONE', ( #41062, #44934, #6398, #59628 ) ) ;
#8494 = ORIENTED_EDGE ( 'NONE', *, *, #404, .T. ) ;
#8495 = AXIS2_PLACEMENT_3D ( 'NONE', #23913, #70868, #70483 ) ;
#8497 = VECTOR ( 'NONE', #56924, 1000.000000000000000 ) ;
#8496 = CARTESIAN_POINT ( 'NONE',  ( -3.000000000000000000, -11.95096189432345390, 23.69967320028757385 ) ) ;
#8498 = EDGE_CURVE ( 'NONE', #27250, #24265, #67640, .T. ) ;
#8499 = ORIENTED_EDGE ( 'NONE', *, *, #62259, .F. ) ;
#8500 = EDGE_CURVE ( 'NONE', #66667, #26840, #18062, .T. ) ;
#8501 = CARTESIAN_POINT ( 'NONE',  ( 0.000000000000000000, -71.91182617369167929, -28.89263327155821059 ) ) ;
#8502 = CARTESIAN_POINT ( 'NONE',  ( 97.30629616937498838, -209.9999999999999716, 78.68906250086715204 ) ) ;
#8503 = CARTESIAN_POINT ( 'NONE',  ( 10.00000000000000000, 0.000000000000000000, 0.000000000000000000 ) ) ;
#8504 = FACE_OUTER_BOUND ( 'NONE', #17303, .T. ) ;
#8505 = DIRECTION ( 'NONE',  ( -1.000000000000000000, -0.000000000000000000, -0.000000000000000000 ) ) ;
#8506 = LINE ( 'NONE', #30311, #35082 ) ;
#8507 = DIRECTION ( 'NONE',  ( -1.000000000000000000, 0.000000000000000000, -0.000000000000000000 ) ) ;
#8508 = CARTESIAN_POINT ( 'NONE',  ( 97.64999999999997726, -211.5299782133524502, 81.37458333333333371 ) ) ;
#8509 = AXIS2_PLACEMENT_3D ( 'NONE', #68850, #17332, #16587 ) ;
#8510 = EDGE_LOOP ( 'NONE', ( #10830, #61773, #30303, #8533 ) ) ;
#8511 = VERTEX_POINT ( 'NONE', #55242 ) ;
#8512 = VERTEX_POINT ( 'NONE', #44340 ) ;
#8513 = ORIENTED_EDGE ( 'NONE', *, *, #18104, .T. ) ;
#8514 = CARTESIAN_POINT ( 'NONE',  ( -0.0004442498525516064278, 0.001194404164626844313, -64.00000000000000000 ) ) ;
#8515 = CIRCLE ( 'NONE', #14510, 31.99999999999998934 ) ;
#8516 = ADVANCED_FACE ( 'NONE', ( #32294 ), #47844, .F. ) ;
#8517 = EDGE_CURVE ( 'NONE', #40304, #56703, #72176, .T. ) ;
#8518 = CIRCLE ( 'NONE', #44539, 3.299999999999983391 ) ;
#8519 =( NAMED_UNIT ( * ) PLANE_ANGLE_UNIT ( ) SI_UNIT ( $, .RADIAN. ) );
#8520 = CARTESIAN_POINT ( 'NONE',  ( -95.00000000000002842, 92.66308142843932671, 84.56281250086716739 ) ) ;
#8521 = CARTESIAN_POINT ( 'NONE',  ( 92.34999999999999432, 90.00000000000002842, 89.44437500173430067 ) ) ;
#8522 = CIRCLE ( 'NONE', #1382, 77.49899999999999523 ) ;
#8523 = DIRECTION ( 'NONE',  ( -1.000000000000000000, -0.000000000000000000, 0.000000000000000000 ) ) ;
#8524 = SHAPE_REPRESENTATION ( 'Input Shaft', ( #43395 ), #21791 ) ;
#8525 = CARTESIAN_POINT ( 'NONE',  ( 11.99999999999999822, 35.91791733033476675, 68.67312586195008350 ) ) ;
#8526 = DIRECTION ( 'NONE',  ( 1.000000000000000000, 0.000000000000000000, 0.000000000000000000 ) ) ;
#8527 = ORIENTED_EDGE ( 'NONE', *, *, #63036, .T. ) ;
#8528 = CARTESIAN_POINT ( 'NONE',  ( -97.64999999999994884, -211.5299782133524502, 84.41729166840097776 ) ) ;
#8529 = ORIENTED_EDGE ( 'NONE', *, *, #64256, .F. ) ;
#8530 = DIRECTION ( 'NONE',  ( -0.000000000000000000, -0.000000000000000000, -1.000000000000000000 ) ) ;
#8531 = ORIENTED_EDGE ( 'NONE', *, *, #65099, .F. ) ;
#8532 = CARTESIAN_POINT ( 'NONE',  ( -95.00000000000002842, 86.94004357329504273, 85.15812500173430521 ) ) ;
#8533 = ORIENTED_EDGE ( 'NONE', *, *, #8854, .T. ) ;
#8534 = CARTESIAN_POINT ( 'NONE',  ( 96.15314808468748708, 88.00268892867053694, 86.83822916753382515 ) ) ;
#8535 = LINE ( 'NONE', #70924, #43044 ) ;
#8536 = CARTESIAN_POINT ( 'NONE',  ( 10.00000000000000000, -22.64427369931148348, -30.00120703465229965 ) ) ;
#8537 = CARTESIAN_POINT ( 'NONE',  ( 0.000000000000000000, -65.58780272294100655, 36.73666225445870737 ) ) ;
#8538 = DIRECTION ( 'NONE',  ( -1.000000000000000000, 7.955419762439749020E-15, 2.563413034563919251E-14 ) ) ;
#8539 = ORIENTED_EDGE ( 'NONE', *, *, #13179, .F. ) ;
#8540 = DIRECTION ( 'NONE',  ( 0.000000000000000000, 0.000000000000000000, 1.000000000000000000 ) ) ;
#8541 = CARTESIAN_POINT ( 'NONE',  ( 0.000000000000000000, -0.8261519478425841667, -77.49459641780886443 ) ) ;
#8542 = ORIENTED_EDGE ( 'NONE', *, *, #30915, .F. ) ;
#8543 = ORIENTED_EDGE ( 'NONE', *, *, #30901, .T. ) ;
#8544 = DIRECTION ( 'NONE',  ( -1.000000000000000000, -0.000000000000000000, 0.000000000000000000 ) ) ;
#8545 = PRODUCT_DEFINITION_SHAPE ( 'NONE', 'NONE',  #5869 ) ;
#8546 = CYLINDRICAL_SURFACE ( 'NONE', #38407, 1.000000000000000000 ) ;
#8547 = LINE ( 'NONE', #67914, #56952 ) ;
#8548 = CARTESIAN_POINT ( 'NONE',  ( -92.69370383062498320, -208.6684592857803011, 85.72697916753381264 ) ) ;
#8549 = ORIENTED_EDGE ( 'NONE', *, *, #28083, .F. ) ;
#8550 = SURFACE_STYLE_FILL_AREA ( #14172 ) ;
#8551 = VERTEX_POINT ( 'NONE', #43613 ) ;
#8552 = ORIENTED_EDGE ( 'NONE', *, *, #68105, .T. ) ;
#8553 = VECTOR ( 'NONE', #71607, 1000.000000000000000 ) ;
#8554 = DIRECTION ( 'NONE',  ( 1.000000000000000000, 0.000000000000000000, 0.000000000000000000 ) ) ;
#8555 = CIRCLE ( 'NONE', #50557, 31.99999999999999645 ) ;
#8556 = CYLINDRICAL_SURFACE ( 'NONE', #69534, 82.00000000000000000 ) ;
#8557 = CARTESIAN_POINT ( 'NONE',  ( 94.99999999999998579, 92.66308142843932671, 78.68906250086713783 ) ) ;
#8558 = LINE ( 'NONE', #71314, #2901 ) ;
#8559 = CARTESIAN_POINT ( 'NONE',  ( 10.00000000000000000, 29.81001611431041098, -22.74946021919100403 ) ) ;
#8560 = CARTESIAN_POINT ( 'NONE',  ( 92.35000000000000853, -209.9999999999999716, 90.00000000000000000 ) ) ;
#8561 = CARTESIAN_POINT ( 'NONE',  ( 93.26435506835481704, 91.73956328105560942, 74.87701898318917415 ) ) ;
#8562 = CARTESIAN_POINT ( 'NONE',  ( -97.65000000000001990, 88.47002178664754979, 76.79729166840095900 ) ) ;
#8563 = CARTESIAN_POINT ( 'NONE',  ( 0.000000000000000000, 35.47612816024556537, -22.48208911017461631 ) ) ;
#8564 = APPLICATION_CONTEXT ( 'automotive_design' ) ;
#8565 = CARTESIAN_POINT ( 'NONE',  ( 10.00000000000000000, -39.78640506895653317, 66.50666863321987421 ) ) ;
#8566 = PRODUCT_DEFINITION_CONTEXT ( 'detailed design', #29179, 'design' ) ;
#8567 = DIRECTION ( 'NONE',  ( -1.000000000000000000, 0.000000000000000000, 0.000000000000000000 ) ) ;
#8568 = VERTEX_POINT ( 'NONE', #61632 ) ;
#8569 = EDGE_CURVE ( 'NONE', #36612, #58170, #51807, .T. ) ;
#8570 = CARTESIAN_POINT ( 'NONE',  ( -92.69370383062505425, 88.66845928578038638, 84.19239583420048234 ) ) ;
#8571 = AXIS2_PLACEMENT_3D ( 'NONE', #6157, #58010, #11401 ) ;
#8572 = CARTESIAN_POINT ( 'NONE',  ( 92.35000000045006630, 89.99996890530464100, 88.81037122970248276 ) ) ;
#8573 = CIRCLE ( 'NONE', #30126, 77.49899999999999523 ) ;
#8574 = EDGE_CURVE ( 'NONE', #12587, #48259, #34952, .T. ) ;
#8575 = AXIS2_PLACEMENT_3D ( 'NONE', #22069, #45012, #67939 ) ;
#8576 = EDGE_CURVE ( 'NONE', #63916, #54914, #49226, .T. ) ;
#8577 = LINE ( 'NONE', #66461, #19836 ) ;
#8578 = ORIENTED_EDGE ( 'NONE', *, *, #2992, .F. ) ;
#8579 = EDGE_CURVE ( 'NONE', #16867, #50672, #70769, .T. ) ;
#8580 = LINE ( 'NONE', #71332, #61854 ) ;
#8581 = DIRECTION ( 'NONE',  ( 0.000000000000000000, -6.938893903907228378E-15, 1.000000000000000000 ) ) ;
#8582 = CARTESIAN_POINT ( 'NONE',  ( 10.00000000000000000, 71.21200624218795383, 40.65526001592638039 ) ) ;
#8583 = CARTESIAN_POINT ( 'NONE',  ( 97.30629616937498838, -208.6684592857803011, 78.10697916753383652 ) ) ;
#8584 = ORIENTED_EDGE ( 'NONE', *, *, #493, .F. ) ;
#8585 = VERTEX_POINT ( 'NONE', #16136 ) ;
#8586 = EDGE_CURVE ( 'NONE', #27635, #8982, #67412, .T. ) ;
#8587 = ADVANCED_FACE ( 'NONE', ( #39073 ), #55614, .F. ) ;
#8588 = CARTESIAN_POINT ( 'NONE',  ( 10.00000000000000000, 0.000000000000000000, 0.000000000000000000 ) ) ;
#8589 = FACE_OUTER_BOUND ( 'NONE', #69836, .T. ) ;
#8590 = DIRECTION ( 'NONE',  ( 0.000000000000000000, -0.1045284632676569680, -0.9945218953682730678 ) ) ;
#8591 = ORIENTED_EDGE ( 'NONE', *, *, #21038, .F. ) ;
#8592 = CARTESIAN_POINT ( 'NONE',  ( -12.49999999999999822, -120.0000000000000000, 125.0000000000000000 ) ) ;
#8593 = CARTESIAN_POINT ( 'NONE',  ( 92.69370383062501162, -208.6684592857803011, 77.04864583420048518 ) ) ;
#8594 = CIRCLE ( 'NONE', #47034, 42.00000000000000000 ) ;
#8595 = ORIENTED_EDGE ( 'NONE', *, *, #25652, .F. ) ;
#8596 = CARTESIAN_POINT ( 'NONE',  ( 5.999999999999999112, -46.11716303203233736, 67.80270845531873647 ) ) ;
#8597 = VERTEX_POINT ( 'NONE', #27027 ) ;
#8598 = ORIENTED_EDGE ( 'NONE', *, *, #3150, .T. ) ;
#8599 = DIRECTION ( 'NONE',  ( -1.000000000000000000, 0.000000000000000000, 0.000000000000000000 ) ) ;
#8600 = ADVANCED_FACE ( 'NONE', ( #49959 ), #4135, .T. ) ;
#8601 = EDGE_CURVE ( 'NONE', #27431, #53345, #20572, .T. ) ;
#8602 = CONICAL_SURFACE ( 'NONE', #30218, 13.71319123027096865, 1.361356816555593596 ) ;
#8603 =( NAMED_UNIT ( * ) SI_UNIT ( $, .STERADIAN. ) SOLID_ANGLE_UNIT ( ) );
#8604 = DIRECTION ( 'NONE',  ( -1.000000000000000000, 0.000000000000000000, -0.000000000000000000 ) ) ;
#8605 = ORIENTED_EDGE ( 'NONE', *, *, #53404, .F. ) ;
#8606 = DIRECTION ( 'NONE',  ( 0.6064928550163511956, 0.7950889364178798102, -0.000000000000000000 ) ) ;
#8607 = CARTESIAN_POINT ( 'NONE',  ( 97.64999999999997726, -208.4700217866474645, 82.19479166840095274 ) ) ;
#8608 = CARTESIAN_POINT ( 'NONE',  ( 92.34999999999999432, 88.47002178664753558, 84.33791666666667197 ) ) ;
#8609 = ORIENTED_EDGE ( 'NONE', *, *, #29332, .T. ) ;
#8610 = CYLINDRICAL_SURFACE ( 'NONE', #37131, 23.50000000000489919 ) ;
#8611 = AXIS2_PLACEMENT_3D ( 'NONE', #56632, #21654, #32558 ) ;
#8612 = CARTESIAN_POINT ( 'NONE',  ( -92.35000000035631729, -210.0000434577671911, 89.12687334326093946 ) ) ;
#8613 = ORIENTED_EDGE ( 'NONE', *, *, #65612, .T. ) ;
#8614 = EDGE_LOOP ( 'NONE', ( #61440, #8985, #27997, #33826 ) ) ;
#8615 =( BOUNDED_CURVE ( )  B_SPLINE_CURVE ( 2, ( #74164, #62157, #10644, #56894, #68162, #5029, #73788, #22679, #67042 ),
 .UNSPECIFIED., .F., .F. ) 
 B_SPLINE_CURVE_WITH_KNOTS ( ( 3, 2, 2, 2, 3 ),
 ( 0.7620226289464454572, 0.7620226784152968058, 0.7690784439561787478, 0.7761342094970608008, 0.7831899741065913023 ),
 .UNSPECIFIED. ) 
 CURVE ( )  GEOMETRIC_REPRESENTATION_ITEM ( )  RATIONAL_B_SPLINE_CURVE ( ( 0.9999981213879984843, 0.9999990606874136212, 1.000000000000000000, 0.8660254037844387076, 1.000000000000000000, 0.8660254037844387076, 1.000000000000000000, 0.8660254037844387076, 1.000000000000000000 ) ) 
 REPRESENTATION_ITEM ( '' )  );
#8616 = CARTESIAN_POINT ( 'NONE',  ( -93.84685191531252713, 88.00268892867056536, 89.37822916753381719 ) ) ;
#8617 = CARTESIAN_POINT ( 'NONE',  ( 97.30629616937498838, 88.66845928578037217, 82.92239583420045790 ) ) ;
#8618 = ORIENTED_EDGE ( 'NONE', *, *, #46698, .F. ) ;
#8619 = CARTESIAN_POINT ( 'NONE',  ( 93.67499999999999716, 87.70503267997126784, 81.93020833506763267 ) ) ;
#8620 = DIRECTION ( 'NONE',  ( 0.000000000000000000, 0.000000000000000000, 1.000000000000000000 ) ) ;
#8621 = VERTEX_POINT ( 'NONE', #15013 ) ;
#8622 = CARTESIAN_POINT ( 'NONE',  ( 93.67500000000001137, -207.7050326799711968, 87.43354166840096298 ) ) ;
#8623 = CIRCLE ( 'NONE', #21812, 77.49899999999999523 ) ;
#8624 = ORIENTED_EDGE ( 'NONE', *, *, #62784, .T. ) ;
#8625 = VECTOR ( 'NONE', #42002, 1000.000000000000000 ) ;
#8626 = ORIENTED_EDGE ( 'NONE', *, *, #6312, .T. ) ;
#8627 = ORIENTED_EDGE ( 'NONE', *, *, #37117, .F. ) ;
#8628 = DIRECTION ( 'NONE',  ( 0.000000000000000000, -0.1564344650402170744, -0.9876883405951398798 ) ) ;
#8629 = AXIS2_PLACEMENT_3D ( 'NONE', #34362, #21974, #57305 ) ;
#8630 = CARTESIAN_POINT ( 'NONE',  ( -23.25244084006223133, -132.7111759872722416, -2.500000000000000000 ) ) ;
#8631 = CARTESIAN_POINT ( 'NONE',  ( -93.67500000000003979, 87.70503267997129626, 84.49666666666666970 ) ) ;
#8632 = ORIENTED_EDGE ( 'NONE', *, *, #12870, .T. ) ;
#8633 = FACE_OUTER_BOUND ( 'NONE', #50559, .T. ) ;
#8634 = CYLINDRICAL_SURFACE ( 'NONE', #28688, 31.99999999999999289 ) ;
#8635 = ORIENTED_EDGE ( 'NONE', *, *, #71085, .T. ) ;
#8636 = CARTESIAN_POINT ( 'NONE',  ( -10.00000000000000000, 0.000000000000000000, 0.000000000000000000 ) ) ;
#8637 = CARTESIAN_POINT ( 'NONE',  ( -92.69370383062498320, -211.3315407142195852, 79.11239583420046984 ) ) ;
#8638 = ORIENTED_EDGE ( 'NONE', *, *, #70802, .F. ) ;
#8639 = CARTESIAN_POINT ( 'NONE',  ( 10.00000000000000000, 73.95703589264006439, -23.16143007188350822 ) ) ;
#8640 = DIRECTION ( 'NONE',  ( -1.000000000000000000, 0.000000000000000000, 0.000000000000000000 ) ) ;
#8641 = DIRECTION ( 'NONE',  ( 1.000000000000000000, 0.000000000000000000, 0.000000000000000000 ) ) ;
#8642 = CARTESIAN_POINT ( 'NONE',  ( 10.00000000000000000, -41.19522573413780009, 65.64334221924896440 ) ) ;
#8643 = FACE_OUTER_BOUND ( 'NONE', #1164, .T. ) ;
#8644 = FILL_AREA_STYLE_COLOUR ( '', #24135 ) ;
#8645 = CARTESIAN_POINT ( 'NONE',  ( 5.000000000000000000, 27.74655509720669500, 77.16300072079670258 ) ) ;
#8646 = EDGE_CURVE ( 'NONE', #3079, #8233, #74011, .T. ) ;
#8647 = DIRECTION ( 'NONE',  ( 0.9227826878668550226, 0.3853207896976523772, -0.000000000000000000 ) ) ;
#8648 = ADVANCED_FACE ( 'NONE', ( #740 ), #22526, .T. ) ;
#8649 = CARTESIAN_POINT ( 'NONE',  ( -2.459674775249762302, -3.512261536895417911E-15, -1.958521724548552858E-15 ) ) ;
#8650 = CARTESIAN_POINT ( 'NONE',  ( -96.15314808468752972, 91.99731107132950569, 76.20197916753380696 ) ) ;
#8651 = CARTESIAN_POINT ( 'NONE',  ( 10.00000000000000000, 77.49459641780886443, 0.8261519478433866359 ) ) ;
#8652 = DIRECTION ( 'NONE',  ( 0.000000000000000000, 0.5877852522924797984, 0.8090169943749426773 ) ) ;
#8653 = EDGE_CURVE ( 'NONE', #50612, #55000, #43170, .T. ) ;
#8654 = CARTESIAN_POINT ( 'NONE',  ( 92.35000000000000853, -209.9999999999999716, 75.39499999999999602 ) ) ;
#8655 = CARTESIAN_POINT ( 'NONE',  ( 6.000000000000000000, -15.33399622253424432, -80.55351364060604169 ) ) ;
#8656 = ADVANCED_FACE ( 'NONE', ( #51831 ), #17618, .T. ) ;
#8657 = PRESENTATION_LAYER_ASSIGNMENT (  '', '', ( #39902 ) ) ;
#8658 = AXIS2_PLACEMENT_3D ( 'NONE', #31547, #1924, #24443 ) ;
#8659 = CARTESIAN_POINT ( 'NONE',  ( 10.00000000000000000, 27.13269053701132094, -25.88420570971372570 ) ) ;
#8660 = DIRECTION ( 'NONE',  ( -1.000000000000000000, 0.000000000000000000, -0.000000000000000000 ) ) ;
#8661 = CARTESIAN_POINT ( 'NONE',  ( -10.00000000000000000, 0.000000000000000000, 0.000000000000000000 ) ) ;
#8662 = AXIS2_PLACEMENT_3D ( 'NONE', #746, #57857, #35284 ) ;
#8663 = EDGE_CURVE ( 'NONE', #26693, #42186, #9775, .T. ) ;
#8664 = FACE_OUTER_BOUND ( 'NONE', #51946, .T. ) ;
#8665 = CARTESIAN_POINT ( 'NONE',  ( -92.34999999999999432, -209.9999999999999716, 89.68250000000000455 ) ) ;
#8666 = DIRECTION ( 'NONE',  ( 1.000000000000000000, 0.000000000000000000, 0.000000000000000000 ) ) ;
#8667 = ORIENTED_EDGE ( 'NONE', *, *, #67032, .T. ) ;
#8668 = EDGE_CURVE ( 'NONE', #71835, #6380, #19383, .T. ) ;
#8669 = CARTESIAN_POINT ( 'NONE',  ( 11.99999999999999822, -77.32052557432837148, -5.256550761633681290 ) ) ;
#8670 = FACE_OUTER_BOUND ( 'NONE', #12643, .T. ) ;
#8671 =( NAMED_UNIT ( * ) SI_UNIT ( $, .STERADIAN. ) SOLID_ANGLE_UNIT ( ) );
#8672 = CARTESIAN_POINT ( 'NONE',  ( 0.000000000000000000, -54.21277698773636899, -55.38113227695839669 ) ) ;
#8673 = AXIS2_PLACEMENT_3D ( 'NONE', #47988, #59267, #8870 ) ;
#8674 = CIRCLE ( 'NONE', #38678, 77.49899999999999523 ) ;
#8675 = ORIENTED_EDGE ( 'NONE', *, *, #5559, .F. ) ;
#8676 = EDGE_CURVE ( 'NONE', #39802, #31963, #48348, .T. ) ;
#8677 = DIRECTION ( 'NONE',  ( 0.000000000000000000, 0.000000000000000000, 1.000000000000000000 ) ) ;
#8678 = ADVANCED_FACE ( 'NONE', ( #62390 ), #34169, .F. ) ;
#8679 = CARTESIAN_POINT ( 'NONE',  ( 0.000000000000000000, -5.202137450156655518, 37.22597642581156663 ) ) ;
#8680 = ORIENTED_EDGE ( 'NONE', *, *, #53581, .T. ) ;
#8681 = CARTESIAN_POINT ( 'NONE',  ( 92.69370383062501162, -208.6684592857803295, 83.23989583420048177 ) ) ;
#8682 = CARTESIAN_POINT ( 'NONE',  ( 93.84685191531249870, -208.0026889286704943, 87.79072916753381151 ) ) ;
#8683 = ORIENTED_EDGE ( 'NONE', *, *, #59437, .T. ) ;
#8684 = CARTESIAN_POINT ( 'NONE',  ( 97.30629616937498838, -211.3315407142195852, 86.25614583420048120 ) ) ;
#8685 = ORIENTED_EDGE ( 'NONE', *, *, #28181, .F. ) ;
#8686 = DIRECTION ( 'NONE',  ( 0.000000000000000000, 0.000000000000000000, 1.000000000000000000 ) ) ;
#8687 = VERTEX_POINT ( 'NONE', #4886 ) ;
#8688 = CARTESIAN_POINT ( 'NONE',  ( -97.30629616937501680, 91.33154071421968467, 77.68364583420047609 ) ) ;
#8689 = ORIENTED_EDGE ( 'NONE', *, *, #45338, .F. ) ;
#8690 = ORIENTED_EDGE ( 'NONE', *, *, #46591, .F. ) ;
#8691 = DIRECTION ( 'NONE',  ( 0.000000000000000000, 0.000000000000000000, -1.000000000000000000 ) ) ;
#8692 = ORIENTED_EDGE ( 'NONE', *, *, #8442, .T. ) ;
#8693 = CARTESIAN_POINT ( 'NONE',  ( 15.00000000000000000, 18.84667830672579569, -18.68964196561269375 ) ) ;
#8694 = FACE_OUTER_BOUND ( 'NONE', #18315, .T. ) ;
#8695 = ORIENTED_EDGE ( 'NONE', *, *, #752, .T. ) ;
#8696 = CYLINDRICAL_SURFACE ( 'NONE', #58636, 2.649999999999985700 ) ;
#8697 = ORIENTED_EDGE ( 'NONE', *, *, #59032, .F. ) ;
#8698 = ORIENTED_EDGE ( 'NONE', *, *, #49162, .F. ) ;
#8699 =( GEOMETRIC_REPRESENTATION_CONTEXT ( 3 ) GLOBAL_UNCERTAINTY_ASSIGNED_CONTEXT ( ( #37041 ) ) GLOBAL_UNIT_ASSIGNED_CONTEXT ( ( #49095, #31796, #65298 ) ) REPRESENTATION_CONTEXT ( 'NONE', 'WORKASPACE' ) );
#8700 = ORIENTED_EDGE ( 'NONE', *, *, #12569, .T. ) ;
#8701 = EDGE_LOOP ( 'NONE', ( #60452, #64169, #44944, #65366 ) ) ;
#8702 = CARTESIAN_POINT ( 'NONE',  ( 96.15314808468750130, -211.9973110713294489, 77.15447916753380753 ) ) ;
#8703 = DIRECTION ( 'NONE',  ( -0.9435911131814402886, 0.3311129884571281101, 0.000000000000000000 ) ) ;
#8704 = ITEM_DEFINED_TRANSFORMATION ( 'NONE', 'NONE', #32778,  #43395 ) ;
#8705 = DIRECTION ( 'NONE',  ( -0.000000000000000000, -0.000000000000000000, 1.000000000000000000 ) ) ;
#8706 = ORIENTED_EDGE ( 'NONE', *, *, #54582, .T. ) ;
#8707 = AXIS2_PLACEMENT_3D ( 'NONE', #72160, #16141, #66897 ) ;
#8708 = ORIENTED_EDGE ( 'NONE', *, *, #31914, .T. ) ;
#8709 = DIRECTION ( 'NONE',  ( -0.000000000000000000, -0.000000000000000000, 1.000000000000000000 ) ) ;
#8710 = ORIENTED_EDGE ( 'NONE', *, *, #5636, .F. ) ;
#8711 = CARTESIAN_POINT ( 'NONE',  ( 0.000000000000000000, 77.16300072079660310, 27.74655509720697211 ) ) ;
#8712 = CYLINDRICAL_SURFACE ( 'NONE', #8268, 37.49900000000000233 ) ;
#8713 = CARTESIAN_POINT ( 'NONE',  ( -97.30629616937495996, -209.9999999999999716, 79.48281250086714067 ) ) ;
#8714 = CARTESIAN_POINT ( 'NONE',  ( -92.69370383062502583, 88.66845928578038638, 78.63614583420049087 ) ) ;
#8716 = EDGE_CURVE ( 'NONE', #29107, #42748, #16980, .T. ) ;
#8715 = AXIS2_PLACEMENT_3D ( 'NONE', #4688, #74197, #50136 ) ;
#8717 = VERTEX_POINT ( 'NONE', #12 ) ;
#8718 = CARTESIAN_POINT ( 'NONE',  ( 93.84685191531248449, 88.00268892867053694, 77.68364583420047609 ) ) ;
#8719 = VECTOR ( 'NONE', #15278, 1000.000000000000000 ) ;
#8720 = ORIENTED_EDGE ( 'NONE', *, *, #51959, .F. ) ;
#8721 = DIRECTION ( 'NONE',  ( 0.000000000000000000, 0.000000000000000000, 1.000000000000000000 ) ) ;
#8722 = CARTESIAN_POINT ( 'NONE',  ( -92.69370383062498320, -208.6684592857803011, 88.74322916753379786 ) ) ;
#8723 = FACE_OUTER_BOUND ( 'NONE', #71462, .T. ) ;
#8724 = FACE_OUTER_BOUND ( 'NONE', #69881, .T. ) ;
#8725 = FACE_OUTER_BOUND ( 'NONE', #57234, .T. ) ;
#8726 = CARTESIAN_POINT ( 'NONE',  ( -94.99999999999997158, -207.3369185715606307, 84.40406250086714124 ) ) ;
#8727 = DIRECTION ( 'NONE',  ( 0.000000000000000000, 0.000000000000000000, -1.000000000000000000 ) ) ;
#8728 = DIRECTION ( 'NONE',  ( 1.000000000000000000, -0.000000000000000000, -0.000000000000000000 ) ) ;
#8729 = AXIS2_PLACEMENT_3D ( 'NONE', #24633, #53574, #37415 ) ;
#8730 = CARTESIAN_POINT ( 'NONE',  ( 11.99999999999999822, -74.65374052328654386, 8.840884882374837161 ) ) ;
#8731 = ORIENTED_EDGE ( 'NONE', *, *, #20605, .T. ) ;
#8732 = AXIS2_PLACEMENT_3D ( 'NONE', #12791, #19906, #52652 ) ;
#8733 = ORIENTED_EDGE ( 'NONE', *, *, #35638, .F. ) ;
#8734 = CARTESIAN_POINT ( 'NONE',  ( 0.000000000000000000, 24.81905959214261514, 9.408202855044825341 ) ) ;
#8735 = EDGE_CURVE ( 'NONE', #28195, #41791, #63793, .T. ) ;
#8736 = LINE ( 'NONE', #70019, #55468 ) ;
#8737 = EDGE_CURVE ( 'NONE', #48817, #57658, #375, .T. ) ;
#8738 = DIRECTION ( 'NONE',  ( -1.000000000000000000, 0.000000000000000000, -0.000000000000000000 ) ) ;
#8739 = CARTESIAN_POINT ( 'NONE',  ( -97.30629616937501680, 88.66845928578038638, 86.52072916753381548 ) ) ;
#8740 = DIRECTION ( 'NONE',  ( 1.000000000000000000, -0.000000000000000000, -0.000000000000000000 ) ) ;
#8741 = CARTESIAN_POINT ( 'NONE',  ( -24.50849501662245800, -109.8101191361138831, 5.500000000000000000 ) ) ;
#8742 = DIRECTION ( 'NONE',  ( 0.000000000000000000, 0.000000000000000000, 1.000000000000000000 ) ) ;
#8743 = VERTEX_POINT ( 'NONE', #52193 ) ;
#8744 = DIRECTION ( 'NONE',  ( 1.000000000000000000, 0.000000000000000000, 0.000000000000000000 ) ) ;
#8745 = EDGE_CURVE ( 'NONE', #36437, #53879, #69487, .T. ) ;
#8746 = ADVANCED_FACE ( 'NONE', ( #17252 ), #57113, .T. ) ;
#8747 = DIRECTION ( 'NONE',  ( -0.000000000000000000, -0.000000000000000000, -1.000000000000000000 ) ) ;
#8748 = FACE_OUTER_BOUND ( 'NONE', #19232, .T. ) ;
#8749 = LINE ( 'NONE', #71511, #60986 ) ;
#8750 = CARTESIAN_POINT ( 'NONE',  ( 97.64999999999997726, -208.4700217866474929, 84.65541666666669585 ) ) ;
#8751 = DIRECTION ( 'NONE',  ( 0.000000000000000000, 0.000000000000000000, 1.000000000000000000 ) ) ;
#8752 = CARTESIAN_POINT ( 'NONE',  ( -92.69370383062498320, -211.3315407142195852, 84.35114583420049428 ) ) ;
#8753 =( NAMED_UNIT ( * ) SI_UNIT ( $, .STERADIAN. ) SOLID_ANGLE_UNIT ( ) );
#8754 = LINE ( 'NONE', #35829, #52052 ) ;
#8755 = EDGE_CURVE ( 'NONE', #43515, #60602, #68396, .T. ) ;
#8756 = DIRECTION ( 'NONE',  ( -1.000000000000000000, 0.000000000000000000, 0.000000000000000000 ) ) ;
#8757 = CARTESIAN_POINT ( 'NONE',  ( 97.64999999999999147, -209.9999999999999716, 90.00000000000000000 ) ) ;
#8758 = CARTESIAN_POINT ( 'NONE',  ( -95.00000000000002842, 86.94004357329504273, 88.88875000000000171 ) ) ;
#8759 = ORIENTED_EDGE ( 'NONE', *, *, #7564, .F. ) ;
#8760 = CARTESIAN_POINT ( 'NONE',  ( 10.00000000000000000, 16.23288003029543347, -33.80338159004267595 ) ) ;
#8761 = CARTESIAN_POINT ( 'NONE',  ( -92.35000000000017906, 91.52997821335260653, 78.30541666666667311 ) ) ;
#8762 = DIRECTION ( 'NONE',  ( -1.000000000000000000, 0.000000000000000000, -0.000000000000000000 ) ) ;
#8763 = AXIS2_PLACEMENT_3D ( 'NONE', #24946, #30214, #8028 ) ;
#8764 = CYLINDRICAL_SURFACE ( 'NONE', #69696, 2.649999999999999467 ) ;
#8765 = ORIENTED_EDGE ( 'NONE', *, *, #61518, .T. ) ;
#8766 = EDGE_CURVE ( 'NONE', #32709, #59366, #9482, .T. ) ;
#8767 = CARTESIAN_POINT ( 'NONE',  ( 92.34999999999998010, 90.00000928824103141, 86.90437468048608594 ) ) ;
#8768 = PLANE ( 'NONE',  #54724 ) ;
#8769 = VERTEX_POINT ( 'NONE', #13806 ) ;
#8770 = VECTOR ( 'NONE', #51721, 1000.000000000000000 ) ;
#8771 = CYLINDRICAL_SURFACE ( 'NONE', #54430, 31.99999999999998579 ) ;
#8772 = EDGE_CURVE ( 'NONE', #1170, #13817, #58573, .T. ) ;
#8773 = EDGE_LOOP ( 'NONE', ( #38359, #35048, #65098, #10354 ) ) ;
#8774 = AXIS2_PLACEMENT_3D ( 'NONE', #68763, #40187, #62008 ) ;
#8775 = DIRECTION ( 'NONE',  ( -1.000000000000000000, 0.000000000000000000, 0.000000000000000000 ) ) ;
#8776 = CIRCLE ( 'NONE', #50791, 82.00000000000000000 ) ;
#8777 = VERTEX_POINT ( 'NONE', #29614 ) ;
#8778 = ORIENTED_EDGE ( 'NONE', *, *, #47523, .F. ) ;
#8779 = ORIENTED_EDGE ( 'NONE', *, *, #73845, .F. ) ;
#8780 = ORIENTED_EDGE ( 'NONE', *, *, #37665, .T. ) ;
#8781 = PLANE ( 'NONE',  #47939 ) ;
#8782 = ORIENTED_EDGE ( 'NONE', *, *, #47473, .F. ) ;
#8783 = ORIENTED_EDGE ( 'NONE', *, *, #39012, .F. ) ;
#8784 = CARTESIAN_POINT ( 'NONE',  ( 94.99999999999998579, 92.66308142843935514, 80.11781250086714579 ) ) ;
#8785 = DIRECTION ( 'NONE',  ( 1.000000000000000000, 0.000000000000000000, -0.000000000000000000 ) ) ;
#8786 = B_SPLINE_CURVE_WITH_KNOTS ( 'NONE', 3,
 ( #42882, #59425, #18816, #64334, #58685, #24835 ),
 .UNSPECIFIED., .F., .F.,
 ( 4, 2, 4 ),
 ( 0.005150343764683553392, 0.006610526168996383109, 0.008070708573309213693 ),
 .UNSPECIFIED. ) ;
#8787 = CARTESIAN_POINT ( 'NONE',  ( -92.35000000000003695, 89.99999996655868983, 87.85687500050293863 ) ) ;
#8788 = ORIENTED_EDGE ( 'NONE', *, *, #13832, .T. ) ;
#8789 = ORIENTED_EDGE ( 'NONE', *, *, #28605, .F. ) ;
#8790 = ORIENTED_EDGE ( 'NONE', *, *, #30732, .T. ) ;
#8791 = FACE_OUTER_BOUND ( 'NONE', #44094, .T. ) ;
#8792 = VERTEX_POINT ( 'NONE', #47662 ) ;
#8793 = CARTESIAN_POINT ( 'NONE',  ( 1.644296007894228351E-15, -120.0000000000000000, 82.00000000000000000 ) ) ;
#8794 = FACE_OUTER_BOUND ( 'NONE', #52708, .T. ) ;
#8795 = DIRECTION ( 'NONE',  ( -1.000000000000000000, -0.000000000000000000, -0.000000000000000000 ) ) ;
#8796 = LINE ( 'NONE', #31713, #23348 ) ;
#8797 = DIRECTION ( 'NONE',  ( -1.000000000000000000, 0.000000000000000000, 0.000000000000000000 ) ) ;
#8798 = DIRECTION ( 'NONE',  ( 0.000000000000000000, -0.7071067811865536790, 0.7071067811865414665 ) ) ;
#8799 = DIRECTION ( 'NONE',  ( 0.000000000000000000, 0.000000000000000000, 1.000000000000000000 ) ) ;
#8800 = CARTESIAN_POINT ( 'NONE',  ( -97.64999999999994884, -208.4700217866474645, 74.78645833506763552 ) ) ;
#8801 = CARTESIAN_POINT ( 'NONE',  ( -92.69370383062502583, 88.66845928578038638, 88.79614583420050167 ) ) ;
#8802 = VERTEX_POINT ( 'NONE', #65704 ) ;
#8803 = CIRCLE ( 'NONE', #37626, 15.99999999999999645 ) ;
#8804 = EDGE_CURVE ( 'NONE', #20251, #62534, #42400, .T. ) ;
#8806 = CARTESIAN_POINT ( 'NONE',  ( -97.30629616937501680, 90.00000000000004263, 89.00781250086714635 ) ) ;
#8805 = CARTESIAN_POINT ( 'NONE',  ( 93.67499999999998295, 92.29496732002878900, 74.73354166840096013 ) ) ;
#8807 = ORIENTED_EDGE ( 'NONE', *, *, #15284, .T. ) ;
#8808 = CARTESIAN_POINT ( 'NONE',  ( 92.69370383062498320, 90.00000000000002842, 75.83156250086716454 ) ) ;
#8809 = CYLINDRICAL_SURFACE ( 'NONE', #24176, 2.649999999999985700 ) ;
#8810 = CARTESIAN_POINT ( 'NONE',  ( 97.64999999999999147, -209.9999999999999716, 87.77749999999998920 ) ) ;
#8811 = DIRECTION ( 'NONE',  ( -1.000000000000000000, 0.000000000000000000, 0.000000000000000000 ) ) ;
#8812 = LINE ( 'NONE', #26092, #73477 ) ;
#8813 = FACE_OUTER_BOUND ( 'NONE', #4850, .T. ) ;
#8814 = AXIS2_PLACEMENT_3D ( 'NONE', #70824, #9157, #3550 ) ;
#8815 = DIRECTION ( 'NONE',  ( -1.000000000000000000, -0.000000000000000000, -0.000000000000000000 ) ) ;
#8816 = FACE_OUTER_BOUND ( 'NONE', #14791, .T. ) ;
#8817 = EDGE_LOOP ( 'NONE', ( #3291, #57455, #4393, #58189, #57552 ) ) ;
#8818 = EDGE_CURVE ( 'NONE', #32719, #63900, #67361, .T. ) ;
#8819 = CIRCLE ( 'NONE', #433, 16.00000000000000000 ) ;
#8820 = ORIENTED_EDGE ( 'NONE', *, *, #50052, .T. ) ;
#8821 = EDGE_CURVE ( 'NONE', #28736, #15229, #6201, .T. ) ;
#8822 = CARTESIAN_POINT ( 'NONE',  ( -3.000000000000000000, 5.835314593368477354, 22.81335362449854642 ) ) ;
#8823 = DIRECTION ( 'NONE',  ( -1.000000000000000000, 0.000000000000000000, 0.000000000000000000 ) ) ;
#8824 = DIRECTION ( 'NONE',  ( 0.000000000000000000, -0.2079116908177532363, -0.9781476007338070211 ) ) ;
#8825 = DIRECTION ( 'NONE',  ( 1.000000000000000000, 0.000000000000000000, 0.000000000000000000 ) ) ;
#8826 = CARTESIAN_POINT ( 'NONE',  ( -92.35000000000005116, 88.47002178664754979, 76.37395833506761278 ) ) ;
#8827 =( BOUNDED_CURVE ( )  B_SPLINE_CURVE ( 2, ( #9622, #15254, #26531, #20893, #73128, #22010, #56228 ),
 .UNSPECIFIED., .F., .F. ) 
 B_SPLINE_CURVE_WITH_KNOTS ( ( 3, 2, 2, 3 ),
 ( 0.04166666666666644231, 0.04861111111111085514, 0.05555555555555525410, 0.06249999999999966693 ),
 .UNSPECIFIED. ) 
 CURVE ( )  GEOMETRIC_REPRESENTATION_ITEM ( )  RATIONAL_B_SPLINE_CURVE ( ( 1.000000000000004219, 0.8660254037844343777, 1.000000000000000000, 0.8660254037844387076, 1.000000000000000000, 0.8660254037844451469, 0.9999999999999935607 ) ) 
 REPRESENTATION_ITEM ( '' )  );
#8828 = CARTESIAN_POINT ( 'NONE',  ( 94.99999999999998579, 86.94004357329502852, 84.44374999999999432 ) ) ;
#8829 = VECTOR ( 'NONE', #72167, 1000.000000000000000 ) ;
#8830 = ORIENTED_EDGE ( 'NONE', *, *, #40385, .T. ) ;
#8831 = EDGE_CURVE ( 'NONE', #54767, #29022, #53616, .T. ) ;
#8832 = CARTESIAN_POINT ( 'NONE',  ( -3.702536634196095910, 8.043911037661889196, 32.98187577049606745 ) ) ;
#8833 = VECTOR ( 'NONE', #14929, 1000.000000000000000 ) ;
#8834 = VECTOR ( 'NONE', #33048, 1000.000000000000000 ) ;
#8835 = VECTOR ( 'NONE', #73728, 1000.000000000000114 ) ;
#8836 = FACE_BOUND ( 'NONE', #13590, .T. ) ;
#8837 = CARTESIAN_POINT ( 'NONE',  ( 0.000000000000000000, 0.000000000000000000, 0.000000000000000000 ) ) ;
#8838 = CARTESIAN_POINT ( 'NONE',  ( 10.00000000000000000, 70.52718814184294160, -26.02418014898236720 ) ) ;
#8839 = DIRECTION ( 'NONE',  ( 1.000000000000000000, 0.000000000000000000, 0.000000000000000000 ) ) ;
#8840 = DIRECTION ( 'NONE',  ( 0.000000000000000000, 0.000000000000000000, -1.000000000000000000 ) ) ;
#8841 = DIRECTION ( 'NONE',  ( 0.000000000000000000, 0.000000000000000000, 1.000000000000000000 ) ) ;
#8842 = LINE ( 'NONE', #71980, #44878 ) ;
#8843 = CARTESIAN_POINT ( 'NONE',  ( -97.64999999998384794, -210.0000060634594661, 88.17456390440159453 ) ) ;
#8844 = ADVANCED_FACE ( 'NONE', ( #53308 ), #7812, .T. ) ;
#8845 = EDGE_CURVE ( 'NONE', #35626, #46890, #48212, .T. ) ;
#8846 = CARTESIAN_POINT ( 'NONE',  ( 92.69370383062498320, 88.66845928578035796, 82.86947916753379673 ) ) ;
#8847 = VECTOR ( 'NONE', #34138, 1000.000000000000000 ) ;
#8848 = CARTESIAN_POINT ( 'NONE',  ( -97.30629616937495996, -209.9999999999999716, 82.18156250086715886 ) ) ;
#8849 = DIRECTION ( 'NONE',  ( 0.000000000000000000, 0.000000000000000000, 1.000000000000000000 ) ) ;
#8850 = ORIENTED_EDGE ( 'NONE', *, *, #2426, .T. ) ;
#8851 = CARTESIAN_POINT ( 'NONE',  ( 10.00000000000000000, 74.65491531819118620, -8.830959090342659579 ) ) ;
#8852 = CARTESIAN_POINT ( 'NONE',  ( -97.64999999999994884, -208.4700217866474645, 79.15208333333332291 ) ) ;
#8853 = DIRECTION ( 'NONE',  ( -1.000000000000000000, -0.000000000000000000, -0.000000000000000000 ) ) ;
#8854 = EDGE_CURVE ( 'NONE', #52264, #44231, #73360, .T. ) ;
#8855 = CARTESIAN_POINT ( 'NONE',  ( 97.30629616937498838, -211.3315407142195852, 82.92239583420045790 ) ) ;
#8856 = ORIENTED_EDGE ( 'NONE', *, *, #6956, .F. ) ;
#8857 = EDGE_CURVE ( 'NONE', #17019, #21881, #70952, .T. ) ;
#8858 = VECTOR ( 'NONE', #41208, 1000.000000000000000 ) ;
#8859 = DIRECTION ( 'NONE',  ( 0.000000000000000000, 0.000000000000000000, 1.000000000000000000 ) ) ;
#8860 = VERTEX_POINT ( 'NONE', #59693 ) ;
#8861 = VERTEX_POINT ( 'NONE', #69850 ) ;
#8862 = VECTOR ( 'NONE', #44359, 1000.000000000000000 ) ;
#8863 = CARTESIAN_POINT ( 'NONE',  ( 10.00000000000000000, 37.16516213103285082, -4.992566952384588141 ) ) ;
#8864 = VECTOR ( 'NONE', #11538, 1000.000000000000000 ) ;
#8865 = ORIENTED_EDGE ( 'NONE', *, *, #58982, .T. ) ;
#8866 = CARTESIAN_POINT ( 'NONE',  ( 97.30629616937498838, -211.3315407142195852, 77.36614583420048064 ) ) ;
#8867 = LINE ( 'NONE', #31780, #35659 ) ;
#8868 = CYLINDRICAL_SURFACE ( 'NONE', #1619, 2.649999999999985700 ) ;
#8869 = CARTESIAN_POINT ( 'NONE',  ( 10.00000000000000000, -35.53030884539077050, -12.26510123303296851 ) ) ;
#8870 = DIRECTION ( 'NONE',  ( 0.000000000000000000, 0.000000000000000000, 1.000000000000000000 ) ) ;
#8871 = VECTOR ( 'NONE', #4334, 1000.000000000000000 ) ;
#8872 = CARTESIAN_POINT ( 'NONE',  ( -93.67500000000003979, 87.70503267997129626, 83.30604166840096525 ) ) ;
#8873 = CARTESIAN_POINT ( 'NONE',  ( 92.35000000000002274, -211.5299782133524502, 83.06791666666664753 ) ) ;
#8874 = ORIENTED_EDGE ( 'NONE', *, *, #17433, .F. ) ;
#8875 = ORIENTED_EDGE ( 'NONE', *, *, #56089, .F. ) ;
#8876 = ORIENTED_EDGE ( 'NONE', *, *, #36597, .F. ) ;
#8877 = AXIS2_PLACEMENT_3D ( 'NONE', #65619, #3595, #70866 ) ;
#8878 = ORIENTED_EDGE ( 'NONE', *, *, #1387, .F. ) ;
#8879 = LINE ( 'NONE', #47618, #59863 ) ;
#8880 = AXIS2_PLACEMENT_3D ( 'NONE', #14287, #37236, #36472 ) ;
#8881 = CARTESIAN_POINT ( 'NONE',  ( -93.84685191531254134, 91.99731107132950569, 82.60489583420049087 ) ) ;
#8882 = DIRECTION ( 'NONE',  ( 0.000000000000000000, 0.000000000000000000, 1.000000000000000000 ) ) ;
#8883 = CARTESIAN_POINT ( 'NONE',  ( 10.00000000000000000, -0.6853352020787742971, -37.58145647212455032 ) ) ;
#8884 = DIRECTION ( 'NONE',  ( 0.000000000000000000, -0.7431448254773871387, 0.6691306063588661202 ) ) ;
#8885 = CARTESIAN_POINT ( 'NONE',  ( 10.00000000000000000, 16.45098606841126454, 33.79645857604518966 ) ) ;
#8886 = ORIENTED_EDGE ( 'NONE', *, *, #46587, .T. ) ;
#8887 = CARTESIAN_POINT ( 'NONE',  ( -92.34999999999999432, -209.9999999999999716, 86.58687500173429896 ) ) ;
#8888 = ORIENTED_EDGE ( 'NONE', *, *, #51771, .T. ) ;
#8889 = LINE ( 'NONE', #42734, #72255 ) ;
#8890 = ORIENTED_EDGE ( 'NONE', *, *, #71338, .F. ) ;
#8891 = CARTESIAN_POINT ( 'NONE',  ( -96.32500000000001705, 87.70503267997129626, 82.56520833506762358 ) ) ;
#8892 = ORIENTED_EDGE ( 'NONE', *, *, #22702, .F. ) ;
#8893 = CARTESIAN_POINT ( 'NONE',  ( 93.84685191531248449, 91.99731107132950569, 87.79072916753381151 ) ) ;
#8894 = DIRECTION ( 'NONE',  ( 1.000000000000000000, -0.000000000000000000, 0.000000000000000000 ) ) ;
#8895 = CARTESIAN_POINT ( 'NONE',  ( -7.499999999999969802, 76.30000000000001137, -204.9999999999999716 ) ) ;
#8896 = AXIS2_PLACEMENT_3D ( 'NONE', #33948, #72665, #21168 ) ;
#8897 = EDGE_CURVE ( 'NONE', #73838, #1522, #8555, .T. ) ;
#8898 = DIRECTION ( 'NONE',  ( -1.000000000000000000, -0.000000000000000000, 0.000000000000000000 ) ) ;
#8899 = CARTESIAN_POINT ( 'NONE',  ( 97.65000000000006253, 88.47002178664757821, 88.99458333333333826 ) ) ;
#8900 = ADVANCED_FACE ( 'NONE', ( #64231 ), #47304, .F. ) ;
#8901 = CARTESIAN_POINT ( 'NONE',  ( 2.861260715122138586E-12, -120.0000000000000000, -75.00000000000000000 ) ) ;
#8902 = EDGE_LOOP ( 'NONE', ( #61469, #24181, #17598, #56020 ) ) ;
#8903 = CARTESIAN_POINT ( 'NONE',  ( 0.000000000000000000, 0.000000000000000000, 42.00000000000001421 ) ) ;
#8904 = DIRECTION ( 'NONE',  ( -1.000000000000000000, 0.000000000000000000, -0.000000000000000000 ) ) ;
#8905 = ORIENTED_EDGE ( 'NONE', *, *, #43896, .T. ) ;
#8906 = EDGE_CURVE ( 'NONE', #42522, #22100, #70571, .T. ) ;
#8907 = ORIENTED_EDGE ( 'NONE', *, *, #12719, .F. ) ;
#8908 = DIRECTION ( 'NONE',  ( -3.061616997868382648E-16, -1.000000000000000000, 0.000000000000000000 ) ) ;
#8909 = EDGE_CURVE ( 'NONE', #7754, #3179, #52940, .T. ) ;
#8910 = LINE ( 'NONE', #32568, #42008 ) ;
#8911 = VECTOR ( 'NONE', #30350, 1000.000000000000000 ) ;
#8912 = DIRECTION ( 'NONE',  ( -0.000000000000000000, 0.8090169943749426773, -0.5877852522924796874 ) ) ;
#8913 = EDGE_CURVE ( 'NONE', #56500, #64668, #21794, .T. ) ;
#8914 = CARTESIAN_POINT ( 'NONE',  ( -96.15314808468745866, -211.9973110713294489, 85.46239583420047836 ) ) ;
#8915 = EDGE_LOOP ( 'NONE', ( #58379, #71808, #12743, #71647 ) ) ;
#8916 = DIRECTION ( 'NONE',  ( 1.000000000000000000, 0.000000000000000000, 0.000000000000000000 ) ) ;
#8917 = ORIENTED_EDGE ( 'NONE', *, *, #16462, .T. ) ;
#8918 = CARTESIAN_POINT ( 'NONE',  ( 0.000000000000000000, -70.53064760720336324, 26.01480285779810231 ) ) ;
#8919 = VECTOR ( 'NONE', #64363, 1000.000000000000000 ) ;
#8920 = DIRECTION ( 'NONE',  ( -1.000000000000000000, 0.000000000000000000, 0.000000000000000000 ) ) ;
#8921 = CARTESIAN_POINT ( 'NONE',  ( 19.12409105625796357, -101.5943176906707919, -2.500000000000000000 ) ) ;
#8922 = CARTESIAN_POINT ( 'NONE',  ( 96.15314808468748708, 88.00268892867053694, 76.51947916753380241 ) ) ;
#8923 = LINE ( 'NONE', #31841, #26855 ) ;
#8924 = DIRECTION ( 'NONE',  ( 0.000000000000000000, -0.2079116908177554846, 0.9781476007338064660 ) ) ;
#8925 = DIRECTION ( 'NONE',  ( 1.000000000000000000, -0.000000000000000000, 0.000000000000000000 ) ) ;
#8926 = CARTESIAN_POINT ( 'NONE',  ( -7.500000000000011546, -62.04836822995428491, -270.0000000000000000 ) ) ;
#8927 = CARTESIAN_POINT ( 'NONE',  ( 3.429551818649054340, -146.3199197248623875, -5.500000000000000000 ) ) ;
#8928 = DIRECTION ( 'NONE',  ( 0.000000000000000000, -0.7604059656000227152, -0.6494480483301933171 ) ) ;
#8929 = AXIS2_PLACEMENT_3D ( 'NONE', #69891, #63909, #35325 ) ;
#8930 = AXIS2_PLACEMENT_3D ( 'NONE', #72995, #15879, #16612 ) ;
#8931 = LINE ( 'NONE', #55162, #57629 ) ;
#8932 = DIRECTION ( 'NONE',  ( -1.000000000000000000, 0.000000000000000000, -0.000000000000000000 ) ) ;
#8933 = ORIENTED_EDGE ( 'NONE', *, *, #58938, .T. ) ;
#8934 = VECTOR ( 'NONE', #22624, 1000.000000000000000 ) ;
#8935 = CARTESIAN_POINT ( 'NONE',  ( -92.69370383062505425, 91.33154071421968467, 81.75822916753381264 ) ) ;
#8936 = EDGE_CURVE ( 'NONE', #10371, #66496, #54231, .T. ) ;
#8938 = ADVANCED_FACE ( 'NONE', ( #24734, #59318 ), #19457, .T. ) ;
#8937 = AXIS2_PLACEMENT_3D ( 'NONE', #5262, #34181, #750 ) ;
#8939 = CARTESIAN_POINT ( 'NONE',  ( 3.000000000000000000, 1.467624384280025174, -2.542000000000001592 ) ) ;
#8940 = CIRCLE ( 'NONE', #40023, 16.00000000000000000 ) ;
#8941 = PLANE ( 'NONE',  #58222 ) ;
#8942 = EDGE_CURVE ( 'NONE', #16444, #57918, #44634, .T. ) ;
#8943 = CIRCLE ( 'NONE', #5369, 15.99999999999999822 ) ;
#8944 = ORIENTED_EDGE ( 'NONE', *, *, #19014, .F. ) ;
#8945 = DIRECTION ( 'NONE',  ( -1.000000000000000000, 0.000000000000000000, 0.000000000000000000 ) ) ;
#8946 = DIRECTION ( 'NONE',  ( 0.000000000000000000, 0.000000000000000000, 1.000000000000000000 ) ) ;
#8947 = DIRECTION ( 'NONE',  ( 1.000000000000000000, -0.000000000000000000, 0.000000000000000000 ) ) ;
#8948 = CIRCLE ( 'NONE', #18548, 77.49899999999999523 ) ;
#8949 = DIRECTION ( 'NONE',  ( -1.000000000000000000, 0.000000000000000000, 0.000000000000000000 ) ) ;
#8950 = CARTESIAN_POINT ( 'NONE',  ( 92.69370383062501162, -208.6684592857803011, 80.22364583420048234 ) ) ;
#8951 = VERTEX_POINT ( 'NONE', #3310 ) ;
#8952 = ORIENTED_EDGE ( 'NONE', *, *, #60130, .F. ) ;
#8953 = CARTESIAN_POINT ( 'NONE',  ( -6.880223345695647197, -142.5202692415819854, 5.500000000000000000 ) ) ;
#8954 = DIRECTION ( 'NONE',  ( -1.000000000000000000, 0.000000000000000000, -0.000000000000000000 ) ) ;
#8955 = DIRECTION ( 'NONE',  ( -2.603472992746261562E-14, -2.546204323184492723E-14, 1.000000000000000000 ) ) ;
#8956 = ORIENTED_EDGE ( 'NONE', *, *, #38614, .F. ) ;
#8957 = CARTESIAN_POINT ( 'NONE',  ( 0.000000000000000000, 2.935248768560057897, -3.252606517456513302E-15 ) ) ;
#8958 = CARTESIAN_POINT ( 'NONE',  ( 92.69370383062501162, -208.6684592857803011, 76.41364583420049428 ) ) ;
#8959 = ORIENTED_EDGE ( 'NONE', *, *, #28802, .F. ) ;
#8960 = CARTESIAN_POINT ( 'NONE',  ( 10.00000000000000000, 0.000000000000000000, 0.000000000000000000 ) ) ;
#8961 = VERTEX_POINT ( 'NONE', #49871 ) ;
#8962 = ORIENTED_EDGE ( 'NONE', *, *, #61110, .T. ) ;
#8963 = CARTESIAN_POINT ( 'NONE',  ( -97.65000000000001990, 90.00000000000004263, 83.01499999999998636 ) ) ;
#8964 = CIRCLE ( 'NONE', #36548, 31.99999999999998224 ) ;
#8965 =( NAMED_UNIT ( * ) SI_UNIT ( $, .STERADIAN. ) SOLID_ANGLE_UNIT ( ) );
#8966 = DIRECTION ( 'NONE',  ( -1.000000000000000000, 0.000000000000000000, 0.000000000000000000 ) ) ;
#8967 = VERTEX_POINT ( 'NONE', #26943 ) ;
#8968 = CARTESIAN_POINT ( 'NONE',  ( 5.000000000000002665, 80.55351364060589958, 15.33399622253511829 ) ) ;
#8969 = CARTESIAN_POINT ( 'NONE',  ( 93.67500000000001137, -212.2949673200287179, 81.29520833506762756 ) ) ;
#8970 = CARTESIAN_POINT ( 'NONE',  ( 97.64999999999997726, 91.52997821335252127, 84.65541666666666742 ) ) ;
#8971 = ORIENTED_EDGE ( 'NONE', *, *, #45406, .T. ) ;
#8972 = LINE ( 'NONE', #66497, #29858 ) ;
#8973 = CARTESIAN_POINT ( 'NONE',  ( 2.499999999999979572, -90.00000000000000000, -310.0000000000000000 ) ) ;
#8974 = ORIENTED_EDGE ( 'NONE', *, *, #63035, .F. ) ;
#8975 = ORIENTED_EDGE ( 'NONE', *, *, #39970, .F. ) ;
#8976 = CARTESIAN_POINT ( 'NONE',  ( -92.69370383062504004, 90.00000000000004263, 86.94406250086716170 ) ) ;
#8977 = CARTESIAN_POINT ( 'NONE',  ( 97.30629616937498838, 91.33154071421968467, 81.75822916753381264 ) ) ;
#8978 = VECTOR ( 'NONE', #50862, 1000.000000000000000 ) ;
#8979 = EDGE_LOOP ( 'NONE', ( #68718, #68039, #14338, #53202 ) ) ;
#8980 = CARTESIAN_POINT ( 'NONE',  ( 97.64999999999999147, 90.00000000000002842, 81.50687500173430067 ) ) ;
#8981 = DIRECTION ( 'NONE',  ( 2.603472992746261562E-14, 2.546204323184492723E-14, -1.000000000000000000 ) ) ;
#8982 = VERTEX_POINT ( 'NONE', #31842 ) ;
#8983 = FACE_BOUND ( 'NONE', #3745, .T. ) ;
#8984 = CIRCLE ( 'NONE', #51016, 37.49900000000000233 ) ;
#8985 = ORIENTED_EDGE ( 'NONE', *, *, #29586, .F. ) ;
#8986 = ORIENTED_EDGE ( 'NONE', *, *, #40752, .T. ) ;
#8987 = EDGE_CURVE ( 'NONE', #25052, #60133, #72434, .T. ) ;
#8988 = ORIENTED_EDGE ( 'NONE', *, *, #42369, .F. ) ;
#8989 = LINE ( 'NONE', #19521, #10930 ) ;
#8990 = EDGE_CURVE ( 'NONE', #5309, #2536, #72792, .T. ) ;
#8991 = VERTEX_POINT ( 'NONE', #48770 ) ;
#8992 = CARTESIAN_POINT ( 'NONE',  ( -94.99999999999997158, -209.9999999999999716, 90.00000000000000000 ) ) ;
#8993 = CARTESIAN_POINT ( 'NONE',  ( 96.32499999999997442, 92.29496732002878900, 87.96270833506763154 ) ) ;
#8994 = ORIENTED_EDGE ( 'NONE', *, *, #43037, .F. ) ;
#8995 = DIRECTION ( 'NONE',  ( -1.000000000000000000, 0.000000000000000000, -0.000000000000000000 ) ) ;
#8996 = CARTESIAN_POINT ( 'NONE',  ( -96.15314808468745866, -211.9973110713294489, 80.22364583420046813 ) ) ;
#8998 = ORIENTED_EDGE ( 'NONE', *, *, #73691, .T. ) ;
#8997 = ADVANCED_FACE ( 'NONE', ( #32949 ), #2948, .T. ) ;
#8999 = CARTESIAN_POINT ( 'NONE',  ( 0.000000000000000000, 65.64334221924964652, -41.19522573413665611 ) ) ;
#9000 = CARTESIAN_POINT ( 'NONE',  ( 15.00000000000000000, 16.83928648764945635, 16.46020748918027010 ) ) ;
#9001 = FACE_OUTER_BOUND ( 'NONE', #51790, .T. ) ;
#9002 = CARTESIAN_POINT ( 'NONE',  ( -92.34999999999998010, -210.0000217321222635, 89.12687425009517028 ) ) ;
#9003 = VECTOR ( 'NONE', #20553, 1000.000000000000000 ) ;
#9004 = LINE ( 'NONE', #26285, #70368 ) ;
#9005 = DIRECTION ( 'NONE',  ( 1.000000000000000000, 0.000000000000000000, 0.000000000000000000 ) ) ;
#9006 = CARTESIAN_POINT ( 'NONE',  ( 96.15314808468748708, 88.00268892867053694, 88.58447916753381435 ) ) ;
#9007 = DIRECTION ( 'NONE',  ( -1.000000000000000000, 0.000000000000000000, 0.000000000000000000 ) ) ;
#9008 = DIRECTION ( 'NONE',  ( 0.000000000000000000, 0.000000000000000000, 1.000000000000000000 ) ) ;
#9009 = CARTESIAN_POINT ( 'NONE',  ( 11.99999999999999822, 12.93880638057315657, 76.41127070299278046 ) ) ;
#9010 = ADVANCED_FACE ( 'NONE', ( #14558 ), #20937, .T. ) ;
#9011 = DIRECTION ( 'NONE',  ( 0.000000000000000000, -0.4539904997395541875, 0.8910065241883642351 ) ) ;
#9012 = ADVANCED_FACE ( 'NONE', ( #54415 ), #55152, .T. ) ;
#9013 = CARTESIAN_POINT ( 'NONE',  ( 0.000000000000000000, -0.8299999999999999600, -1.199999999999999956 ) ) ;
#9014 = CARTESIAN_POINT ( 'NONE',  ( 94.99999999999998579, 86.94004357329502852, 76.18874999999999886 ) ) ;
#9015 = DIRECTION ( 'NONE',  ( 1.000000000000000000, 0.000000000000000000, 0.000000000000000000 ) ) ;
#9016 = DIRECTION ( 'NONE',  ( -0.000000000000000000, -0.000000000000000000, 1.000000000000000000 ) ) ;
#9017 = DIRECTION ( 'NONE',  ( -0.000000000000000000, -0.000000000000000000, 1.000000000000000000 ) ) ;
#9018 = DIRECTION ( 'NONE',  ( 1.000000000000000000, 0.000000000000000000, 0.000000000000000000 ) ) ;
#9019 = EDGE_CURVE ( 'NONE', #42337, #62167, #58891, .T. ) ;
#9020 = EDGE_CURVE ( 'NONE', #56782, #32186, #28158, .T. ) ;
#9021 = DIRECTION ( 'NONE',  ( -0.2079116908177527367, 0.000000000000000000, 0.9781476007338070211 ) ) ;
#9022 = DIRECTION ( 'NONE',  ( 7.962523111839282146E-16, -1.065814103640130873E-14, -1.000000000000000000 ) ) ;
#9023 = CARTESIAN_POINT ( 'NONE',  ( -96.32499999999996021, -212.2949673200287179, 88.83583333333334053 ) ) ;
#9024 = DIRECTION ( 'NONE',  ( -0.000000000000000000, -0.000000000000000000, 1.000000000000000000 ) ) ;
#9025 = ORIENTED_EDGE ( 'NONE', *, *, #723, .T. ) ;
#9026 = AXIS2_PLACEMENT_3D ( 'NONE', #63429, #11903, #675 ) ;
#9027 = DIRECTION ( 'NONE',  ( 0.000000000000000000, -6.982962677686267499E-15, 1.000000000000000000 ) ) ;
#9028 = VECTOR ( 'NONE', #22208, 1000.000000000000000 ) ;
#9029 = DIRECTION ( 'NONE',  ( -1.000000000000000000, 0.000000000000000000, 0.000000000000000000 ) ) ;
#9030 = CARTESIAN_POINT ( 'NONE',  ( 7.400000000000003908, 1.056673655987569448E-14, 5.892267102770835596E-15 ) ) ;
#9031 = CARTESIAN_POINT ( 'NONE',  ( 11.99999999999999822, -80.55351364060599906, 15.33399622253457295 ) ) ;
#9032 = CIRCLE ( 'NONE', #46290, 82.00000000000000000 ) ;
#9033 = ORIENTED_EDGE ( 'NONE', *, *, #44039, .T. ) ;
#9034 = CIRCLE ( 'NONE', #4400, 31.99999999999998579 ) ;
#9035 = VERTEX_POINT ( 'NONE', #37508 ) ;
#9036 = DIRECTION ( 'NONE',  ( -1.000000000000000000, -1.390371824233641368E-16, 0.000000000000000000 ) ) ;
#9037 = FACE_OUTER_BOUND ( 'NONE', #15125, .T. ) ;
#9038 = ORIENTED_EDGE ( 'NONE', *, *, #52804, .F. ) ;
#9039 =( BOUNDED_CURVE ( )  B_SPLINE_CURVE ( 2, ( #44345, #32299, #20666, #55987, #4139, #43617, #15388, #9758, #56375 ),
 .UNSPECIFIED., .F., .F. ) 
 B_SPLINE_CURVE_WITH_KNOTS ( ( 3, 2, 2, 2, 3 ),
 ( 0.1058364832022826857, 0.1128922486541179271, 0.1199480141950002854, 0.1270037797358826437, 0.1270039290051391268 ),
 .UNSPECIFIED. ) 
 CURVE ( )  GEOMETRIC_REPRESENTATION_ITEM ( )  RATIONAL_B_SPLINE_CURVE ( ( 1.000000000000000000, 0.8660254037844387076, 1.000000000000000000, 0.8660254037844387076, 1.000000000000000000, 0.8660254037844387076, 1.000000000000000000, 0.9999971656812787213, 0.9999943314824810692 ) ) 
 REPRESENTATION_ITEM ( '' )  );
#9040 = CARTESIAN_POINT ( 'NONE',  ( 95.00000000000000000, -212.6630814284392557, 82.81656250086712134 ) ) ;
#9041 = CARTESIAN_POINT ( 'NONE',  ( 93.84685191531251292, -211.9973110713294489, 84.19239583420049655 ) ) ;
#9042 = VERTEX_POINT ( 'NONE', #66446 ) ;
#9043 = AXIS2_PLACEMENT_3D ( 'NONE', #17778, #7253, #34701 ) ;
#9044 = CARTESIAN_POINT ( 'NONE',  ( 97.30629616937498838, -209.9999999999999716, 86.94406250086716170 ) ) ;
#9045 = EDGE_LOOP ( 'NONE', ( #64652, #1106, #70017 ) ) ;
#9046 = FACE_BOUND ( 'NONE', #55309, .T. ) ;
#9047 = ORIENTED_EDGE ( 'NONE', *, *, #73510, .F. ) ;
#9048 = CARTESIAN_POINT ( 'NONE',  ( -96.15314808468751551, 88.00268892867056536, 76.57239583420049200 ) ) ;
#9049 = ORIENTED_EDGE ( 'NONE', *, *, #7869, .T. ) ;
#9050 = AXIS2_PLACEMENT_3D ( 'NONE', #74206, #46381, #39638 ) ;
#9051 = ORIENTED_EDGE ( 'NONE', *, *, #52128, .F. ) ;
#9052 = FACE_OUTER_BOUND ( 'NONE', #3794, .T. ) ;
#9053 = ORIENTED_EDGE ( 'NONE', *, *, #55746, .T. ) ;
#9054 = DIRECTION ( 'NONE',  ( -1.000000000000000000, 0.000000000000000000, 0.000000000000000000 ) ) ;
#9055 = DIRECTION ( 'NONE',  ( -1.000000000000000000, -0.000000000000000000, 0.000000000000000000 ) ) ;
#9056 = EDGE_LOOP ( 'NONE', ( #6093, #21507, #47476, #36442 ) ) ;
#9057 = DIRECTION ( 'NONE',  ( -1.000000000000000000, 0.000000000000000000, 0.000000000000000000 ) ) ;
#9058 = ADVANCED_FACE ( 'NONE', ( #72069 ), #14930, .T. ) ;
#9059 = ORIENTED_EDGE ( 'NONE', *, *, #73261, .T. ) ;
#9060 = CARTESIAN_POINT ( 'NONE',  ( 95.00000000000000000, -213.0599564267049857, 81.34812500173430294 ) ) ;
#9061 = ORIENTED_EDGE ( 'NONE', *, *, #60701, .F. ) ;
#9062 = ADVANCED_FACE ( 'NONE', ( #43156 ), #26578, .F. ) ;
#9063 = VERTEX_POINT ( 'NONE', #38613 ) ;
#9064 = ORIENTED_EDGE ( 'NONE', *, *, #8601, .T. ) ;
#9065 = CARTESIAN_POINT ( 'NONE',  ( 92.69370383062501162, -208.6684592857803011, 80.06489583420047040 ) ) ;
#9066 = FACE_OUTER_BOUND ( 'NONE', #30586, .T. ) ;
#9067 = CONTEXT_DEPENDENT_SHAPE_REPRESENTATION ( #30180, #28415 ) ;
#9068 = DIRECTION ( 'NONE',  ( 1.000000000000000000, 0.000000000000000000, 0.000000000000000000 ) ) ;
#9069 = EDGE_LOOP ( 'NONE', ( #46542, #23231 ) ) ;
#9070 = VERTEX_POINT ( 'NONE', #54786 ) ;
#9071 = EDGE_CURVE ( 'NONE', #46914, #39517, #3691, .T. ) ;
#9072 = ORIENTED_EDGE ( 'NONE', *, *, #57148, .F. ) ;
#9073 = PLANE ( 'NONE',  #72090 ) ;
#9074 = CARTESIAN_POINT ( 'NONE',  ( 97.64999999999999147, 90.00000000000002842, 90.00000000000000000 ) ) ;
#9075 = EDGE_CURVE ( 'NONE', #3167, #38633, #60806, .T. ) ;
#9076 = CARTESIAN_POINT ( 'NONE',  ( -96.15314808468752972, 91.99731107132950569, 78.26572916753382003 ) ) ;
#9077 = VERTEX_POINT ( 'NONE', #73179 ) ;
#9078 = CARTESIAN_POINT ( 'NONE',  ( 93.84685191531248449, 91.99731107132950569, 78.10697916753380809 ) ) ;
#9079 = ORIENTED_EDGE ( 'NONE', *, *, #54247, .T. ) ;
#9080 = SURFACE_STYLE_FILL_AREA ( #72225 ) ;
#9081 = CARTESIAN_POINT ( 'NONE',  ( 0.000000000000000000, 0.000000000000000000, 0.000000000000000000 ) ) ;
#9082 = EDGE_CURVE ( 'NONE', #44963, #47803, #16882, .T. ) ;
#9083 = LINE ( 'NONE', #25638, #51803 ) ;
#9084 = AXIS2_PLACEMENT_3D ( 'NONE', #29504, #41181, #52440 ) ;
#9085 = CARTESIAN_POINT ( 'NONE',  ( 15.00000000000000000, -19.89357724625003598, -12.59942793731059041 ) ) ;
#9086 = DIRECTION ( 'NONE',  ( 0.000000000000000000, 0.000000000000000000, -1.000000000000000000 ) ) ;
#9087 = CARTESIAN_POINT ( 'NONE',  ( -93.84685191531247028, -211.9973110713294489, 84.13947916753380696 ) ) ;
#9088 = CARTESIAN_POINT ( 'NONE',  ( 0.000000000000000000, -50.95692526931286181, -58.39081064771806240 ) ) ;
#9089 = CARTESIAN_POINT ( 'NONE',  ( 7.543218489614351263, -11.91259227951415056, -1.199999999999999956 ) ) ;
#9090 = AXIS2_PLACEMENT_3D ( 'NONE', #22770, #5486, #28383 ) ;
#9091 = DIRECTION ( 'NONE',  ( -1.000000000000000000, -0.000000000000000000, 0.000000000000000000 ) ) ;
#9092 = ORIENTED_EDGE ( 'NONE', *, *, #30363, .T. ) ;
#9093 = CIRCLE ( 'NONE', #51112, 82.00000000000000000 ) ;
#9094 = VERTEX_POINT ( 'NONE', #50999 ) ;
#9095 = DIRECTION ( 'NONE',  ( -0.000000000000000000, -0.000000000000000000, 1.000000000000000000 ) ) ;
#9096 = CARTESIAN_POINT ( 'NONE',  ( 96.32499999999997442, 92.29496732002878900, 84.70833333333332860 ) ) ;
#9097 = EDGE_CURVE ( 'NONE', #67138, #40854, #74302, .T. ) ;
#9098 = CARTESIAN_POINT ( 'NONE',  ( 5.000000000000002665, -3.894527615418464705, 81.90746397400387480 ) ) ;
#9099 = EDGE_CURVE ( 'NONE', #61610, #58013, #22901, .T. ) ;
#9100 = CARTESIAN_POINT ( 'NONE',  ( -97.30629616937501680, 91.33154071421968467, 85.14489583420048291 ) ) ;
#9101 = CARTESIAN_POINT ( 'NONE',  ( 10.00000000000000000, 0.000000000000000000, 0.000000000000000000 ) ) ;
#9102 = DIRECTION ( 'NONE',  ( 0.9827303690289279636, 0.1850432970638682395, 0.000000000000000000 ) ) ;
#9103 = CIRCLE ( 'NONE', #29534, 16.00000000000000000 ) ;
#9104 = AXIS2_PLACEMENT_3D ( 'NONE', #23797, #46737, #69661 ) ;
#9105 = ORIENTED_EDGE ( 'NONE', *, *, #45797, .F. ) ;
#9106 = DIRECTION ( 'NONE',  ( 0.000000000000000000, 0.8090169943749487835, -0.5877852522924713607 ) ) ;
#9107 = CARTESIAN_POINT ( 'NONE',  ( 10.00000000000000000, 62.20884554314086046, -46.21855187248561236 ) ) ;
#9108 = DIRECTION ( 'NONE',  ( 0.000000000000000000, 0.7604059656000322631, -0.6494480483301821039 ) ) ;
#9109 = CARTESIAN_POINT ( 'NONE',  ( 10.00000000000000000, -8.840884882374576037, -74.65374052328658649 ) ) ;
#9110 = CARTESIAN_POINT ( 'NONE',  ( -94.99999999999997158, -209.9999999999999716, 90.00000000000000000 ) ) ;
#9111 = AXIS2_PLACEMENT_3D ( 'NONE', #16623, #21890, #16251 ) ;
#9112 = DIRECTION ( 'NONE',  ( -1.000000000000000000, -0.000000000000000000, -0.000000000000000000 ) ) ;
#9113 = CARTESIAN_POINT ( 'NONE',  ( -97.30629616937497417, -208.6684592857803011, 84.03364583420049883 ) ) ;
#9114 = SURFACE_STYLE_USAGE ( .BOTH. , #37702 ) ;
#9115 = CARTESIAN_POINT ( 'NONE',  ( -92.34999999999999432, -211.5299782133524218, 87.16895833506762870 ) ) ;
#9116 = DIRECTION ( 'NONE',  ( -1.000000000000000000, -0.000000000000000000, 0.000000000000000000 ) ) ;
#9117 = CARTESIAN_POINT ( 'NONE',  ( 2.500000000000029754, 73.00000000000001421, -208.2999999999999261 ) ) ;
#9118 = FACE_OUTER_BOUND ( 'NONE', #70268, .T. ) ;
#9119 = ORIENTED_EDGE ( 'NONE', *, *, #17264, .T. ) ;
#9120 = DIRECTION ( 'NONE',  ( -0.9781476007338042455, -0.2079116908177664758, 0.000000000000000000 ) ) ;
#9121 = FACE_OUTER_BOUND ( 'NONE', #8320, .T. ) ;
#9122 = CARTESIAN_POINT ( 'NONE',  ( 10.00000000000000000, 10.41901085202078114, 40.68715046381932865 ) ) ;
#9123 = DIRECTION ( 'NONE',  ( -1.000000000000000000, 0.000000000000000000, 0.000000000000000000 ) ) ;
#9124 = ORIENTED_EDGE ( 'NONE', *, *, #5473, .F. ) ;
#9125 = CARTESIAN_POINT ( 'NONE',  ( -97.64998530153629019, 91.52998669951453792, 76.05645774805350356 ) ) ;
#9126 = ORIENTED_EDGE ( 'NONE', *, *, #61726, .F. ) ;
#9127 = CARTESIAN_POINT ( 'NONE',  ( 11.99999999999999822, 65.59268652807210742, 36.72794159290264560 ) ) ;
#9128 = CARTESIAN_POINT ( 'NONE',  ( 97.65000000000009095, -208.4700217866475214, 85.92541666666664923 ) ) ;
#9129 = VECTOR ( 'NONE', #7612, 1000.000000000000227 ) ;
#9130 = EDGE_LOOP ( 'NONE', ( #30669, #34625, #1709, #43592 ) ) ;
#9131 = EDGE_CURVE ( 'NONE', #5742, #7138, #10866, .T. ) ;
#9132 = ORIENTED_EDGE ( 'NONE', *, *, #22914, .T. ) ;
#9133 = CARTESIAN_POINT ( 'NONE',  ( -2.500000000000015543, -73.00000000000001421, -201.6999999999999602 ) ) ;
#9134 = VERTEX_POINT ( 'NONE', #29164 ) ;
#9135 = ORIENTED_EDGE ( 'NONE', *, *, #24462, .F. ) ;
#9136 = EDGE_CURVE ( 'NONE', #34500, #4731, #32473, .T. ) ;
#9137 = AXIS2_PLACEMENT_3D ( 'NONE', #33608, #61827, #4696 ) ;
#9138 = ORIENTED_EDGE ( 'NONE', *, *, #14680, .T. ) ;
#9139 = VERTEX_POINT ( 'NONE', #11154 ) ;
#9140 = CARTESIAN_POINT ( 'NONE',  ( -22.53294031248082163, -134.0273518838794757, -5.500000000000000000 ) ) ;
#9141 = EDGE_CURVE ( 'NONE', #4678, #4428, #46874, .T. ) ;
#9142 = VERTEX_POINT ( 'NONE', #45001 ) ;
#9143 = PRODUCT_DEFINITION_SHAPE ( 'NONE', 'NONE',  #31551 ) ;
#9144 = VECTOR ( 'NONE', #46647, 1000.000000000000000 ) ;
#9145 = CIRCLE ( 'NONE', #30757, 31.99999999999998934 ) ;
#9146 = ORIENTED_EDGE ( 'NONE', *, *, #50430, .F. ) ;
#9147 = CARTESIAN_POINT ( 'NONE',  ( 96.15314808468748708, 91.99731107132950569, 75.61989583420049144 ) ) ;
#9148 = FACE_BOUND ( 'NONE', #9069, .T. ) ;
#9149 = CARTESIAN_POINT ( 'NONE',  ( -100.0000000000000142, 85.00000000000002842, 90.00000000000000000 ) ) ;
#9150 = ORIENTED_EDGE ( 'NONE', *, *, #58047, .T. ) ;
#9151 = EDGE_CURVE ( 'NONE', #58172, #63936, #647, .T. ) ;
#9152 = ORIENTED_EDGE ( 'NONE', *, *, #33861, .F. ) ;
#9153 = EDGE_LOOP ( 'NONE', ( #8956, #49579, #9411, #1338 ) ) ;
#9154 = FACE_OUTER_BOUND ( 'NONE', #32063, .T. ) ;
#9155 = ORIENTED_EDGE ( 'NONE', *, *, #38356, .F. ) ;
#9156 = CARTESIAN_POINT ( 'NONE',  ( 97.64999999999999147, -211.0689600337108516, 74.48490336299447279 ) ) ;
#9157 = DIRECTION ( 'NONE',  ( -7.678525154775187278E-18, -1.934875936422313489E-17, 0.9999999999999998890 ) ) ;
#9158 = DIRECTION ( 'NONE',  ( 0.000000000000000000, 0.1564344650402244019, 0.9876883405951387696 ) ) ;
#9159 = VECTOR ( 'NONE', #70324, 1000.000000000000000 ) ;
#9160 = DIRECTION ( 'NONE',  ( -0.000000000000000000, -0.000000000000000000, 1.000000000000000000 ) ) ;
#9161 = CARTESIAN_POINT ( 'NONE',  ( -8.000000000000023093, 2.103003552093192713E-13, 20.19999999999999574 ) ) ;
#9162 = DIRECTION ( 'NONE',  ( 0.000000000000000000, 0.000000000000000000, 1.000000000000000000 ) ) ;
#9163 = FACE_OUTER_BOUND ( 'NONE', #810, .T. ) ;
#9164 = DIRECTION ( 'NONE',  ( -1.000000000000000000, -0.000000000000000000, 0.000000000000000000 ) ) ;
#9165 = CARTESIAN_POINT ( 'NONE',  ( -93.67499999999998295, -212.2949673200287179, 75.68604166840097491 ) ) ;
#9166 = CARTESIAN_POINT ( 'NONE',  ( -92.69370383062502583, 91.33154071421968467, 88.90197916753382401 ) ) ;
#9167 = ORIENTED_EDGE ( 'NONE', *, *, #26303, .F. ) ;
#9168 = UNCERTAINTY_MEASURE_WITH_UNIT (LENGTH_MEASURE( 1.000000000000000082E-05 ), #64422, 'distance_accuracy_value', 'NONE');
#9170 = CARTESIAN_POINT ( 'NONE',  ( -97.30629616937501680, 88.66845928578038638, 88.42572916753380241 ) ) ;
#9169 = CARTESIAN_POINT ( 'NONE',  ( 94.99999999999998579, 87.33691857156068750, 88.53156250086713897 ) ) ;
#9171 = ORIENTED_EDGE ( 'NONE', *, *, #2505, .T. ) ;
#9172 = CARTESIAN_POINT ( 'NONE',  ( 97.30629616937498838, 88.66845928578037217, 76.73114583420048973 ) ) ;
#9173 = EDGE_CURVE ( 'NONE', #46172, #43278, #52105, .T. ) ;
#9174 = DIRECTION ( 'NONE',  ( -1.000000000000000000, 0.000000000000000000, 0.000000000000000000 ) ) ;
#9175 = LINE ( 'NONE', #13698, #6676 ) ;
#9176 = CARTESIAN_POINT ( 'NONE',  ( 0.000000000000000000, -120.0000000000000000, -5.500000000000000000 ) ) ;
#9177 = LINE ( 'NONE', #3203, #65077 ) ;
#9178 = DIRECTION ( 'NONE',  ( -1.000000000000000000, -0.000000000000000000, -0.000000000000000000 ) ) ;
#9179 = DIRECTION ( 'NONE',  ( 0.000000000000000000, 0.000000000000000000, 1.000000000000000000 ) ) ;
#9180 = DIRECTION ( 'NONE',  ( -1.000000000000000000, 0.000000000000000000, 0.000000000000000000 ) ) ;
#9181 = ORIENTED_EDGE ( 'NONE', *, *, #43055, .F. ) ;
#9182 = VECTOR ( 'NONE', #43584, 1000.000000000000000 ) ;
#9183 = EDGE_LOOP ( 'NONE', ( #61514, #69800, #5956, #38867 ) ) ;
#9184 = CARTESIAN_POINT ( 'NONE',  ( -95.00000000000002842, 86.94004357329504273, 80.63375000000000625 ) ) ;
#9185 = EDGE_CURVE ( 'NONE', #25170, #39943, #10404, .T. ) ;
#9186 = PLANE ( 'NONE',  #39101 ) ;
#9187 = EDGE_CURVE ( 'NONE', #29480, #51502, #22434, .T. ) ;
#9188 = CARTESIAN_POINT ( 'NONE',  ( 4.999999999999999112, 38.55633173627034438, -16.65560815589369881 ) ) ;
#9189 = DIRECTION ( 'NONE',  ( -1.000000000000000000, -0.000000000000000000, -0.000000000000000000 ) ) ;
#9190 = CARTESIAN_POINT ( 'NONE',  ( 96.32499999999997442, 92.29496732002878900, 87.32770833506762642 ) ) ;
#9191 = DIRECTION ( 'NONE',  ( 0.000000000000000000, 0.000000000000000000, 1.000000000000000000 ) ) ;
#9192 = PLANE ( 'NONE',  #31127 ) ;
#9193 = EDGE_CURVE ( 'NONE', #28941, #40320, #23181, .T. ) ;
#9194 = AXIS2_PLACEMENT_3D ( 'NONE', #11309, #41372, #17695 ) ;
#9195 = VERTEX_POINT ( 'NONE', #68302 ) ;
#9196 = CARTESIAN_POINT ( 'NONE',  ( -97.30629616937501680, 90.00000000000004263, 81.38781250086714181 ) ) ;
#9197 = CARTESIAN_POINT ( 'NONE',  ( 96.32499999999998863, 87.70503267997126784, 82.67104166840096013 ) ) ;
#9198 = LINE ( 'NONE', #56176, #67881 ) ;
#9199 = SURFACE_STYLE_FILL_AREA ( #44157 ) ;
#9200 = DIRECTION ( 'NONE',  ( 0.000000000000000000, 0.000000000000000000, 1.000000000000000000 ) ) ;
#9201 = FACE_BOUND ( 'NONE', #37817, .T. ) ;
#9202 = PLANE ( 'NONE',  #38241 ) ;
#9203 = VECTOR ( 'NONE', #21391, 1000.000000000000000 ) ;
#9204 = CARTESIAN_POINT ( 'NONE',  ( 50.00005079999999680, 12.24744871391589207, -2.500000000000000000 ) ) ;
#9205 = FACE_OUTER_BOUND ( 'NONE', #18582, .T. ) ;
#9206 = VECTOR ( 'NONE', #6355, 1000.000000000000000 ) ;
#9207 = CARTESIAN_POINT ( 'NONE',  ( 96.15314808468748708, 91.99731107132950569, 80.69989583420047552 ) ) ;
#9208 = CARTESIAN_POINT ( 'NONE',  ( -96.15314808468745866, -211.9973110713294489, 83.55739583420049144 ) ) ;
#9209 = LINE ( 'NONE', #3604, #39821 ) ;
#9210 = ORIENTED_EDGE ( 'NONE', *, *, #49703, .T. ) ;
#9211 = CARTESIAN_POINT ( 'NONE',  ( 11.99999999999999822, 0.000000000000000000, 0.000000000000000000 ) ) ;
#9212 = CARTESIAN_POINT ( 'NONE',  ( -93.67499999999998295, -207.7050326799711968, 76.45333333333333314 ) ) ;
#9213 = LINE ( 'NONE', #55077, #36564 ) ;
#9214 = VECTOR ( 'NONE', #34197, 1000.000000000000000 ) ;
#9215 = CARTESIAN_POINT ( 'NONE',  ( 93.84685191531249870, -208.0026889286704943, 83.18697916753382060 ) ) ;
#9216 = ORIENTED_EDGE ( 'NONE', *, *, #16193, .T. ) ;
#9217 = DIRECTION ( 'NONE',  ( -1.000000000000000000, -0.000000000000000000, -0.000000000000000000 ) ) ;
#9218 = ORIENTED_EDGE ( 'NONE', *, *, #11370, .T. ) ;
#9219 = CARTESIAN_POINT ( 'NONE',  ( -10.00000000000000000, 0.000000000000000000, 0.000000000000000000 ) ) ;
#9220 = VERTEX_POINT ( 'NONE', #39734 ) ;
#9221 = EDGE_CURVE ( 'NONE', #14488, #54604, #16043, .T. ) ;
#9222 = LINE ( 'NONE', #8496, #16568 ) ;
#9223 = CIRCLE ( 'NONE', #18824, 82.00000000000000000 ) ;
#9224 = EDGE_CURVE ( 'NONE', #34982, #38545, #28058, .T. ) ;
#9225 = CARTESIAN_POINT ( 'NONE',  ( 95.00000000000000000, -207.3369185715606307, 78.21281250086717307 ) ) ;
#9226 = EDGE_CURVE ( 'NONE', #26794, #60251, #25747, .T. ) ;
#9227 = FACE_OUTER_BOUND ( 'NONE', #59026, .T. ) ;
#9228 = CARTESIAN_POINT ( 'NONE',  ( 3.000000000000000000, -1.467624384280027838, 2.542000000000001592 ) ) ;
#9229 = CARTESIAN_POINT ( 'NONE',  ( -97.20211296432958648, 88.68334238502464473, 74.94590613650809985 ) ) ;
#9230 = CARTESIAN_POINT ( 'NONE',  ( 92.69370383062498320, 90.00000000000002842, 85.99156250086716113 ) ) ;
#9231 = VECTOR ( 'NONE', #23620, 999.9999999999998863 ) ;
#9232 = LINE ( 'NONE', #37824, #47790 ) ;
#9233 = CARTESIAN_POINT ( 'NONE',  ( 92.35000000000000853, -209.9999999999999716, 82.37999999999999545 ) ) ;
#9234 = CIRCLE ( 'NONE', #38062, 20.99999999999999645 ) ;
#9235 = EDGE_LOOP ( 'NONE', ( #60570, #11534, #14327, #6048 ) ) ;
#9236 = ADVANCED_FACE ( 'NONE', ( #61921 ), #57760, .T. ) ;
#9237 = ORIENTED_EDGE ( 'NONE', *, *, #33093, .T. ) ;
#9238 = ORIENTED_EDGE ( 'NONE', *, *, #54631, .F. ) ;
#9239 = ORIENTED_EDGE ( 'NONE', *, *, #54508, .T. ) ;
#9240 = FACE_OUTER_BOUND ( 'NONE', #23239, .T. ) ;
#9241 = SHAPE_REPRESENTATION_RELATIONSHIP ( 'NONE' , 'NONE' ,  #15311, #51651 ) ;
#9242 = CARTESIAN_POINT ( 'NONE',  ( -97.30629616937501680, 88.66845928578038638, 84.77447916753381207 ) ) ;
#9243 = AXIS2_PLACEMENT_3D ( 'NONE', #6729, #23650, #41674 ) ;
#9244 = LINE ( 'NONE', #20899, #59064 ) ;
#9245 = VECTOR ( 'NONE', #36625, 1000.000000000000000 ) ;
#9246 = FACE_OUTER_BOUND ( 'NONE', #52221, .T. ) ;
#9247 = DIRECTION ( 'NONE',  ( 0.000000000000000000, 0.9876883405951382144, -0.1564344650402276493 ) ) ;
#9248 = CYLINDRICAL_SURFACE ( 'NONE', #68029, 2.649999999999985700 ) ;
#9249 = ORIENTED_EDGE ( 'NONE', *, *, #65311, .F. ) ;
#9250 = CARTESIAN_POINT ( 'NONE',  ( -96.32499999999996021, -212.2949673200287179, 85.74020833506763495 ) ) ;
#9251 = ORIENTED_EDGE ( 'NONE', *, *, #40402, .F. ) ;
#9252 = DIRECTION ( 'NONE',  ( -0.000000000000000000, -0.000000000000000000, -1.000000000000000000 ) ) ;
#9253 = EDGE_CURVE ( 'NONE', #14738, #49489, #14451, .T. ) ;
#9254 = AXIS2_PLACEMENT_3D ( 'NONE', #29720, #12807, #69952 ) ;
#9255 = ORIENTED_EDGE ( 'NONE', *, *, #11301, .F. ) ;
#9256 = CARTESIAN_POINT ( 'NONE',  ( -93.67500000000003979, 87.70503267997129626, 82.03604166840096923 ) ) ;
#9257 =( BOUNDED_CURVE ( )  B_SPLINE_CURVE ( 2, ( #67211, #41597, #57056, #46143, #51395, #64539, #7013 ),
 .UNSPECIFIED., .F., .F. ) 
 B_SPLINE_CURVE_WITH_KNOTS ( ( 3, 2, 2, 3 ),
 ( 0.8541666666666666297, 0.8611111111111110494, 0.8680555555555554692, 0.8749999999999997780 ),
 .UNSPECIFIED. ) 
 CURVE ( )  GEOMETRIC_REPRESENTATION_ITEM ( )  RATIONAL_B_SPLINE_CURVE ( ( 1.000000000000000000, 0.8660254037844387076, 1.000000000000000000, 0.8660254037844387076, 1.000000000000000000, 0.8660254037844430375, 0.9999999999999956701 ) ) 
 REPRESENTATION_ITEM ( '' )  );
#9258 = ORIENTED_EDGE ( 'NONE', *, *, #52101, .T. ) ;
#9259 = CARTESIAN_POINT ( 'NONE',  ( 92.69370383062498320, 88.66845928578037217, 85.40947916753380298 ) ) ;
#9260 = EDGE_CURVE ( 'NONE', #46225, #73479, #27697, .T. ) ;
#9261 = AXIS2_PLACEMENT_3D ( 'NONE', #34184, #67659, #39465 ) ;
#9262 = CARTESIAN_POINT ( 'NONE',  ( 0.000000000000000000, 12.26510123303308752, -35.53030884539072787 ) ) ;
#9263 = DIRECTION ( 'NONE',  ( -2.603472992746261562E-14, -2.546204323184492723E-14, 1.000000000000000000 ) ) ;
#9264 = CARTESIAN_POINT ( 'NONE',  ( -92.98549755320794930, 88.86758821614978388, 74.79348190356850523 ) ) ;
#9265 = FACE_OUTER_BOUND ( 'NONE', #67603, .T. ) ;
#9266 = LINE ( 'NONE', #60418, #32307 ) ;
#9267 = VERTEX_POINT ( 'NONE', #24646 ) ;
#9268 = FACE_OUTER_BOUND ( 'NONE', #26072, .T. ) ;
#9269 = DIRECTION ( 'NONE',  ( 0.4565542962317865050, 0.000000000000000000, 0.8896955516311735312 ) ) ;
#9270 = EDGE_LOOP ( 'NONE', ( #43216, #60796, #43750, #52706 ) ) ;
#9271 = ORIENTED_EDGE ( 'NONE', *, *, #69519, .F. ) ;
#9272 = CYLINDRICAL_SURFACE ( 'NONE', #37925, 31.99999999999999289 ) ;
#9273 = EDGE_CURVE ( 'NONE', #39865, #32014, #13270, .T. ) ;
#9274 = DIRECTION ( 'NONE',  ( -1.000000000000000000, -0.000000000000000000, 0.000000000000000000 ) ) ;
#9275 = EDGE_CURVE ( 'NONE', #65739, #14207, #49268, .T. ) ;
#9276 = CARTESIAN_POINT ( 'NONE',  ( -3.702536634196095910, 8.043911037661889196, 42.00000000000001421 ) ) ;
#9277 = CARTESIAN_POINT ( 'NONE',  ( -94.99999999999997158, -212.6630814284392557, 86.15031250086714465 ) ) ;
#9278 = ORIENTED_EDGE ( 'NONE', *, *, #51679, .T. ) ;
#9279 = DIRECTION ( 'NONE',  ( -0.000000000000000000, -0.000000000000000000, 1.000000000000000000 ) ) ;
#9280 = ORIENTED_EDGE ( 'NONE', *, *, #42140, .T. ) ;
#9281 = CARTESIAN_POINT ( 'NONE',  ( 0.000000000000000000, 46.11716303203283474, -67.80270845531839541 ) ) ;
#9282 = FACE_OUTER_BOUND ( 'NONE', #63, .T. ) ;
#9283 = FACE_OUTER_BOUND ( 'NONE', #1801, .T. ) ;
#9284 = CARTESIAN_POINT ( 'NONE',  ( 92.69370383062498320, 91.33154071421968467, 79.42989583420047950 ) ) ;
#9285 = DIRECTION ( 'NONE',  ( 0.000000000000000000, 0.000000000000000000, 1.000000000000000000 ) ) ;
#9286 = CARTESIAN_POINT ( 'NONE',  ( 15.70000000000000284, -120.0000000000000000, -85.59999999999999432 ) ) ;
#9287 = CARTESIAN_POINT ( 'NONE',  ( 10.00000000000000000, 23.16143007188532366, -73.95703589263949596 ) ) ;
#9288 = CARTESIAN_POINT ( 'NONE',  ( 93.65592807507074724, 92.02656496471888659, 74.86703477254887673 ) ) ;
#9289 = DIRECTION ( 'NONE',  ( -1.000000000000000000, 0.000000000000000000, -0.000000000000000000 ) ) ;
#9290 = DIRECTION ( 'NONE',  ( 0.000000000000000000, 0.9510565162951521989, 0.3090169943749515591 ) ) ;
#9291 = VECTOR ( 'NONE', #25091, 1000.000000000000000 ) ;
#9292 = DIRECTION ( 'NONE',  ( -3.061616997868382648E-16, -1.000000000000000000, 0.000000000000000000 ) ) ;
#9293 = PRODUCT_DEFINITION_CONTEXT ( 'detailed design', #921, 'design' ) ;
#9294 = AXIS2_PLACEMENT_3D ( 'NONE', #36073, #53733, #2276 ) ;
#9295 = FACE_OUTER_BOUND ( 'NONE', #35570, .T. ) ;
#9296 = ORIENTED_EDGE ( 'NONE', *, *, #25138, .F. ) ;
#9297 = CARTESIAN_POINT ( 'NONE',  ( -92.69370383062504004, 90.00000000000004263, 84.24531250086714351 ) ) ;
#9298 = CYLINDRICAL_SURFACE ( 'NONE', #7161, 3.299999999999983391 ) ;
#9299 = AXIS2_PLACEMENT_3D ( 'NONE', #15844, #26374, #32743 ) ;
#9300 = VECTOR ( 'NONE', #61832, 1000.000000000000000 ) ;
#9301 = CARTESIAN_POINT ( 'NONE',  ( 11.99999999999999822, -27.74655509720725277, 77.16300072079650363 ) ) ;
#9302 = ORIENTED_EDGE ( 'NONE', *, *, #30570, .T. ) ;
#9303 = CARTESIAN_POINT ( 'NONE',  ( 92.35000000010806787, -209.9999848944895007, 78.64888723592486031 ) ) ;
#9304 = FACE_OUTER_BOUND ( 'NONE', #41574, .T. ) ;
#9305 = CARTESIAN_POINT ( 'NONE',  ( -7.500000000000015987, -76.29999999999999716, -255.0000000000000000 ) ) ;
#9306 = ADVANCED_FACE ( 'NONE', ( #41946 ), #47577, .T. ) ;
#9307 = CARTESIAN_POINT ( 'NONE',  ( -94.99999999999997158, -209.9999999999999716, 90.00000000000000000 ) ) ;
#9308 = CARTESIAN_POINT ( 'NONE',  ( 93.84685191531251292, -211.9973110713294489, 77.84239583420048803 ) ) ;
#9309 = ADVANCED_FACE ( 'NONE', ( #36662 ), #30640, .T. ) ;
#9310 = CIRCLE ( 'NONE', #70528, 31.99999999999998579 ) ;
#9311 = VERTEX_POINT ( 'NONE', #64142 ) ;
#9312 = EDGE_CURVE ( 'NONE', #39397, #32442, #63778, .T. ) ;
#9313 = ORIENTED_EDGE ( 'NONE', *, *, #32434, .T. ) ;
#9314 = DIRECTION ( 'NONE',  ( -0.000000000000000000, -0.000000000000000000, 1.000000000000000000 ) ) ;
#9315 = CARTESIAN_POINT ( 'NONE',  ( 0.000000000000000000, 2.375000000000000444, 0.000000000000000000 ) ) ;
#9316 = CARTESIAN_POINT ( 'NONE',  ( 10.00000000000000000, 0.000000000000000000, 0.000000000000000000 ) ) ;
#9317 = DIRECTION ( 'NONE',  ( 0.000000000000000000, 0.8090169943749426773, 0.5877852522924797984 ) ) ;
#9318 = CARTESIAN_POINT ( 'NONE',  ( 97.30629616937498838, -209.9999999999999716, 75.51406250086715488 ) ) ;
#9319 = EDGE_CURVE ( 'NONE', #43104, #63923, #1758, .T. ) ;
#9320 = EDGE_LOOP ( 'NONE', ( #51600, #69077, #38006, #28204 ) ) ;
#9321 = CARTESIAN_POINT ( 'NONE',  ( -96.32499999999996021, -207.7050326799711968, 87.98916666666666231 ) ) ;
#9322 = ORIENTED_EDGE ( 'NONE', *, *, #68240, .T. ) ;
#9323 = ORIENTED_EDGE ( 'NONE', *, *, #29189, .T. ) ;
#9324 = DIRECTION ( 'NONE',  ( 0.000000000000000000, 0.000000000000000000, 1.000000000000000000 ) ) ;
#9325 = SHAPE_REPRESENTATION_RELATIONSHIP ( 'NONE' , 'NONE' ,  #72820, #21132 ) ;
#9326 = CYLINDRICAL_SURFACE ( 'NONE', #551, 77.49899999999999523 ) ;
#9327 = ORIENTED_EDGE ( 'NONE', *, *, #9782, .F. ) ;
#9328 = CARTESIAN_POINT ( 'NONE',  ( 0.000000000000000000, 27.05870788708267582, -26.08949754952995903 ) ) ;
#9329 = CARTESIAN_POINT ( 'NONE',  ( 95.00000000000000000, -206.9400435732949575, 81.66562500173431260 ) ) ;
#9330 = CARTESIAN_POINT ( 'NONE',  ( 93.67499999999998295, 92.29496732002878900, 85.44916666666665606 ) ) ;
#9331 = ORIENTED_EDGE ( 'NONE', *, *, #49334, .T. ) ;
#9332 = FACE_OUTER_BOUND ( 'NONE', #68745, .T. ) ;
#9333 = CARTESIAN_POINT ( 'NONE',  ( 99.99999999999997158, -80.00000000000001421, -90.00000000000014211 ) ) ;
#9334 = ADVANCED_FACE ( 'NONE', ( #53970 ), #12253, .T. ) ;
#9335 = ORIENTED_EDGE ( 'NONE', *, *, #12557, .T. ) ;
#9336 = CARTESIAN_POINT ( 'NONE',  ( -92.35000000002612808, 89.99999999999992895, -74.99999999999992895 ) ) ;
#9337 = CARTESIAN_POINT ( 'NONE',  ( -95.00000000000002842, 87.33691857156074434, 86.15031250086717307 ) ) ;
#9338 = AXIS2_PLACEMENT_3D ( 'NONE', #46602, #63908, #12378 ) ;
#9339 = CARTESIAN_POINT ( 'NONE',  ( 94.99999999999998579, 87.33691857156068750, 82.81656250086713555 ) ) ;
#9340 = ADVANCED_FACE ( 'NONE', ( #41205 ), #31013, .T. ) ;
#9341 = ORIENTED_EDGE ( 'NONE', *, *, #33801, .F. ) ;
#9342 = AXIS2_PLACEMENT_3D ( 'NONE', #47301, #42033, #64228 ) ;
#9343 = CIRCLE ( 'NONE', #48996, 77.49899999999999523 ) ;
#9344 = DIRECTION ( 'NONE',  ( -1.000000000000000000, -0.000000000000000000, -0.000000000000000000 ) ) ;
#9345 = VERTEX_POINT ( 'NONE', #35919 ) ;
#9346 = CARTESIAN_POINT ( 'NONE',  ( 24.95699195200416654, -110.9640411295978595, -5.500000000000000000 ) ) ;
#9347 = EDGE_CURVE ( 'NONE', #47656, #61855, #120, .T. ) ;
#9348 = EDGE_CURVE ( 'NONE', #50206, #25707, #29528, .T. ) ;
#9349 = ORIENTED_EDGE ( 'NONE', *, *, #63822, .F. ) ;
#9350 = ORIENTED_EDGE ( 'NONE', *, *, #1593, .F. ) ;
#9351 = CIRCLE ( 'NONE', #51376, 77.49900000000000944 ) ;
#9352 = ORIENTED_EDGE ( 'NONE', *, *, #46965, .F. ) ;
#9353 = VECTOR ( 'NONE', #48232, 1000.000000000000000 ) ;
#9354 = LINE ( 'NONE', #3015, #52898 ) ;
#9355 = ORIENTED_EDGE ( 'NONE', *, *, #20258, .T. ) ;
#9356 = ADVANCED_FACE ( 'NONE', ( #2507 ), #52468, .T. ) ;
#9357 = CARTESIAN_POINT ( 'NONE',  ( -3.000000000000000000, -11.95096189432312350, -23.69967320028773372 ) ) ;
#9358 = PLANE ( 'NONE',  #31094 ) ;
#9359 = ORIENTED_EDGE ( 'NONE', *, *, #22404, .F. ) ;
#9360 = CARTESIAN_POINT ( 'NONE',  ( 0.000000000000000000, 22.07842321921481243, 8.187992925817422218 ) ) ;
#9361 = CARTESIAN_POINT ( 'NONE',  ( -97.30629616937497417, -211.3315407142195852, 80.17072916753379275 ) ) ;
#9362 = VERTEX_POINT ( 'NONE', #23912 ) ;
#9363 = CARTESIAN_POINT ( 'NONE',  ( -95.00000000000002842, 86.94004357329504273, 86.34874999999999545 ) ) ;
#9364 = CARTESIAN_POINT ( 'NONE',  ( 10.00000000000000000, 0.000000000000000000, 0.000000000000000000 ) ) ;
#9365 = CARTESIAN_POINT ( 'NONE',  ( 1.560000000000000053, 0.000000000000000000, 0.000000000000000000 ) ) ;
#9366 = DIRECTION ( 'NONE',  ( -1.000000000000000000, 0.000000000000000000, 0.000000000000000000 ) ) ;
#9367 = EDGE_CURVE ( 'NONE', #1777, #43566, #2487, .T. ) ;
#9368 = CARTESIAN_POINT ( 'NONE',  ( 0.000000000000000000, -89.50000000000000000, 2.500000000000000000 ) ) ;
#9369 = VECTOR ( 'NONE', #9615, 1000.000000000000000 ) ;
#9370 = DIRECTION ( 'NONE',  ( -1.000000000000000000, 0.000000000000000000, -0.000000000000000000 ) ) ;
#9372 = VECTOR ( 'NONE', #46910, 1000.000000000000000 ) ;
#9371 = CARTESIAN_POINT ( 'NONE',  ( 96.15314808468748708, 88.00268892867053694, 87.31447916753380412 ) ) ;
#9373 = CARTESIAN_POINT ( 'NONE',  ( 16.84844760790522855, -103.5491698323862124, -5.500000000000000000 ) ) ;
#9374 = CARTESIAN_POINT ( 'NONE',  ( 92.34999999999999432, 90.00003728274771220, 81.18937371225271704 ) ) ;
#9375 = AXIS2_PLACEMENT_3D ( 'NONE', #1336, #6200, #6561 ) ;
#9376 = CARTESIAN_POINT ( 'NONE',  ( -92.34999999999999432, -209.9999999999999716, 87.77749999999998920 ) ) ;
#9377 = CIRCLE ( 'NONE', #22591, 77.49899999999999523 ) ;
#9378 = DIRECTION ( 'NONE',  ( 1.000000000000000000, 0.000000000000000000, 0.000000000000000000 ) ) ;
#9379 = DIRECTION ( 'NONE',  ( -1.000000000000000000, -0.000000000000000000, 0.000000000000000000 ) ) ;
#9380 = DIRECTION ( 'NONE',  ( -0.6064928550163511956, -0.7950889364178798102, 0.000000000000000000 ) ) ;
#9381 = AXIS2_PLACEMENT_3D ( 'NONE', #62880, #38805, #21498 ) ;
#9382 = DIRECTION ( 'NONE',  ( -0.000000000000000000, 0.5000000000000039968, -0.8660254037844363761 ) ) ;
#9383 = CARTESIAN_POINT ( 'NONE',  ( 0.000000000000000000, 0.000000000000000000, 0.000000000000000000 ) ) ;
#9384 = CARTESIAN_POINT ( 'NONE',  ( 94.99999999999998579, 90.00000000000002842, 90.00000000000000000 ) ) ;
#9385 = FACE_OUTER_BOUND ( 'NONE', #52527, .T. ) ;
#9386 = CARTESIAN_POINT ( 'NONE',  ( -94.99999999999997158, -209.9999999999999716, 90.00000000000000000 ) ) ;
#9387 = CARTESIAN_POINT ( 'NONE',  ( -92.34999999999999432, -208.4700217866474645, 89.10041666666667481 ) ) ;
#9388 = CARTESIAN_POINT ( 'NONE',  ( -2.500000000000000000, 16.00000000000000000, 0.000000000000000000 ) ) ;
#9389 = AXIS2_PLACEMENT_3D ( 'NONE', #63819, #22857, #29567 ) ;
#9390 = DIRECTION ( 'NONE',  ( -1.000000000000000000, 0.000000000000000000, -0.000000000000000000 ) ) ;
#9391 = CARTESIAN_POINT ( 'NONE',  ( 95.00000000000000000, -213.0599564267049857, 78.17312500173430578 ) ) ;
#9392 = FILL_AREA_STYLE ('',( #72173 ) ) ;
#9393 = AXIS2_PLACEMENT_3D ( 'NONE', #21872, #60359, #8478 ) ;
#9394 = DIRECTION ( 'NONE',  ( -1.000000000000000000, -0.000000000000000000, -0.000000000000000000 ) ) ;
#9395 = EDGE_CURVE ( 'NONE', #44188, #24060, #12030, .T. ) ;
#9396 = CIRCLE ( 'NONE', #51432, 16.00000000000000000 ) ;
#9397 = EDGE_CURVE ( 'NONE', #34217, #44790, #58484, .T. ) ;
#9398 = AXIS2_PLACEMENT_3D ( 'NONE', #23549, #39742, #69403 ) ;
#9399 = ORIENTED_EDGE ( 'NONE', *, *, #47945, .F. ) ;
#9400 = EDGE_CURVE ( 'NONE', #7257, #33537, #40866, .T. ) ;
#9401 = EDGE_LOOP ( 'NONE', ( #54073, #46609, #21900, #33225 ) ) ;
#9402 = EDGE_CURVE ( 'NONE', #8802, #7419, #50454, .T. ) ;
#9403 = CARTESIAN_POINT ( 'NONE',  ( -35.37301231164799731, -117.0000000000000000, 2.500000000000000000 ) ) ;
#9404 = DIRECTION ( 'NONE',  ( 0.000000000000000000, -0.000000000000000000, -1.000000000000000000 ) ) ;
#9405 = ORIENTED_EDGE ( 'NONE', *, *, #55841, .T. ) ;
#9406 = CARTESIAN_POINT ( 'NONE',  ( 97.30629616937498838, -208.6684592857803295, 83.02822916753379445 ) ) ;
#9407 = CARTESIAN_POINT ( 'NONE',  ( 92.69370383062501162, -211.3315407142195852, 84.77447916753381207 ) ) ;
#9408 = EDGE_LOOP ( 'NONE', ( #5675, #64520, #68726, #3996, #73997, #51818, #74117, #71005 ) ) ;
#9409 = CARTESIAN_POINT ( 'NONE',  ( 97.30629616937498838, -208.6684592857803011, 87.63197916753382799 ) ) ;
#9410 = AXIS2_PLACEMENT_3D ( 'NONE', #17449, #22736, #44926 ) ;
#9411 = ORIENTED_EDGE ( 'NONE', *, *, #2588, .T. ) ;
#9412 = CARTESIAN_POINT ( 'NONE',  ( 97.64999999994533653, 89.99998298270493535, 88.49187441316099978 ) ) ;
#9413 = VERTEX_POINT ( 'NONE', #58869 ) ;
#9414 = CARTESIAN_POINT ( 'NONE',  ( -92.69370383062504004, 90.00000000000004263, 77.41906250086715602 ) ) ;
#9415 = CIRCLE ( 'NONE', #51448, 42.00000000000000000 ) ;
#9416 = ORIENTED_EDGE ( 'NONE', *, *, #49320, .F. ) ;
#9417 = EDGE_CURVE ( 'NONE', #20222, #51520, #60091, .T. ) ;
#9418 = ORIENTED_EDGE ( 'NONE', *, *, #34616, .T. ) ;
#9419 = CARTESIAN_POINT ( 'NONE',  ( 11.99999999999999822, 0.000000000000000000, 0.000000000000000000 ) ) ;
#9420 = CIRCLE ( 'NONE', #26269, 42.00000000000000000 ) ;
#9421 = ORIENTED_EDGE ( 'NONE', *, *, #3284, .T. ) ;
#9422 = CARTESIAN_POINT ( 'NONE',  ( 0.000000000000000000, -36.73666225445940370, 65.58780272294062286 ) ) ;
#9423 = FACE_OUTER_BOUND ( 'NONE', #37899, .T. ) ;
#9424 = EDGE_CURVE ( 'NONE', #44140, #60240, #58629, .T. ) ;
#9425 = AXIS2_PLACEMENT_3D ( 'NONE', #65440, #18807, #41748 ) ;
#9426 = EDGE_LOOP ( 'NONE', ( #33269, #56608, #19894, #63000 ) ) ;
#9427 = FACE_OUTER_BOUND ( 'NONE', #3563, .T. ) ;
#9428 = ORIENTED_EDGE ( 'NONE', *, *, #18568, .F. ) ;
#9429 = CIRCLE ( 'NONE', #61073, 22.90000000000041780 ) ;
#9430 = CARTESIAN_POINT ( 'NONE',  ( 97.64999999999324132, 90.00000598221777182, 82.14187520865721126 ) ) ;
#9431 = EDGE_LOOP ( 'NONE', ( #38871, #10379, #46703, #69712 ) ) ;
#9432 = VERTEX_POINT ( 'NONE', #72354 ) ;
#9433 = ORIENTED_EDGE ( 'NONE', *, *, #55879, .F. ) ;
#9434 = CARTESIAN_POINT ( 'NONE',  ( -4.180704885107413560, -3.359771601077115921, -5.801655677627839403 ) ) ;
#9435 = EDGE_CURVE ( 'NONE', #38100, #25802, #5126, .T. ) ;
#9436 = EDGE_CURVE ( 'NONE', #55763, #47354, #33447, .T. ) ;
#9437 = FACE_BOUND ( 'NONE', #57516, .T. ) ;
#9438 = VERTEX_POINT ( 'NONE', #54700 ) ;
#9439 = ORIENTED_EDGE ( 'NONE', *, *, #69770, .F. ) ;
#9440 = EDGE_LOOP ( 'NONE', ( #28553, #27929, #16855, #18728 ) ) ;
#9441 = CYLINDRICAL_SURFACE ( 'NONE', #62522, 31.99999999999999289 ) ;
#9442 = LINE ( 'NONE', #19610, #22727 ) ;
#9444 = CARTESIAN_POINT ( 'NONE',  ( -93.84685191531252713, 88.00268892867056536, 80.48822916753381662 ) ) ;
#9443 = CIRCLE ( 'NONE', #20404, 31.99999999999998579 ) ;
#9445 = EDGE_LOOP ( 'NONE', ( #46450, #58721, #63168, #57965 ) ) ;
#9446 = CARTESIAN_POINT ( 'NONE',  ( 94.99999999999998579, 92.66308142843935514, 77.41906250086714181 ) ) ;
#9447 = ORIENTED_EDGE ( 'NONE', *, *, #57754, .T. ) ;
#9448 = DIRECTION ( 'NONE',  ( -1.000000000000000000, -0.000000000000000000, 0.000000000000000000 ) ) ;
#9449 = DIRECTION ( 'NONE',  ( -1.000000000000000000, 0.000000000000000000, 0.000000000000000000 ) ) ;
#9450 = AXIS2_PLACEMENT_3D ( 'NONE', #46061, #69722, #29484 ) ;
#9451 = FACE_OUTER_BOUND ( 'NONE', #50693, .T. ) ;
#9452 = FACE_OUTER_BOUND ( 'NONE', #25349, .T. ) ;
#9453 = LINE ( 'NONE', #21462, #12893 ) ;
#9454 = CARTESIAN_POINT ( 'NONE',  ( -94.99999999999997158, -207.3369185715606307, 80.59406250086715318 ) ) ;
#9455 = AXIS2_PLACEMENT_3D ( 'NONE', #65804, #8280, #31208 ) ;
#9456 = FACE_OUTER_BOUND ( 'NONE', #62134, .T. ) ;
#9457 = DIRECTION ( 'NONE',  ( -1.000000000000000000, -0.000000000000000000, -0.000000000000000000 ) ) ;
#9458 = DIRECTION ( 'NONE',  ( 0.000000000000000000, 0.8090169943749445647, 0.5877852522924770229 ) ) ;
#9459 = ORIENTED_EDGE ( 'NONE', *, *, #10122, .T. ) ;
#9460 = CIRCLE ( 'NONE', #50240, 77.49899999999999523 ) ;
#9461 = ORIENTED_EDGE ( 'NONE', *, *, #29715, .T. ) ;
#9462 = CARTESIAN_POINT ( 'NONE',  ( 11.99999999999999822, 41.19522573413826194, -65.64334221924865176 ) ) ;
#9463 = CIRCLE ( 'NONE', #8285, 23.50000000000000355 ) ;
#9464 = DIRECTION ( 'NONE',  ( 0.000000000000000000, 1.000000000000000000, 3.491481338843133355E-15 ) ) ;
#9465 = LINE ( 'NONE', #21860, #48757 ) ;
#9466 = CARTESIAN_POINT ( 'NONE',  ( -93.84685191531252713, 88.00268892867056536, 80.96447916753380980 ) ) ;
#9467 = LINE ( 'NONE', #33500, #7049 ) ;
#9468 = CARTESIAN_POINT ( 'NONE',  ( 11.99999999999999822, 77.19088730480524418, 6.903761155838049390 ) ) ;
#9469 = EDGE_LOOP ( 'NONE', ( #33001, #60948, #27646, #23876 ) ) ;
#9470 = CARTESIAN_POINT ( 'NONE',  ( 0.000000000000000000, -5.202137450156655518, 37.22597642581156663 ) ) ;
#9471 = CIRCLE ( 'NONE', #58864, 82.00000000000000000 ) ;
#9472 = AXIS2_PLACEMENT_3D ( 'NONE', #58281, #42478, #24437 ) ;
#9473 = DIRECTION ( 'NONE',  ( 0.000000000000000000, 0.9876883405951372152, 0.1564344650402347547 ) ) ;
#9475 = CARTESIAN_POINT ( 'NONE',  ( 10.00000000000000000, 16.23288003029543347, -33.80338159004267595 ) ) ;
#9474 = AXIS2_PLACEMENT_3D ( 'NONE', #37836, #60403, #43112 ) ;
#9476 = CARTESIAN_POINT ( 'NONE',  ( -1.552113441248129000, 4.877389578778817736, -0.7348938709837885552 ) ) ;
#9477 = FACE_OUTER_BOUND ( 'NONE', #4951, .T. ) ;
#9478 = CARTESIAN_POINT ( 'NONE',  ( -97.30629616937497417, -211.3315407142195852, 82.86947916753382515 ) ) ;
#9479 = CIRCLE ( 'NONE', #51501, 31.99999999999999289 ) ;
#9480 = CARTESIAN_POINT ( 'NONE',  ( -97.64999999999996305, -209.9999907117602618, 86.90437468048614278 ) ) ;
#9481 = VECTOR ( 'NONE', #63150, 1000.000000000000000 ) ;
#9482 =( BOUNDED_CURVE ( )  B_SPLINE_CURVE ( 2, ( #5616, #57477, #11590, #34530, #5991, #23268, #64973 ),
 .UNSPECIFIED., .F., .F. ) 
 B_SPLINE_CURVE_WITH_KNOTS ( ( 3, 2, 2, 3 ),
 ( 0.1041666666666670182, 0.1111111111111114103, 0.1180555555555558161, 0.1250000000000002220 ),
 .UNSPECIFIED. ) 
 CURVE ( )  GEOMETRIC_REPRESENTATION_ITEM ( )  RATIONAL_B_SPLINE_CURVE ( ( 0.9999999999999933387, 0.8660254037844453689, 1.000000000000000000, 0.8660254037844387076, 1.000000000000000000, 0.8660254037844343777, 1.000000000000004219 ) ) 
 REPRESENTATION_ITEM ( '' )  );
#9483 = ORIENTED_EDGE ( 'NONE', *, *, #59406, .F. ) ;
#9484 = DIRECTION ( 'NONE',  ( 1.000000000000000000, 0.000000000000000000, 0.000000000000000000 ) ) ;
#9485 = EDGE_CURVE ( 'NONE', #10617, #66007, #14092, .T. ) ;
#9486 = CARTESIAN_POINT ( 'NONE',  ( 0.000000000000000000, -31.52238457039619490, 27.75498641678731104 ) ) ;
#9487 = CARTESIAN_POINT ( 'NONE',  ( -25.50183398199384044, -112.6408924756582053, -2.500000000000000000 ) ) ;
#9488 = EDGE_LOOP ( 'NONE', ( #45822, #7332, #68645, #66316, #47086, #10653 ) ) ;
#9489 = CARTESIAN_POINT ( 'NONE',  ( 10.00000000000000000, -3.925862922255855647, -41.81611651403866858 ) ) ;
#9490 = CARTESIAN_POINT ( 'NONE',  ( 10.00000000000000000, 16.95692799528845995, 2.500000000000000000 ) ) ;
#9491 = CARTESIAN_POINT ( 'NONE',  ( 1.560000000000000053, 1.299038105676658228, 0.7500000000000009992 ) ) ;
#9492 = ADVANCED_FACE ( 'NONE', ( #67085 ), #9202, .T. ) ;
#9493 = DIRECTION ( 'NONE',  ( 2.603472992746261562E-14, 2.546204323184492723E-14, -1.000000000000000000 ) ) ;
#9494 = EDGE_LOOP ( 'NONE', ( #9302, #63183, #32940, #20057 ) ) ;
#9495 = EDGE_CURVE ( 'NONE', #54579, #8511, #15211, .T. ) ;
#9496 = AXIS2_PLACEMENT_3D ( 'NONE', #7967, #30884, #2378 ) ;
#9497 = CARTESIAN_POINT ( 'NONE',  ( 1.384174031800307736, -119.4220188154534981, -2.500000000000000000 ) ) ;
#9498 = CARTESIAN_POINT ( 'NONE',  ( 17.50000000000000355, 2.143131898507868643E-15, -20.00000000000000000 ) ) ;
#9499 = ORIENTED_EDGE ( 'NONE', *, *, #36150, .T. ) ;
#9500 = ADVANCED_FACE ( 'NONE', ( #55063 ), #42680, .T. ) ;
#9501 = CIRCLE ( 'NONE', #59982, 16.00000000000000000 ) ;
#9502 = CARTESIAN_POINT ( 'NONE',  ( -10.00000000000000000, 0.000000000000000000, 0.000000000000000000 ) ) ;
#9503 = CARTESIAN_POINT ( 'NONE',  ( 11.99999999999999822, -74.65491531819111515, -8.830959090343204920 ) ) ;
#9504 = ORIENTED_EDGE ( 'NONE', *, *, #18935, .T. ) ;
#9505 = AXIS2_PLACEMENT_3D ( 'NONE', #231, #18207, #7306 ) ;
#9506 = CIRCLE ( 'NONE', #35956, 32.00000000000000000 ) ;
#9507 = CARTESIAN_POINT ( 'NONE',  ( -4.250000000000000000, -13.95926121303099343, -1.199999999999999956 ) ) ;
#9508 = AXIS2_PLACEMENT_3D ( 'NONE', #19060, #42011, #64947 ) ;
#9509 = EDGE_LOOP ( 'NONE', ( #29607, #40610 ) ) ;
#9510 = LINE ( 'NONE', #45216, #68260 ) ;
#9511 = AXIS2_PLACEMENT_3D ( 'NONE', #61636, #43253, #66176 ) ;
#9512 = VERTEX_POINT ( 'NONE', #71231 ) ;
#9513 = ORIENTED_EDGE ( 'NONE', *, *, #35169, .T. ) ;
#9514 = VECTOR ( 'NONE', #56766, 1000.000000000000000 ) ;
#9515 = ORIENTED_EDGE ( 'NONE', *, *, #63941, .T. ) ;
#9516 = ORIENTED_EDGE ( 'NONE', *, *, #9683, .T. ) ;
#9517 = DIRECTION ( 'NONE',  ( -0.9038112904824853189, 0.4279312458752976833, 0.000000000000000000 ) ) ;
#9518 = EDGE_CURVE ( 'NONE', #19568, #25068, #51446, .T. ) ;
#9519 = ADVANCED_FACE ( 'NONE', ( #3596 ), #26859, .T. ) ;
#9520 = EDGE_LOOP ( 'NONE', ( #25737, #51509, #27207, #39210 ) ) ;
#9521 = VERTEX_POINT ( 'NONE', #59991 ) ;
#9522 = CARTESIAN_POINT ( 'NONE',  ( 92.69370383062498320, 91.33154071421968467, 75.77864583420048916 ) ) ;
#9523 = CARTESIAN_POINT ( 'NONE',  ( 0.000000000000000000, 0.000000000000000000, 90.00000000000000000 ) ) ;
#9524 = DIRECTION ( 'NONE',  ( 0.000000000000000000, 0.000000000000000000, 1.000000000000000000 ) ) ;
#9525 = ORIENTED_EDGE ( 'NONE', *, *, #11894, .F. ) ;
#9527 = ORIENTED_EDGE ( 'NONE', *, *, #43968, .T. ) ;
#9526 = CIRCLE ( 'NONE', #51553, 42.00000000000000000 ) ;
#9528 = VERTEX_POINT ( 'NONE', #38146 ) ;
#9529 = CYLINDRICAL_SURFACE ( 'NONE', #67089, 82.00000000000000000 ) ;
#9530 = EDGE_LOOP ( 'NONE', ( #19219, #12934, #1813, #60820 ) ) ;
#9531 = CARTESIAN_POINT ( 'NONE',  ( 96.15314808468748708, -208.0026889286704943, 89.43114583420047836 ) ) ;
#9532 = VECTOR ( 'NONE', #14051, 1000.000000000000000 ) ;
#9533 = EDGE_CURVE ( 'NONE', #16806, #23559, #26116, .T. ) ;
#9534 = EDGE_CURVE ( 'NONE', #47366, #69481, #74267, .T. ) ;
#9535 =( NAMED_UNIT ( * ) PLANE_ANGLE_UNIT ( ) SI_UNIT ( $, .RADIAN. ) );
#9536 = CYLINDRICAL_SURFACE ( 'NONE', #12570, 31.99999999999999289 ) ;
#9537 = CARTESIAN_POINT ( 'NONE',  ( -97.65000000000000568, 89.99996514701868477, 77.37937620717865173 ) ) ;
#9538 = DIRECTION ( 'NONE',  ( -1.000000000000000000, -0.000000000000000000, 0.000000000000000000 ) ) ;
#9539 = CARTESIAN_POINT ( 'NONE',  ( 0.000000000000000000, 0.000000000000000000, -1.199999999999999956 ) ) ;
#9540 = DIRECTION ( 'NONE',  ( -1.000000000000000000, -0.000000000000000000, -0.000000000000000000 ) ) ;
#9541 = AXIS2_PLACEMENT_3D ( 'NONE', #27548, #49728, #10628 ) ;
#9542 = DIRECTION ( 'NONE',  ( 0.000000000000000000, 0.9723699203976756689, 0.2334453638559095823 ) ) ;
#9543 = AXIS2_PLACEMENT_3D ( 'NONE', #27420, #21400, #61652 ) ;
#9544 = CARTESIAN_POINT ( 'NONE',  ( -93.67499999999998295, -207.7050326799711968, 75.89770833506763381 ) ) ;
#9545 = ORIENTED_EDGE ( 'NONE', *, *, #30817, .F. ) ;
#9546 =( REPRESENTATION_RELATIONSHIP ('NONE','NONE', #31117, #23897 ) REPRESENTATION_RELATIONSHIP_WITH_TRANSFORMATION ( #70352 )SHAPE_REPRESENTATION_RELATIONSHIP( ) );
#9548 = CARTESIAN_POINT ( 'NONE',  ( -97.30629616937501680, 88.66845928578038638, 87.15572916753380639 ) ) ;
#9547 = CARTESIAN_POINT ( 'NONE',  ( 96.15314808468748708, 88.00268892867053694, 89.21947916753380525 ) ) ;
#9549 = ORIENTED_EDGE ( 'NONE', *, *, #73602, .T. ) ;
#9550 = CARTESIAN_POINT ( 'NONE',  ( 97.65000000000000568, -211.5299782133524218, 84.62895833506763665 ) ) ;
#9551 = DIRECTION ( 'NONE',  ( -1.000000000000000000, -0.000000000000000000, -0.000000000000000000 ) ) ;
#9552 = CARTESIAN_POINT ( 'NONE',  ( 0.000000000000000000, 16.65560815589464028, -38.55633173626993226 ) ) ;
#9553 = CARTESIAN_POINT ( 'NONE',  ( 5.000000000000000000, -36.13751322684404244, -21.40280677340410165 ) ) ;
#9554 = CARTESIAN_POINT ( 'NONE',  ( 15.00000000000000000, 26.50000000000000355, -1.500000000000000000 ) ) ;
#9555 = DIRECTION ( 'NONE',  ( -1.000000000000000000, -0.000000000000000000, -0.000000000000000000 ) ) ;
#9556 = CARTESIAN_POINT ( 'NONE',  ( 11.99999999999999822, 0.000000000000000000, 0.000000000000000000 ) ) ;
#9557 = DIRECTION ( 'NONE',  ( 1.000000000000000000, 0.000000000000000000, 0.000000000000000000 ) ) ;
#9558 = ORIENTED_EDGE ( 'NONE', *, *, #26884, .F. ) ;
#9559 = VERTEX_POINT ( 'NONE', #25756 ) ;
#9560 = CARTESIAN_POINT ( 'NONE',  ( -92.35000000000005116, 88.47002178664754979, 81.37458333333333371 ) ) ;
#9561 = PLANE ( 'NONE',  #45122 ) ;
#9562 = CARTESIAN_POINT ( 'NONE',  ( 92.35001423713265467, -211.5299864331648223, 75.52729223699087413 ) ) ;
#9563 = CARTESIAN_POINT ( 'NONE',  ( 0.000000000000000000, 0.000000000000000000, 0.000000000000000000 ) ) ;
#9564 = DIRECTION ( 'NONE',  ( 0.000000000000000000, 0.9510565162951546414, -0.3090169943749446202 ) ) ;
#9565 = CARTESIAN_POINT ( 'NONE',  ( 11.99999999999999822, 0.000000000000000000, 0.000000000000000000 ) ) ;
#9566 = DIRECTION ( 'NONE',  ( -1.000000000000000000, 0.000000000000000000, 0.000000000000000000 ) ) ;
#9567 = VERTEX_POINT ( 'NONE', #48686 ) ;
#9568 = CARTESIAN_POINT ( 'NONE',  ( -97.30629616937501680, 90.00000000000004263, 80.75281250086715090 ) ) ;
#9569 = EDGE_CURVE ( 'NONE', #18028, #36601, #40666, .T. ) ;
#9570 = AXIS2_PLACEMENT_3D ( 'NONE', #45259, #50508, #56154 ) ;
#9572 = CARTESIAN_POINT ( 'NONE',  ( 92.34999999999999432, 88.47002178664752137, 82.51229166840094820 ) ) ;
#9571 = AXIS2_PLACEMENT_3D ( 'NONE', #16393, #16017, #21657 ) ;
#9573 = CARTESIAN_POINT ( 'NONE',  ( 12.19999999999998863, 0.000000000000000000, -4.400000000000001243 ) ) ;
#9574 = LINE ( 'NONE', #15585, #63411 ) ;
#9575 = DIRECTION ( 'NONE',  ( 0.000000000000000000, 0.000000000000000000, 1.000000000000000000 ) ) ;
#9576 = CIRCLE ( 'NONE', #33548, 31.99999999999999289 ) ;
#9577 = DIRECTION ( 'NONE',  ( 0.000000000000000000, 0.000000000000000000, 1.000000000000000000 ) ) ;
#9578 = DIRECTION ( 'NONE',  ( -1.000000000000000000, 0.000000000000000000, 0.000000000000000000 ) ) ;
#9579 = EDGE_CURVE ( 'NONE', #26686, #36758, #8235, .T. ) ;
#9580 = LINE ( 'NONE', #55441, #61410 ) ;
#9581 = CARTESIAN_POINT ( 'NONE',  ( 0.000000000000000000, -34.44570377933647620, 69.42325613327427902 ) ) ;
#9582 = EDGE_CURVE ( 'NONE', #23124, #16471, #7000, .T. ) ;
#9583 = EDGE_CURVE ( 'NONE', #35612, #33344, #74210, .T. ) ;
#9584 = CARTESIAN_POINT ( 'NONE',  ( 94.99999999999998579, 87.33691857156068750, 81.07031250086716057 ) ) ;
#9585 = EDGE_CURVE ( 'NONE', #11102, #10014, #46025, .T. ) ;
#9586 = CARTESIAN_POINT ( 'NONE',  ( -96.15314808468747287, -208.0026889286704943, 83.34572916753383254 ) ) ;
#9587 = CARTESIAN_POINT ( 'NONE',  ( 5.000000000000002665, -40.65526001592565564, -71.21200624218839437 ) ) ;
#9588 = CIRCLE ( 'NONE', #45614, 42.00000000000000000 ) ;
#9589 = EDGE_LOOP ( 'NONE', ( #64936, #724, #69789, #22005 ) ) ;
#9590 = DIRECTION ( 'NONE',  ( -1.000000000000000000, 0.000000000000000000, 0.000000000000000000 ) ) ;
#9591 = CARTESIAN_POINT ( 'NONE',  ( -93.67499999999998295, -212.2949673200287179, 77.51166666666665606 ) ) ;
#9592 = DIRECTION ( 'NONE',  ( 0.000000000000000000, -0.9510565162951565288, 0.3090169943749384029 ) ) ;
#9593 = AXIS2_PLACEMENT_3D ( 'NONE', #57858, #52202, #69496 ) ;
#9594 = CIRCLE ( 'NONE', #51606, 1.500000000000000000 ) ;
#9595 = AXIS2_PLACEMENT_3D ( 'NONE', #12480, #47081, #68899 ) ;
#9596 = VECTOR ( 'NONE', #58594, 1000.000000000000000 ) ;
#9597 = CARTESIAN_POINT ( 'NONE',  ( -92.69370383062504004, 90.00000000000004263, 76.78406250086715090 ) ) ;
#9598 = CARTESIAN_POINT ( 'NONE',  ( 96.15314808468750130, -211.9973110713294489, 82.23447916753380582 ) ) ;
#9599 = ORIENTED_EDGE ( 'NONE', *, *, #17647, .F. ) ;
#9600 = DIRECTION ( 'NONE',  ( 1.000000000000000000, 0.000000000000000000, 0.000000000000000000 ) ) ;
#9601 = ORIENTED_EDGE ( 'NONE', *, *, #9955, .T. ) ;
#9602 = EDGE_CURVE ( 'NONE', #50254, #18134, #62968, .T. ) ;
#9603 = ORIENTED_EDGE ( 'NONE', *, *, #56716, .T. ) ;
#9604 = ORIENTED_EDGE ( 'NONE', *, *, #50225, .F. ) ;
#9605 = ORIENTED_EDGE ( 'NONE', *, *, #5144, .F. ) ;
#9606 = CARTESIAN_POINT ( 'NONE',  ( 92.69370383062501162, -209.9999999999999716, 75.83156250086716454 ) ) ;
#9607 = ADVANCED_FACE ( 'NONE', ( #63317 ), #67836, .F. ) ;
#9608 = DIRECTION ( 'NONE',  ( 0.000000000000000000, 1.000000000000000000, 0.000000000000000000 ) ) ;
#9609 = EDGE_CURVE ( 'NONE', #5325, #55639, #73082, .T. ) ;
#9610 = CARTESIAN_POINT ( 'NONE',  ( -97.64999999960629395, 90.00002930740643592, 76.74344264317980446 ) ) ;
#9611 = DIRECTION ( 'NONE',  ( 0.000000000000000000, 0.000000000000000000, 1.000000000000000000 ) ) ;
#9612 = CARTESIAN_POINT ( 'NONE',  ( 92.69370383062498320, 90.00000000000002842, 87.26156250086715715 ) ) ;
#9613 = AXIS2_PLACEMENT_3D ( 'NONE', #45218, #16261, #23031 ) ;
#9614 = EDGE_CURVE ( 'NONE', #64620, #52133, #33989, .T. ) ;
#9615 = DIRECTION ( 'NONE',  ( -1.000000000000000000, 0.000000000000000000, 0.000000000000000000 ) ) ;
#9616 = CARTESIAN_POINT ( 'NONE',  ( 97.64999999999999147, -209.9999999999999716, 81.42749999999999488 ) ) ;
#9617 = ORIENTED_EDGE ( 'NONE', *, *, #59491, .F. ) ;
#9618 = VERTEX_POINT ( 'NONE', #62199 ) ;
#9619 = AXIS2_PLACEMENT_3D ( 'NONE', #15577, #39999, #61823 ) ;
#9620 = EDGE_LOOP ( 'NONE', ( #70267, #23701, #52304, #9833 ) ) ;
#9621 = ORIENTED_EDGE ( 'NONE', *, *, #31251, .T. ) ;
#9622 = CARTESIAN_POINT ( 'NONE',  ( 92.35000000000000853, -209.9999999999999716, 89.36499999999999488 ) ) ;
#9623 = FACE_OUTER_BOUND ( 'NONE', #51130, .T. ) ;
#9624 = CARTESIAN_POINT ( 'NONE',  ( 92.69370383062498320, 90.00000000000002842, 89.64281250086713726 ) ) ;
#9625 = DIRECTION ( 'NONE',  ( -1.000000000000000000, -0.000000000000000000, -0.000000000000000000 ) ) ;
#9626 = LINE ( 'NONE', #67136, #51555 ) ;
#9627 = CARTESIAN_POINT ( 'NONE',  ( 10.00000000000000000, -16.23288003029521320, 33.80338159004277543 ) ) ;
#9628 = ORIENTED_EDGE ( 'NONE', *, *, #54896, .F. ) ;
#9629 = CARTESIAN_POINT ( 'NONE',  ( -92.34999999999999432, -211.5299782133524502, 86.53395833506763779 ) ) ;
#9630 = VERTEX_POINT ( 'NONE', #61834 ) ;
#9631 = CARTESIAN_POINT ( 'NONE',  ( 10.00000000000000000, -73.72996012237429397, -14.67089635893794508 ) ) ;
#9632 = VERTEX_POINT ( 'NONE', #202 ) ;
#9633 = CARTESIAN_POINT ( 'NONE',  ( -92.35000000000003695, 90.00000000000004263, 81.50687500173430067 ) ) ;
#9634 = EDGE_LOOP ( 'NONE', ( #15336, #63512, #40741, #26798 ) ) ;
#9635 = CARTESIAN_POINT ( 'NONE',  ( 97.30629616937498838, 91.33154071421968467, 83.18697916753382060 ) ) ;
#9636 = FACE_OUTER_BOUND ( 'NONE', #20721, .T. ) ;
#9637 = CARTESIAN_POINT ( 'NONE',  ( 10.00000000000000000, 8.840884882375075193, 74.65374052328651544 ) ) ;
#9638 = CYLINDRICAL_SURFACE ( 'NONE', #62616, 16.00000000000000000 ) ;
#9639 = VECTOR ( 'NONE', #13985, 1000.000000000000000 ) ;
#9640 = DIRECTION ( 'NONE',  ( -0.1850432970638656582, 0.9827303690289285187, 0.000000000000000000 ) ) ;
#9641 = DIRECTION ( 'NONE',  ( 0.000000000000000000, 0.7604059656000277112, 0.6494480483301875440 ) ) ;
#9642 = EDGE_LOOP ( 'NONE', ( #51211, #12269, #33003, #37061 ) ) ;
#9643 = CARTESIAN_POINT ( 'NONE',  ( 94.99999999999998579, 90.00000000000002842, 90.00000000000000000 ) ) ;
#9644 = AXIS2_PLACEMENT_3D ( 'NONE', #56434, #38395, #37662 ) ;
#9645 = CARTESIAN_POINT ( 'NONE',  ( 12.00000000000000000, -13.04903810567646971, 19.60159698893442481 ) ) ;
#9646 = ORIENTED_EDGE ( 'NONE', *, *, #73983, .T. ) ;
#9647 = ORIENTED_EDGE ( 'NONE', *, *, #72649, .T. ) ;
#9648 = VECTOR ( 'NONE', #16938, 1000.000000000000227 ) ;
#9649 = AXIS2_PLACEMENT_3D ( 'NONE', #54626, #25326, #26045 ) ;
#9650 = ADVANCED_FACE ( 'NONE', ( #45290 ), #41127, .F. ) ;
#9651 = FACE_OUTER_BOUND ( 'NONE', #41059, .T. ) ;
#9652 = CARTESIAN_POINT ( 'NONE',  ( 10.00000000000000000, 0.000000000000000000, 0.000000000000000000 ) ) ;
#9653 = CARTESIAN_POINT ( 'NONE',  ( 5.000000000000000000, 41.91543099594818500, -2.663952781846291362 ) ) ;
#9654 = CARTESIAN_POINT ( 'NONE',  ( -94.99999999999997158, -207.3369185715606307, 85.19781250086714408 ) ) ;
#9655 = ORIENTED_EDGE ( 'NONE', *, *, #55444, .T. ) ;
#9656 = DIRECTION ( 'NONE',  ( 0.000000000000000000, 0.000000000000000000, 1.000000000000000000 ) ) ;
#9657 = ORIENTED_EDGE ( 'NONE', *, *, #31848, .F. ) ;
#9658 = CARTESIAN_POINT ( 'NONE',  ( 0.000000000000000000, 0.000000000000000000, 0.000000000000000000 ) ) ;
#9659 = DIRECTION ( 'NONE',  ( -0.000000000000000000, -0.000000000000000000, -1.000000000000000000 ) ) ;
#9660 = CARTESIAN_POINT ( 'NONE',  ( 0.000000000000000000, 0.000000000000000000, 0.000000000000000000 ) ) ;
#9661 = CARTESIAN_POINT ( 'NONE',  ( 97.30629616937498838, 91.33154071421968467, 77.94822916753381037 ) ) ;
#9662 = CARTESIAN_POINT ( 'NONE',  ( 0.000000000000000000, 24.73286445877703699, 73.44644590900068692 ) ) ;
#9663 = DIRECTION ( 'NONE',  ( 0.000000000000000000, 0.000000000000000000, 1.000000000000000000 ) ) ;
#9664 = ADVANCED_FACE ( 'NONE', ( #5082 ), #68964, .T. ) ;
#9665 = DIRECTION ( 'NONE',  ( -0.000000000000000000, -0.000000000000000000, 1.000000000000000000 ) ) ;
#9666 = CARTESIAN_POINT ( 'NONE',  ( 93.55421244156863736, 91.96030971134655374, 74.86947676125078033 ) ) ;
#9667 = DIRECTION ( 'NONE',  ( -1.000000000000000000, -0.000000000000000000, 0.000000000000000000 ) ) ;
#9668 = EDGE_CURVE ( 'NONE', #14681, #57613, #3429, .T. ) ;
#9669 = CARTESIAN_POINT ( 'NONE',  ( -43.60332556124591719, -107.0000000000000000, -2.500000000000002220 ) ) ;
#9670 = CARTESIAN_POINT ( 'NONE',  ( -10.00000000000000000, 0.000000000000000000, 0.000000000000000000 ) ) ;
#9671 = ADVANCED_FACE ( 'NONE', ( #28349 ), #73469, .T. ) ;
#9672 = CARTESIAN_POINT ( 'NONE',  ( 92.35000000000000853, -209.9999999999999716, 78.57000000000000739 ) ) ;
#9673 = CARTESIAN_POINT ( 'NONE',  ( 92.35000000000000853, 90.00003217427531865, 76.74437388893713319 ) ) ;
#9674 = ORIENTED_EDGE ( 'NONE', *, *, #66600, .T. ) ;
#9675 = EDGE_CURVE ( 'NONE', #23551, #5835, #15416, .T. ) ;
#9676 = CARTESIAN_POINT ( 'NONE',  ( -97.30629616937501680, 90.00000000000004263, 82.02281250086714692 ) ) ;
#9677 = AXIS2_PLACEMENT_3D ( 'NONE', #60441, #32585, #8924 ) ;
#9678 = CARTESIAN_POINT ( 'NONE',  ( 10.00000000000000000, -46.54456581323847786, 59.03342792756247093 ) ) ;
#9679 = CYLINDRICAL_SURFACE ( 'NONE', #6651, 82.00000000000000000 ) ;
#9680 = ORIENTED_EDGE ( 'NONE', *, *, #25291, .F. ) ;
#9681 = CYLINDRICAL_SURFACE ( 'NONE', #66678, 2.649999999999999467 ) ;
#9682 = DIRECTION ( 'NONE',  ( 0.000000000000000000, 0.4999999999999995004, -0.8660254037844389297 ) ) ;
#9683 = EDGE_CURVE ( 'NONE', #27851, #28632, #57471, .T. ) ;
#9684 = DIRECTION ( 'NONE',  ( -1.000000000000000000, 0.000000000000000000, 0.000000000000000000 ) ) ;
#9685 = VECTOR ( 'NONE', #49222, 1000.000000000000000 ) ;
#9686 = CARTESIAN_POINT ( 'NONE',  ( 94.99999999999998579, 86.94004357329502852, 83.25312500173430408 ) ) ;
#9687 = CARTESIAN_POINT ( 'NONE',  ( 92.69370383062501162, -208.6684592857803011, 78.31864583420050963 ) ) ;
#9688 = CIRCLE ( 'NONE', #51729, 37.49900000000000944 ) ;
#9689 = ORIENTED_EDGE ( 'NONE', *, *, #58645, .T. ) ;
#9690 = CIRCLE ( 'NONE', #45741, 31.99999999999999289 ) ;
#9691 = ORIENTED_EDGE ( 'NONE', *, *, #26050, .F. ) ;
#9692 = EDGE_CURVE ( 'NONE', #11414, #13516, #2274, .T. ) ;
#9693 = EDGE_CURVE ( 'NONE', #20201, #71364, #41842, .T. ) ;
#9694 = FACE_OUTER_BOUND ( 'NONE', #31175, .T. ) ;
#9695 = EDGE_CURVE ( 'NONE', #20645, #44110, #29807, .T. ) ;
#9696 = CYLINDRICAL_SURFACE ( 'NONE', #10169, 31.99999999999998579 ) ;
#9697 =( BOUNDED_CURVE ( )  B_SPLINE_CURVE ( 2, ( #53096, #41806, #65862, #54213, #12855, #19976, #42931, #71476, #14347, #59477, #36530 ),
 .UNSPECIFIED., .F., .F. ) 
 B_SPLINE_CURVE_WITH_KNOTS ( ( 3, 2, 2, 2, 2, 3 ),
 ( 0.04233441017615420521, 0.04233459324550207376, 0.04939035878641885591, 0.05644612432733563112, 0.06350188986825240633, 0.06350193517771154927 ),
 .UNSPECIFIED. ) 
 CURVE ( )  GEOMETRIC_REPRESENTATION_ITEM ( )  RATIONAL_B_SPLINE_CURVE ( ( 0.9999930479533516436, 0.9999965238864843009, 1.000000000000000000, 0.8660254037844387076, 1.000000000000000000, 0.8660254037844387076, 1.000000000000000000, 0.8660254037844387076, 1.000000000000000000, 0.9999991396657871290, 0.9999982793426236416 ) ) 
 REPRESENTATION_ITEM ( '' )  );
#9698 = DIRECTION ( 'NONE',  ( 2.603472992746261562E-14, 2.546204323184492723E-14, -1.000000000000000000 ) ) ;
#9699 = CARTESIAN_POINT ( 'NONE',  ( 5.000000000000002665, 8.966570791701863996, -81.50828551894218776 ) ) ;
#9700 = LINE ( 'NONE', #37542, #39341 ) ;
#9701 = CARTESIAN_POINT ( 'NONE',  ( 97.30629616937498838, -211.3315407142195852, 76.09614583420048461 ) ) ;
#9702 = VERTEX_POINT ( 'NONE', #45675 ) ;
#9703 = DIRECTION ( 'NONE',  ( 0.000000000000000000, 0.6494480483301849905, -0.7604059656000299317 ) ) ;
#9704 = VERTEX_POINT ( 'NONE', #40377 ) ;
#9705 = ORIENTED_EDGE ( 'NONE', *, *, #21968, .F. ) ;
#9706 = CYLINDRICAL_SURFACE ( 'NONE', #33320, 31.99999999999999289 ) ;
#9707 = SURFACE_STYLE_FILL_AREA ( #32625 ) ;
#9708 = CARTESIAN_POINT ( 'NONE',  ( 10.00000000000000000, 65.64334221924966073, -41.19522573413664190 ) ) ;
#9709 = ORIENTED_EDGE ( 'NONE', *, *, #54402, .F. ) ;
#9710 = DIRECTION ( 'NONE',  ( -0.000000000000000000, -0.000000000000000000, 1.000000000000000000 ) ) ;
#9711 = CARTESIAN_POINT ( 'NONE',  ( 92.35000000000002274, -208.4700217866474645, 79.86645833506761960 ) ) ;
#9712 = CARTESIAN_POINT ( 'NONE',  ( 93.67499999999998295, 92.29496732002878900, 81.00416666666666288 ) ) ;
#9713 = ORIENTED_EDGE ( 'NONE', *, *, #66976, .F. ) ;
#9714 = CARTESIAN_POINT ( 'NONE',  ( 0.000000000000000000, -74.65491531819111515, -8.830959090343204920 ) ) ;
#9715 = VERTEX_POINT ( 'NONE', #63329 ) ;
#9716 = DIRECTION ( 'NONE',  ( -1.000000000000000000, 0.000000000000000000, 0.000000000000000000 ) ) ;
#9717 = ORIENTED_EDGE ( 'NONE', *, *, #7795, .F. ) ;
#9718 = CYLINDRICAL_SURFACE ( 'NONE', #33154, 31.99999999999998579 ) ;
#9719 = CARTESIAN_POINT ( 'NONE',  ( -97.30629616937501680, 90.00000000000004263, 84.08656250086716000 ) ) ;
#9720 = CARTESIAN_POINT ( 'NONE',  ( 94.99999999999998579, 87.33691857156068750, 82.18156250086714465 ) ) ;
#9721 = ORIENTED_EDGE ( 'NONE', *, *, #43732, .T. ) ;
#9722 = CARTESIAN_POINT ( 'NONE',  ( 11.99999999999999822, 73.95703589264006439, -23.16143007188350822 ) ) ;
#9723 = CIRCLE ( 'NONE', #57769, 17.30399999999999849 ) ;
#9724 = AXIS2_PLACEMENT_3D ( 'NONE', #56538, #72677, #45257 ) ;
#9725 = DIRECTION ( 'NONE',  ( 1.000000000000000000, 0.000000000000000000, 0.000000000000000000 ) ) ;
#9726 = ORIENTED_EDGE ( 'NONE', *, *, #38449, .T. ) ;
#9727 = CARTESIAN_POINT ( 'NONE',  ( -10.00000000000000000, 0.000000000000000000, 0.000000000000000000 ) ) ;
#9728 = AXIS2_PLACEMENT_3D ( 'NONE', #43052, #3580, #25745 ) ;
#9729 = ORIENTED_EDGE ( 'NONE', *, *, #15091, .F. ) ;
#9730 = ORIENTED_EDGE ( 'NONE', *, *, #53581, .F. ) ;
#9731 = DIRECTION ( 'NONE',  ( 0.000000000000000000, 0.000000000000000000, 1.000000000000000000 ) ) ;
#9732 = ORIENTED_EDGE ( 'NONE', *, *, #44659, .T. ) ;
#9733 = CARTESIAN_POINT ( 'NONE',  ( 0.000000000000000000, 69.42325613327439271, 34.44570377933623462 ) ) ;
#9734 = EDGE_CURVE ( 'NONE', #20087, #49658, #39280, .T. ) ;
#9735 = CARTESIAN_POINT ( 'NONE',  ( 94.99999999999998579, 93.05995642670504253, 88.65062500173431204 ) ) ;
#9736 = ORIENTED_EDGE ( 'NONE', *, *, #44559, .F. ) ;
#9737 = DIRECTION ( 'NONE',  ( 2.889240119132116694E-16, -1.000000000000000000, 0.000000000000000000 ) ) ;
#9738 = CARTESIAN_POINT ( 'NONE',  ( -93.84685191531247028, -211.9973110713294489, 79.69447916753379957 ) ) ;
#9739 = ORIENTED_EDGE ( 'NONE', *, *, #28718, .F. ) ;
#9740 = LINE ( 'NONE', #55604, #1502 ) ;
#9741 = DIRECTION ( 'NONE',  ( 0.9730327541852497042, -0.2306669878475622604, 0.000000000000000000 ) ) ;
#9742 = FACE_OUTER_BOUND ( 'NONE', #4874, .T. ) ;
#9743 = FACE_OUTER_BOUND ( 'NONE', #9589, .T. ) ;
#9744 = EDGE_CURVE ( 'NONE', #2080, #58390, #62210, .T. ) ;
#9745 = VECTOR ( 'NONE', #42397, 1000.000000000000000 ) ;
#9746 = DIRECTION ( 'NONE',  ( -1.000000000000000000, -0.000000000000000000, -0.000000000000000000 ) ) ;
#9747 = AXIS2_PLACEMENT_3D ( 'NONE', #13339, #37766, #65598 ) ;
#9748 = EDGE_CURVE ( 'NONE', #4389, #32475, #26212, .T. ) ;
#9749 = CARTESIAN_POINT ( 'NONE',  ( 92.35000000039364920, -209.9999706968037287, 82.45844277051352833 ) ) ;
#9750 = DIRECTION ( 'NONE',  ( -0.7071067811865485719, 0.000000000000000000, -0.7071067811865465735 ) ) ;
#9751 = DIRECTION ( 'NONE',  ( 0.000000000000000000, 0.000000000000000000, 1.000000000000000000 ) ) ;
#9752 = VECTOR ( 'NONE', #45852, 1000.000000000000227 ) ;
#9753 = CARTESIAN_POINT ( 'NONE',  ( 97.64999999999447766, 89.99999459739470353, 81.50687481489491404 ) ) ;
#9754 = EDGE_CURVE ( 'NONE', #43361, #30878, #46773, .T. ) ;
#9755 = LINE ( 'NONE', #60530, #47209 ) ;
#9756 = DIRECTION ( 'NONE',  ( 0.000000000000000000, -0.9510565162951543083, 0.3090169943749448977 ) ) ;
#9757 = DIRECTION ( 'NONE',  ( -1.000000000000000000, 0.000000000000000000, 0.000000000000000000 ) ) ;
#9758 = CARTESIAN_POINT ( 'NONE',  ( -97.65000000000001990, 90.00002803130638540, 87.53937403222812463 ) ) ;
#9759 = CARTESIAN_POINT ( 'NONE',  ( -10.90076147243505211, 0.000000000000000000, 13.71319123027096865 ) ) ;
#9760 = CARTESIAN_POINT ( 'NONE',  ( 94.99999999999998579, 93.05995642670504253, 75.95062500173428077 ) ) ;
#9761 = EDGE_CURVE ( 'NONE', #71645, #37324, #67060, .T. ) ;
#9762 = DIRECTION ( 'NONE',  ( -0.000000000000000000, -0.000000000000000000, 1.000000000000000000 ) ) ;
#9763 = DIRECTION ( 'NONE',  ( -1.000000000000000000, 0.000000000000000000, 0.000000000000000000 ) ) ;
#9764 = CARTESIAN_POINT ( 'NONE',  ( -97.64999999999994884, -211.5299782133524502, 83.06791666666664753 ) ) ;
#9765 = CARTESIAN_POINT ( 'NONE',  ( -94.95306897617113862, 87.35041560265752025, 75.00000002508417651 ) ) ;
#9766 = PRODUCT ( 'BR-542', 'BR-542', '', ( #73033 ) ) ;
#9767 = ADVANCED_FACE ( 'NONE', ( #24214 ), #18189, .F. ) ;
#9768 = LINE ( 'NONE', #49607, #31107 ) ;
#9769 = ADVANCED_FACE ( 'NONE', ( #13649 ), #70049, .T. ) ;
#9770 = DIRECTION ( 'NONE',  ( 0.000000000000000000, -0.7431448254773954654, -0.6691306063588569053 ) ) ;
#9771 = FILL_AREA_STYLE_COLOUR ( '', #45476 ) ;
#9772 = FACE_OUTER_BOUND ( 'NONE', #59467, .T. ) ;
#9773 = AXIS2_PLACEMENT_3D ( 'NONE', #32500, #20853, #49052 ) ;
#9774 = VECTOR ( 'NONE', #9551, 1000.000000000000000 ) ;
#9775 = CIRCLE ( 'NONE', #58997, 42.00000000000000000 ) ;
#9776 = EDGE_CURVE ( 'NONE', #45747, #12010, #35819, .T. ) ;
#9777 = CARTESIAN_POINT ( 'NONE',  ( 95.00000000000000000, -207.3369185715606307, 88.37281250086715545 ) ) ;
#9778 = CONICAL_SURFACE ( 'NONE', #59165, 2.445500000000000007, 0.7853981633974678189 ) ;
#9779 = VERTEX_POINT ( 'NONE', #18553 ) ;
#9780 = EDGE_LOOP ( 'NONE', ( #22673, #18693, #12667, #33202 ) ) ;
#9781 = DIRECTION ( 'NONE',  ( -1.000000000000000000, 0.000000000000000000, 0.000000000000000000 ) ) ;
#9782 = EDGE_CURVE ( 'NONE', #11119, #59559, #13006, .T. ) ;
#9783 = CARTESIAN_POINT ( 'NONE',  ( 10.00000000000000000, -10.41901085202107247, 40.68715046381925049 ) ) ;
#9784 = VERTEX_POINT ( 'NONE', #941 ) ;
#9785 = CARTESIAN_POINT ( 'NONE',  ( 96.15314808468748708, -208.0026889286704943, 82.44614583420046472 ) ) ;
#9786 = CARTESIAN_POINT ( 'NONE',  ( 97.30629616937498838, -209.9999999999999716, 85.67406250086715147 ) ) ;
#9787 = VERTEX_POINT ( 'NONE', #12542 ) ;
#9788 = CARTESIAN_POINT ( 'NONE',  ( 93.84685191531251292, -211.9973110713294489, 86.73239583420048859 ) ) ;
#9789 = ADVANCED_FACE ( 'NONE', ( #41488 ), #30568, .T. ) ;
#9790 = ORIENTED_EDGE ( 'NONE', *, *, #1037, .T. ) ;
#9791 = CARTESIAN_POINT ( 'NONE',  ( 0.000000000000000000, -18.13022148937263012, 15.02647892043544608 ) ) ;
#9792 = ORIENTED_EDGE ( 'NONE', *, *, #2499, .F. ) ;
#9793 = CIRCLE ( 'NONE', #8571, 42.00000000000000000 ) ;
#9794 = DIRECTION ( 'NONE',  ( -1.000000000000000000, 0.000000000000000000, 0.000000000000000000 ) ) ;
#9795 = ORIENTED_EDGE ( 'NONE', *, *, #73044, .F. ) ;
#9796 = ORIENTED_EDGE ( 'NONE', *, *, #41731, .F. ) ;
#9797 = FACE_OUTER_BOUND ( 'NONE', #67470, .T. ) ;
#9798 = VECTOR ( 'NONE', #658, 1000.000000000000000 ) ;
#9799 = EDGE_LOOP ( 'NONE', ( #15518, #59543, #33915, #58794 ) ) ;
#9800 = DIRECTION ( 'NONE',  ( -1.000000000000000000, 0.000000000000000000, 0.000000000000000000 ) ) ;
#9801 = CARTESIAN_POINT ( 'NONE',  ( 10.00000000000000000, 30.84782396557218931, 21.32104025579126017 ) ) ;
#9802 = VERTEX_POINT ( 'NONE', #35112 ) ;
#9803 = CARTESIAN_POINT ( 'NONE',  ( 0.000000000000000000, 0.000000000000000000, 0.000000000000000000 ) ) ;
#9804 = VERTEX_POINT ( 'NONE', #35839 ) ;
#9805 = CARTESIAN_POINT ( 'NONE',  ( 4.999999999999999112, -2.663952781846440576, 41.91543099594817789 ) ) ;
#9806 = ORIENTED_EDGE ( 'NONE', *, *, #31050, .F. ) ;
#9807 = VERTEX_POINT ( 'NONE', #58042 ) ;
#9808 = ORIENTED_EDGE ( 'NONE', *, *, #65190, .F. ) ;
#9809 = CARTESIAN_POINT ( 'NONE',  ( -97.30629616937501680, 90.00000000000004263, 89.80156250086714920 ) ) ;
#9810 = CYLINDRICAL_SURFACE ( 'NONE', #6626, 77.49899999999999523 ) ;
#9811 = VERTEX_POINT ( 'NONE', #8017 ) ;
#9812 = ORIENTED_EDGE ( 'NONE', *, *, #25825, .F. ) ;
#9813 = EDGE_LOOP ( 'NONE', ( #10811, #43695, #57535, #2642 ) ) ;
#9814 = CARTESIAN_POINT ( 'NONE',  ( -93.67499999999998295, -212.2949673200287179, 84.49666666666666970 ) ) ;
#9815 = CARTESIAN_POINT ( 'NONE',  ( -93.67499999999998295, -207.7050326799711968, 88.51833333333333087 ) ) ;
#9816 = CARTESIAN_POINT ( 'NONE',  ( -97.30629616937501680, 90.00000000000004263, 75.19656250086714522 ) ) ;
#9817 = ORIENTED_EDGE ( 'NONE', *, *, #4967, .F. ) ;
#9818 = CARTESIAN_POINT ( 'NONE',  ( 96.15314808468748708, 88.00268892867053694, 77.15447916753380753 ) ) ;
#9819 = ORIENTED_EDGE ( 'NONE', *, *, #50908, .F. ) ;
#9820 = DIRECTION ( 'NONE',  ( 0.000000000000000000, 0.000000000000000000, 1.000000000000000000 ) ) ;
#9821 = DIRECTION ( 'NONE',  ( 0.000000000000000000, -0.7071067811865389130, -0.7071067811865561215 ) ) ;
#9822 = ORIENTED_EDGE ( 'NONE', *, *, #23184, .T. ) ;
#9823 = CARTESIAN_POINT ( 'NONE',  ( 0.000000000000000000, 0.000000000000000000, 0.000000000000000000 ) ) ;
#9824 = DIRECTION ( 'NONE',  ( 1.000000000000000000, 1.343011723336883198E-16, -0.000000000000000000 ) ) ;
#9825 = LINE ( 'NONE', #66247, #52491 ) ;
#9826 = CARTESIAN_POINT ( 'NONE',  ( -92.69370383062498320, -208.6684592857803295, 79.85322916753379729 ) ) ;
#9827 = MECHANICAL_DESIGN_GEOMETRIC_PRESENTATION_REPRESENTATION (  '', ( #47033 ), #49434 ) ;
#9828 = AXIS2_PLACEMENT_3D ( 'NONE', #25918, #48114, #70285 ) ;
#9829 = EDGE_CURVE ( 'NONE', #26516, #22350, #69011, .T. ) ;
#9830 = DIRECTION ( 'NONE',  ( -1.000000000000000000, 0.000000000000000000, 0.000000000000000000 ) ) ;
#9831 = DIRECTION ( 'NONE',  ( 1.000000000000000000, 0.000000000000000000, 0.000000000000000000 ) ) ;
#9832 = CARTESIAN_POINT ( 'NONE',  ( -92.34999999999999432, -209.9999999999999716, 83.96750000000000114 ) ) ;
#9833 = ORIENTED_EDGE ( 'NONE', *, *, #5881, .T. ) ;
#9834 = EDGE_CURVE ( 'NONE', #46909, #21857, #42244, .T. ) ;
#9835 = VECTOR ( 'NONE', #12431, 1000.000000000000000 ) ;
#9836 = ORIENTED_EDGE ( 'NONE', *, *, #70170, .F. ) ;
#9837 = FACE_OUTER_BOUND ( 'NONE', #4562, .T. ) ;
#9838 = EDGE_CURVE ( 'NONE', #54942, #69529, #31035, .T. ) ;
#9839 = DIRECTION ( 'NONE',  ( 1.000000000000000000, 1.427937372958405461E-15, 7.962523111839130290E-16 ) ) ;
#9840 = FACE_OUTER_BOUND ( 'NONE', #39109, .T. ) ;
#9841 = CIRCLE ( 'NONE', #35068, 16.00000000000000000 ) ;
#9842 = CARTESIAN_POINT ( 'NONE',  ( -92.69370383062502583, 88.66845928578038638, 82.28739583420048120 ) ) ;
#9843 = FACE_OUTER_BOUND ( 'NONE', #61442, .T. ) ;
#9844 = CARTESIAN_POINT ( 'NONE',  ( 3.000000000000000000, -1.467624384280032501, -2.541999999999998039 ) ) ;
#9845 = VECTOR ( 'NONE', #30601, 1000.000000000000000 ) ;
#9846 = ORIENTED_EDGE ( 'NONE', *, *, #68411, .T. ) ;
#9847 = CARTESIAN_POINT ( 'NONE',  ( 0.000000000000000000, -75.11725578898470701, 2.956366410620372864 ) ) ;
#9848 = AXIS2_PLACEMENT_3D ( 'NONE', #39904, #17697, #63579 ) ;
#9849 = CYLINDRICAL_SURFACE ( 'NONE', #24494, 23.50000000000489919 ) ;
#9850 = CARTESIAN_POINT ( 'NONE',  ( 5.000000000000002665, -81.34940948281328588, -10.30890764327469711 ) ) ;
#9851 = VECTOR ( 'NONE', #53555, 1000.000000000000000 ) ;
#9852 = CARTESIAN_POINT ( 'NONE',  ( 5.000000000000000000, 22.48208911017500355, 35.47612816024530957 ) ) ;
#9853 = CARTESIAN_POINT ( 'NONE',  ( 11.99999999999999822, 0.000000000000000000, 0.000000000000000000 ) ) ;
#9854 = CARTESIAN_POINT ( 'NONE',  ( -94.99999999999997158, -207.3369185715606307, 78.21281250086717307 ) ) ;
#9855 = EDGE_CURVE ( 'NONE', #20819, #19963, #70789, .T. ) ;
#9856 = LINE ( 'NONE', #38057, #16052 ) ;
#9857 = EDGE_LOOP ( 'NONE', ( #30592, #61676, #22381, #15674 ) ) ;
#9858 = CYLINDRICAL_SURFACE ( 'NONE', #55090, 82.00000000000000000 ) ;
#9859 = CARTESIAN_POINT ( 'NONE',  ( 11.99999999999999822, -46.53671651293907274, -59.03961581697448935 ) ) ;
#9860 = CARTESIAN_POINT ( 'NONE',  ( -22.67106064244953245, -113.6342314410295842, 5.500000000000000000 ) ) ;
#9861 = EDGE_LOOP ( 'NONE', ( #22424, #70711, #14151, #65268 ) ) ;
#9862 = LINE ( 'NONE', #50451, #5353 ) ;
#9863 = FACE_OUTER_BOUND ( 'NONE', #26775, .T. ) ;
#9864 = EDGE_CURVE ( 'NONE', #30584, #37124, #47504, .T. ) ;
#9865 = EDGE_CURVE ( 'NONE', #41695, #24873, #48246, .T. ) ;
#9866 = CARTESIAN_POINT ( 'NONE',  ( -2.499999999999970690, 73.00000000000001421, -251.7000000000000455 ) ) ;
#9867 = ORIENTED_EDGE ( 'NONE', *, *, #51725, .T. ) ;
#9868 = DIRECTION ( 'NONE',  ( 0.000000000000000000, 0.000000000000000000, -1.000000000000000000 ) ) ;
#9869 = ADVANCED_FACE ( 'NONE', ( #41859 ), #6908, .F. ) ;
#9870 = LINE ( 'NONE', #20777, #72685 ) ;
#9871 = EDGE_LOOP ( 'NONE', ( #4648, #4869, #37631, #56550 ) ) ;
#9872 = CARTESIAN_POINT ( 'NONE',  ( 0.000000000000000000, -40.65526001592663619, 71.21200624218782593 ) ) ;
#9873 = DIRECTION ( 'NONE',  ( 0.000000000000000000, 0.000000000000000000, 1.000000000000000000 ) ) ;
#9874 = ORIENTED_EDGE ( 'NONE', *, *, #39727, .F. ) ;
#9875 = CARTESIAN_POINT ( 'NONE',  ( 10.00000000000000000, -37.22597642581161637, 5.202137450156258502 ) ) ;
#9876 = ORIENTED_EDGE ( 'NONE', *, *, #20156, .T. ) ;
#9877 = CARTESIAN_POINT ( 'NONE',  ( -94.99999999999997158, -206.9400435732949575, 84.84062500173429555 ) ) ;
#9878 = LINE ( 'NONE', #30304, #62399 ) ;
#9879 = AXIS2_PLACEMENT_3D ( 'NONE', #53313, #64595, #70957 ) ;
#9880 = ORIENTED_EDGE ( 'NONE', *, *, #15038, .T. ) ;
#9881 = ORIENTED_EDGE ( 'NONE', *, *, #23845, .T. ) ;
#9882 = ORIENTED_EDGE ( 'NONE', *, *, #30822, .T. ) ;
#9883 = LINE ( 'NONE', #73018, #40756 ) ;
#9884 = AXIS2_PLACEMENT_3D ( 'NONE', #47566, #74003, #16500 ) ;
#9885 = ORIENTED_EDGE ( 'NONE', *, *, #88, .F. ) ;
#9886 = VECTOR ( 'NONE', #32562, 1000.000000000000000 ) ;
#9887 = ORIENTED_EDGE ( 'NONE', *, *, #36435, .T. ) ;
#9888 = CARTESIAN_POINT ( 'NONE',  ( 93.84685191531248449, 91.99731107132950569, 76.36072916753381890 ) ) ;
#9889 = DIRECTION ( 'NONE',  ( 0.000000000000000000, -0.9723699203976789995, 0.2334453638558956767 ) ) ;
#9890 = DIRECTION ( 'NONE',  ( 1.000000000000000000, 0.000000000000000000, 0.000000000000000000 ) ) ;
#9891 = VERTEX_POINT ( 'NONE', #65542 ) ;
#9892 = EDGE_LOOP ( 'NONE', ( #28587, #69990, #698, #50394 ) ) ;
#9893 = VERTEX_POINT ( 'NONE', #21131 ) ;
#9894 = CARTESIAN_POINT ( 'NONE',  ( 94.99999999999998579, 87.33691857156068750, 88.53156250086713897 ) ) ;
#9895 = ORIENTED_EDGE ( 'NONE', *, *, #34092, .T. ) ;
#9896 = CARTESIAN_POINT ( 'NONE',  ( 96.15314808468750130, -211.9973110713294489, 86.67947916753381321 ) ) ;
#9897 = AXIS2_PLACEMENT_3D ( 'NONE', #60971, #9839, #32390 ) ;
#9898 = APPLICATION_PROTOCOL_DEFINITION ( 'draft international standard', 'automotive_design', 1998, #29179 ) ;
#9899 = CYLINDRICAL_SURFACE ( 'NONE', #41396, 2.649999999999985700 ) ;
#9900 = CARTESIAN_POINT ( 'NONE',  ( 6.000000000000003553, 3.980102097228899218E-16, 3.250000000000001332 ) ) ;
#9901 = DIRECTION ( 'NONE',  ( 0.000000000000000000, 0.000000000000000000, 1.000000000000000000 ) ) ;
#9902 = CYLINDRICAL_SURFACE ( 'NONE', #58292, 31.99999999999999289 ) ;
#9903 = CARTESIAN_POINT ( 'NONE',  ( -10.00000000000000000, 0.000000000000000000, 0.000000000000000000 ) ) ;
#9904 = CARTESIAN_POINT ( 'NONE',  ( 10.00000000000000000, 0.000000000000000000, 0.000000000000000000 ) ) ;
#9905 = CARTESIAN_POINT ( 'NONE',  ( -93.84685191531247028, -211.9973110713294489, 87.94947916753380923 ) ) ;
#9906 = CARTESIAN_POINT ( 'NONE',  ( -95.00000000000002842, 92.66308142843932671, 85.19781250086714408 ) ) ;
#9907 = VERTEX_POINT ( 'NONE', #26771 ) ;
#9909 = CARTESIAN_POINT ( 'NONE',  ( -92.69370383062502583, 91.33154071421968467, 89.37822916753381719 ) ) ;
#9908 = CARTESIAN_POINT ( 'NONE',  ( 94.99999999999998579, 87.33691857156068750, 87.26156250086714294 ) ) ;
#9910 = VERTEX_POINT ( 'NONE', #37712 ) ;
#9911 = CARTESIAN_POINT ( 'NONE',  ( 96.66077099052519372, 88.39973697852393286, 74.80065534806809069 ) ) ;
#9912 = CARTESIAN_POINT ( 'NONE',  ( -92.34999999999999432, -210.0000000207151629, 80.87187500099602744 ) ) ;
#9913 = DIRECTION ( 'NONE',  ( 0.7533909544171996098, 0.6575728627325955200, -7.625282249115660656E-32 ) ) ;
#9914 = CARTESIAN_POINT ( 'NONE',  ( 92.35003714631601213, 91.52999965978808916, 82.40645685155122635 ) ) ;
#9915 = DIRECTION ( 'NONE',  ( -0.6575728627325957421, 0.7533909544171993877, 1.230411769795008318E-16 ) ) ;
#9916 = CARTESIAN_POINT ( 'NONE',  ( 11.99999999999999822, -73.72996012237429397, -14.67089635893794508 ) ) ;
#9917 = EDGE_CURVE ( 'NONE', #55034, #70934, #20412, .T. ) ;
#9918 = DIRECTION ( 'NONE',  ( 0.000000000000000000, 0.8660254037844363761, -0.5000000000000039968 ) ) ;
#9919 = DIRECTION ( 'NONE',  ( 0.000000000000000000, 0.000000000000000000, 1.000000000000000000 ) ) ;
#9920 = ORIENTED_EDGE ( 'NONE', *, *, #39907, .F. ) ;
#9921 = EDGE_CURVE ( 'NONE', #47732, #64554, #10712, .T. ) ;
#9922 = ORIENTED_EDGE ( 'NONE', *, *, #63102, .F. ) ;
#9923 = ADVANCED_FACE ( 'NONE', ( #42980 ), #71896, .T. ) ;
#9924 = CARTESIAN_POINT ( 'NONE',  ( -92.35000000000005116, 91.52997821335253548, 82.11541666666666117 ) ) ;
#9925 = CARTESIAN_POINT ( 'NONE',  ( 10.00000000000000000, 35.95386929396241271, 10.96151621346552751 ) ) ;
#9926 = FACE_OUTER_BOUND ( 'NONE', #50166, .T. ) ;
#9927 = CYLINDRICAL_SURFACE ( 'NONE', #34808, 77.49899999999999523 ) ;
#9928 = CARTESIAN_POINT ( 'NONE',  ( -92.34999999999999432, -211.5299782133524218, 77.00895833506763211 ) ) ;
#9929 = CARTESIAN_POINT ( 'NONE',  ( 92.35000000030105127, 90.00002455906435728, 87.53856274002153270 ) ) ;
#9930 = DIRECTION ( 'NONE',  ( 0.000000000000000000, -0.8090169943749531134, 0.5877852522924653655 ) ) ;
#9931 = CARTESIAN_POINT ( 'NONE',  ( 11.99999999999999822, 81.34940948281335693, 10.30890764327412334 ) ) ;
#9932 =( BOUNDED_CURVE ( )  B_SPLINE_CURVE ( 2, ( #49955, #61262, #10115, #33038, #3761, #39070, #4498 ),
 .UNSPECIFIED., .F., .F. ) 
 B_SPLINE_CURVE_WITH_KNOTS ( ( 3, 2, 2, 3 ),
 ( 0.02083333333333322115, 0.02777777777777762705, 0.03472222222222204335, 0.04166666666666644231 ),
 .UNSPECIFIED. ) 
 CURVE ( )  GEOMETRIC_REPRESENTATION_ITEM ( )  RATIONAL_B_SPLINE_CURVE ( ( 1.000000000000002220, 0.8660254037844365982, 1.000000000000000000, 0.8660254037844387076, 1.000000000000000000, 0.8660254037844430375, 0.9999999999999956701 ) ) 
 REPRESENTATION_ITEM ( '' )  );
#9933 = ADVANCED_FACE ( 'NONE', ( #72626 ), #38065, .T. ) ;
#9934 = EDGE_LOOP ( 'NONE', ( #38381, #20928, #26410, #18533 ) ) ;
#9935 = CARTESIAN_POINT ( 'NONE',  ( -97.30629616937501680, 91.33154071421968467, 81.33489583420048064 ) ) ;
#9936 = COLOUR_RGB ( '', 0.09019608, 0.27058824, 0.51372549) ;
#9937 = ADVANCED_FACE ( 'NONE', ( #9121 ), #3508, .T. ) ;
#9938 = CARTESIAN_POINT ( 'NONE',  ( 92.35000000000000853, -209.9999999999999716, 86.18999999999999773 ) ) ;
#9939 = CIRCLE ( 'NONE', #19538, 42.00000000000000000 ) ;
#9940 = PRESENTATION_STYLE_ASSIGNMENT (( #14840 ) ) ;
#9941 = DIRECTION ( 'NONE',  ( 0.000000000000000000, -1.000000000000000000, 0.000000000000000000 ) ) ;
#9942 = DIRECTION ( 'NONE',  ( 0.000000000000000000, 0.000000000000000000, 1.000000000000000000 ) ) ;
#9943 = CARTESIAN_POINT ( 'NONE',  ( 11.99999999999999822, -70.53064760720297954, -26.01480285779911839 ) ) ;
#9944 = EDGE_CURVE ( 'NONE', #65739, #24686, #49700, .T. ) ;
#9945 = ADVANCED_FACE ( 'NONE', ( #49342 ), #14013, .T. ) ;
#9946 = CARTESIAN_POINT ( 'NONE',  ( 96.15314808468748708, 91.99731107132950569, 79.42989583420049371 ) ) ;
#9947 = CARTESIAN_POINT ( 'NONE',  ( -93.84685191531247028, -211.9973110713294489, 81.75822916753382685 ) ) ;
#9948 = CARTESIAN_POINT ( 'NONE',  ( 11.99999999999999822, 0.000000000000000000, 0.000000000000000000 ) ) ;
#9949 = EDGE_LOOP ( 'NONE', ( #38138, #9239, #71183, #58428 ) ) ;
#9950 = CARTESIAN_POINT ( 'NONE',  ( -97.64999999953499810, 89.99996900126896548, 83.09538598081491045 ) ) ;
#9951 = CARTESIAN_POINT ( 'NONE',  ( -97.64999999999994884, -208.4700217866474645, 77.24708333333332178 ) ) ;
#9952 = DIRECTION ( 'NONE',  ( -1.000000000000000000, 0.000000000000000000, -0.000000000000000000 ) ) ;
#9953 = EDGE_CURVE ( 'NONE', #36612, #60921, #55087, .T. ) ;
#9955 = EDGE_CURVE ( 'NONE', #5579, #37620, #60993, .T. ) ;
#9954 = VECTOR ( 'NONE', #55615, 1000.000000000000000 ) ;
#9956 = CARTESIAN_POINT ( 'NONE',  ( -95.00000000000002842, 87.33691857156074434, 76.62531250086715318 ) ) ;
#9957 = CARTESIAN_POINT ( 'NONE',  ( 93.84685191531251292, -211.9973110713294489, 80.85864583420047325 ) ) ;
#9958 = EDGE_LOOP ( 'NONE', ( #20346, #69259, #3930, #9335 ) ) ;
#9959 = CARTESIAN_POINT ( 'NONE',  ( -10.90076147243505211, 1.679381574624689562E-15, -13.71319123027096865 ) ) ;
#9960 = VERTEX_POINT ( 'NONE', #26037 ) ;
#9961 = CARTESIAN_POINT ( 'NONE',  ( 0.000000000000000000, -71.21200624218825226, 40.65526001592589722 ) ) ;
#9962 = VERTEX_POINT ( 'NONE', #9490 ) ;
#9963 = DIRECTION ( 'NONE',  ( -0.000000000000000000, -0.000000000000000000, 1.000000000000000000 ) ) ;
#9964 = ORIENTED_EDGE ( 'NONE', *, *, #69501, .T. ) ;
#9965 = EDGE_LOOP ( 'NONE', ( #57253, #8240, #12675, #58713 ) ) ;
#9966 = VERTEX_POINT ( 'NONE', #32413 ) ;
#9967 = CARTESIAN_POINT ( 'NONE',  ( 97.64999999999999147, -209.9999999999999716, 83.33250000000001023 ) ) ;
#9968 = CARTESIAN_POINT ( 'NONE',  ( 11.99999999999999822, -71.27951684758045303, 30.41916302227090085 ) ) ;
#9969 = APPLICATION_CONTEXT ( 'automotive_design' ) ;
#9970 = DIRECTION ( 'NONE',  ( 2.603472992746261562E-14, 2.546204323184492723E-14, -1.000000000000000000 ) ) ;
#9971 = AXIS2_PLACEMENT_3D ( 'NONE', #55903, #10032, #67185 ) ;
#9972 = CARTESIAN_POINT ( 'NONE',  ( 10.00000000000000000, 0.000000000000000000, 0.000000000000000000 ) ) ;
#9973 = CARTESIAN_POINT ( 'NONE',  ( 92.69370383062498320, 90.00000000000002842, 86.62656250086715204 ) ) ;
#9974 = CARTESIAN_POINT ( 'NONE',  ( -97.64999999996638280, -210.0000076551254722, 78.01464417100379478 ) ) ;
#9975 = CARTESIAN_POINT ( 'NONE',  ( 97.64999999999999147, -209.9999999999999716, 76.98250000000000171 ) ) ;
#9976 = EDGE_LOOP ( 'NONE', ( #60940, #26239, #8221, #6131 ) ) ;
#9977 = AXIS2_PLACEMENT_3D ( 'NONE', #37381, #30969, #60317 ) ;
#9978 = VERTEX_POINT ( 'NONE', #36958 ) ;
#9979 = VERTEX_POINT ( 'NONE', #2789 ) ;
#9980 = ORIENTED_EDGE ( 'NONE', *, *, #42054, .T. ) ;
#9981 = FILL_AREA_STYLE_COLOUR ( '', #35794 ) ;
#9982 = VECTOR ( 'NONE', #70983, 1000.000000000000000 ) ;
#9983 = DIRECTION ( 'NONE',  ( 0.000000000000000000, -0.8090169943749503378, -0.5877852522924690293 ) ) ;
#9984 = CARTESIAN_POINT ( 'NONE',  ( -93.09170270117147084, 88.16127723153179829, 74.99954709728268654 ) ) ;
#9985 = EDGE_CURVE ( 'NONE', #59733, #51512, #63746, .T. ) ;
#9986 = CARTESIAN_POINT ( 'NONE',  ( -12.49999999999999645, 0.000000000000000000, -125.0000000000000000 ) ) ;
#9987 = CARTESIAN_POINT ( 'NONE',  ( -2.499999999999970690, 73.00000000000001421, -258.2999999999999545 ) ) ;
#9988 = LINE ( 'NONE', #55112, #53587 ) ;
#9989 = EDGE_CURVE ( 'NONE', #4105, #62322, #59939, .T. ) ;
#9990 = ORIENTED_EDGE ( 'NONE', *, *, #31852, .T. ) ;
#9991 = CARTESIAN_POINT ( 'NONE',  ( -93.67499999999998295, -212.2949673200287179, 82.03604166840096923 ) ) ;
#9992 = ORIENTED_EDGE ( 'NONE', *, *, #2229, .T. ) ;
#9993 = DIRECTION ( 'NONE',  ( -1.000000000000000000, -0.000000000000000000, -0.000000000000000000 ) ) ;
#9995 = ORIENTED_EDGE ( 'NONE', *, *, #34629, .F. ) ;
#9994 = EDGE_CURVE ( 'NONE', #52585, #68824, #2289, .T. ) ;
#9996 = CARTESIAN_POINT ( 'NONE',  ( -97.65000000000001990, 90.00000000000004263, 82.45937500173430124 ) ) ;
#9997 = AXIS2_PLACEMENT_3D ( 'NONE', #40490, #53253, #12648 ) ;
#9998 = ORIENTED_EDGE ( 'NONE', *, *, #33145, .T. ) ;
#9999 = CARTESIAN_POINT ( 'NONE',  ( 92.69370383062498320, 90.00000000000002842, 82.81656250086714977 ) ) ;
#10000 = VECTOR ( 'NONE', #23924, 1000.000000000000000 ) ;
#10001 = CARTESIAN_POINT ( 'NONE',  ( -9.332068499558253905, 6.890028847512361665, -54.99999999999998579 ) ) ;
#10002 = CARTESIAN_POINT ( 'NONE',  ( 11.99999999999999822, 0.000000000000000000, 0.000000000000000000 ) ) ;
#10003 = EDGE_CURVE ( 'NONE', #16822, #69125, #38296, .T. ) ;
#10004 = DIRECTION ( 'NONE',  ( -0.000000000000000000, -0.3090169943749572767, -0.9510565162951503115 ) ) ;
#10005 = DIRECTION ( 'NONE',  ( 1.000000000000000000, 0.000000000000000000, -0.000000000000000000 ) ) ;
#10006 = CARTESIAN_POINT ( 'NONE',  ( 93.67499999999998295, 92.29496732002878900, 87.98916666666666231 ) ) ;
#10007 = ORIENTED_EDGE ( 'NONE', *, *, #70342, .F. ) ;
#10008 = DIRECTION ( 'NONE',  ( 0.000000000000000000, 0.000000000000000000, 1.000000000000000000 ) ) ;
#10010 = CYLINDRICAL_SURFACE ( 'NONE', #39755, 16.00000000000000000 ) ;
#10009 = CIRCLE ( 'NONE', #52026, 77.49900000000002365 ) ;
#10011 = VECTOR ( 'NONE', #55249, 1000.000000000000000 ) ;
#10012 = AXIS2_PLACEMENT_3D ( 'NONE', #72436, #61180, #72794 ) ;
#10013 = DIRECTION ( 'NONE',  ( 0.000000000000000000, 0.9876883405951372152, 0.1564344650402347547 ) ) ;
#10014 = VERTEX_POINT ( 'NONE', #47375 ) ;
#10015 = EDGE_CURVE ( 'NONE', #55034, #47629, #12410, .T. ) ;
#10016 = VERTEX_POINT ( 'NONE', #25541 ) ;
#10017 = DIRECTION ( 'NONE',  ( 0.000000000000000000, 0.9510565162951544194, -0.3090169943749448977 ) ) ;
#10018 = LINE ( 'NONE', #54404, #72534 ) ;
#10019 = CARTESIAN_POINT ( 'NONE',  ( -96.15314808468747287, -208.0026889286704943, 82.07572916753382231 ) ) ;
#10020 = ORIENTED_EDGE ( 'NONE', *, *, #4422, .F. ) ;
#10021 = EDGE_CURVE ( 'NONE', #69466, #55663, #8293, .T. ) ;
#10022 = DIRECTION ( 'NONE',  ( -1.000000000000000000, 0.000000000000000000, -0.000000000000000000 ) ) ;
#10023 = ORIENTED_EDGE ( 'NONE', *, *, #54268, .F. ) ;
#10024 = FACE_OUTER_BOUND ( 'NONE', #2730, .T. ) ;
#10025 = CARTESIAN_POINT ( 'NONE',  ( 94.99999999999998579, 86.94004357329502852, 81.98312500173430806 ) ) ;
#10026 = CARTESIAN_POINT ( 'NONE',  ( -97.64999999993850111, -209.9999881782113675, 76.10900611559516449 ) ) ;
#10027 = CARTESIAN_POINT ( 'NONE',  ( 97.30629616937498838, 91.33154071421968467, 79.21822916753380639 ) ) ;
#10028 = CARTESIAN_POINT ( 'NONE',  ( 10.00000000000000000, -77.16300072079680206, 27.74655509720639657 ) ) ;
#10029 = CARTESIAN_POINT ( 'NONE',  ( 0.000000000000000000, 74.65491531819105830, 8.830959090343693418 ) ) ;
#10030 = DIRECTION ( 'NONE',  ( 0.000000000000000000, -0.8526401643540970632, 0.5224985647159411384 ) ) ;
#10031 = CARTESIAN_POINT ( 'NONE',  ( 92.69400202757778118, 90.94645204372866942, 74.89836836546783161 ) ) ;
#10032 = DIRECTION ( 'NONE',  ( -1.000000000000000000, 0.000000000000000000, 0.000000000000000000 ) ) ;
#10033 = EDGE_CURVE ( 'NONE', #66558, #5889, #20248, .T. ) ;
#10034 = DIRECTION ( 'NONE',  ( -1.000000000000000000, -0.000000000000000000, 0.000000000000000000 ) ) ;
#10035 = ADVANCED_FACE ( 'NONE', ( #48478 ), #24804, .T. ) ;
#10036 = AXIS2_PLACEMENT_3D ( 'NONE', #43811, #31757, #55442 ) ;
#10037 = FACE_OUTER_BOUND ( 'NONE', #23609, .T. ) ;
#10038 = VECTOR ( 'NONE', #45230, 1000.000000000000000 ) ;
#10039 = CARTESIAN_POINT ( 'NONE',  ( 0.000000000000000000, -40.68715046381937128, 10.41901085202062660 ) ) ;
#10040 = DIRECTION ( 'NONE',  ( 0.000000000000000000, 0.000000000000000000, -1.000000000000000000 ) ) ;
#10041 = ORIENTED_EDGE ( 'NONE', *, *, #66376, .T. ) ;
#10042 = CARTESIAN_POINT ( 'NONE',  ( -95.00000000000002842, 92.66308142843932671, 83.13406250086714522 ) ) ;
#10043 = DIRECTION ( 'NONE',  ( -1.000000000000000000, 0.000000000000000000, -0.000000000000000000 ) ) ;
#10044 = CIRCLE ( 'NONE', #65333, 16.00000000000000000 ) ;
#10045 = SHAPE_REPRESENTATION ( 'CIRCLIP DIN 471 - 25 \X2\00d7\X0\ 1.2_GB_CONNECTING_PIECE_RING_RRA 25', ( #43395 ), #32718 ) ;
#10046 = FACE_OUTER_BOUND ( 'NONE', #30433, .T. ) ;
#10047 = ORIENTED_EDGE ( 'NONE', *, *, #69075, .F. ) ;
#10048 = VECTOR ( 'NONE', #22193, 1000.000000000000000 ) ;
#10049 = CARTESIAN_POINT ( 'NONE',  ( 0.000000000000000000, 0.000000000000000000, -275.0000000000000000 ) ) ;
#10051 = CARTESIAN_POINT ( 'NONE',  ( 0.000000000000000000, 27.74655509720779634, -77.16300072079631889 ) ) ;
#10050 = VECTOR ( 'NONE', #71239, 1000.000000000000114 ) ;
#10052 = CARTESIAN_POINT ( 'NONE',  ( 0.000000000000000000, 0.000000000000000000, 0.000000000000000000 ) ) ;
#10053 = AXIS2_PLACEMENT_3D ( 'NONE', #71689, #37873, #14183 ) ;
#10054 = CARTESIAN_POINT ( 'NONE',  ( 97.65000000000000568, -211.5299782133524218, 85.89895833506763267 ) ) ;
#10055 = VECTOR ( 'NONE', #64325, 1000.000000000000000 ) ;
#10056 = CARTESIAN_POINT ( 'NONE',  ( 96.15314808468748708, -208.0026889286704943, 78.79489583420048859 ) ) ;
#10057 = ORIENTED_EDGE ( 'NONE', *, *, #24022, .T. ) ;
#10058 = ORIENTED_EDGE ( 'NONE', *, *, #51354, .T. ) ;
#10059 = EDGE_CURVE ( 'NONE', #21642, #46085, #20311, .T. ) ;
#10060 = CARTESIAN_POINT ( 'NONE',  ( 11.99999999999999822, -10.30890764327323872, -81.34940948281347062 ) ) ;
#10061 = DIRECTION ( 'NONE',  ( -0.5687579148473743684, 0.8225049752423791993, 0.000000000000000000 ) ) ;
#10062 = FACE_OUTER_BOUND ( 'NONE', #34289, .T. ) ;
#10063 = CYLINDRICAL_SURFACE ( 'NONE', #23120, 37.49900000000000233 ) ;
#10064 = CARTESIAN_POINT ( 'NONE',  ( 10.00000000000000000, -12.26510123303284594, 35.53030884539080603 ) ) ;
#10065 = CARTESIAN_POINT ( 'NONE',  ( 93.67500000000001137, -207.7050326799711968, 87.98916666666666231 ) ) ;
#10066 = CIRCLE ( 'NONE', #56885, 82.00000000000000000 ) ;
#10067 = VERTEX_POINT ( 'NONE', #7521 ) ;
#10068 = CARTESIAN_POINT ( 'NONE',  ( 10.00000000000000000, 31.47745569255140552, 68.26794271651274926 ) ) ;
#10069 = VERTEX_POINT ( 'NONE', #1551 ) ;
#10070 = ORIENTED_EDGE ( 'NONE', *, *, #26619, .F. ) ;
#10071 = CARTESIAN_POINT ( 'NONE',  ( 11.59999999999999787, 1.420590287010929336E-15, -43.79999999999998295 ) ) ;
#10072 = LINE ( 'NONE', #66126, #62956 ) ;
#10073 = EDGE_CURVE ( 'NONE', #41590, #48015, #52740, .T. ) ;
#10074 = EDGE_LOOP ( 'NONE', ( #31170, #72002, #47823, #58927 ) ) ;
#10075 = CARTESIAN_POINT ( 'NONE',  ( 0.000000000000000000, -40.98264845739743123, -9.188173127307734944 ) ) ;
#10076 = CARTESIAN_POINT ( 'NONE',  ( 92.35000000000000853, -209.9999999999999716, 81.82437500173429612 ) ) ;
#10077 = CARTESIAN_POINT ( 'NONE',  ( 93.67499999999999716, 87.70503267997126784, 83.12083333333332291 ) ) ;
#10078 = EDGE_CURVE ( 'NONE', #48721, #7988, #50305, .T. ) ;
#10079 = ORIENTED_EDGE ( 'NONE', *, *, #73385, .T. ) ;
#10080 = DIRECTION ( 'NONE',  ( 0.000000000000000000, 0.3090169943749580539, -0.9510565162951499785 ) ) ;
#10081 = EDGE_LOOP ( 'NONE', ( #31693, #54210, #1625, #72846 ) ) ;
#10082 = CARTESIAN_POINT ( 'NONE',  ( 11.99999999999999822, -73.44644590900077219, 24.73286445877677764 ) ) ;
#10083 = VECTOR ( 'NONE', #23615, 1000.000000000000114 ) ;
#10084 = ORIENTED_EDGE ( 'NONE', *, *, #56033, .F. ) ;
#10085 = LINE ( 'NONE', #15346, #9182 ) ;
#10086 = CARTESIAN_POINT ( 'NONE',  ( -93.84685191531252713, 88.00268892867056536, 83.02822916753380866 ) ) ;
#10087 = CARTESIAN_POINT ( 'NONE',  ( 93.84685191531248449, 88.00268892867053694, 78.95364583420047211 ) ) ;
#10088 = ORIENTED_EDGE ( 'NONE', *, *, #25903, .F. ) ;
#10089 = ADVANCED_FACE ( 'NONE', ( #48109 ), #65416, .T. ) ;
#10090 = DIRECTION ( 'NONE',  ( 0.000000000000000000, 0.9945218953682730678, -0.1045284632676570929 ) ) ;
#10091 = ADVANCED_FACE ( 'NONE', ( #53746 ), #59034, .F. ) ;
#10092 = FACE_OUTER_BOUND ( 'NONE', #67310, .T. ) ;
#10093 = DIRECTION ( 'NONE',  ( 0.000000000000000000, 0.4067366430757887730, -0.9135454576426059736 ) ) ;
#10094 = ORIENTED_EDGE ( 'NONE', *, *, #47052, .T. ) ;
#10095 = LINE ( 'NONE', #33017, #59704 ) ;
#10096 = CARTESIAN_POINT ( 'NONE',  ( -94.99999999999997158, -212.6630814284392557, 81.54656250086715374 ) ) ;
#10097 = VECTOR ( 'NONE', #35765, 1000.000000000000114 ) ;
#10098 = ORIENTED_EDGE ( 'NONE', *, *, #17345, .T. ) ;
#10099 = ORIENTED_EDGE ( 'NONE', *, *, #51648, .F. ) ;
#10100 = CARTESIAN_POINT ( 'NONE',  ( 97.64999999999997726, 91.52997821335253548, 78.94041666666664980 ) ) ;
#10101 = VERTEX_POINT ( 'NONE', #71392 ) ;
#10102 = DIRECTION ( 'NONE',  ( -1.000000000000000000, 0.000000000000000000, -0.000000000000000000 ) ) ;
#10103 = VECTOR ( 'NONE', #57068, 1000.000000000000000 ) ;
#10104 = CARTESIAN_POINT ( 'NONE',  ( 93.67499999999998295, 92.29496732002878900, 89.33854166840096411 ) ) ;
#10105 = EDGE_LOOP ( 'NONE', ( #52493, #65577, #62284, #36774 ) ) ;
#10106 = CARTESIAN_POINT ( 'NONE',  ( -94.99999999999997158, -207.3369185715606307, 79.95906250086713385 ) ) ;
#10107 = ORIENTED_EDGE ( 'NONE', *, *, #42346, .F. ) ;
#10109 = ADVANCED_FACE ( 'NONE', ( #47734 ), #12774, .T. ) ;
#10108 = CARTESIAN_POINT ( 'NONE',  ( -92.34999999999998010, 88.47002178664757821, 86.45458333333331780 ) ) ;
#10110 = DIRECTION ( 'NONE',  ( 0.000000000000000000, -0.9876883405951359940, -0.1564344650402420267 ) ) ;
#10111 = CARTESIAN_POINT ( 'NONE',  ( -15.44521549751111422, -137.7748507232956001, 5.500000000000000000 ) ) ;
#10112 = DIRECTION ( 'NONE',  ( -7.728965982074743403E-16, -1.065814103640131346E-14, -1.000000000000000000 ) ) ;
#10113 = CARTESIAN_POINT ( 'NONE',  ( -95.00000000000002842, 86.94004357329504273, 81.26874999999999716 ) ) ;
#10114 = AXIS2_PLACEMENT_3D ( 'NONE', #11432, #44554, #73841 ) ;
#10115 = CARTESIAN_POINT ( 'NONE',  ( -93.67500000000003979, 87.70503267997129626, 89.57666666666666799 ) ) ;
#10116 = CARTESIAN_POINT ( 'NONE',  ( 97.30629616937498838, 91.33154071421968467, 89.37822916753378877 ) ) ;
#10117 = DIRECTION ( 'NONE',  ( -0.000000000000000000, -0.000000000000000000, 1.000000000000000000 ) ) ;
#10118 = DIRECTION ( 'NONE',  ( 0.000000000000000000, -0.5877852522924624790, -0.8090169943749553338 ) ) ;
#10119 = CYLINDRICAL_SURFACE ( 'NONE', #36070, 31.99999999999998579 ) ;
#10120 = DIRECTION ( 'NONE',  ( -0.000000000000000000, -0.000000000000000000, -1.000000000000000000 ) ) ;
#10121 = CARTESIAN_POINT ( 'NONE',  ( 92.35002600474520307, 88.47000677280088610, 86.32229270695526679 ) ) ;
#10122 = EDGE_CURVE ( 'NONE', #44625, #36499, #30797, .T. ) ;
#10123 = DIRECTION ( 'NONE',  ( 0.000000000000000000, 0.000000000000000000, -1.000000000000000000 ) ) ;
#10124 = DIRECTION ( 'NONE',  ( 1.000000000000000000, 0.000000000000000000, 0.000000000000000000 ) ) ;
#10125 = VECTOR ( 'NONE', #18022, 1000.000000000000000 ) ;
#10126 = DIRECTION ( 'NONE',  ( 0.000000000000000000, -0.8526401643540860720, -0.5224985647159590130 ) ) ;
#10127 = EDGE_CURVE ( 'NONE', #8792, #8349, #62304, .T. ) ;
#10128 = LINE ( 'NONE', #54154, #5263 ) ;
#10129 = CIRCLE ( 'NONE', #5330, 16.00000000000000000 ) ;
#10130 = DIRECTION ( 'NONE',  ( -1.000000000000000000, 0.000000000000000000, 0.000000000000000000 ) ) ;
#10131 = CARTESIAN_POINT ( 'NONE',  ( 0.000000000000000000, -26.79245525562738095, 32.34446384429961796 ) ) ;
#10132 = DIRECTION ( 'NONE',  ( 0.8571673007021122226, 0.000000000000000000, 0.5150380749100542666 ) ) ;
#10133 = CARTESIAN_POINT ( 'NONE',  ( -94.99999999999997158, -206.9400435732949575, 84.12625000000001307 ) ) ;
#10134 = DIRECTION ( 'NONE',  ( 0.000000000000000000, 0.000000000000000000, 1.000000000000000000 ) ) ;
#10135 = VECTOR ( 'NONE', #19358, 1000.000000000000000 ) ;
#10136 =( BOUNDED_CURVE ( )  B_SPLINE_CURVE ( 2, ( #56868, #45597, #15519, #9877, #27906, #51208, #73764 ),
 .UNSPECIFIED., .F., .F. ) 
 B_SPLINE_CURVE_WITH_KNOTS ( ( 3, 2, 2, 3 ),
 ( 0.2963422021995995026, 0.3033979182594312429, 0.3104536838003485455, 0.3175094496522546383 ),
 .UNSPECIFIED. ) 
 CURVE ( )  GEOMETRIC_REPRESENTATION_ITEM ( )  RATIONAL_B_SPLINE_CURVE ( ( 0.9999981209233991253, 0.8660263433293280411, 1.000000000000000000, 0.8660254037844387076, 1.000000000000000000, 0.8660254037844387076, 1.000000000000000000 ) ) 
 REPRESENTATION_ITEM ( '' )  );
#10137 = DIRECTION ( 'NONE',  ( -0.000000000000000000, 0.4999999999999921174, -0.8660254037844432595 ) ) ;
#10138 = CYLINDRICAL_SURFACE ( 'NONE', #28729, 77.49899999999999523 ) ;
#10139 = DIRECTION ( 'NONE',  ( 0.000000000000000000, 0.000000000000000000, 1.000000000000000000 ) ) ;
#10140 = CARTESIAN_POINT ( 'NONE',  ( -2.500000000000000000, 3.061616997868383141E-16, -6.000000000000000000 ) ) ;
#10141 = CIRCLE ( 'NONE', #52170, 31.99999999999998579 ) ;
#10142 = CARTESIAN_POINT ( 'NONE',  ( 97.30629616937498838, -208.6684592857803011, 88.26697916753381890 ) ) ;
#10143 = ORIENTED_EDGE ( 'NONE', *, *, #29799, .T. ) ;
#10144 = EDGE_LOOP ( 'NONE', ( #74260, #42905, #52448, #15659 ) ) ;
#10145 = LINE ( 'NONE', #33067, #45566 ) ;
#10146 = DIRECTION ( 'NONE',  ( 0.000000000000000000, -0.4539904997395540764, 0.8910065241883642351 ) ) ;
#10147 = ORIENTED_EDGE ( 'NONE', *, *, #43144, .F. ) ;
#10148 = CARTESIAN_POINT ( 'NONE',  ( 96.15314808468748708, -208.0026889286704943, 79.27114583420046756 ) ) ;
#10149 = CARTESIAN_POINT ( 'NONE',  ( 95.00000000000000000, -212.6630814284392557, 86.15031250086717307 ) ) ;
#10150 = AXIS2_PLACEMENT_3D ( 'NONE', #482, #18102, #34643 ) ;
#10151 = ORIENTED_EDGE ( 'NONE', *, *, #14610, .T. ) ;
#10152 = VECTOR ( 'NONE', #70732, 1000.000000000000000 ) ;
#10153 = CARTESIAN_POINT ( 'NONE',  ( 96.15314808468748708, -208.0026889286704943, 87.04989583420048405 ) ) ;
#10154 = EDGE_CURVE ( 'NONE', #6866, #2581, #19076, .T. ) ;
#10155 = ORIENTED_EDGE ( 'NONE', *, *, #17095, .T. ) ;
#10156 = CARTESIAN_POINT ( 'NONE',  ( 10.00000000000000000, 0.000000000000000000, 0.000000000000000000 ) ) ;
#10157 = ORIENTED_EDGE ( 'NONE', *, *, #46673, .T. ) ;
#10158 = AXIS2_PLACEMENT_3D ( 'NONE', #38066, #2430, #54622 ) ;
#10159 =( LENGTH_UNIT ( ) NAMED_UNIT ( * ) SI_UNIT ( .MILLI., .METRE. ) );
#10160 = EDGE_LOOP ( 'NONE', ( #60662, #45532, #70859, #24155 ) ) ;
#10161 = DIRECTION ( 'NONE',  ( 0.9730327541852493711, -0.2306669878475637314, 0.000000000000000000 ) ) ;
#10162 = EDGE_CURVE ( 'NONE', #26875, #44562, #54129, .T. ) ;
#10163 = ORIENTED_EDGE ( 'NONE', *, *, #45450, .F. ) ;
#10164 = CARTESIAN_POINT ( 'NONE',  ( -95.00000000000002842, 86.94004357329504273, 77.45874999999999488 ) ) ;
#10165 = CARTESIAN_POINT ( 'NONE',  ( 0.000000000000000000, -75.11764819372149304, 2.946379043146075905 ) ) ;
#10166 = EDGE_CURVE ( 'NONE', #68072, #11081, #58650, .T. ) ;
#10167 = ORIENTED_EDGE ( 'NONE', *, *, #31062, .F. ) ;
#10168 = CARTESIAN_POINT ( 'NONE',  ( 0.000000000000000000, 8.966570791700705811, 81.50828551894228724 ) ) ;
#10169 = AXIS2_PLACEMENT_3D ( 'NONE', #4076, #59725, #26973 ) ;
#10170 = ORIENTED_EDGE ( 'NONE', *, *, #35051, .F. ) ;
#10171 = DIRECTION ( 'NONE',  ( -1.000000000000000000, 0.000000000000000000, 0.000000000000000000 ) ) ;
#10172 = ORIENTED_EDGE ( 'NONE', *, *, #9668, .F. ) ;
#10173 = CIRCLE ( 'NONE', #67829, 15.99999999999999645 ) ;
#10174 = EDGE_CURVE ( 'NONE', #23811, #6866, #11884, .T. ) ;
#10175 = ORIENTED_EDGE ( 'NONE', *, *, #44383, .F. ) ;
#10176 = ORIENTED_EDGE ( 'NONE', *, *, #18154, .T. ) ;
#10177 = CARTESIAN_POINT ( 'NONE',  ( 0.000000000000000000, 41.81611651403861885, 3.925862922256313503 ) ) ;
#10178 = CARTESIAN_POINT ( 'NONE',  ( 21.85433023846371370, -135.0628101570779620, 5.500000000000000000 ) ) ;
#10179 = ORIENTED_EDGE ( 'NONE', *, *, #18280, .F. ) ;
#10180 = ORIENTED_EDGE ( 'NONE', *, *, #55064, .F. ) ;
#10181 = VERTEX_POINT ( 'NONE', #60873 ) ;
#10182 = LINE ( 'NONE', #33103, #12101 ) ;
#10183 = CARTESIAN_POINT ( 'NONE',  ( -97.30629616937501680, 88.66845928578038638, 75.88447916753382572 ) ) ;
#10184 = VERTEX_POINT ( 'NONE', #49209 ) ;
#10185 = EDGE_CURVE ( 'NONE', #237, #25980, #38687, .T. ) ;
#10186 = CARTESIAN_POINT ( 'NONE',  ( 94.99999999999998579, 92.66308142843935514, 76.78406250086712248 ) ) ;
#10187 = EDGE_LOOP ( 'NONE', ( #41812, #65272, #41711, #17592 ) ) ;
#10188 = CARTESIAN_POINT ( 'NONE',  ( 97.65000000000000568, 91.52997821335252127, 78.38479166840096468 ) ) ;
#10189 = CARTESIAN_POINT ( 'NONE',  ( -93.84685191531247028, -211.9973110713294489, 89.21947916753380525 ) ) ;
#10190 = ORIENTED_EDGE ( 'NONE', *, *, #53039, .F. ) ;
#10192 = ADVANCED_FACE ( 'NONE', ( #4486 ), #9358, .F. ) ;
#10191 = CARTESIAN_POINT ( 'NONE',  ( 92.35000000046409241, 89.99996903277681781, 77.38038495127642591 ) ) ;
#10193 = CARTESIAN_POINT ( 'NONE',  ( 0.000000000000000000, -37.58145647212455032, 16.68533520207890319 ) ) ;
#10194 = DIRECTION ( 'NONE',  ( -1.000000000000000000, 0.000000000000000000, 0.000000000000000000 ) ) ;
#10195 = ADVANCED_FACE ( 'NONE', ( #31542 ), #32655, .T. ) ;
#10196 = CARTESIAN_POINT ( 'NONE',  ( -92.69370383062498320, -208.6684592857803295, 79.21822916753380639 ) ) ;
#10197 = CARTESIAN_POINT ( 'NONE',  ( 10.00000000000000000, 0.000000000000000000, 0.000000000000000000 ) ) ;
#10198 = CARTESIAN_POINT ( 'NONE',  ( 10.00000000000000000, 2.956366410620650420, 75.11725578898469280 ) ) ;
#10199 = CARTESIAN_POINT ( 'NONE',  ( -93.67499999999998295, -212.2949673200287179, 79.41666666666665719 ) ) ;
#10200 = VERTEX_POINT ( 'NONE', #32281 ) ;
#10201 = CIRCLE ( 'NONE', #52219, 31.99999999999998579 ) ;
#10202 = ORIENTED_EDGE ( 'NONE', *, *, #68598, .F. ) ;
#10203 = DIRECTION ( 'NONE',  ( -1.000000000000000000, -0.000000000000000000, -0.000000000000000000 ) ) ;
#10204 = DIRECTION ( 'NONE',  ( -1.000000000000000000, 0.000000000000000000, 0.000000000000000000 ) ) ;
#10205 = CARTESIAN_POINT ( 'NONE',  ( 92.48632958231168288, -210.0000000000000284, 74.91808492278046572 ) ) ;
#10206 = EDGE_CURVE ( 'NONE', #51805, #24766, #27013, .T. ) ;
#10207 = CARTESIAN_POINT ( 'NONE',  ( -97.30629616937501680, 90.00000000000004263, 83.29281250086714294 ) ) ;
#10208 = CARTESIAN_POINT ( 'NONE',  ( 0.000000000000000000, 68.67312586195046720, -35.91791733033402068 ) ) ;
#10209 = DIRECTION ( 'NONE',  ( -1.000000000000000000, -0.000000000000000000, 0.000000000000000000 ) ) ;
#10210 = CIRCLE ( 'NONE', #1833, 82.00000000000000000 ) ;
#10211 = ORIENTED_EDGE ( 'NONE', *, *, #49340, .F. ) ;
#10212 = AXIS2_PLACEMENT_3D ( 'NONE', #44030, #50396, #31991 ) ;
#10213 = CARTESIAN_POINT ( 'NONE',  ( 3.000000000000000000, 2.935248768560057897, -3.252606517456513302E-15 ) ) ;
#10215 = DIRECTION ( 'NONE',  ( -1.000000000000000000, -0.000000000000000000, 0.000000000000000000 ) ) ;
#10214 = CIRCLE ( 'NONE', #63116, 82.00000000000000000 ) ;
#10216 = CYLINDRICAL_SURFACE ( 'NONE', #23761, 2.649999999999985700 ) ;
#10217 = CARTESIAN_POINT ( 'NONE',  ( 10.00000000000000000, 0.000000000000000000, 0.000000000000000000 ) ) ;
#10218 = CARTESIAN_POINT ( 'NONE',  ( -96.32500000000001705, 92.29496732002878900, 89.89416666666666345 ) ) ;
#10219 = CARTESIAN_POINT ( 'NONE',  ( 10.00000000000000000, -46.53671651293907274, -59.03961581697448935 ) ) ;
#10220 = CARTESIAN_POINT ( 'NONE',  ( -92.69370383062498320, -211.3315407142195852, 79.90614583420048689 ) ) ;
#10221 = VECTOR ( 'NONE', #21766, 1000.000000000000000 ) ;
#10222 = CARTESIAN_POINT ( 'NONE',  ( 92.34999999999999432, 88.47002178664752137, 76.16229166840095388 ) ) ;
#10223 = ORIENTED_EDGE ( 'NONE', *, *, #27512, .F. ) ;
#10224 = CARTESIAN_POINT ( 'NONE',  ( 11.99999999999999822, 81.50828551894227303, 8.966570791700986476 ) ) ;
#10225 = VECTOR ( 'NONE', #9640, 1000.000000000000114 ) ;
#10226 = LINE ( 'NONE', #56096, #5896 ) ;
#10227 = DIRECTION ( 'NONE',  ( -7.571541139946887334E-15, 1.000000000000000000, 2.546204323184473159E-14 ) ) ;
#10228 = VERTEX_POINT ( 'NONE', #43598 ) ;
#10229 = CARTESIAN_POINT ( 'NONE',  ( 0.000000000000000000, -22.90783923731685334, 78.73519480814945837 ) ) ;
#10230 = DIRECTION ( 'NONE',  ( 0.000000000000000000, -0.5877852522924801315, 0.8090169943749423442 ) ) ;
#10231 = LINE ( 'NONE', #26774, #11980 ) ;
#10232 = ORIENTED_EDGE ( 'NONE', *, *, #53316, .T. ) ;
#10233 = CARTESIAN_POINT ( 'NONE',  ( -92.35000000000005116, 91.52997821335253548, 75.84479166840098685 ) ) ;
#10234 = FACE_OUTER_BOUND ( 'NONE', #73021, .T. ) ;
#10235 = VERTEX_POINT ( 'NONE', #15749 ) ;
#10236 = AXIS2_PLACEMENT_3D ( 'NONE', #49522, #72448, #48783 ) ;
#10237 = CARTESIAN_POINT ( 'NONE',  ( 93.84685191531249870, -208.0026889286704943, 89.53697916753381492 ) ) ;
#10238 = CARTESIAN_POINT ( 'NONE',  ( 0.000000000000000000, -55.16347631942998220, -60.67117009219196433 ) ) ;
#10239 = ORIENTED_EDGE ( 'NONE', *, *, #62397, .F. ) ;
#10240 = ADVANCED_FACE ( 'NONE', ( #37209 ), #8634, .T. ) ;
#10241 = CARTESIAN_POINT ( 'NONE',  ( 0.000000000000000000, -25.60904388321916514, -6.976881207771517879 ) ) ;
#10242 = ORIENTED_EDGE ( 'NONE', *, *, #60934, .T. ) ;
#10243 = DIRECTION ( 'NONE',  ( 0.000000000000000000, 0.000000000000000000, 1.000000000000000000 ) ) ;
#10244 = ORIENTED_EDGE ( 'NONE', *, *, #26040, .T. ) ;
#10245 = AXIS2_PLACEMENT_3D ( 'NONE', #42644, #8437, #43407 ) ;
#10246 = CARTESIAN_POINT ( 'NONE',  ( 3.429551818649054340, -146.3199197248623875, 2.500000000000000000 ) ) ;
#10247 = ADVANCED_FACE ( 'NONE', ( #49946 ), #58452, .F. ) ;
#10248 = VERTEX_POINT ( 'NONE', #33479 ) ;
#10249 = VERTEX_POINT ( 'NONE', #68464 ) ;
#10250 = EDGE_CURVE ( 'NONE', #25604, #73822, #39518, .T. ) ;
#10251 = EDGE_CURVE ( 'NONE', #29023, #32074, #24106, .T. ) ;
#10252 = ORIENTED_EDGE ( 'NONE', *, *, #13815, .T. ) ;
#10253 = DIRECTION ( 'NONE',  ( 0.000000000000000000, 0.000000000000000000, -1.000000000000000000 ) ) ;
#10254 = ORIENTED_EDGE ( 'NONE', *, *, #10623, .F. ) ;
#10256 = EDGE_CURVE ( 'NONE', #23771, #48987, #48785, .T. ) ;
#10255 = VERTEX_POINT ( 'NONE', #51149 ) ;
#10257 = CARTESIAN_POINT ( 'NONE',  ( 93.84685191531248449, 88.00268892867053694, 75.93739583420048689 ) ) ;
#10258 = VECTOR ( 'NONE', #57373, 1000.000000000000000 ) ;
#10259 = DIRECTION ( 'NONE',  ( 0.000000000000000000, 0.4539904997395414754, 0.8910065241883706744 ) ) ;
#10261 = CARTESIAN_POINT ( 'NONE',  ( 5.999999999999998224, 6.123233995736766282E-16, -5.000000000000000000 ) ) ;
#10260 = AXIS2_PLACEMENT_3D ( 'NONE', #69739, #70100, #18601 ) ;
#10262 = ORIENTED_EDGE ( 'NONE', *, *, #66198, .F. ) ;
#10263 = ORIENTED_EDGE ( 'NONE', *, *, #43882, .T. ) ;
#10264 = EDGE_CURVE ( 'NONE', #18236, #50093, #46735, .T. ) ;
#10265 = ORIENTED_EDGE ( 'NONE', *, *, #42684, .F. ) ;
#10266 = CARTESIAN_POINT ( 'NONE',  ( 96.15314808468748708, 91.99731107132950569, 88.16114583420046813 ) ) ;
#10267 = VERTEX_POINT ( 'NONE', #5684 ) ;
#10268 = VECTOR ( 'NONE', #43015, 1000.000000000000114 ) ;
#10269 = CARTESIAN_POINT ( 'NONE',  ( 95.00000000000000000, -212.6630814284392557, 85.35656250086714181 ) ) ;
#10270 = APPLICATION_PROTOCOL_DEFINITION ( 'draft international standard', 'automotive_design', 1998, #43597 ) ;
#10271 = FACE_OUTER_BOUND ( 'NONE', #61898, .T. ) ;
#10272 = CARTESIAN_POINT ( 'NONE',  ( -97.64999999999986358, -208.4700217866474361, 80.42208333333330472 ) ) ;
#10273 = CARTESIAN_POINT ( 'NONE',  ( 10.00000000000000000, 26.08949754953062694, -27.05870788708203989 ) ) ;
#10274 = CARTESIAN_POINT ( 'NONE',  ( 2.949999999999999734, 0.000000000000000000, 2.499999999999999556 ) ) ;
#10275 = AXIS2_PLACEMENT_3D ( 'NONE', #19364, #59600, #42315 ) ;
#10276 = CARTESIAN_POINT ( 'NONE',  ( 0.000000000000000000, -62.50884508063453637, 41.76106447765467777 ) ) ;
#10277 = DIRECTION ( 'NONE',  ( 0.000000000000000000, 0.2079116908177664758, -0.9781476007338042455 ) ) ;
#10278 = CARTESIAN_POINT ( 'NONE',  ( -97.30629616937495996, -209.9999999999999716, 87.73781250086713612 ) ) ;
#10279 = CARTESIAN_POINT ( 'NONE',  ( -97.30629616937501680, 88.66845928578038638, 86.04447916753382231 ) ) ;
#10280 = ORIENTED_EDGE ( 'NONE', *, *, #3744, .F. ) ;
#10282 = CARTESIAN_POINT ( 'NONE',  ( -93.84685191531252713, 88.00268892867056536, 88.58447916753381435 ) ) ;
#10281 = CARTESIAN_POINT ( 'NONE',  ( 93.84685191531248449, 91.99731107132950569, 86.99697916753380866 ) ) ;
#10283 = AXIS2_PLACEMENT_3D ( 'NONE', #12510, #36183, #59129 ) ;
#10284 = EDGE_LOOP ( 'NONE', ( #48432, #38739, #46367, #2711, #52690, #21077 ) ) ;
#10285 = LINE ( 'NONE', #61803, #39466 ) ;
#10287 = EDGE_CURVE ( 'NONE', #33066, #3022, #56811, .T. ) ;
#10286 = DIRECTION ( 'NONE',  ( -0.000000000000000000, -0.000000000000000000, 1.000000000000000000 ) ) ;
#10288 = CYLINDRICAL_SURFACE ( 'NONE', #71537, 5.000000000000000000 ) ;
#10289 = DIRECTION ( 'NONE',  ( -1.000000000000000000, 0.000000000000000000, -0.000000000000000000 ) ) ;
#10291 = EDGE_CURVE ( 'NONE', #38100, #5092, #22595, .T. ) ;
#10290 = AXIS2_PLACEMENT_3D ( 'NONE', #71205, #37403, #60334 ) ;
#10292 = CARTESIAN_POINT ( 'NONE',  ( -96.32500000000001705, 92.29496732002878900, 86.71916666666666629 ) ) ;
#10293 = LINE ( 'NONE', #68181, #73870 ) ;
#10294 = DIRECTION ( 'NONE',  ( -0.000000000000000000, 0.1045284632676436315, 0.9945218953682742891 ) ) ;
#10295 = ADVANCED_FACE ( 'NONE', ( #51526 ), #57551, .F. ) ;
#10296 = EDGE_CURVE ( 'NONE', #13681, #12324, #22976, .T. ) ;
#10297 = DIRECTION ( 'NONE',  ( 2.603472992745699578E-14, -2.546204323184531851E-14, 1.000000000000000000 ) ) ;
#10298 = ORIENTED_EDGE ( 'NONE', *, *, #51013, .T. ) ;
#10299 = STYLED_ITEM ( 'NONE', ( #49708 ), #37525 ) ;
#10300 = ORIENTED_EDGE ( 'NONE', *, *, #10933, .F. ) ;
#10301 = CARTESIAN_POINT ( 'NONE',  ( -96.32500000000001705, 92.29496732002878900, 80.36916666666665776 ) ) ;
#10302 = DIRECTION ( 'NONE',  ( 0.000000000000000000, -0.3090169943749548898, 0.9510565162951511997 ) ) ;
#10303 = EDGE_CURVE ( 'NONE', #6668, #67482, #1149, .T. ) ;
#10304 = DIRECTION ( 'NONE',  ( -1.000000000000000000, 0.000000000000000000, 0.000000000000000000 ) ) ;
#10305 = CARTESIAN_POINT ( 'NONE',  ( 0.000000000000000000, 6.555932627142952995, -37.01155633439051940 ) ) ;
#10306 = CARTESIAN_POINT ( 'NONE',  ( 4.999999999999999112, -40.68715046381921496, -10.41901085202121280 ) ) ;
#10307 = CARTESIAN_POINT ( 'NONE',  ( 10.00000000000000000, -76.41127070299262414, -12.93880638057396304 ) ) ;
#10308 = CARTESIAN_POINT ( 'NONE',  ( 0.000000000000000000, 41.19522573413826194, -65.64334221924865176 ) ) ;
#10309 = ORIENTED_EDGE ( 'NONE', *, *, #47890, .F. ) ;
#10310 = CARTESIAN_POINT ( 'NONE',  ( -97.30629616937501680, 91.33154071421968467, 82.60489583420047666 ) ) ;
#10311 = FACE_OUTER_BOUND ( 'NONE', #11808, .T. ) ;
#10312 = LINE ( 'NONE', #20849, #21015 ) ;
#10313 = CYLINDRICAL_SURFACE ( 'NONE', #69401, 31.99999999999998579 ) ;
#10314 = LINE ( 'NONE', #27605, #46495 ) ;
#10315 = CARTESIAN_POINT ( 'NONE',  ( -93.67500000000003979, 92.29496732002878900, 82.16833333333332234 ) ) ;
#10316 = CARTESIAN_POINT ( 'NONE',  ( -94.99999999999997158, -212.6630814284392557, 88.05531250086716000 ) ) ;
#10317 =( NAMED_UNIT ( * ) PLANE_ANGLE_UNIT ( ) SI_UNIT ( $, .RADIAN. ) );
#10318 = VECTOR ( 'NONE', #35076, 1000.000000000000000 ) ;
#10319 = CARTESIAN_POINT ( 'NONE',  ( 92.69370383062498320, 91.33154071421968467, 79.58864583420049144 ) ) ;
#10320 = CARTESIAN_POINT ( 'NONE',  ( -92.69370383062498320, -208.6684592857803295, 80.01197916753382344 ) ) ;
#10321 = CARTESIAN_POINT ( 'NONE',  ( -2.500000000000000000, 16.00000000000000000, -10.00000000000000178 ) ) ;
#10322 = ORIENTED_EDGE ( 'NONE', *, *, #13581, .T. ) ;
#10323 = CARTESIAN_POINT ( 'NONE',  ( 93.67500000000001137, -207.7050326799711968, 81.08354166840096866 ) ) ;
#10324 = CARTESIAN_POINT ( 'NONE',  ( -92.34999999999999432, -208.4700217866474645, 75.76541666666666686 ) ) ;
#10325 = CARTESIAN_POINT ( 'NONE',  ( 92.35000000010806787, -209.9999848944895007, 78.64888723592486031 ) ) ;
#10326 = CIRCLE ( 'NONE', #3115, 77.49900000000000944 ) ;
#10327 = VECTOR ( 'NONE', #32674, 1000.000000000000000 ) ;
#10328 = CARTESIAN_POINT ( 'NONE',  ( -93.84685191531254134, 91.99731107132950569, 78.15989583420049769 ) ) ;
#10329 = CARTESIAN_POINT ( 'NONE',  ( 93.84685191531249870, -208.0026889286704943, 80.01197916753380923 ) ) ;
#10330 = ORIENTED_EDGE ( 'NONE', *, *, #20110, .F. ) ;
#10331 = ORIENTED_EDGE ( 'NONE', *, *, #17541, .T. ) ;
#10332 = CIRCLE ( 'NONE', #52354, 37.49900000000000944 ) ;
#10333 = LINE ( 'NONE', #20510, #39267 ) ;
#10334 = ORIENTED_EDGE ( 'NONE', *, *, #45699, .F. ) ;
#10335 = EDGE_CURVE ( 'NONE', #32157, #3438, #440, .T. ) ;
#10336 = DIRECTION ( 'NONE',  ( -1.000000000000000000, -0.000000000000000000, -0.000000000000000000 ) ) ;
#10337 = ADVANCED_FACE ( 'NONE', ( #30069 ), #48476, .T. ) ;
#10338 = CIRCLE ( 'NONE', #33141, 16.00000000000000000 ) ;
#10339 = ORIENTED_EDGE ( 'NONE', *, *, #58569, .T. ) ;
#10340 = ORIENTED_EDGE ( 'NONE', *, *, #42466, .F. ) ;
#10342 = EDGE_CURVE ( 'NONE', #719, #27052, #64768, .T. ) ;
#10341 = ORIENTED_EDGE ( 'NONE', *, *, #13473, .T. ) ;
#10343 = EDGE_CURVE ( 'NONE', #62606, #57645, #47373, .T. ) ;
#10344 = CARTESIAN_POINT ( 'NONE',  ( 96.15314808468750130, -211.9973110713294489, 76.04322916753382344 ) ) ;
#10345 = VERTEX_POINT ( 'NONE', #7150 ) ;
#10346 = CYLINDRICAL_SURFACE ( 'NONE', #53211, 12.75000000000265565 ) ;
#10347 = CARTESIAN_POINT ( 'NONE',  ( 92.35000000000000853, -209.9999999999999716, 83.65000000000000568 ) ) ;
#10348 = CARTESIAN_POINT ( 'NONE',  ( 92.69370383062498320, 91.33154071421968467, 85.93864583420048575 ) ) ;
#10349 = PLANE ( 'NONE',  #30935 ) ;
#10350 = CARTESIAN_POINT ( 'NONE',  ( 97.64999999999997726, -208.4700217866474645, 79.57541666666665492 ) ) ;
#10351 = ORIENTED_EDGE ( 'NONE', *, *, #30279, .T. ) ;
#10352 = ORIENTED_EDGE ( 'NONE', *, *, #14283, .F. ) ;
#10353 = ORIENTED_EDGE ( 'NONE', *, *, #28330, .F. ) ;
#10354 = ORIENTED_EDGE ( 'NONE', *, *, #37523, .T. ) ;
#10355 = CARTESIAN_POINT ( 'NONE',  ( 15.00000000000000000, -4.261787119645322974, -26.19803753235774835 ) ) ;
#10356 =( NAMED_UNIT ( * ) PLANE_ANGLE_UNIT ( ) SI_UNIT ( $, .RADIAN. ) );
#10357 = CARTESIAN_POINT ( 'NONE',  ( 0.000000000000000000, 0.000000000000000000, 0.000000000000000000 ) ) ;
#10358 = LINE ( 'NONE', #4748, #2698 ) ;
#10359 = DIRECTION ( 'NONE',  ( -0.000000000000000000, -0.000000000000000000, -1.000000000000000000 ) ) ;
#10360 = DIRECTION ( 'NONE',  ( 0.000000000000000000, 0.000000000000000000, 1.000000000000000000 ) ) ;
#10361 = ADVANCED_FACE ( 'NONE', ( #71391 ), #64302, .T. ) ;
#10362 = CARTESIAN_POINT ( 'NONE',  ( -94.99999999999997158, -209.9999999999999716, 90.00000000000000000 ) ) ;
#10363 = ORIENTED_EDGE ( 'NONE', *, *, #39164, .F. ) ;
#10364 = CARTESIAN_POINT ( 'NONE',  ( -92.34999999999999432, -208.4700217866474645, 82.19479166840095274 ) ) ;
#10365 = VERTEX_POINT ( 'NONE', #59765 ) ;
#10366 = CARTESIAN_POINT ( 'NONE',  ( -2.500000000000000000, 3.061616997868383141E-16, -0.3501037691048548561 ) ) ;
#10367 = ORIENTED_EDGE ( 'NONE', *, *, #66821, .T. ) ;
#10369 = CARTESIAN_POINT ( 'NONE',  ( -93.67500000000003979, 87.70503267997129626, 81.40104166840096411 ) ) ;
#10368 = CARTESIAN_POINT ( 'NONE',  ( 92.34999999999999432, 90.00000000000002842, 83.09437500173430635 ) ) ;
#10370 =( BOUNDED_CURVE ( )  B_SPLINE_CURVE ( 2, ( #11578, #27771, #11956, #28135, #363, #50698, #22891 ),
 .UNSPECIFIED., .F., .F. ) 
 B_SPLINE_CURVE_WITH_KNOTS ( ( 3, 2, 2, 3 ),
 ( 0.7708333333333328152, 0.7777777777777775681, 0.7847222222222222099, 0.7916666666666669627 ),
 .UNSPECIFIED. ) 
 CURVE ( )  GEOMETRIC_REPRESENTATION_ITEM ( )  RATIONAL_B_SPLINE_CURVE ( ( 1.000000000000010658, 0.8660254037844280495, 1.000000000000000000, 0.8660254037844387076, 1.000000000000000000, 0.8660254037844322683, 1.000000000000006439 ) ) 
 REPRESENTATION_ITEM ( '' )  );
#10371 = VERTEX_POINT ( 'NONE', #1550 ) ;
#10372 = CARTESIAN_POINT ( 'NONE',  ( 93.84685191531248449, 88.00268892867053694, 84.19239583420049655 ) ) ;
#10373 = CIRCLE ( 'NONE', #21198, 31.99999999999998934 ) ;
#10374 = CARTESIAN_POINT ( 'NONE',  ( -97.65000000000001990, 90.00000000000004263, 90.00000000000000000 ) ) ;
#10375 = CARTESIAN_POINT ( 'NONE',  ( 11.99999999999999822, -15.33399622253540606, 80.55351364060582853 ) ) ;
#10376 = LINE ( 'NONE', #22405, #14609 ) ;
#10377 = LINE ( 'NONE', #34799, #34220 ) ;
#10378 = CARTESIAN_POINT ( 'NONE',  ( 0.000000000000000000, 40.98264845739763018, -9.188173127306864529 ) ) ;
#10379 = ORIENTED_EDGE ( 'NONE', *, *, #55741, .F. ) ;
#10380 = CARTESIAN_POINT ( 'NONE',  ( 10.00000000000000000, 35.38097989696512968, 12.42422080174651100 ) ) ;
#10381 = DIRECTION ( 'NONE',  ( -0.000000000000000000, -0.9135454576426058626, -0.4067366430757889395 ) ) ;
#10382 = EDGE_CURVE ( 'NONE', #40438, #5952, #10636, .T. ) ;
#10383 = EDGE_CURVE ( 'NONE', #57918, #50963, #43193, .T. ) ;
#10384 = CARTESIAN_POINT ( 'NONE',  ( -18.12185313557660038, -104.9634299478706794, 5.500000000000000000 ) ) ;
#10385 = ORIENTED_EDGE ( 'NONE', *, *, #8056, .T. ) ;
#10386 = AXIS2_PLACEMENT_3D ( 'NONE', #57638, #51235, #68549 ) ;
#10387 = ORIENTED_EDGE ( 'NONE', *, *, #3403, .T. ) ;
#10388 = VECTOR ( 'NONE', #3274, 1000.000000000000000 ) ;
#10389 = DIRECTION ( 'NONE',  ( 0.000000000000000000, -0.8090169943749531134, 0.5877852522924653655 ) ) ;
#10390 = AXIS2_PLACEMENT_3D ( 'NONE', #71408, #31561, #71041 ) ;
#10391 = VECTOR ( 'NONE', #1109, 1000.000000000000000 ) ;
#10392 = CARTESIAN_POINT ( 'NONE',  ( -3.000000000000000000, 20.85821328998756385, -10.92862929874494959 ) ) ;
#10393 = DIRECTION ( 'NONE',  ( -0.000000000000000000, -0.3090169943749450088, 0.9510565162951543083 ) ) ;
#10394 = CARTESIAN_POINT ( 'NONE',  ( -94.99999999999997158, -212.6630814284392557, 81.70531250086715147 ) ) ;
#10395 = VERTEX_POINT ( 'NONE', #19525 ) ;
#10396 = CYLINDRICAL_SURFACE ( 'NONE', #45321, 2.649999999999985700 ) ;
#10397 = VERTEX_POINT ( 'NONE', #35355 ) ;
#10398 = DIRECTION ( 'NONE',  ( -1.000000000000000000, 0.000000000000000000, 0.000000000000000000 ) ) ;
#10399 = LINE ( 'NONE', #44247, #16730 ) ;
#10400 = MECHANICAL_DESIGN_GEOMETRIC_PRESENTATION_REPRESENTATION (  '', ( #28426 ), #23610 ) ;
#10401 = FACE_OUTER_BOUND ( 'NONE', #6888, .T. ) ;
#10402 = DIRECTION ( 'NONE',  ( -1.000000000000000000, 0.000000000000000000, 0.000000000000000000 ) ) ;
#10403 = CARTESIAN_POINT ( 'NONE',  ( 92.69370383062501162, -209.9999999999999716, 89.64281250086713726 ) ) ;
#10404 = LINE ( 'NONE', #67552, #48099 ) ;
#10405 = DIRECTION ( 'NONE',  ( -1.000000000000000000, 0.000000000000000000, 0.000000000000000000 ) ) ;
#10406 = DIRECTION ( 'NONE',  ( 0.000000000000000000, 0.000000000000000000, 1.000000000000000000 ) ) ;
#10407 = CARTESIAN_POINT ( 'NONE',  ( 0.000000000000000000, -17.80606268964516659, -33.00180498840066434 ) ) ;
#10408 = DIRECTION ( 'NONE',  ( 1.000000000000000000, 0.000000000000000000, 0.000000000000000000 ) ) ;
#10409 = CARTESIAN_POINT ( 'NONE',  ( 23.41451323550360186, -132.5004227906269989, 5.500000000000000000 ) ) ;
#10410 = CARTESIAN_POINT ( 'NONE',  ( 0.000000000000000000, 0.000000000000000000, 0.000000000000000000 ) ) ;
#10411 = DIRECTION ( 'NONE',  ( 0.000000000000000000, 0.7071067811865487940, -0.7071067811865462405 ) ) ;
#10412 = EDGE_LOOP ( 'NONE', ( #4564, #68328, #52431, #54737 ) ) ;
#10413 = CARTESIAN_POINT ( 'NONE',  ( -93.84685191531254134, 91.99731107132950569, 79.90614583420047268 ) ) ;
#10414 = CARTESIAN_POINT ( 'NONE',  ( 0.000000000000000000, 17.28742895386189105, -75.54627589209924565 ) ) ;
#10415 = ORIENTED_EDGE ( 'NONE', *, *, #54147, .T. ) ;
#10416 = CARTESIAN_POINT ( 'NONE',  ( -3.000000000000000000, 22.07842321921492612, -8.187992925817130896 ) ) ;
#10417 = CARTESIAN_POINT ( 'NONE',  ( 0.000000000000000000, 0.000000000000000000, -125.0000000000000000 ) ) ;
#10418 = AXIS2_PLACEMENT_3D ( 'NONE', #61623, #66882, #15370 ) ;
#10419 = DIRECTION ( 'NONE',  ( -1.000000000000000000, 0.000000000000000000, 0.000000000000000000 ) ) ;
#10420 = PRODUCT_RELATED_PRODUCT_CATEGORY ( 'part', '', ( #71551 ) ) ;
#10421 = EDGE_CURVE ( 'NONE', #13202, #60472, #55144, .T. ) ;
#10422 = VECTOR ( 'NONE', #36512, 1000.000000000000000 ) ;
#10423 = PLANE ( 'NONE',  #6964 ) ;
#10424 = CARTESIAN_POINT ( 'NONE',  ( 93.84685191531249870, -208.0026889286704943, 76.36072916753381890 ) ) ;
#10425 = VECTOR ( 'NONE', #26876, 1000.000000000000000 ) ;
#10426 = ADVANCED_FACE ( 'NONE', ( #41003 ), #16731, .F. ) ;
#10427 = ORIENTED_EDGE ( 'NONE', *, *, #39817, .T. ) ;
#10428 = VERTEX_POINT ( 'NONE', #63934 ) ;
#10429 = EDGE_CURVE ( 'NONE', #52144, #15980, #12773, .T. ) ;
#10430 = DIRECTION ( 'NONE',  ( -1.000000000000000000, 7.571539615859142926E-15, 2.592266024478009537E-14 ) ) ;
#10431 = VECTOR ( 'NONE', #72157, 1000.000000000000000 ) ;
#10432 = LINE ( 'NONE', #51774, #19547 ) ;
#10433 = DIRECTION ( 'NONE',  ( 0.08130631524010120681, -0.9966891607226784355, 0.000000000000000000 ) ) ;
#10434 = CARTESIAN_POINT ( 'NONE',  ( 11.99999999999999822, 65.59268652807210742, 36.72794159290264560 ) ) ;
#10435 = EDGE_CURVE ( 'NONE', #42455, #52827, #45522, .T. ) ;
#10436 = CARTESIAN_POINT ( 'NONE',  ( 96.32499999999998863, -207.7050326799711968, 86.61333333333332973 ) ) ;
#10437 = ORIENTED_EDGE ( 'NONE', *, *, #45452, .F. ) ;
#10438 = CARTESIAN_POINT ( 'NONE',  ( 10.00000000000000000, 0.000000000000000000, 0.000000000000000000 ) ) ;
#10439 = VERTEX_POINT ( 'NONE', #70646 ) ;
#10440 = ORIENTED_EDGE ( 'NONE', *, *, #42513, .F. ) ;
#10441 = DIRECTION ( 'NONE',  ( -1.000000000000000000, 0.000000000000000000, -0.000000000000000000 ) ) ;
#10442 = VECTOR ( 'NONE', #29191, 1000.000000000000000 ) ;
#10443 =( NAMED_UNIT ( * ) PLANE_ANGLE_UNIT ( ) SI_UNIT ( $, .RADIAN. ) );
#10444 = CYLINDRICAL_SURFACE ( 'NONE', #5351, 16.00000000000000000 ) ;
#10445 = VERTEX_POINT ( 'NONE', #2661 ) ;
#10446 = CARTESIAN_POINT ( 'NONE',  ( 0.000000000000000000, 16.61724383029390140, -20.69703378468903665 ) ) ;
#10447 = CARTESIAN_POINT ( 'NONE',  ( 93.67500000000001137, -207.7050326799711968, 81.08354166840096866 ) ) ;
#10448 = CARTESIAN_POINT ( 'NONE',  ( 96.32499999999997442, 92.29496732002878900, 82.80333333333332746 ) ) ;
#10449 = EDGE_CURVE ( 'NONE', #19930, #72643, #48108, .T. ) ;
#10450 = CIRCLE ( 'NONE', #8037, 52.50000000000002132 ) ;
#10451 = ORIENTED_EDGE ( 'NONE', *, *, #17094, .F. ) ;
#10452 = FACE_OUTER_BOUND ( 'NONE', #22399, .T. ) ;
#10453 = ORIENTED_EDGE ( 'NONE', *, *, #11978, .T. ) ;
#10454 = EDGE_CURVE ( 'NONE', #14986, #59860, #42110, .T. ) ;
#10455 = FACE_OUTER_BOUND ( 'NONE', #19687, .T. ) ;
#10456 = VERTEX_POINT ( 'NONE', #65046 ) ;
#10457 = CARTESIAN_POINT ( 'NONE',  ( 10.00000000000000000, 0.000000000000000000, 0.000000000000000000 ) ) ;
#10458 = CARTESIAN_POINT ( 'NONE',  ( -92.69370383062505425, 91.33154071421968467, 83.82197916753382572 ) ) ;
#10459 = CARTESIAN_POINT ( 'NONE',  ( 97.30629616937498838, 88.66845928578037217, 78.47739583420047893 ) ) ;
#10460 = VERTEX_POINT ( 'NONE', #71025 ) ;
#10461 = CARTESIAN_POINT ( 'NONE',  ( 0.000000000000000000, -58.39081064771787766, 50.95692526931307498 ) ) ;
#10462 = DIRECTION ( 'NONE',  ( 0.000000000000000000, 0.000000000000000000, 1.000000000000000000 ) ) ;
#10463 = LINE ( 'NONE', #62364, #55807 ) ;
#10464 = CARTESIAN_POINT ( 'NONE',  ( 0.000000000000000000, 15.33399622253600292, -80.55351364060572905 ) ) ;
#10465 = ORIENTED_EDGE ( 'NONE', *, *, #20489, .F. ) ;
#10466 = CARTESIAN_POINT ( 'NONE',  ( 0.000000000000000000, 75.11725578898472122, -2.956366410619845730 ) ) ;
#10467 = EDGE_CURVE ( 'NONE', #59483, #808, #61171, .T. ) ;
#10468 = CARTESIAN_POINT ( 'NONE',  ( -94.99999999999997158, -207.3369185715606307, 78.68906250086713783 ) ) ;
#10469 = VERTEX_POINT ( 'NONE', #9733 ) ;
#10470 = ORIENTED_EDGE ( 'NONE', *, *, #54756, .T. ) ;
#10471 = CARTESIAN_POINT ( 'NONE',  ( -3.000000000000002665, 0.000000000000000000, 20.64000000000000057 ) ) ;
#10472 = ORIENTED_EDGE ( 'NONE', *, *, #48624, .F. ) ;
#10473 = PLANE ( 'NONE',  #50361 ) ;
#10474 = DIRECTION ( 'NONE',  ( 0.000000000000000000, 0.000000000000000000, 1.000000000000000000 ) ) ;
#10475 = EDGE_LOOP ( 'NONE', ( #22628, #14674, #1878, #73540 ) ) ;
#10476 = CARTESIAN_POINT ( 'NONE',  ( -96.15314808468745866, -211.9973110713294489, 76.41364583420048007 ) ) ;
#10477 = ORIENTED_EDGE ( 'NONE', *, *, #51104, .F. ) ;
#10478 = CARTESIAN_POINT ( 'NONE',  ( 10.00000000000000000, 0.8828120875905820508, -37.48860685352290290 ) ) ;
#10479 = CARTESIAN_POINT ( 'NONE',  ( 5.000000000000002665, -81.90746397400386059, -3.894527615418773347 ) ) ;
#10480 = FACE_BOUND ( 'NONE', #35331, .T. ) ;
#10481 = CARTESIAN_POINT ( 'NONE',  ( 11.99999999999999822, -8.830959090342926032, 74.65491531819115778 ) ) ;
#10482 = AXIS2_PLACEMENT_3D ( 'NONE', #63554, #58269, #28953 ) ;
#10483 = CARTESIAN_POINT ( 'NONE',  ( 0.000000000000000000, -35.91791733033426226, -68.67312586195033930 ) ) ;
#10484 = CIRCLE ( 'NONE', #5676, 82.00000000000000000 ) ;
#10485 = CARTESIAN_POINT ( 'NONE',  ( 0.000000000000000000, 8.966570791701863996, -81.50828551894218776 ) ) ;
#10486 = CARTESIAN_POINT ( 'NONE',  ( 97.30629616937498838, 91.33154071421968467, 88.74322916753382628 ) ) ;
#10487 = VECTOR ( 'NONE', #23909, 1000.000000000000000 ) ;
#10488 = DIRECTION ( 'NONE',  ( -1.000000000000000000, 0.000000000000000000, -0.000000000000000000 ) ) ;
#10489 = CYLINDRICAL_SURFACE ( 'NONE', #28893, 3.299999999999969624 ) ;
#10490 = DIRECTION ( 'NONE',  ( -1.000000000000000000, -0.000000000000000000, -0.000000000000000000 ) ) ;
#10491 = CARTESIAN_POINT ( 'NONE',  ( 11.99999999999999822, 0.000000000000000000, 0.000000000000000000 ) ) ;
#10492 = CARTESIAN_POINT ( 'NONE',  ( 0.000000000000000000, 44.99326035066149387, -68.55367621811095091 ) ) ;
#10493 = FACE_OUTER_BOUND ( 'NONE', #12187, .T. ) ;
#10494 = CARTESIAN_POINT ( 'NONE',  ( 11.99999999999999822, 71.27951684758069462, -30.41916302227037150 ) ) ;
#10495 = CARTESIAN_POINT ( 'NONE',  ( 12.49999999999999645, 1.530808498934191127E-15, -43.79999999999998295 ) ) ;
#10496 = EDGE_CURVE ( 'NONE', #63285, #58109, #43230, .T. ) ;
#10497 = CARTESIAN_POINT ( 'NONE',  ( 0.000000000000000000, 26.01480285779837232, 70.53064760720326376 ) ) ;
#10498 = DIRECTION ( 'NONE',  ( -0.000000000000000000, -0.000000000000000000, 1.000000000000000000 ) ) ;
#10499 = CARTESIAN_POINT ( 'NONE',  ( 10.00000000000000000, 0.000000000000000000, 0.000000000000000000 ) ) ;
#10500 = VECTOR ( 'NONE', #69253, 1000.000000000000000 ) ;
#10501 = CARTESIAN_POINT ( 'NONE',  ( -97.64999999999994884, -211.5299782133524502, 83.70291666666668107 ) ) ;
#10502 = EDGE_CURVE ( 'NONE', #51690, #67688, #71926, .T. ) ;
#10504 = EDGE_CURVE ( 'NONE', #70995, #59464, #20372, .T. ) ;
#10503 = AXIS2_PLACEMENT_3D ( 'NONE', #64283, #7131, #2267 ) ;
#10505 = FACE_OUTER_BOUND ( 'NONE', #2383, .T. ) ;
#10506 = CARTESIAN_POINT ( 'NONE',  ( 0.000000000000000000, 0.000000000000000000, 0.000000000000000000 ) ) ;
#10507 = DIRECTION ( 'NONE',  ( -1.000000000000000000, 0.000000000000000000, 0.000000000000000000 ) ) ;
#10508 = CARTESIAN_POINT ( 'NONE',  ( 10.00000000000000000, 0.000000000000000000, 0.000000000000000000 ) ) ;
#10509 = ADVANCED_FACE ( 'NONE', ( #37208 ), #71757, .F. ) ;
#10510 = CARTESIAN_POINT ( 'NONE',  ( 0.000000000000000000, 25.88420570971438650, -27.13269053701069566 ) ) ;
#10511 = CARTESIAN_POINT ( 'NONE',  ( 97.30629616937498838, -208.6684592857803011, 88.90197916753382401 ) ) ;
#10512 = ORIENTED_EDGE ( 'NONE', *, *, #157, .F. ) ;
#10513 = ORIENTED_EDGE ( 'NONE', *, *, #44605, .F. ) ;
#10514 = FILL_AREA_STYLE_COLOUR ( '', #18810 ) ;
#10515 = ORIENTED_EDGE ( 'NONE', *, *, #38709, .T. ) ;
#10516 = LINE ( 'NONE', #17652, #50965 ) ;
#10517 = CARTESIAN_POINT ( 'NONE',  ( 93.84685191531249870, -208.0026889286704943, 78.10697916753380809 ) ) ;
#10518 = EDGE_CURVE ( 'NONE', #58524, #66160, #26647, .T. ) ;
#10519 = AXIS2_PLACEMENT_3D ( 'NONE', #53714, #2256, #48080 ) ;
#10520 = ORIENTED_EDGE ( 'NONE', *, *, #54756, .F. ) ;
#10521 = CARTESIAN_POINT ( 'NONE',  ( 92.69370383062501162, -209.9999999999999716, 81.54656250086715374 ) ) ;
#10522 = STYLED_ITEM ( 'NONE', ( #2124 ), #12416 ) ;
#10523 = ORIENTED_EDGE ( 'NONE', *, *, #34356, .F. ) ;
#10524 = DIRECTION ( 'NONE',  ( -0.000000000000000000, -0.000000000000000000, 1.000000000000000000 ) ) ;
#10525 = ORIENTED_EDGE ( 'NONE', *, *, #38648, .F. ) ;
#10526 = CARTESIAN_POINT ( 'NONE',  ( -92.69370383062504004, 90.00000000000004263, 74.87906250086714977 ) ) ;
#10527 = CIRCLE ( 'NONE', #23734, 31.99999999999999645 ) ;
#10528 = DIRECTION ( 'NONE',  ( -0.000000000000000000, -0.000000000000000000, 1.000000000000000000 ) ) ;
#10529 = AXIS2_PLACEMENT_3D ( 'NONE', #57585, #40654, #47038 ) ;
#10530 = ORIENTED_EDGE ( 'NONE', *, *, #948, .T. ) ;
#10531 = FACE_BOUND ( 'NONE', #73356, .T. ) ;
#10532 = EDGE_CURVE ( 'NONE', #5816, #49658, #33557, .T. ) ;
#10533 = ORIENTED_EDGE ( 'NONE', *, *, #3103, .T. ) ;
#10534 = DIRECTION ( 'NONE',  ( 0.000000000000000000, 0.000000000000000000, 1.000000000000000000 ) ) ;
#10535 = EDGE_CURVE ( 'NONE', #66338, #37865, #2291, .T. ) ;
#10536 = EDGE_LOOP ( 'NONE', ( #45213, #29736, #39322, #12549 ) ) ;
#10537 = CARTESIAN_POINT ( 'NONE',  ( 0.000000000000000000, 49.70050353004889132, 59.46389618801982380 ) ) ;
#10538 = EDGE_CURVE ( 'NONE', #17376, #46993, #66154, .T. ) ;
#10539 = ORIENTED_EDGE ( 'NONE', *, *, #60762, .T. ) ;
#10540 = ORIENTED_EDGE ( 'NONE', *, *, #40653, .T. ) ;
#10541 = ORIENTED_EDGE ( 'NONE', *, *, #58817, .T. ) ;
#10542 = CARTESIAN_POINT ( 'NONE',  ( 97.30629616937498838, -208.6684592857803011, 75.40822916753381833 ) ) ;
#10543 = ITEM_DEFINED_TRANSFORMATION ( 'NONE', 'NONE', #72385,  #43395 ) ;
#10544 = FACE_OUTER_BOUND ( 'NONE', #48101, .T. ) ;
#10545 = ORIENTED_EDGE ( 'NONE', *, *, #50756, .T. ) ;
#10546 = CIRCLE ( 'NONE', #34592, 16.00000000000000355 ) ;
#10547 = EDGE_LOOP ( 'NONE', ( #4813, #16224, #64213, #56670 ) ) ;
#10548 = AXIS2_PLACEMENT_3D ( 'NONE', #63110, #50682, #45812 ) ;
#10549 = VERTEX_POINT ( 'NONE', #61616 ) ;
#10550 = FACE_OUTER_BOUND ( 'NONE', #6466, .T. ) ;
#10551 = DIRECTION ( 'NONE',  ( 0.000000000000000000, -0.000000000000000000, -1.000000000000000000 ) ) ;
#10552 = AXIS2_PLACEMENT_3D ( 'NONE', #64903, #13383, #70145 ) ;
#10553 = VECTOR ( 'NONE', #37696, 1000.000000000000000 ) ;
#10554 = CARTESIAN_POINT ( 'NONE',  ( -97.30629616937501680, 91.33154071421968467, 76.41364583420049428 ) ) ;
#10555 = ORIENTED_EDGE ( 'NONE', *, *, #55706, .F. ) ;
#10556 = CARTESIAN_POINT ( 'NONE',  ( 97.64999999999997726, -208.4700217866474929, 89.73541666666663730 ) ) ;
#10557 = VECTOR ( 'NONE', #29363, 1000.000000000000000 ) ;
#10558 = EDGE_LOOP ( 'NONE', ( #58522, #5648, #21809, #44942 ) ) ;
#10559 = CARTESIAN_POINT ( 'NONE',  ( -94.99999999999997158, -207.3369185715606307, 85.67406250086715147 ) ) ;
#10560 = ORIENTED_EDGE ( 'NONE', *, *, #24718, .T. ) ;
#10561 = CARTESIAN_POINT ( 'NONE',  ( 1.332830945733272987, -5.003992386592898356, -0.8603634151101718919 ) ) ;
#10562 = DIRECTION ( 'NONE',  ( 0.000000000000000000, -0.1564344650402170744, -0.9876883405951399908 ) ) ;
#10563 = CARTESIAN_POINT ( 'NONE',  ( 11.59999999999999787, 1.420590287010929336E-15, -43.79999999999998295 ) ) ;
#10564 = CARTESIAN_POINT ( 'NONE',  ( -93.84685191531248449, -208.0026889286704943, 81.17614583420048291 ) ) ;
#10565 = CARTESIAN_POINT ( 'NONE',  ( 5.000000000000000000, 81.96053171279902472, 2.543863470248670211 ) ) ;
#10566 = DIRECTION ( 'NONE',  ( -1.000000000000000000, 0.000000000000000000, 0.000000000000000000 ) ) ;
#10567 = CARTESIAN_POINT ( 'NONE',  ( -97.64999999999996305, -209.9999999999999716, 79.20499999999999829 ) ) ;
#10568 = ORIENTED_EDGE ( 'NONE', *, *, #54671, .F. ) ;
#10569 = FACE_OUTER_BOUND ( 'NONE', #62660, .T. ) ;
#10570 = DIRECTION ( 'NONE',  ( -0.7950889364178781449, 0.6064928550163533050, 0.000000000000000000 ) ) ;
#10571 = CARTESIAN_POINT ( 'NONE',  ( -96.15314808468751551, 88.00268892867056536, 82.12864583420046927 ) ) ;
#10572 = CARTESIAN_POINT ( 'NONE',  ( 10.00000000000000000, 69.42325613327489009, -34.44570377933524696 ) ) ;
#10573 = DIRECTION ( 'NONE',  ( -1.000000000000000000, 0.000000000000000000, 0.000000000000000000 ) ) ;
#10574 =( BOUNDED_CURVE ( )  B_SPLINE_CURVE ( 2, ( #13747, #26518, #36687, #32145, #71251, #65278, #60746, #3251, #15235 ),
 .UNSPECIFIED., .F., .F. ) 
 B_SPLINE_CURVE_WITH_KNOTS ( ( 3, 2, 2, 2, 3 ),
 ( 0.6561861948910822084, 0.6632419608429419577, 0.6702977263838236777, 0.6773534919247052866, 0.6773535682752291898 ),
 .UNSPECIFIED. ) 
 CURVE ( )  GEOMETRIC_REPRESENTATION_ITEM ( )  RATIONAL_B_SPLINE_CURVE ( ( 1.000000000000000000, 0.8660254037844387076, 1.000000000000000000, 0.8660254037844387076, 1.000000000000000000, 0.8660254037844387076, 1.000000000000000000, 0.9999985502592815267, 0.9999971005499384002 ) ) 
 REPRESENTATION_ITEM ( '' )  );
#10575 = VECTOR ( 'NONE', #5114, 1000.000000000000000 ) ;
#10576 = ORIENTED_EDGE ( 'NONE', *, *, #13754, .F. ) ;
#10577 = FACE_BOUND ( 'NONE', #74153, .T. ) ;
#10578 = PRESENTATION_LAYER_ASSIGNMENT (  '', '', ( #61027 ) ) ;
#10579 = VECTOR ( 'NONE', #21684, 1000.000000000000114 ) ;
#10580 = EDGE_CURVE ( 'NONE', #56916, #62512, #37172, .T. ) ;
#10581 = DIRECTION ( 'NONE',  ( -0.2306669878475648139, -0.9730327541852491491, 0.000000000000000000 ) ) ;
#10582 = PLANE ( 'NONE',  #33410 ) ;
#10584 = VECTOR ( 'NONE', #65156, 1000.000000000000000 ) ;
#10583 = CARTESIAN_POINT ( 'NONE',  ( 0.000000000000000000, 0.000000000000000000, 52.00000000000002132 ) ) ;
#10585 = CARTESIAN_POINT ( 'NONE',  ( 97.64999999999999147, -209.9999999999999716, 85.87249999999998806 ) ) ;
#10586 = CARTESIAN_POINT ( 'NONE',  ( -92.35000000000003695, 90.00000000000004263, 87.14249999999999829 ) ) ;
#10587 = CARTESIAN_POINT ( 'NONE',  ( -96.15314808468747287, -208.0026889286704943, 78.90072916753382515 ) ) ;
#10588 = ADVANCED_FACE ( 'NONE', ( #8633 ), #14995, .F. ) ;
#10589 = EDGE_CURVE ( 'NONE', #67486, #60096, #21005, .T. ) ;
#10590 = DIRECTION ( 'NONE',  ( 0.000000000000000000, 0.4067366430757889950, -0.9135454576426058626 ) ) ;
#10591 = ORIENTED_EDGE ( 'NONE', *, *, #60851, .T. ) ;
#10592 = CARTESIAN_POINT ( 'NONE',  ( -17.50000000000000355, 0.000000000000000000, 20.00000000000000000 ) ) ;
#10593 = CARTESIAN_POINT ( 'NONE',  ( 2.746707903440850533E-12, -120.0000000000000000, -70.59999999999999432 ) ) ;
#10594 = EDGE_LOOP ( 'NONE', ( #10733, #29419, #4053, #40256 ) ) ;
#10595 = EDGE_CURVE ( 'NONE', #37081, #45592, #4485, .T. ) ;
#10596 = DIRECTION ( 'NONE',  ( 0.000000000000000000, -0.000000000000000000, 1.000000000000000000 ) ) ;
#10597 = AXIS2_PLACEMENT_3D ( 'NONE', #52393, #65175, #63701 ) ;
#10598 = DIRECTION ( 'NONE',  ( 0.000000000000000000, 0.000000000000000000, 1.000000000000000000 ) ) ;
#10599 = AXIS2_PLACEMENT_3D ( 'NONE', #54198, #71458, #52707 ) ;
#10600 = UNCERTAINTY_MEASURE_WITH_UNIT (LENGTH_MEASURE( 1.000000000000000082E-05 ), #795, 'distance_accuracy_value', 'NONE');
#10601 = AXIS2_PLACEMENT_3D ( 'NONE', #13781, #59665, #20550 ) ;
#10603 = DIRECTION ( 'NONE',  ( -1.000000000000000000, -0.000000000000000000, 0.000000000000000000 ) ) ;
#10602 = CIRCLE ( 'NONE', #59832, 32.00000000000000000 ) ;
#10604 = VERTEX_POINT ( 'NONE', #27382 ) ;
#10605 = AXIS2_PLACEMENT_3D ( 'NONE', #42875, #67560, #31572 ) ;
#10606 = DIRECTION ( 'NONE',  ( -1.000000000000000000, -0.000000000000000000, 0.000000000000000000 ) ) ;
#10607 = CARTESIAN_POINT ( 'NONE',  ( 0.000000000000000000, -30.00120703465222149, 22.64427369931158296 ) ) ;
#10608 = EDGE_LOOP ( 'NONE', ( #19099, #6850, #7873, #12565 ) ) ;
#10609 = AXIS2_PLACEMENT_3D ( 'NONE', #33431, #27422, #10139 ) ;
#10610 = CARTESIAN_POINT ( 'NONE',  ( 92.69370383062501162, -209.9999999999999716, 89.64281250086713726 ) ) ;
#10611 = CARTESIAN_POINT ( 'NONE',  ( -94.99999999999997158, -206.9400435732949575, 87.38062500173430180 ) ) ;
#10612 = EDGE_CURVE ( 'NONE', #48915, #1061, #73171, .T. ) ;
#10613 = ORIENTED_EDGE ( 'NONE', *, *, #48656, .T. ) ;
#10614 = CARTESIAN_POINT ( 'NONE',  ( 96.32499999999998863, -212.2949673200287179, 89.57666666666666799 ) ) ;
#10615 = ORIENTED_EDGE ( 'NONE', *, *, #10206, .F. ) ;
#10616 = CARTESIAN_POINT ( 'NONE',  ( 10.00000000000000000, -77.16300072079640415, -27.74655509720751567 ) ) ;
#10617 = VERTEX_POINT ( 'NONE', #14257 ) ;
#10618 = DIRECTION ( 'NONE',  ( 0.000000000000000000, 0.4539904997395477482, -0.8910065241883674547 ) ) ;
#10619 = ORIENTED_EDGE ( 'NONE', *, *, #45855, .F. ) ;
#10620 = VERTEX_POINT ( 'NONE', #60150 ) ;
#10621 = ORIENTED_EDGE ( 'NONE', *, *, #33242, .F. ) ;
#10622 = CARTESIAN_POINT ( 'NONE',  ( -10.00000000000000000, 0.000000000000000000, 0.000000000000000000 ) ) ;
#10623 = EDGE_CURVE ( 'NONE', #21187, #5866, #29968, .T. ) ;
#10624 = ORIENTED_EDGE ( 'NONE', *, *, #47521, .T. ) ;
#10625 = EDGE_CURVE ( 'NONE', #15472, #34053, #40775, .T. ) ;
#10626 = ORIENTED_EDGE ( 'NONE', *, *, #38642, .F. ) ;
#10627 = CARTESIAN_POINT ( 'NONE',  ( 96.15314808468748708, 91.99731107132950569, 76.25489583420049655 ) ) ;
#10628 = DIRECTION ( 'NONE',  ( 0.000000000000000000, -1.065814103640131346E-14, -1.000000000000000000 ) ) ;
#10629 = AXIS2_PLACEMENT_3D ( 'NONE', #29856, #24243, #51314 ) ;
#10630 = B_SPLINE_CURVE_WITH_KNOTS ( 'NONE', 3,
 ( #18246, #63760, #7706, #53201, #24992, #70107, #52447, #1740 ),
 .UNSPECIFIED., .F., .F.,
 ( 4, 2, 2, 4 ),
 ( 0.002921158011986710323, 0.003648658599403066614, 0.004376159186819422904, 0.005831160361652134617 ),
 .UNSPECIFIED. ) ;
#10631 = DIRECTION ( 'NONE',  ( -0.000000000000000000, -0.000000000000000000, -1.000000000000000000 ) ) ;
#10632 = VECTOR ( 'NONE', #29437, 1000.000000000000000 ) ;
#10633 = VERTEX_POINT ( 'NONE', #3376 ) ;
#10634 = AXIS2_PLACEMENT_3D ( 'NONE', #39544, #22248, #60725 ) ;
#10635 = VERTEX_POINT ( 'NONE', #9357 ) ;
#10636 = B_SPLINE_CURVE_WITH_KNOTS ( 'NONE', 3,
 ( #2287, #53745, #36817, #13522, #25540, #59033 ),
 .UNSPECIFIED., .F., .F.,
 ( 4, 2, 4 ),
 ( 0.000000000000000000, 0.0008269033587275365343, 0.001653806717455073069 ),
 .UNSPECIFIED. ) ;
#10637 = ORIENTED_EDGE ( 'NONE', *, *, #11530, .F. ) ;
#10638 = CARTESIAN_POINT ( 'NONE',  ( 93.84685191531248449, 88.00268892867053694, 88.47864583420047779 ) ) ;
#10639 = ORIENTED_EDGE ( 'NONE', *, *, #73894, .T. ) ;
#10640 = CARTESIAN_POINT ( 'NONE',  ( 92.69370383062501162, -208.6684592857803011, 83.87489583420047268 ) ) ;
#10641 = APPLICATION_PROTOCOL_DEFINITION ( 'draft international standard', 'automotive_design', 1998, #72439 ) ;
#10642 = DIRECTION ( 'NONE',  ( 0.000000000000000000, 0.1564344650402312298, -0.9876883405951375483 ) ) ;
#10643 = AXIS2_PLACEMENT_3D ( 'NONE', #42134, #70666, #2307 ) ;
#10644 = CARTESIAN_POINT ( 'NONE',  ( -97.65000000000001990, 90.00000000000004263, 78.01437500173430806 ) ) ;
#10645 = FACE_OUTER_BOUND ( 'NONE', #46091, .T. ) ;
#10646 = DIRECTION ( 'NONE',  ( 0.000000000000000000, 0.1564344650402244852, 0.9876883405951387696 ) ) ;
#10647 = DIRECTION ( 'NONE',  ( -1.000000000000000000, -0.000000000000000000, -0.000000000000000000 ) ) ;
#10648 = CARTESIAN_POINT ( 'NONE',  ( -93.84685191531248449, -208.0026889286704943, 89.43114583420047836 ) ) ;
#10649 = CARTESIAN_POINT ( 'NONE',  ( -97.30629616937501680, 88.66845928578038638, 84.77447916753381207 ) ) ;
#10650 = ORIENTED_EDGE ( 'NONE', *, *, #65218, .T. ) ;
#10652 = CARTESIAN_POINT ( 'NONE',  ( -96.15314808468751551, 88.00268892867056536, 84.66864583420047552 ) ) ;
#10651 = CARTESIAN_POINT ( 'NONE',  ( 94.99999999999998579, 87.33691857156068750, 86.62656250086715204 ) ) ;
#10653 = ORIENTED_EDGE ( 'NONE', *, *, #66791, .F. ) ;
#10654 = LINE ( 'NONE', #33580, #29831 ) ;
#10655 = DIRECTION ( 'NONE',  ( -1.000000000000000000, -0.000000000000000000, -0.000000000000000000 ) ) ;
#10656 = CARTESIAN_POINT ( 'NONE',  ( 12.49999999999999645, 0.000000000000000000, -175.0000000000000000 ) ) ;
#10657 = DIRECTION ( 'NONE',  ( 0.000000000000000000, 0.000000000000000000, 1.000000000000000000 ) ) ;
#10658 = CARTESIAN_POINT ( 'NONE',  ( 10.00000000000000000, 33.17418723428333749, -17.67226234102790272 ) ) ;
#10659 = VECTOR ( 'NONE', #2428, 1000.000000000000114 ) ;
#10660 = DIRECTION ( 'NONE',  ( -0.000000000000000000, -0.000000000000000000, 1.000000000000000000 ) ) ;
#10661 = CARTESIAN_POINT ( 'NONE',  ( 23.41451323550362318, -132.5004227906269989, -2.500000000000000000 ) ) ;
#10662 = CARTESIAN_POINT ( 'NONE',  ( 10.00000000000000000, 0.000000000000000000, 0.000000000000000000 ) ) ;
#10663 = ORIENTED_EDGE ( 'NONE', *, *, #63071, .F. ) ;
#10664 = CIRCLE ( 'NONE', #28694, 42.00000000000000000 ) ;
#10665 = ORIENTED_EDGE ( 'NONE', *, *, #15292, .T. ) ;
#10666 = AXIS2_PLACEMENT_3D ( 'NONE', #10156, #33080, #56021 ) ;
#10667 = AXIS2_PLACEMENT_3D ( 'NONE', #71891, #43718, #3872 ) ;
#10668 = CARTESIAN_POINT ( 'NONE',  ( -93.67500000000003979, 87.70503267997129626, 82.59166666666665435 ) ) ;
#10669 = DIRECTION ( 'NONE',  ( -1.000000000000000000, 0.000000000000000000, 0.000000000000000000 ) ) ;
#10670 = DIRECTION ( 'NONE',  ( 0.000000000000000000, 0.000000000000000000, 1.000000000000000000 ) ) ;
#10671 = DIRECTION ( 'NONE',  ( 1.000000000000000000, -9.814797785686868941E-17, 0.000000000000000000 ) ) ;
#10672 = DIRECTION ( 'NONE',  ( -1.000000000000000000, -0.000000000000000000, 0.000000000000000000 ) ) ;
#10673 = CARTESIAN_POINT ( 'NONE',  ( -12.50000000000000000, -107.5000000000000000, -40.00000000000000000 ) ) ;
#10674 = EDGE_CURVE ( 'NONE', #1522, #6553, #32279, .T. ) ;
#10675 = DIRECTION ( 'NONE',  ( -1.000000000000000000, -0.000000000000000000, -0.000000000000000000 ) ) ;
#10676 = CARTESIAN_POINT ( 'NONE',  ( 0.000000000000000000, -30.84782396557233142, 21.32104025579104345 ) ) ;
#10677 = ORIENTED_EDGE ( 'NONE', *, *, #29843, .T. ) ;
#10678 = CARTESIAN_POINT ( 'NONE',  ( -97.30629616937501680, 88.66845928578038638, 78.90072916753381094 ) ) ;
#10679 = ADVANCED_FACE ( 'NONE', ( #62376 ), #40168, .F. ) ;
#10680 = CARTESIAN_POINT ( 'NONE',  ( -94.99999999999997158, -209.9999999999999716, 73.40771935957695860 ) ) ;
#10681 = CARTESIAN_POINT ( 'NONE',  ( 11.99999999999999822, -69.42325613327466272, 34.44570377933573724 ) ) ;
#10682 = EDGE_CURVE ( 'NONE', #48259, #23577, #9526, .T. ) ;
#10683 = DIRECTION ( 'NONE',  ( 0.000000000000000000, 1.000000000000000000, 3.469446951953614978E-15 ) ) ;
#10684 = DIRECTION ( 'NONE',  ( -1.000000000000000000, 0.000000000000000000, -0.000000000000000000 ) ) ;
#10685 = CYLINDRICAL_SURFACE ( 'NONE', #6532, 1.000000000000000888 ) ;
#10686 = CARTESIAN_POINT ( 'NONE',  ( 12.00000000000000000, -25.60904388321925040, -6.976881207771165272 ) ) ;
#10687 = EDGE_CURVE ( 'NONE', #13012, #25707, #5978, .T. ) ;
#10688 = CIRCLE ( 'NONE', #14511, 12.74999999999999822 ) ;
#10689 = AXIS2_PLACEMENT_3D ( 'NONE', #31272, #36174, #71113 ) ;
#10690 = CARTESIAN_POINT ( 'NONE',  ( 94.99999999999998579, 87.33691857156068750, 80.43531250086715545 ) ) ;
#10691 = AXIS2_PLACEMENT_3D ( 'NONE', #71918, #8036, #53531 ) ;
#10692 = VECTOR ( 'NONE', #32309, 1000.000000000000000 ) ;
#10693 = CARTESIAN_POINT ( 'NONE',  ( -93.84685191531247028, -211.9973110713294489, 79.85322916753381151 ) ) ;
#10694 = FACE_OUTER_BOUND ( 'NONE', #46553, .T. ) ;
#10695 = ORIENTED_EDGE ( 'NONE', *, *, #68241, .F. ) ;
#10696 = EDGE_CURVE ( 'NONE', #25695, #11562, #11219, .T. ) ;
#10697 = CARTESIAN_POINT ( 'NONE',  ( -95.00000000000002842, 86.94004357329504273, 87.06312500173429214 ) ) ;
#10698 = DIRECTION ( 'NONE',  ( 0.000000000000000000, 0.000000000000000000, -1.000000000000000000 ) ) ;
#10699 = CYLINDRICAL_SURFACE ( 'NONE', #29312, 2.649999999999985700 ) ;
#10700 = AXIS2_PLACEMENT_3D ( 'NONE', #9013, #3768, #32672 ) ;
#10701 = AXIS2_PLACEMENT_3D ( 'NONE', #6727, #18366, #41673 ) ;
#10702 = CARTESIAN_POINT ( 'NONE',  ( -93.84685191531254134, 91.99731107132950569, 78.79489583420048859 ) ) ;
#10703 = CARTESIAN_POINT ( 'NONE',  ( 92.69370383062501162, -208.6684592857803011, 81.96989583420048575 ) ) ;
#10704 = ORIENTED_EDGE ( 'NONE', *, *, #30068, .T. ) ;
#10705 = CARTESIAN_POINT ( 'NONE',  ( 10.00000000000000000, 0.000000000000000000, 0.000000000000000000 ) ) ;
#10706 = ADVANCED_FACE ( 'NONE', ( #27769 ), #34512, .T. ) ;
#10707 = ORIENTED_EDGE ( 'NONE', *, *, #15452, .F. ) ;
#10708 = CARTESIAN_POINT ( 'NONE',  ( -23.97194136764370498, -131.3950000906648938, 5.500000000000000000 ) ) ;
#10709 = EDGE_CURVE ( 'NONE', #73310, #22617, #38346, .T. ) ;
#10710 = ORIENTED_EDGE ( 'NONE', *, *, #58545, .T. ) ;
#10711 = AXIS2_PLACEMENT_3D ( 'NONE', #15676, #32945, #55895 ) ;
#10712 = CIRCLE ( 'NONE', #7063, 31.99999999999998579 ) ;
#10713 = FACE_OUTER_BOUND ( 'NONE', #37868, .T. ) ;
#10714 = ADVANCED_FACE ( 'NONE', ( #51816 ), #56354, .T. ) ;
#10715 = AXIS2_PLACEMENT_3D ( 'NONE', #72543, #66197, #44371 ) ;
#10716 = AXIS2_PLACEMENT_3D ( 'NONE', #27289, #4029, #73158 ) ;
#10717 = ORIENTED_EDGE ( 'NONE', *, *, #22798, .F. ) ;
#10718 = ORIENTED_EDGE ( 'NONE', *, *, #50307, .F. ) ;
#10719 = AXIS2_PLACEMENT_3D ( 'NONE', #31879, #54823, #3348 ) ;
#10720 = ORIENTED_EDGE ( 'NONE', *, *, #64843, .F. ) ;
#10721 = VECTOR ( 'NONE', #36119, 1000.000000000000000 ) ;
#10722 = DIRECTION ( 'NONE',  ( 0.9781476007338069101, 2.546183866652752180E-17, 0.2079116908177528755 ) ) ;
#10723 = EDGE_CURVE ( 'NONE', #47502, #33969, #1853, .T. ) ;
#10724 = VERTEX_POINT ( 'NONE', #63478 ) ;
#10725 = DIRECTION ( 'NONE',  ( 0.000000000000000000, 0.000000000000000000, 1.000000000000000000 ) ) ;
#10726 = DIRECTION ( 'NONE',  ( -1.000000000000000000, 0.000000000000000000, 0.000000000000000000 ) ) ;
#10727 = CARTESIAN_POINT ( 'NONE',  ( 92.69370383062498320, 91.33154071421968467, 85.30364583420048064 ) ) ;
#10728 = CARTESIAN_POINT ( 'NONE',  ( 0.000000000000000000, -37.22597642581153821, -5.202137450156795850 ) ) ;
#10729 = CARTESIAN_POINT ( 'NONE',  ( 95.00000000000000000, -206.9400435732949575, 77.77624999999999034 ) ) ;
#10730 = ORIENTED_EDGE ( 'NONE', *, *, #56302, .T. ) ;
#10731 = ADVANCED_FACE ( 'NONE', ( #481 ), #23251, .F. ) ;
#10732 = VERTEX_POINT ( 'NONE', #17602 ) ;
#10733 = ORIENTED_EDGE ( 'NONE', *, *, #27237, .T. ) ;
#10734 = ORIENTED_EDGE ( 'NONE', *, *, #49989, .F. ) ;
#10735 = CARTESIAN_POINT ( 'NONE',  ( -10.00000000000000000, 0.000000000000000000, 0.000000000000000000 ) ) ;
#10736 = DIRECTION ( 'NONE',  ( -1.000000000000000000, -0.000000000000000000, -0.000000000000000000 ) ) ;
#10737 = DIRECTION ( 'NONE',  ( -1.000000000000000000, 0.000000000000000000, 0.000000000000000000 ) ) ;
#10738 = CYLINDRICAL_SURFACE ( 'NONE', #58232, 82.00000000000000000 ) ;
#10739 = DIRECTION ( 'NONE',  ( 0.000000000000000000, 0.000000000000000000, 1.000000000000000000 ) ) ;
#10740 = CARTESIAN_POINT ( 'NONE',  ( 11.99999999999999822, 0.000000000000000000, 0.000000000000000000 ) ) ;
#10741 = ORIENTED_EDGE ( 'NONE', *, *, #37441, .T. ) ;
#10742 = CARTESIAN_POINT ( 'NONE',  ( -93.67499999999998295, -207.7050326799711968, 81.61270833506763722 ) ) ;
#10743 = ORIENTED_EDGE ( 'NONE', *, *, #68856, .T. ) ;
#10744 = DIRECTION ( 'NONE',  ( 0.000000000000000000, 0.000000000000000000, 1.000000000000000000 ) ) ;
#10745 = VERTEX_POINT ( 'NONE', #40530 ) ;
#10747 = CARTESIAN_POINT ( 'NONE',  ( -93.67500000000003979, 92.29496732002878900, 80.34270833506762699 ) ) ;
#10746 = CARTESIAN_POINT ( 'NONE',  ( 92.34999999999999432, 88.47002178664753558, 81.87729166840097150 ) ) ;
#10748 = ORIENTED_EDGE ( 'NONE', *, *, #38950, .F. ) ;
#10749 = CARTESIAN_POINT ( 'NONE',  ( 94.99999999999998579, 92.66308142843935514, 84.56281250086716739 ) ) ;
#10750 = CARTESIAN_POINT ( 'NONE',  ( 97.64999999999987779, 91.52997821335259232, 83.38541666666667140 ) ) ;
#10751 = CYLINDRICAL_SURFACE ( 'NONE', #28284, 77.49899999999999523 ) ;
#10752 = AXIS2_PLACEMENT_3D ( 'NONE', #54068, #2963, #19831 ) ;
#10753 = DIRECTION ( 'NONE',  ( -0.000000000000000000, -0.000000000000000000, 1.000000000000000000 ) ) ;
#10754 = DIRECTION ( 'NONE',  ( -1.000000000000000000, -0.000000000000000000, 0.000000000000000000 ) ) ;
#10755 = CIRCLE ( 'NONE', #26354, 77.49899999999999523 ) ;
#10756 = CARTESIAN_POINT ( 'NONE',  ( 10.00000000000000000, 10.41901085202135668, -40.68715046381917944 ) ) ;
#10757 = ORIENTED_EDGE ( 'NONE', *, *, #34830, .F. ) ;
#10758 = CARTESIAN_POINT ( 'NONE',  ( -89.99999999999998579, -204.9999999999999716, 90.00000000000000000 ) ) ;
#10759 = CARTESIAN_POINT ( 'NONE',  ( -97.65000000000001990, 90.00000000000004263, 82.45937500173430124 ) ) ;
#10760 = DIRECTION ( 'NONE',  ( -0.1276937514489679404, -0.9918136447140103451, 0.000000000000000000 ) ) ;
#10761 = EDGE_LOOP ( 'NONE', ( #31247, #57768, #34294, #71749 ) ) ;
#10762 = VERTEX_POINT ( 'NONE', #5602 ) ;
#10763 = VECTOR ( 'NONE', #16437, 1000.000000000000000 ) ;
#10764 = DIRECTION ( 'NONE',  ( 0.000000000000000000, -0.5877852522924802425, 0.8090169943749422332 ) ) ;
#10765 = CARTESIAN_POINT ( 'NONE',  ( -10.00000000000000000, 0.000000000000000000, 0.000000000000000000 ) ) ;
#10766 = CARTESIAN_POINT ( 'NONE',  ( -0.0004442498525516064278, 0.001194404164626844313, -64.00000000000000000 ) ) ;
#10767 = CARTESIAN_POINT ( 'NONE',  ( -96.15314808468747287, -208.0026889286704943, 80.80572916753382628 ) ) ;
#10768 = VERTEX_POINT ( 'NONE', #11955 ) ;
#10769 = CARTESIAN_POINT ( 'NONE',  ( -92.69370383062504004, 90.00000000000004263, 87.42031250086714067 ) ) ;
#10770 = ORIENTED_EDGE ( 'NONE', *, *, #52710, .F. ) ;
#10771 = EDGE_CURVE ( 'NONE', #50470, #16727, #6339, .T. ) ;
#10772 = CARTESIAN_POINT ( 'NONE',  ( 0.000000000000000000, -56.15606465354917276, -59.75363087400133111 ) ) ;
#10773 = VECTOR ( 'NONE', #58443, 1000.000000000000000 ) ;
#10774 = AXIS2_PLACEMENT_3D ( 'NONE', #43133, #71672, #66067 ) ;
#10775 = FACE_BOUND ( 'NONE', #55298, .T. ) ;
#10776 = EDGE_CURVE ( 'NONE', #47891, #17447, #2390, .T. ) ;
#10777 = CARTESIAN_POINT ( 'NONE',  ( -0.0004442498525516064278, 0.001194404164626844313, -64.00000000000000000 ) ) ;
#10778 = CARTESIAN_POINT ( 'NONE',  ( 10.00000000000000000, -31.47745569255189224, 68.26794271651249346 ) ) ;
#10779 = DIRECTION ( 'NONE',  ( -1.000000000000000000, 0.000000000000000000, -0.000000000000000000 ) ) ;
#10780 = CARTESIAN_POINT ( 'NONE',  ( -24.50849501662245800, -109.8101191361138831, 5.500000000000000000 ) ) ;
#10781 = FACE_OUTER_BOUND ( 'NONE', #50587, .T. ) ;
#10782 = AXIS2_PLACEMENT_3D ( 'NONE', #44106, #21914, #9889 ) ;
#10783 = CARTESIAN_POINT ( 'NONE',  ( -93.67499999999998295, -207.7050326799711968, 76.53270833506762472 ) ) ;
#10784 = ADVANCED_FACE ( 'NONE', ( #21756 ), #67621, .F. ) ;
#10785 = AXIS2_PLACEMENT_3D ( 'NONE', #27330, #16068, #39374 ) ;
#10787 = ADVANCED_FACE ( 'NONE', ( #51070 ), #10473, .T. ) ;
#10786 = LINE ( 'NONE', #74304, #5235 ) ;
#10788 = LINE ( 'NONE', #27701, #53965 ) ;
#10789 = DIRECTION ( 'NONE',  ( 0.000000000000000000, -1.000000000000000000, -1.047444401652940007E-14 ) ) ;
#10790 = CARTESIAN_POINT ( 'NONE',  ( 10.00000000000000000, -2.956366410620109519, -75.11725578898472122 ) ) ;
#10791 = CARTESIAN_POINT ( 'NONE',  ( -70.53423027509626309, -217.0820393249940423, 5.500000000000000000 ) ) ;
#10792 = DIRECTION ( 'NONE',  ( -1.000000000000000000, -0.000000000000000000, 0.000000000000000000 ) ) ;
#10793 = ORIENTED_EDGE ( 'NONE', *, *, #33362, .T. ) ;
#10794 = DIRECTION ( 'NONE',  ( -1.000000000000000000, -0.000000000000000000, -0.000000000000000000 ) ) ;
#10795 = CARTESIAN_POINT ( 'NONE',  ( -97.30629616937501680, 90.00000000000004263, 78.84781250086714977 ) ) ;
#10796 = EDGE_CURVE ( 'NONE', #64719, #56201, #45075, .T. ) ;
#10797 = CARTESIAN_POINT ( 'NONE',  ( 92.69370383062501162, -208.6684592857803011, 88.95489583420048518 ) ) ;
#10798 = EDGE_LOOP ( 'NONE', ( #69527, #52040, #25731, #33109 ) ) ;
#10799 =( BOUNDED_CURVE ( )  B_SPLINE_CURVE ( 2, ( #40972, #7491, #24405, #47340, #53346, #1886, #29294 ),
 .UNSPECIFIED., .F., .F. ) 
 B_SPLINE_CURVE_WITH_KNOTS ( ( 3, 2, 2, 3 ),
 ( 0.1693384224419982043, 0.1763941385220585967, 0.1834499040629412603, 0.1905056698837211959 ),
 .UNSPECIFIED. ) 
 CURVE ( )  GEOMETRIC_REPRESENTATION_ITEM ( )  RATIONAL_B_SPLINE_CURVE ( ( 0.9999981216929038075, 0.8660263429445702599, 1.000000000000000000, 0.8660254037844387076, 1.000000000000000000, 0.8660254037844387076, 1.000000000000000000 ) ) 
 REPRESENTATION_ITEM ( '' )  );
#10800 = DIRECTION ( 'NONE',  ( 1.000000000000000000, 1.427937372958405461E-15, 7.962523111839130290E-16 ) ) ;
#10801 = CYLINDRICAL_SURFACE ( 'NONE', #53987, 2.649999999999985700 ) ;
#10802 = FACE_OUTER_BOUND ( 'NONE', #47240, .T. ) ;
#10803 = AXIS2_PLACEMENT_3D ( 'NONE', #21181, #38118, #27948 ) ;
#10804 = VECTOR ( 'NONE', #69672, 1000.000000000000000 ) ;
#10805 = CARTESIAN_POINT ( 'NONE',  ( -97.64999999999996305, -209.9999999999999716, 84.92000000000000171 ) ) ;
#10806 = ADVANCED_FACE ( 'NONE', ( #52540 ), #59302, .T. ) ;
#10807 = EDGE_CURVE ( 'NONE', #68344, #63923, #55191, .T. ) ;
#10808 = CARTESIAN_POINT ( 'NONE',  ( 97.30629616937498838, -211.3315407142195852, 76.73114583420048973 ) ) ;
#10809 = CIRCLE ( 'NONE', #45664, 12.75000000000265565 ) ;
#10810 = EDGE_LOOP ( 'NONE', ( #11437, #38814, #25531, #66559 ) ) ;
#10811 = ORIENTED_EDGE ( 'NONE', *, *, #70760, .T. ) ;
#10812 = CYLINDRICAL_SURFACE ( 'NONE', #56071, 12.49999999999999822 ) ;
#10813 = CARTESIAN_POINT ( 'NONE',  ( 10.00000000000000000, 36.13751322684449718, -21.40280677340333071 ) ) ;
#10814 = FACE_OUTER_BOUND ( 'NONE', #44075, .T. ) ;
#10815 =( BOUNDED_CURVE ( )  B_SPLINE_CURVE ( 2, ( #33813, #51101, #22542, #39838, #51470, #62790, #34546 ),
 .UNSPECIFIED., .F., .F. ) 
 B_SPLINE_CURVE_WITH_KNOTS ( ( 3, 2, 2, 3 ),
 ( 0.6458333333333334814, 0.6527777777777779011, 0.6597222222222223209, 0.6666666666666667407 ),
 .UNSPECIFIED. ) 
 CURVE ( )  GEOMETRIC_REPRESENTATION_ITEM ( )  RATIONAL_B_SPLINE_CURVE ( ( 0.9999999999999978906, 0.8660254037844408170, 1.000000000000000000, 0.8660254037844387076, 1.000000000000000000, 0.8660254037844365982, 1.000000000000002220 ) ) 
 REPRESENTATION_ITEM ( '' )  );
#10816 = FACE_OUTER_BOUND ( 'NONE', #10919, .T. ) ;
#10817 = LINE ( 'NONE', #33354, #68140 ) ;
#10818 = CARTESIAN_POINT ( 'NONE',  ( 92.35000000000000853, -209.9999999999999716, 88.09499999999999886 ) ) ;
#10819 = AXIS2_PLACEMENT_3D ( 'NONE', #11495, #73162, #16404 ) ;
#10820 = EDGE_LOOP ( 'NONE', ( #30215, #6031, #5671, #52031 ) ) ;
#10821 = CARTESIAN_POINT ( 'NONE',  ( 23.30762065077924916, -123.0008031590507329, 2.500000000000000000 ) ) ;
#10822 = EDGE_LOOP ( 'NONE', ( #60216, #35336 ) ) ;
#10823 = AXIS2_PLACEMENT_3D ( 'NONE', #16050, #44258, #4418 ) ;
#10824 = ORIENTED_EDGE ( 'NONE', *, *, #55503, .T. ) ;
#10825 = DIRECTION ( 'NONE',  ( -0.000000000000000000, -0.000000000000000000, 1.000000000000000000 ) ) ;
#10826 = VECTOR ( 'NONE', #47909, 1000.000000000000227 ) ;
#10827 = VECTOR ( 'NONE', #49671, 1000.000000000000000 ) ;
#10828 = DIRECTION ( 'NONE',  ( -0.000000000000000000, -0.000000000000000000, 1.000000000000000000 ) ) ;
#10829 = VECTOR ( 'NONE', #40317, 1000.000000000000000 ) ;
#10830 = ORIENTED_EDGE ( 'NONE', *, *, #12119, .F. ) ;
#10831 = CARTESIAN_POINT ( 'NONE',  ( 92.34999999999999432, 90.00000000000002842, 87.45999999999999375 ) ) ;
#10832 = CARTESIAN_POINT ( 'NONE',  ( 95.00000000000000000, -206.9400435732949575, 77.22062500173429100 ) ) ;
#10833 = CARTESIAN_POINT ( 'NONE',  ( 96.32499999999997442, 92.29496732002878900, 80.89833333333332632 ) ) ;
#10834 = ORIENTED_EDGE ( 'NONE', *, *, #869, .T. ) ;
#10835 = CARTESIAN_POINT ( 'NONE',  ( 97.64999999999999147, -210.0000000024471092, 75.15687493081163950 ) ) ;
#10836 = ORIENTED_EDGE ( 'NONE', *, *, #17676, .T. ) ;
#10837 = DIRECTION ( 'NONE',  ( 0.000000000000000000, -0.6494480483301904306, 0.7604059656000252687 ) ) ;
#10838 = VERTEX_POINT ( 'NONE', #1466 ) ;
#10839 = CARTESIAN_POINT ( 'NONE',  ( 5.000000000000002665, -44.99326035066006568, -68.55367621811190304 ) ) ;
#10840 = CARTESIAN_POINT ( 'NONE',  ( -93.84685191531254134, 91.99731107132950569, 83.23989583420049598 ) ) ;
#10841 = CARTESIAN_POINT ( 'NONE',  ( 96.15314808468748708, 88.00268892867053694, 77.78947916753381264 ) ) ;
#10842 = VERTEX_POINT ( 'NONE', #19438 ) ;
#10843 = DIRECTION ( 'NONE',  ( -1.000000000000000000, 0.000000000000000000, 0.000000000000000000 ) ) ;
#10844 = CARTESIAN_POINT ( 'NONE',  ( -10.00000000000000000, 0.000000000000000000, 0.000000000000000000 ) ) ;
#10845 = CARTESIAN_POINT ( 'NONE',  ( -3.000000000000000000, 24.81905959214275370, -9.408202855044498492 ) ) ;
#10846 = LINE ( 'NONE', #15739, #43292 ) ;
#10847 = ORIENTED_EDGE ( 'NONE', *, *, #57358, .F. ) ;
#10848 = CARTESIAN_POINT ( 'NONE',  ( 11.99999999999999822, 55.20638768913760686, 51.02545421589343988 ) ) ;
#10849 = CARTESIAN_POINT ( 'NONE',  ( -92.69370383062498320, -211.3315407142195852, 75.93739583420047268 ) ) ;
#10850 = ORIENTED_EDGE ( 'NONE', *, *, #62916, .F. ) ;
#10851 = ORIENTED_EDGE ( 'NONE', *, *, #35256, .F. ) ;
#10852 = DIRECTION ( 'NONE',  ( -1.000000000000000000, -0.000000000000000000, -0.000000000000000000 ) ) ;
#10853 = ORIENTED_EDGE ( 'NONE', *, *, #59107, .T. ) ;
#10854 = CARTESIAN_POINT ( 'NONE',  ( -17.26469406256017791, -140.1601175325492648, -5.500000000000000000 ) ) ;
#10855 = PLANE ( 'NONE',  #47289 ) ;
#10856 = ORIENTED_EDGE ( 'NONE', *, *, #66390, .F. ) ;
#10857 = CARTESIAN_POINT ( 'NONE',  ( -97.30629616937497417, -211.3315407142195852, 76.36072916753381890 ) ) ;
#10858 = ORIENTED_EDGE ( 'NONE', *, *, #23662, .F. ) ;
#10859 = CARTESIAN_POINT ( 'NONE',  ( -96.32500000000001705, 87.70503267997129626, 76.77083333333332860 ) ) ;
#10860 = CARTESIAN_POINT ( 'NONE',  ( 0.000000000000000000, -59.03961581697432592, 46.53671651293927880 ) ) ;
#10861 = CARTESIAN_POINT ( 'NONE',  ( 5.000000000000000000, 38.55633173627010279, 16.65560815589424593 ) ) ;
#10862 = DIRECTION ( 'NONE',  ( -1.000000000000000000, -0.000000000000000000, -0.000000000000000000 ) ) ;
#10863 = VECTOR ( 'NONE', #29995, 1000.000000000000000 ) ;
#10864 = EDGE_CURVE ( 'NONE', #46178, #38445, #11995, .T. ) ;
#10865 = PLANE ( 'NONE',  #13969 ) ;
#10866 = CIRCLE ( 'NONE', #62504, 42.00000000000000000 ) ;
#10867 = UNCERTAINTY_MEASURE_WITH_UNIT (LENGTH_MEASURE( 1.000000000000000082E-05 ), #72476, 'distance_accuracy_value', 'NONE');
#10868 = EDGE_CURVE ( 'NONE', #2983, #63033, #24355, .T. ) ;
#10869 = CARTESIAN_POINT ( 'NONE',  ( 10.00000000000000000, 0.000000000000000000, 0.000000000000000000 ) ) ;
#10871 = CARTESIAN_POINT ( 'NONE',  ( 96.15314808468748708, 88.00268892867053694, 84.77447916753381207 ) ) ;
#10870 = VECTOR ( 'NONE', #71669, 1000.000000000000000 ) ;
#10872 = LINE ( 'NONE', #50336, #43623 ) ;
#10873 = CARTESIAN_POINT ( 'NONE',  ( 23.49916127795269460, -121.5130826919798039, 5.500000000000000000 ) ) ;
#10874 = DIRECTION ( 'NONE',  ( 0.000000000000000000, 0.000000000000000000, -1.000000000000000000 ) ) ;
#10875 = CARTESIAN_POINT ( 'NONE',  ( 10.00000000000000000, 0.000000000000000000, 0.000000000000000000 ) ) ;
#10877 = EDGE_CURVE ( 'NONE', #31156, #56792, #7176, .T. ) ;
#10876 = DIRECTION ( 'NONE',  ( -1.000000000000000000, -0.000000000000000000, -0.000000000000000000 ) ) ;
#10878 = CARTESIAN_POINT ( 'NONE',  ( 96.32499999999998863, -212.2949673200287179, 87.75104166840095843 ) ) ;
#10879 = CARTESIAN_POINT ( 'NONE',  ( 96.32499999999998863, 87.70503267997126784, 77.51166666666665606 ) ) ;
#10880 = DIRECTION ( 'NONE',  ( 0.000000000000000000, 0.000000000000000000, 1.000000000000000000 ) ) ;
#10881 = EDGE_CURVE ( 'NONE', #42731, #67963, #23992, .T. ) ;
#10882 = DIRECTION ( 'NONE',  ( -1.000000000000000000, 0.000000000000000000, 0.000000000000000000 ) ) ;
#10883 = AXIS2_PLACEMENT_3D ( 'NONE', #70759, #8365, #13622 ) ;
#10884 = DIRECTION ( 'NONE',  ( 0.000000000000000000, 0.8526401643540897357, 0.5224985647159527957 ) ) ;
#10885 = CARTESIAN_POINT ( 'NONE',  ( -93.84685191531254134, 91.99731107132950569, 88.16114583420046813 ) ) ;
#10886 = AXIS2_PLACEMENT_3D ( 'NONE', #22212, #52260, #51521 ) ;
#10887 = CARTESIAN_POINT ( 'NONE',  ( -15.70044424985387188, 0.001194404164747221980, -74.99999999999958789 ) ) ;
#10888 = CARTESIAN_POINT ( 'NONE',  ( -94.99999999999997158, -206.9400435732949575, 84.76125000000000398 ) ) ;
#10889 = AXIS2_PLACEMENT_3D ( 'NONE', #31315, #37716, #42246 ) ;
#10890 = EDGE_CURVE ( 'NONE', #16321, #22970, #67214, .T. ) ;
#10891 = PLANE ( 'NONE',  #9261 ) ;
#10892 = ADVANCED_FACE ( 'NONE', ( #42388 ), #2199, .F. ) ;
#10893 = ORIENTED_EDGE ( 'NONE', *, *, #27823, .T. ) ;
#10894 = CARTESIAN_POINT ( 'NONE',  ( -3.000000000000000000, -3.948201729842038432, -23.21447184625298021 ) ) ;
#10895 = CARTESIAN_POINT ( 'NONE',  ( -10.43921258969510824, -98.89258801967538659, -5.500000000000000000 ) ) ;
#10896 = DIRECTION ( 'NONE',  ( -1.000000000000000000, 0.000000000000000000, -0.000000000000000000 ) ) ;
#10897 = FACE_OUTER_BOUND ( 'NONE', #37920, .T. ) ;
#10898 = EDGE_CURVE ( 'NONE', #45130, #6635, #2444, .T. ) ;
#10899 = EDGE_CURVE ( 'NONE', #45508, #55684, #25207, .T. ) ;
#10900 = CARTESIAN_POINT ( 'NONE',  ( 96.15314808468748708, -208.0026889286704943, 86.41489583420049314 ) ) ;
#10901 = ORIENTED_EDGE ( 'NONE', *, *, #51599, .T. ) ;
#10902 = ORIENTED_EDGE ( 'NONE', *, *, #6247, .T. ) ;
#10903 = CARTESIAN_POINT ( 'NONE',  ( -12.50000000000000000, -132.5000000000000000, 40.00000000000000000 ) ) ;
#10904 = ORIENTED_EDGE ( 'NONE', *, *, #64352, .F. ) ;
#10905 = CYLINDRICAL_SURFACE ( 'NONE', #29323, 16.00000000000000000 ) ;
#10906 = CARTESIAN_POINT ( 'NONE',  ( 97.30629616937498838, -211.3315407142195852, 77.84239583420047381 ) ) ;
#10907 = ORIENTED_EDGE ( 'NONE', *, *, #25227, .T. ) ;
#10908 = CARTESIAN_POINT ( 'NONE',  ( 95.00000000000000000, -207.3369185715606307, 84.56281250086716739 ) ) ;
#10909 = ORIENTED_EDGE ( 'NONE', *, *, #14453, .T. ) ;
#10910 = DIRECTION ( 'NONE',  ( -1.000000000000000000, -0.000000000000000000, -0.000000000000000000 ) ) ;
#10911 = ORIENTED_EDGE ( 'NONE', *, *, #27499, .T. ) ;
#10912 = CIRCLE ( 'NONE', #64966, 77.49900000000000944 ) ;
#10913 = ORIENTED_EDGE ( 'NONE', *, *, #71633, .F. ) ;
#10914 = FILL_AREA_STYLE_COLOUR ( '', #46488 ) ;
#10915 = CYLINDRICAL_SURFACE ( 'NONE', #66463, 35.50000000000000711 ) ;
#10916 = VERTEX_POINT ( 'NONE', #69834 ) ;
#10917 = CARTESIAN_POINT ( 'NONE',  ( 97.65000000000000568, -211.5299782133524218, 77.00895833506763211 ) ) ;
#10918 = CARTESIAN_POINT ( 'NONE',  ( 92.35000000000000853, -209.9999999999999716, 86.90437500173429441 ) ) ;
#10919 = EDGE_LOOP ( 'NONE', ( #67892, #22869, #74067, #71018 ) ) ;
#10920 = DIRECTION ( 'NONE',  ( -1.000000000000000000, 0.000000000000000000, 0.000000000000000000 ) ) ;
#10921 = ORIENTED_EDGE ( 'NONE', *, *, #48707, .T. ) ;
#10922 = DIRECTION ( 'NONE',  ( -1.000000000000000000, -0.000000000000000000, -0.000000000000000000 ) ) ;
#10923 = VERTEX_POINT ( 'NONE', #8161 ) ;
#10924 = ORIENTED_EDGE ( 'NONE', *, *, #11540, .F. ) ;
#10925 = VERTEX_POINT ( 'NONE', #63851 ) ;
#10926 = CARTESIAN_POINT ( 'NONE',  ( 93.84685191531249870, -208.0026889286704943, 76.20197916753380696 ) ) ;
#10927 = CIRCLE ( 'NONE', #52952, 12.50000000000000000 ) ;
#10928 = CARTESIAN_POINT ( 'NONE',  ( 11.99999999999999822, 74.65374052328648702, 8.840884882375350529 ) ) ;
#10929 = VERTEX_POINT ( 'NONE', #1099 ) ;
#10930 = VECTOR ( 'NONE', #54480, 999.9999999999998863 ) ;
#10931 = ORIENTED_EDGE ( 'NONE', *, *, #52692, .T. ) ;
#10933 = EDGE_CURVE ( 'NONE', #62989, #70987, #9588, .T. ) ;
#10932 = ORIENTED_EDGE ( 'NONE', *, *, #51071, .T. ) ;
#10934 = CARTESIAN_POINT ( 'NONE',  ( 0.000000000000000000, -14.67089635893764665, 73.72996012237435082 ) ) ;
#10935 = AXIS2_PLACEMENT_3D ( 'NONE', #28163, #11600, #11247 ) ;
#10936 =( BOUNDED_CURVE ( )  B_SPLINE_CURVE ( 2, ( #41168, #64106, #53184, #1720, #24607, #47546, #20660 ),
 .UNSPECIFIED., .F., .F. ) 
 B_SPLINE_CURVE_WITH_KNOTS ( ( 3, 2, 2, 3 ),
 ( 0.7916666666666669627, 0.7986111111111114935, 0.8055555555555558023, 0.8125000000000002220 ),
 .UNSPECIFIED. ) 
 CURVE ( )  GEOMETRIC_REPRESENTATION_ITEM ( )  RATIONAL_B_SPLINE_CURVE ( ( 0.9999999999999935607, 0.8660254037844451469, 1.000000000000000000, 0.8660254037844387076, 1.000000000000000000, 0.8660254037844343777, 1.000000000000004219 ) ) 
 REPRESENTATION_ITEM ( '' )  );
#10937 = LINE ( 'NONE', #44038, #65922 ) ;
#10938 = ADVANCED_FACE ( 'NONE', ( #23614 ), #13792, .T. ) ;
#10939 = CARTESIAN_POINT ( 'NONE',  ( -92.69370383062502583, 88.66845928578038638, 76.73114583420048973 ) ) ;
#10940 = EDGE_LOOP ( 'NONE', ( #44216, #2007, #60032, #65884 ) ) ;
#10941 = CARTESIAN_POINT ( 'NONE',  ( 93.84685191531248449, 91.99731107132950569, 75.56697916753381605 ) ) ;
#10942 = EDGE_CURVE ( 'NONE', #18969, #852, #51863, .T. ) ;
#10943 = ORIENTED_EDGE ( 'NONE', *, *, #22515, .F. ) ;
#10944 = DIRECTION ( 'NONE',  ( -1.000000000000000000, 0.000000000000000000, 0.000000000000000000 ) ) ;
#10945 = CARTESIAN_POINT ( 'NONE',  ( -93.84685191531247028, -211.9973110713294489, 87.31447916753380412 ) ) ;
#10946 = ORIENTED_EDGE ( 'NONE', *, *, #71800, .F. ) ;
#10947 = LINE ( 'NONE', #44794, #19380 ) ;
#10948 = DIRECTION ( 'NONE',  ( 1.000000000000000000, -0.000000000000000000, 0.000000000000000000 ) ) ;
#10949 = CARTESIAN_POINT ( 'NONE',  ( -22.53294031248082163, -134.0273518838794757, 5.500000000000000000 ) ) ;
#10950 = CARTESIAN_POINT ( 'NONE',  ( -94.99999999999997158, -212.6630814284392557, 80.91156250086714863 ) ) ;
#10951 = EDGE_CURVE ( 'NONE', #70963, #66932, #46920, .T. ) ;
#10952 = CARTESIAN_POINT ( 'NONE',  ( 15.00000000000000000, 5.835314593368777558, 22.81335362449846471 ) ) ;
#10953 = FACE_OUTER_BOUND ( 'NONE', #41158, .T. ) ;
#10954 = EDGE_CURVE ( 'NONE', #779, #27461, #27614, .T. ) ;
#10955 = CARTESIAN_POINT ( 'NONE',  ( 0.000000000000000000, -37.16516213103273714, -4.992566952385376844 ) ) ;
#10956 = CARTESIAN_POINT ( 'NONE',  ( 0.000000000000000000, 75.11764819372149304, -2.946379043146603482 ) ) ;
#10957 = CARTESIAN_POINT ( 'NONE',  ( -97.47814808468746151, -209.9999999999999716, 89.90078125043358170 ) ) ;
#10958 = CARTESIAN_POINT ( 'NONE',  ( -96.15314808468752972, 91.99731107132950569, 82.55197916753380127 ) ) ;
#10959 = CARTESIAN_POINT ( 'NONE',  ( 10.00000000000000000, -35.95386929396264009, 10.96151621346475658 ) ) ;
#10960 = DIRECTION ( 'NONE',  ( 0.000000000000000000, 0.000000000000000000, -1.000000000000000000 ) ) ;
#10961 = ADVANCED_FACE ( 'NONE', ( #29983 ), #47288, .T. ) ;
#10962 = VERTEX_POINT ( 'NONE', #14544 ) ;
#10963 = CARTESIAN_POINT ( 'NONE',  ( -92.34999999999999432, -208.4700217866474645, 80.28979166840095161 ) ) ;
#10964 = VECTOR ( 'NONE', #71979, 1000.000000000000000 ) ;
#10965 = VECTOR ( 'NONE', #53193, 1000.000000000000114 ) ;
#10966 = AXIS2_PLACEMENT_3D ( 'NONE', #38325, #66891, #19270 ) ;
#10967 = CARTESIAN_POINT ( 'NONE',  ( 95.00000000000000000, -206.9400435732949575, 89.28562500173430294 ) ) ;
#10968 = LINE ( 'NONE', #27505, #29752 ) ;
#10969 = CARTESIAN_POINT ( 'NONE',  ( 10.00000000000000000, 59.03961581697399907, 46.53671651293969802 ) ) ;
#10970 = DIRECTION ( 'NONE',  ( -1.000000000000000000, 0.000000000000000000, 0.000000000000000000 ) ) ;
#10971 = DIRECTION ( 'NONE',  ( 1.000000000000000000, 0.000000000000000000, 0.000000000000000000 ) ) ;
#10972 = CARTESIAN_POINT ( 'NONE',  ( -94.99999999999997158, -212.6630814284392557, 81.07031250086716057 ) ) ;
#10973 = ADVANCED_FACE ( 'NONE', ( #9651 ), #26563, .F. ) ;
#10974 = CYLINDRICAL_SURFACE ( 'NONE', #26048, 32.00000000000000000 ) ;
#10975 = ADVANCED_FACE ( 'NONE', ( #60427 ), #61533, .T. ) ;
#10976 =( REPRESENTATION_RELATIONSHIP ('NONE','NONE', #31117, #50888 ) REPRESENTATION_RELATIONSHIP_WITH_TRANSFORMATION ( #4560 )SHAPE_REPRESENTATION_RELATIONSHIP( ) );
#10977 = ORIENTED_EDGE ( 'NONE', *, *, #18160, .F. ) ;
#10978 = FACE_OUTER_BOUND ( 'NONE', #11581, .T. ) ;
#10979 = CARTESIAN_POINT ( 'NONE',  ( -95.00000000000002842, 93.05995642670504253, 88.57124999999999204 ) ) ;
#10980 = CARTESIAN_POINT ( 'NONE',  ( 10.00000000000000000, 22.64427369931169309, 30.00120703465213623 ) ) ;
#10981 = PLANE ( 'NONE',  #19707 ) ;
#10982 = DIRECTION ( 'NONE',  ( 0.000000000000000000, -0.3090169943749549453, 0.9510565162951511997 ) ) ;
#10983 = VECTOR ( 'NONE', #16681, 1000.000000000000000 ) ;
#10984 = VECTOR ( 'NONE', #42386, 1000.000000000000000 ) ;
#10985 = CIRCLE ( 'NONE', #42237, 31.99999999999999289 ) ;
#10986 = DIRECTION ( 'NONE',  ( -1.000000000000000000, 0.000000000000000000, 0.000000000000000000 ) ) ;
#10987 = ORIENTED_EDGE ( 'NONE', *, *, #26795, .T. ) ;
#10988 = CARTESIAN_POINT ( 'NONE',  ( -2.981742216678212820, 0.000000000000000000, 0.000000000000000000 ) ) ;
#10989 = CARTESIAN_POINT ( 'NONE',  ( 10.00000000000000000, -15.48615015657555816, -39.04073710021360455 ) ) ;
#10990 = ORIENTED_EDGE ( 'NONE', *, *, #4705, .T. ) ;
#10991 = CARTESIAN_POINT ( 'NONE',  ( 92.69370383062501162, -211.3315407142195852, 87.15572916753380639 ) ) ;
#10992 = LINE ( 'NONE', #857, #38270 ) ;
#10993 = EDGE_LOOP ( 'NONE', ( #32548, #7806, #13311, #71495 ) ) ;
#10994 = DIRECTION ( 'NONE',  ( 1.000000000000000000, 0.000000000000000000, 0.000000000000000000 ) ) ;
#10995 = ORIENTED_EDGE ( 'NONE', *, *, #34092, .F. ) ;
#10996 = PLANE ( 'NONE',  #14198 ) ;
#10997 = ORIENTED_EDGE ( 'NONE', *, *, #37550, .T. ) ;
#10998 = CARTESIAN_POINT ( 'NONE',  ( -94.99999999999997158, -209.9999999999999716, 90.00000000000000000 ) ) ;
#10999 = ORIENTED_EDGE ( 'NONE', *, *, #30469, .T. ) ;
#11000 = ORIENTED_EDGE ( 'NONE', *, *, #27220, .T. ) ;
#11001 = VERTEX_POINT ( 'NONE', #31088 ) ;
#11002 = FACE_OUTER_BOUND ( 'NONE', #72293, .T. ) ;
#11003 = EDGE_CURVE ( 'NONE', #72303, #50389, #51598, .T. ) ;
#11004 = ORIENTED_EDGE ( 'NONE', *, *, #40605, .T. ) ;
#11005 = PRODUCT ( 'Shift Fork Lever Arm', 'Shift Fork Lever Arm', '', ( #62921 ) ) ;
#11006 = VERTEX_POINT ( 'NONE', #15668 ) ;
#11007 = CARTESIAN_POINT ( 'NONE',  ( 94.99999999999998579, 86.94004357329500010, 86.98374999999998636 ) ) ;
#11008 = CARTESIAN_POINT ( 'NONE',  ( 94.99999999999998579, 90.00000000000002842, 90.00000000000000000 ) ) ;
#11009 = DIRECTION ( 'NONE',  ( -1.000000000000000000, -1.427937372958405461E-15, -7.962523111839130290E-16 ) ) ;
#11010 = VERTEX_POINT ( 'NONE', #37495 ) ;
#11011 = ORIENTED_EDGE ( 'NONE', *, *, #35130, .T. ) ;
#11012 = AXIS2_PLACEMENT_3D ( 'NONE', #89, #62848, #68838 ) ;
#11013 = ORIENTED_EDGE ( 'NONE', *, *, #52015, .T. ) ;
#11014 = CARTESIAN_POINT ( 'NONE',  ( 93.84685191531248449, 91.99731107132950569, 85.09197916753380753 ) ) ;
#11015 = ORIENTED_EDGE ( 'NONE', *, *, #56100, .T. ) ;
#11016 = CARTESIAN_POINT ( 'NONE',  ( 93.84685191531249870, -208.0026889286704943, 85.72697916753379843 ) ) ;
#11017 =( NAMED_UNIT ( * ) SI_UNIT ( $, .STERADIAN. ) SOLID_ANGLE_UNIT ( ) );
#11018 = CARTESIAN_POINT ( 'NONE',  ( 10.00000000000000000, 76.66974797899852945, -11.30684508768257679 ) ) ;
#11020 = CARTESIAN_POINT ( 'NONE',  ( 0.000000000000000000, 0.000000000000000000, 0.000000000000000000 ) ) ;
#11019 = VECTOR ( 'NONE', #15479, 1000.000000000000000 ) ;
#11021 = LINE ( 'NONE', #39599, #567 ) ;
#11022 = DIRECTION ( 'NONE',  ( 0.000000000000000000, 0.000000000000000000, 1.000000000000000000 ) ) ;
#11023 = EDGE_CURVE ( 'NONE', #8327, #42112, #8910, .T. ) ;
#11024 = DIRECTION ( 'NONE',  ( 0.000000000000000000, 0.000000000000000000, -1.000000000000000000 ) ) ;
#11025 = CARTESIAN_POINT ( 'NONE',  ( 92.34999999999999432, 90.00000000000002842, 84.99937500173429328 ) ) ;
#11026 = CARTESIAN_POINT ( 'NONE',  ( -92.69370383062498320, -209.9999999999999716, 86.78531250086714977 ) ) ;
#11027 = ADVANCED_FACE ( 'NONE', ( #67164 ), #4034, .T. ) ;
#11028 = CARTESIAN_POINT ( 'NONE',  ( -92.69370383062504004, 90.00000000000004263, 86.30906250086715659 ) ) ;
#11029 = CIRCLE ( 'NONE', #18269, 3.299999999999997158 ) ;
#11030 = ORIENTED_EDGE ( 'NONE', *, *, #1604, .T. ) ;
#11032 = CARTESIAN_POINT ( 'NONE',  ( -92.69370383062504004, 90.00000000000004263, 84.24531250086714351 ) ) ;
#11031 = CARTESIAN_POINT ( 'NONE',  ( 97.30629616937498838, 90.00000000000002842, 82.97531250086714749 ) ) ;
#11033 = VECTOR ( 'NONE', #27652, 1000.000000000000000 ) ;
#11034 =( BOUNDED_CURVE ( )  B_SPLINE_CURVE ( 2, ( #8066, #18966, #37400, #19341, #19710, #41916, #65227, #71203, #60332 ),
 .UNSPECIFIED., .F., .F. ) 
 B_SPLINE_CURVE_WITH_KNOTS ( ( 3, 2, 2, 2, 3 ),
 ( 0.8043570860654229993, 0.8043572716605899009, 0.8114130372014723980, 0.8184688027423547840, 0.8255245790564498254 ),
 .UNSPECIFIED. ) 
 CURVE ( )  GEOMETRIC_REPRESENTATION_ITEM ( )  RATIONAL_B_SPLINE_CURVE ( ( 0.9999929520380603787, 0.9999964759263327840, 1.000000000000000000, 0.8660254037844387076, 1.000000000000000000, 0.8660254037844387076, 1.000000000000000000, 0.8660254037844387076, 1.000000000000000000 ) ) 
 REPRESENTATION_ITEM ( '' )  );
#11035 = VERTEX_POINT ( 'NONE', #49127 ) ;
#11036 = DIRECTION ( 'NONE',  ( -1.000000000000000000, 0.000000000000000000, 0.000000000000000000 ) ) ;
#11037 = DIRECTION ( 'NONE',  ( 1.000000000000000000, 0.000000000000000000, 0.000000000000000000 ) ) ;
#11038 = CARTESIAN_POINT ( 'NONE',  ( -31.74999999999995737, 0.000000000000000000, 0.000000000000000000 ) ) ;
#11039 = CARTESIAN_POINT ( 'NONE',  ( 95.00000000000000000, -206.9400435732949575, 85.39624999999998067 ) ) ;
#11040 = CARTESIAN_POINT ( 'NONE',  ( -94.99999999999997158, -207.3369185715606307, 88.21406250086712930 ) ) ;
#11041 = CARTESIAN_POINT ( 'NONE',  ( 0.000000000000000000, -16.65972982744877484, -80.28980883073775487 ) ) ;
#11042 = ADVANCED_FACE ( 'NONE', ( #48756 ), #49857, .T. ) ;
#11043 = ADVANCED_FACE ( 'NONE', ( #31824 ), #28799, .T. ) ;
#11044 = FACE_OUTER_BOUND ( 'NONE', #62351, .T. ) ;
#11045 = DIRECTION ( 'NONE',  ( -1.000000000000000000, 0.000000000000000000, 0.000000000000000000 ) ) ;
#11046 = VECTOR ( 'NONE', #21328, 1000.000000000000000 ) ;
#11047 = DIRECTION ( 'NONE',  ( -0.000000000000000000, -0.000000000000000000, 1.000000000000000000 ) ) ;
#11048 = ORIENTED_EDGE ( 'NONE', *, *, #24894, .T. ) ;
#11049 = VECTOR ( 'NONE', #14898, 1000.000000000000000 ) ;
#11050 = ORIENTED_EDGE ( 'NONE', *, *, #64960, .F. ) ;
#11051 = VECTOR ( 'NONE', #16335, 1000.000000000000227 ) ;
#11052 = CARTESIAN_POINT ( 'NONE',  ( -97.65000000000001990, 90.00000000000004263, 78.57000000000000739 ) ) ;
#11053 = DIRECTION ( 'NONE',  ( 1.000000000000000000, 0.000000000000000000, 0.000000000000000000 ) ) ;
#11054 = CARTESIAN_POINT ( 'NONE',  ( 95.00000000000000000, -213.0599564267049857, 75.63312500173429953 ) ) ;
#11055 = CARTESIAN_POINT ( 'NONE',  ( -97.64999999999996305, -209.9999999999999716, 76.74437500173429783 ) ) ;
#11056 = DIRECTION ( 'NONE',  ( 1.000000000000000000, 0.000000000000000000, 0.000000000000000000 ) ) ;
#11057 = FACE_BOUND ( 'NONE', #29187, .T. ) ;
#11058 = EDGE_CURVE ( 'NONE', #54680, #37666, #33, .T. ) ;
#11059 = VERTEX_POINT ( 'NONE', #44236 ) ;
#11060 = CARTESIAN_POINT ( 'NONE',  ( -96.15314808468751551, 88.00268892867056536, 77.04864583420047097 ) ) ;
#11061 = DIRECTION ( 'NONE',  ( 1.000000000000000000, 0.000000000000000000, 0.000000000000000000 ) ) ;
#11062 = CARTESIAN_POINT ( 'NONE',  ( 0.000000000000000000, 23.50000000000000000, -1.500000000000001332 ) ) ;
#11063 = CARTESIAN_POINT ( 'NONE',  ( -12.50000000000000000, -132.5000000000000000, -2.500000000000000000 ) ) ;
#11064 = CARTESIAN_POINT ( 'NONE',  ( 10.00000000000000000, 16.45098606841126454, 33.79645857604518966 ) ) ;
#11065 = CARTESIAN_POINT ( 'NONE',  ( 10.00000000000000000, -36.72794159290288718, 65.59268652807197952 ) ) ;
#11066 = CARTESIAN_POINT ( 'NONE',  ( 10.00000000000000000, 0.000000000000000000, 0.000000000000000000 ) ) ;
#11067 =( NAMED_UNIT ( * ) SI_UNIT ( $, .STERADIAN. ) SOLID_ANGLE_UNIT ( ) );
#11068 = EDGE_CURVE ( 'NONE', #54488, #43660, #66435, .T. ) ;
#11069 = EDGE_CURVE ( 'NONE', #6695, #34982, #20563, .T. ) ;
#11070 = CARTESIAN_POINT ( 'NONE',  ( 97.30629616937498838, 88.66845928578035796, 75.46114583420049371 ) ) ;
#11071 = CARTESIAN_POINT ( 'NONE',  ( -94.99999999999997158, -207.3369185715606307, 80.75281250086716511 ) ) ;
#11072 = LINE ( 'NONE', #39648, #50635 ) ;
#11073 = ORIENTED_EDGE ( 'NONE', *, *, #66153, .F. ) ;
#11074 = CARTESIAN_POINT ( 'NONE',  ( 10.00000000000000000, 0.000000000000000000, 0.000000000000000000 ) ) ;
#11075 = AXIS2_PLACEMENT_3D ( 'NONE', #44330, #73625, #54860 ) ;
#11076 = DIRECTION ( 'NONE',  ( -1.000000000000000000, 0.000000000000000000, -0.000000000000000000 ) ) ;
#11077 = CARTESIAN_POINT ( 'NONE',  ( 10.00000000000000000, -0.6853352020787742971, -37.58145647212455032 ) ) ;
#11078 = CIRCLE ( 'NONE', #53092, 31.99999999999998579 ) ;
#11079 = CARTESIAN_POINT ( 'NONE',  ( -97.30629616937501680, 90.00000000000004263, 77.10156250086714635 ) ) ;
#11080 = CARTESIAN_POINT ( 'NONE',  ( 93.84685191531249870, -208.0026889286704943, 78.74197916753381321 ) ) ;
#11081 = VERTEX_POINT ( 'NONE', #48386 ) ;
#11082 = CIRCLE ( 'NONE', #5143, 77.49900000000000944 ) ;
#11083 = DIRECTION ( 'NONE',  ( 0.000000000000000000, 0.5877852522924684742, 0.8090169943749506709 ) ) ;
#11084 = ORIENTED_EDGE ( 'NONE', *, *, #38618, .T. ) ;
#11085 = CYLINDRICAL_SURFACE ( 'NONE', #32726, 31.99999999999999289 ) ;
#11086 = VERTEX_POINT ( 'NONE', #71301 ) ;
#11087 = DIRECTION ( 'NONE',  ( 0.000000000000000000, 0.000000000000000000, 1.000000000000000000 ) ) ;
#11088 = AXIS2_PLACEMENT_3D ( 'NONE', #22394, #45342, #68266 ) ;
#11089 = ORIENTED_EDGE ( 'NONE', *, *, #32143, .T. ) ;
#11090 = ORIENTED_EDGE ( 'NONE', *, *, #61010, .F. ) ;
#11091 = ORIENTED_EDGE ( 'NONE', *, *, #10174, .T. ) ;
#11092 = CARTESIAN_POINT ( 'NONE',  ( 97.30629616937498838, -210.9303121318039871, 74.84209103131397001 ) ) ;
#11093 = ORIENTED_EDGE ( 'NONE', *, *, #32817, .F. ) ;
#11094 = FACE_OUTER_BOUND ( 'NONE', #35940, .T. ) ;
#11095 = ADVANCED_FACE ( 'NONE', ( #65690 ), #2931, .T. ) ;
#11096 = CARTESIAN_POINT ( 'NONE',  ( -95.62844927801778283, 87.44368763736515859, 74.98613922222766348 ) ) ;
#11097 = CARTESIAN_POINT ( 'NONE',  ( 97.30629616937498838, 91.33154071421968467, 83.82197916753382572 ) ) ;
#11098 = FACE_OUTER_BOUND ( 'NONE', #2751, .T. ) ;
#11099 = CARTESIAN_POINT ( 'NONE',  ( 97.64999999999997726, -211.5299782133524502, 79.46958333333333258 ) ) ;
#11100 = ORIENTED_EDGE ( 'NONE', *, *, #19825, .T. ) ;
#11101 = ORIENTED_EDGE ( 'NONE', *, *, #11197, .F. ) ;
#11102 = VERTEX_POINT ( 'NONE', #60791 ) ;
#11103 = ORIENTED_EDGE ( 'NONE', *, *, #38528, .T. ) ;
#11104 = CARTESIAN_POINT ( 'NONE',  ( -19.27444613274700913, -101.8135840178490668, -2.500000000000000000 ) ) ;
#11105 = ADVANCED_FACE ( 'NONE', ( #60070 ), #8546, .F. ) ;
#11106 = DIRECTION ( 'NONE',  ( 2.603472992746261562E-14, 2.546204323184492723E-14, -1.000000000000000000 ) ) ;
#11107 = CARTESIAN_POINT ( 'NONE',  ( 95.00000000000000000, -209.9999999999999716, 90.00000000000000000 ) ) ;
#11108 = CYLINDRICAL_SURFACE ( 'NONE', #49797, 31.99999999999999289 ) ;
#11109 = EDGE_CURVE ( 'NONE', #47680, #34322, #20176, .T. ) ;
#11110 = DIRECTION ( 'NONE',  ( 1.000000000000000000, 0.000000000000000000, 0.000000000000000000 ) ) ;
#11111 = DIRECTION ( 'NONE',  ( 0.000000000000000000, 0.000000000000000000, -1.000000000000000000 ) ) ;
#11112 = ORIENTED_EDGE ( 'NONE', *, *, #18676, .F. ) ;
#11113 = CARTESIAN_POINT ( 'NONE',  ( -93.67499999999998295, -207.7050326799711968, 80.97770833506763211 ) ) ;
#11114 = ORIENTED_EDGE ( 'NONE', *, *, #46678, .T. ) ;
#11115 = DIRECTION ( 'NONE',  ( -1.000000000000000000, 0.000000000000000000, 0.000000000000000000 ) ) ;
#11116 = ORIENTED_EDGE ( 'NONE', *, *, #73085, .F. ) ;
#11118 = CARTESIAN_POINT ( 'NONE',  ( -93.67500000000003979, 92.29496732002878900, 80.97770833506763211 ) ) ;
#11117 = CARTESIAN_POINT ( 'NONE',  ( 92.34999999999999432, 88.47002178664753558, 79.33729166840096525 ) ) ;
#11119 = VERTEX_POINT ( 'NONE', #43873 ) ;
#11120 = CARTESIAN_POINT ( 'NONE',  ( 94.99999999999998579, 87.33691857156068750, 84.88031250086714863 ) ) ;
#11121 = LINE ( 'NONE', #27667, #50196 ) ;
#11122 = DIRECTION ( 'NONE',  ( 0.000000000000000000, 0.3090169943749412340, 0.9510565162951556406 ) ) ;
#11123 = DIRECTION ( 'NONE',  ( 1.000000000000000000, 0.000000000000000000, 0.000000000000000000 ) ) ;
#11124 = DIRECTION ( 'NONE',  ( -1.000000000000000000, 0.000000000000000000, -0.000000000000000000 ) ) ;
#11125 = ADVANCED_FACE ( 'NONE', ( #66075 ), #5883, .F. ) ;
#11126 = PRESENTATION_LAYER_ASSIGNMENT (  '', '', ( #1561 ) ) ;
#11127 = CARTESIAN_POINT ( 'NONE',  ( 100.0010000000000190, -115.9999999999999716, 39.99999999999996447 ) ) ;
#11128 = ORIENTED_EDGE ( 'NONE', *, *, #35867, .T. ) ;
#11129 = FACE_OUTER_BOUND ( 'NONE', #67867, .T. ) ;
#11130 = LINE ( 'NONE', #57005, #26532 ) ;
#11131 = DIRECTION ( 'NONE',  ( -0.000000000000000000, -0.000000000000000000, 1.000000000000000000 ) ) ;
#11132 = EDGE_LOOP ( 'NONE', ( #64907, #43086, #70338, #28440 ) ) ;
#11133 = VECTOR ( 'NONE', #3185, 1000.000000000000000 ) ;
#11134 = EDGE_LOOP ( 'NONE', ( #64151, #70431, #68226, #34572 ) ) ;
#11135 = CARTESIAN_POINT ( 'NONE',  ( 0.000000000000000000, 0.000000000000000000, 20.00000000000000000 ) ) ;
#11136 = CIRCLE ( 'NONE', #37535, 77.49900000000000944 ) ;
#11137 = CARTESIAN_POINT ( 'NONE',  ( 10.00000000000000000, 30.00120703465205452, 22.64427369931179967 ) ) ;
#11138 = ADVANCED_FACE ( 'NONE', ( #274 ), #34063, .T. ) ;
#11139 = DIRECTION ( 'NONE',  ( 0.000000000000000000, 0.000000000000000000, 1.000000000000000000 ) ) ;
#11140 = CARTESIAN_POINT ( 'NONE',  ( 11.99999999999999822, 0.000000000000000000, 0.000000000000000000 ) ) ;
#11141 = CIRCLE ( 'NONE', #21970, 17.30399999999999849 ) ;
#11142 = CARTESIAN_POINT ( 'NONE',  ( -93.84685191531248449, -208.0026889286704943, 80.06489583420048461 ) ) ;
#11143 = ORIENTED_EDGE ( 'NONE', *, *, #36952, .T. ) ;
#11144 = ADVANCED_FACE ( 'NONE', ( #33692 ), #69026, .F. ) ;
#11145 = ORIENTED_EDGE ( 'NONE', *, *, #7164, .F. ) ;
#11146 = CARTESIAN_POINT ( 'NONE',  ( -95.00000000000002842, 90.00000000000004263, 90.00000000000000000 ) ) ;
#11147 = VECTOR ( 'NONE', #23083, 1000.000000000000000 ) ;
#11148 = EDGE_CURVE ( 'NONE', #63122, #19859, #1260, .T. ) ;
#11149 = CIRCLE ( 'NONE', #17102, 15.39727592608509177 ) ;
#11150 = CARTESIAN_POINT ( 'NONE',  ( -95.62844927796862748, -212.5563123626481001, 74.98613922222868666 ) ) ;
#11151 = CARTESIAN_POINT ( 'NONE',  ( 0.000000000000000000, 0.000000000000000000, 0.000000000000000000 ) ) ;
#11152 = DIRECTION ( 'NONE',  ( 0.000000000000000000, 0.000000000000000000, 1.000000000000000000 ) ) ;
#11153 = CARTESIAN_POINT ( 'NONE',  ( 1.560000000000000053, 0.000000000000000000, 2.999999999999998668 ) ) ;
#11154 = CARTESIAN_POINT ( 'NONE',  ( 0.000000000000000000, -37.16516213103273714, -4.992566952385376844 ) ) ;
#11155 = CARTESIAN_POINT ( 'NONE',  ( 5.000000000000000000, -56.15606465355001120, 59.75363087400055662 ) ) ;
#11156 = CARTESIAN_POINT ( 'NONE',  ( 0.000000000000000000, 36.73666225445988687, -65.58780272294035285 ) ) ;
#11157 = DIRECTION ( 'NONE',  ( 0.000000000000000000, -0.8090169943749531134, 0.5877852522924653655 ) ) ;
#11158 = CARTESIAN_POINT ( 'NONE',  ( 26.49955575014914189, 0.001194404164634644498, -64.99999999999930367 ) ) ;
#11159 = EDGE_CURVE ( 'NONE', #12862, #42731, #45742, .T. ) ;
#11160 = CARTESIAN_POINT ( 'NONE',  ( 97.30629616937498838, 90.00000000000002842, 86.94406250086716170 ) ) ;
#11161 = CARTESIAN_POINT ( 'NONE',  ( -92.69370383062498320, -208.6684592857803295, 88.90197916753382401 ) ) ;
#11162 = LINE ( 'NONE', #62691, #14571 ) ;
#11163 = EDGE_LOOP ( 'NONE', ( #23026, #35625, #48356, #2067 ) ) ;
#11164 = CYLINDRICAL_SURFACE ( 'NONE', #62893, 82.00000000000000000 ) ;
#11165 = CARTESIAN_POINT ( 'NONE',  ( -95.00000000000002842, 92.66308142843932671, 79.32406250086714294 ) ) ;
#11166 = DIRECTION ( 'NONE',  ( 0.000000000000000000, -0.8090169943749422332, -0.5877852522924803536 ) ) ;
#11167 = VERTEX_POINT ( 'NONE', #4398 ) ;
#11168 = DIRECTION ( 'NONE',  ( 0.000000000000000000, 0.000000000000000000, 1.000000000000000000 ) ) ;
#11169 = CARTESIAN_POINT ( 'NONE',  ( 96.32499999999998863, 87.70503267997126784, 83.22666666666665947 ) ) ;
#11170 = DIRECTION ( 'NONE',  ( 1.000000000000000000, -0.000000000000000000, -0.000000000000000000 ) ) ;
#11171 = AXIS2_PLACEMENT_3D ( 'NONE', #38846, #74160, #27173 ) ;
#11172 = FACE_BOUND ( 'NONE', #47297, .T. ) ;
#11173 = CARTESIAN_POINT ( 'NONE',  ( 96.15314808468748708, -208.0026889286704943, 75.61989583420049144 ) ) ;
#11174 = ORIENTED_EDGE ( 'NONE', *, *, #32592, .F. ) ;
#11175 = EDGE_LOOP ( 'NONE', ( #43372, #22746, #15529, #54203 ) ) ;
#11176 = CARTESIAN_POINT ( 'NONE',  ( 10.00000000000000000, 35.53030884539084866, 12.26510123303271982 ) ) ;
#11177 = FACE_OUTER_BOUND ( 'NONE', #63192, .T. ) ;
#11178 = CARTESIAN_POINT ( 'NONE',  ( 100.0010000000000900, 64.99999999999997158, -290.0000000000000568 ) ) ;
#11179 = CARTESIAN_POINT ( 'NONE',  ( -0.0004442498512760095037, 0.001194404164628348752, -49.00000000000000000 ) ) ;
#11180 = CIRCLE ( 'NONE', #23216, 42.00000000000000000 ) ;
#11181 = CARTESIAN_POINT ( 'NONE',  ( -3.000000000000000000, 16.61724383029361718, 20.69703378468926402 ) ) ;
#11182 = CARTESIAN_POINT ( 'NONE',  ( 92.35000000000002274, -211.5299782133524502, 89.41791666666667027 ) ) ;
#11183 = EDGE_CURVE ( 'NONE', #42834, #2120, #27682, .T. ) ;
#11184 = EDGE_LOOP ( 'NONE', ( #63193, #6323, #8830, #38578 ) ) ;
#11185 = ORIENTED_EDGE ( 'NONE', *, *, #39817, .F. ) ;
#11186 = EDGE_CURVE ( 'NONE', #12067, #48989, #39588, .T. ) ;
#11187 = DIRECTION ( 'NONE',  ( 0.000000000000000000, 1.000000000000000000, -1.224646799147353207E-16 ) ) ;
#11188 = ORIENTED_EDGE ( 'NONE', *, *, #28444, .T. ) ;
#11189 = AXIS2_PLACEMENT_3D ( 'NONE', #62771, #50710, #51086 ) ;
#11190 = ORIENTED_EDGE ( 'NONE', *, *, #42465, .T. ) ;
#11191 = DIRECTION ( 'NONE',  ( -0.7071067811865336949, 0.000000000000000000, 0.7071067811865613395 ) ) ;
#11192 = CIRCLE ( 'NONE', #2802, 37.49900000000000944 ) ;
#11193 = EDGE_CURVE ( 'NONE', #45315, #63075, #13174, .T. ) ;
#11194 = CARTESIAN_POINT ( 'NONE',  ( 10.00000000000000000, 0.000000000000000000, 0.000000000000000000 ) ) ;
#11195 = DIRECTION ( 'NONE',  ( 2.628368902995164490E-16, 1.000000000000000000, 0.000000000000000000 ) ) ;
#11196 = CARTESIAN_POINT ( 'NONE',  ( 96.32499999999998863, -212.2949673200287179, 77.59104166840097605 ) ) ;
#11197 = EDGE_CURVE ( 'NONE', #34299, #3022, #50985, .T. ) ;
#11198 = CARTESIAN_POINT ( 'NONE',  ( 97.64999999999997726, 88.47002178664753558, 83.27958333333333485 ) ) ;
#11199 = VERTEX_POINT ( 'NONE', #40443 ) ;
#11200 = CARTESIAN_POINT ( 'NONE',  ( 94.99999999999998579, 90.00000000000002842, 90.00000000000000000 ) ) ;
#11201 = VERTEX_POINT ( 'NONE', #21667 ) ;
#11202 = DIRECTION ( 'NONE',  ( 0.000000000000000000, 0.3826834323650905589, -0.9238795325112864054 ) ) ;
#11203 = VERTEX_POINT ( 'NONE', #28794 ) ;
#11204 = CARTESIAN_POINT ( 'NONE',  ( -96.32500000000001705, 87.70503267997129626, 88.91520833506763211 ) ) ;
#11205 = EDGE_CURVE ( 'NONE', #66879, #42446, #55250, .T. ) ;
#11206 = CARTESIAN_POINT ( 'NONE',  ( -97.30629616937501680, 90.00000000000004263, 81.54656250086715374 ) ) ;
#11207 = CARTESIAN_POINT ( 'NONE',  ( 92.69370383062498320, 91.33154071421968467, 76.88989583420047325 ) ) ;
#11208 = VERTEX_POINT ( 'NONE', #39720 ) ;
#11209 = CARTESIAN_POINT ( 'NONE',  ( 10.00000000000000000, 0.000000000000000000, 0.000000000000000000 ) ) ;
#11210 = FACE_OUTER_BOUND ( 'NONE', #16939, .T. ) ;
#11211 = DIRECTION ( 'NONE',  ( 0.000000000000000000, 0.000000000000000000, 1.000000000000000000 ) ) ;
#11212 = CARTESIAN_POINT ( 'NONE',  ( -97.64999999999996305, -209.9999999999999716, 77.93499999999998806 ) ) ;
#11213 = ORIENTED_EDGE ( 'NONE', *, *, #56716, .F. ) ;
#11214 = PLANE ( 'NONE',  #21911 ) ;
#11215 = CARTESIAN_POINT ( 'NONE',  ( -92.69370383062498320, -209.9999999999999716, 79.16531250086714522 ) ) ;
#11216 = ORIENTED_EDGE ( 'NONE', *, *, #29521, .F. ) ;
#11217 = VERTEX_POINT ( 'NONE', #44619 ) ;
#11218 = ORIENTED_EDGE ( 'NONE', *, *, #4273, .T. ) ;
#11219 = LINE ( 'NONE', #10854, #19126 ) ;
#11220 = AXIS2_PLACEMENT_3D ( 'NONE', #25842, #53311, #29997 ) ;
#11221 = DIRECTION ( 'NONE',  ( 0.000000000000000000, 0.8660254037844368202, 0.5000000000000029976 ) ) ;
#11222 = EDGE_LOOP ( 'NONE', ( #25239, #49070, #65762, #52744 ) ) ;
#11223 = CARTESIAN_POINT ( 'NONE',  ( -92.69370383062498320, -209.9999999999999716, 77.26031250086714408 ) ) ;
#11224 = VERTEX_POINT ( 'NONE', #22419 ) ;
#11225 = FACE_OUTER_BOUND ( 'NONE', #5378, .T. ) ;
#11226 = DIRECTION ( 'NONE',  ( 1.000000000000000000, -0.000000000000000000, -0.000000000000000000 ) ) ;
#11227 = CARTESIAN_POINT ( 'NONE',  ( 11.99999999999999822, 81.90746397400394585, -3.894527615416972566 ) ) ;
#11228 = EDGE_CURVE ( 'NONE', #66160, #52399, #26427, .T. ) ;
#11229 = PLANE ( 'NONE',  #9884 ) ;
#11230 = EDGE_CURVE ( 'NONE', #62276, #59771, #30079, .T. ) ;
#11231 = EDGE_CURVE ( 'NONE', #17107, #16098, #27670, .T. ) ;
#11232 = DIRECTION ( 'NONE',  ( -1.000000000000000000, -0.000000000000000000, -0.000000000000000000 ) ) ;
#11233 = CARTESIAN_POINT ( 'NONE',  ( 93.84685191531248449, 91.99731107132950569, 85.72697916753379843 ) ) ;
#11234 = PLANE ( 'NONE',  #29202 ) ;
#11235 = CARTESIAN_POINT ( 'NONE',  ( -93.67500000000003979, 87.70503267997129626, 75.60666666666665492 ) ) ;
#11236 = DIRECTION ( 'NONE',  ( 0.000000000000000000, 0.000000000000000000, 1.000000000000000000 ) ) ;
#11237 = DIRECTION ( 'NONE',  ( -1.000000000000000000, 0.000000000000000000, 0.000000000000000000 ) ) ;
#11238 = CARTESIAN_POINT ( 'NONE',  ( 0.000000000000000000, -65.64334221924937651, 41.19522573413711797 ) ) ;
#11239 = CARTESIAN_POINT ( 'NONE',  ( -92.35000000000003695, 89.99999997442942856, 84.04687500080852658 ) ) ;
#11240 = CARTESIAN_POINT ( 'NONE',  ( 11.99999999999999822, 0.000000000000000000, 0.000000000000000000 ) ) ;
#11241 = ADVANCED_FACE ( 'NONE', ( #27294 ), #44986, .T. ) ;
#11242 = VECTOR ( 'NONE', #73680, 1000.000000000000000 ) ;
#11243 =( BOUNDED_CURVE ( )  B_SPLINE_CURVE ( 2, ( #7990, #59880, #4590, #67730, #9096, #39159, #15475 ),
 .UNSPECIFIED., .F., .F. ) 
 B_SPLINE_CURVE_WITH_KNOTS ( ( 3, 2, 2, 3 ),
 ( 0.3333333333333333703, 0.3402777777777777901, 0.3472222222222221544, 0.3541666666666665741 ),
 .UNSPECIFIED. ) 
 CURVE ( )  GEOMETRIC_REPRESENTATION_ITEM ( )  RATIONAL_B_SPLINE_CURVE ( ( 0.9999999999999988898, 0.8660254037844398178, 1.000000000000000000, 0.8660254037844387076, 1.000000000000000000, 0.8660254037844408170, 0.9999999999999978906 ) ) 
 REPRESENTATION_ITEM ( '' )  );
#11244 = CARTESIAN_POINT ( 'NONE',  ( 0.000000000000000000, -9.188173127307001309, -40.98264845739759465 ) ) ;
#11245 = CIRCLE ( 'NONE', #41235, 31.99999999999998934 ) ;
#11246 = DIRECTION ( 'NONE',  ( 0.000000000000000000, 0.3090169943749480619, -0.9510565162951533091 ) ) ;
#11247 = DIRECTION ( 'NONE',  ( 0.000000000000000000, 0.000000000000000000, 1.000000000000000000 ) ) ;
#11248 = CIRCLE ( 'NONE', #30443, 42.00000000000000000 ) ;
#11249 = DIRECTION ( 'NONE',  ( 0.000000000000000000, 0.000000000000000000, 1.000000000000000000 ) ) ;
#11250 = AXIS2_PLACEMENT_3D ( 'NONE', #61924, #22059, #10406 ) ;
#11251 = DIRECTION ( 'NONE',  ( -1.000000000000000000, 0.000000000000000000, 0.000000000000000000 ) ) ;
#11252 = CARTESIAN_POINT ( 'NONE',  ( -93.67499999999998295, -207.7050326799711968, 83.43833333333333258 ) ) ;
#11253 = DIRECTION ( 'NONE',  ( 0.000000000000000000, 0.000000000000000000, 1.000000000000000000 ) ) ;
#11255 = VERTEX_POINT ( 'NONE', #38970 ) ;
#11254 =( BOUNDED_CURVE ( )  B_SPLINE_CURVE ( 2, ( #17216, #22492, #73977, #46163, #23236, #57814, #6320 ),
 .UNSPECIFIED., .F., .F. ) 
 B_SPLINE_CURVE_WITH_KNOTS ( ( 3, 2, 2, 3 ),
 ( 0.06350193517735297499, 0.07055765540882327769, 0.07761342094970608008, 0.08466915177892291033 ),
 .UNSPECIFIED. ) 
 CURVE ( )  GEOMETRIC_REPRESENTATION_ITEM ( )  RATIONAL_B_SPLINE_CURVE ( ( 0.9999982793443948914, 0.8660262641177659537, 1.000000000000000000, 0.8660254037844387076, 1.000000000000000000, 0.8660260628881748524, 0.9999986817990127452 ) ) 
 REPRESENTATION_ITEM ( '' )  );
#11256 = CARTESIAN_POINT ( 'NONE',  ( 11.99999999999999822, 0.000000000000000000, 0.000000000000000000 ) ) ;
#11257 = CARTESIAN_POINT ( 'NONE',  ( 0.000000000000000000, -5.256550761633393520, 77.32052557432838569 ) ) ;
#11258 = CYLINDRICAL_SURFACE ( 'NONE', #19030, 37.49900000000000233 ) ;
#11259 = VECTOR ( 'NONE', #24515, 1000.000000000000000 ) ;
#11260 = CARTESIAN_POINT ( 'NONE',  ( 0.000000000000000000, 0.000000000000000000, 0.000000000000000000 ) ) ;
#11261 = CARTESIAN_POINT ( 'NONE',  ( 95.00000000000000000, -212.6630814284392557, 86.15031250086714465 ) ) ;
#11262 = ORIENTED_EDGE ( 'NONE', *, *, #68442, .T. ) ;
#11263 = ORIENTED_EDGE ( 'NONE', *, *, #45856, .T. ) ;
#11264 = CARTESIAN_POINT ( 'NONE',  ( 10.00000000000000000, 44.99326035066149387, -68.55367621811095091 ) ) ;
#11265 = ORIENTED_EDGE ( 'NONE', *, *, #32489, .F. ) ;
#11266 = CIRCLE ( 'NONE', #29235, 15.99999999999999645 ) ;
#11267 = CARTESIAN_POINT ( 'NONE',  ( 97.30629616937498838, -209.9999999999999716, 79.16531250086714522 ) ) ;
#11268 = ORIENTED_EDGE ( 'NONE', *, *, #61396, .T. ) ;
#11269 = CARTESIAN_POINT ( 'NONE',  ( 92.69370383062501162, -208.6684592857803011, 82.12864583420048348 ) ) ;
#11270 = ORIENTED_EDGE ( 'NONE', *, *, #9955, .F. ) ;
#11271 = CARTESIAN_POINT ( 'NONE',  ( 0.000000000000000000, 0.000000000000000000, 0.000000000000000000 ) ) ;
#11272 = ORIENTED_EDGE ( 'NONE', *, *, #49544, .F. ) ;
#11273 = ORIENTED_EDGE ( 'NONE', *, *, #63346, .F. ) ;
#11274 = FILL_AREA_STYLE ('',( #10914 ) ) ;
#11275 = EDGE_CURVE ( 'NONE', #31341, #8511, #54078, .T. ) ;
#11276 = DIRECTION ( 'NONE',  ( -0.000000000000000000, -0.000000000000000000, 1.000000000000000000 ) ) ;
#11277 = VERTEX_POINT ( 'NONE', #28416 ) ;
#11278 = DIRECTION ( 'NONE',  ( -1.000000000000000000, -0.000000000000000000, 0.000000000000000000 ) ) ;
#11279 = CARTESIAN_POINT ( 'NONE',  ( 96.32499999999998863, -212.2949673200287179, 87.11604166840096752 ) ) ;
#11280 = EDGE_CURVE ( 'NONE', #51135, #63042, #51349, .T. ) ;
#11281 = VERTEX_POINT ( 'NONE', #59878 ) ;
#11282 = CARTESIAN_POINT ( 'NONE',  ( 11.99999999999999822, 0.000000000000000000, 0.000000000000000000 ) ) ;
#11283 = ORIENTED_EDGE ( 'NONE', *, *, #54318, .F. ) ;
#11284 = CARTESIAN_POINT ( 'NONE',  ( -95.00000000000002842, 92.66308142843932671, 89.64281250086715147 ) ) ;
#11285 = ADVANCED_FACE ( 'NONE', ( #71496 ), #34810, .T. ) ;
#11286 = VECTOR ( 'NONE', #38154, 1000.000000000000000 ) ;
#11287 = ORIENTED_EDGE ( 'NONE', *, *, #71770, .T. ) ;
#11288 = ORIENTED_EDGE ( 'NONE', *, *, #52726, .F. ) ;
#11289 = AXIS2_PLACEMENT_3D ( 'NONE', #37789, #53585, #14472 ) ;
#11290 = VERTEX_POINT ( 'NONE', #26013 ) ;
#11291 = DIRECTION ( 'NONE',  ( -1.000000000000000000, 0.000000000000000000, -0.000000000000000000 ) ) ;
#11292 = CONTEXT_DEPENDENT_SHAPE_REPRESENTATION ( #15798, #17633 ) ;
#11293 = CARTESIAN_POINT ( 'NONE',  ( 11.99999999999999822, -78.73519480814969995, 22.90783923731599359 ) ) ;
#11294 = ORIENTED_EDGE ( 'NONE', *, *, #35084, .F. ) ;
#11295 = ORIENTED_EDGE ( 'NONE', *, *, #50307, .T. ) ;
#11296 = ORIENTED_EDGE ( 'NONE', *, *, #68606, .F. ) ;
#11297 = DIRECTION ( 'NONE',  ( -1.000000000000000000, -0.000000000000000000, 0.000000000000000000 ) ) ;
#11298 = CARTESIAN_POINT ( 'NONE',  ( 11.99999999999999822, -76.41127070299280888, 12.93880638057290788 ) ) ;
#11299 = EDGE_CURVE ( 'NONE', #71089, #73769, #42217, .T. ) ;
#11300 = CARTESIAN_POINT ( 'NONE',  ( -97.30629616937501680, 91.33154071421968467, 75.14364583420049826 ) ) ;
#11301 = EDGE_CURVE ( 'NONE', #37316, #1281, #12238, .T. ) ;
#11302 = EDGE_LOOP ( 'NONE', ( #11814, #57626, #42635, #43381 ) ) ;
#11303 = CARTESIAN_POINT ( 'NONE',  ( 97.64999999999999147, -209.9999999999999716, 89.68250000000000455 ) ) ;
#11304 = ORIENTED_EDGE ( 'NONE', *, *, #13826, .T. ) ;
#11305 = CARTESIAN_POINT ( 'NONE',  ( 94.99999999999998579, 93.05995642670504253, 75.23624999999998408 ) ) ;
#11306 = CARTESIAN_POINT ( 'NONE',  ( -96.15314808468747287, -208.0026889286704943, 85.09197916753380753 ) ) ;
#11307 = VERTEX_POINT ( 'NONE', #35174 ) ;
#11308 = DIRECTION ( 'NONE',  ( -1.000000000000000000, 0.000000000000000000, -0.000000000000000000 ) ) ;
#11309 = CARTESIAN_POINT ( 'NONE',  ( -10.00000000000000000, 0.000000000000000000, 0.000000000000000000 ) ) ;
#11310 = CARTESIAN_POINT ( 'NONE',  ( 92.35000000000006537, -208.4700217866474077, 88.04208333333330927 ) ) ;
#11311 = CARTESIAN_POINT ( 'NONE',  ( -97.30629616937497417, -208.6684592857803295, 77.52489583420046415 ) ) ;
#11312 = AXIS2_PLACEMENT_3D ( 'NONE', #2469, #71189, #42643 ) ;
#11313 = CARTESIAN_POINT ( 'NONE',  ( -97.64999999999996305, -209.9999999999999716, 88.73000000000000398 ) ) ;
#11314 = DIRECTION ( 'NONE',  ( 0.000000000000000000, 0.3826834323650840086, 0.9238795325112891810 ) ) ;
#11315 = EDGE_CURVE ( 'NONE', #13415, #21312, #40827, .T. ) ;
#11316 = EDGE_CURVE ( 'NONE', #13377, #49169, #51661, .T. ) ;
#11317 = CARTESIAN_POINT ( 'NONE',  ( -93.67500000000003979, 87.70503267997129626, 85.21104166840096639 ) ) ;
#11318 = CARTESIAN_POINT ( 'NONE',  ( -2.981742216678212820, 0.000000000000000000, 0.000000000000000000 ) ) ;
#11319 = LINE ( 'NONE', #69213, #31949 ) ;
#11320 = CARTESIAN_POINT ( 'NONE',  ( -97.30629616937501680, 90.00000000000004263, 80.11781250086713158 ) ) ;
#11321 = CARTESIAN_POINT ( 'NONE',  ( 22.75000000000000000, 0.000000000000000000, 0.000000000000000000 ) ) ;
#11322 = LINE ( 'NONE', #51549, #14600 ) ;
#11323 = ORIENTED_EDGE ( 'NONE', *, *, #24020, .T. ) ;
#11324 = PLANE ( 'NONE',  #49601 ) ;
#11325 = DIRECTION ( 'NONE',  ( -1.000000000000000000, 0.000000000000000000, 0.000000000000000000 ) ) ;
#11326 = CARTESIAN_POINT ( 'NONE',  ( 0.000000000000000000, 0.000000000000000000, 0.000000000000000000 ) ) ;
#11327 = AXIS2_PLACEMENT_3D ( 'NONE', #20983, #60487, #49187 ) ;
#11328 = CARTESIAN_POINT ( 'NONE',  ( -3.000000000000000000, 22.07842321921481243, 8.187992925817422218 ) ) ;
#11329 = DIRECTION ( 'NONE',  ( 0.000000000000000000, -0.8090169943749531134, 0.5877852522924653655 ) ) ;
#11330 = PLANE ( 'NONE',  #40181 ) ;
#11331 = CARTESIAN_POINT ( 'NONE',  ( -92.69370383062498320, -211.3315407142195852, 79.27114583420048177 ) ) ;
#11332 = CARTESIAN_POINT ( 'NONE',  ( 97.64999999999999147, -209.9999999999999716, 90.00000000000000000 ) ) ;
#11333 = AXIS2_PLACEMENT_3D ( 'NONE', #46515, #24327, #40885 ) ;
#11334 = ORIENTED_EDGE ( 'NONE', *, *, #52049, .F. ) ;
#11335 = CARTESIAN_POINT ( 'NONE',  ( 0.000000000000000000, 0.000000000000000000, 0.000000000000000000 ) ) ;
#11336 = CARTESIAN_POINT ( 'NONE',  ( -12.40464318976452596, 10.41032311384371489, 52.00000000000002132 ) ) ;
#11337 = PLANE ( 'NONE',  #49755 ) ;
#11338 = AXIS2_PLACEMENT_3D ( 'NONE', #20758, #62105, #56087 ) ;
#11339 = CIRCLE ( 'NONE', #7752, 31.99999999999998224 ) ;
#11340 = AXIS2_PLACEMENT_3D ( 'NONE', #58304, #7175, #31201 ) ;
#11341 = DIRECTION ( 'NONE',  ( -1.000000000000000000, -0.000000000000000000, 0.000000000000000000 ) ) ;
#11342 = ORIENTED_EDGE ( 'NONE', *, *, #25545, .T. ) ;
#11343 = LINE ( 'NONE', #125, #31214 ) ;
#11344 = CARTESIAN_POINT ( 'NONE',  ( 0.000000000000000000, -74.18225833017864090, -34.94270380257717790 ) ) ;
#11345 = EDGE_LOOP ( 'NONE', ( #40339, #8128, #26990, #1723 ) ) ;
#11346 = AXIS2_PLACEMENT_3D ( 'NONE', #2975, #44281, #3342 ) ;
#11347 = EDGE_CURVE ( 'NONE', #38625, #71349, #6070, .T. ) ;
#11348 = CARTESIAN_POINT ( 'NONE',  ( 96.15314808468748708, -208.0026889286704943, 88.79614583420047325 ) ) ;
#11349 = CARTESIAN_POINT ( 'NONE',  ( -97.64999999999996305, -208.4700217866474645, 83.67645833506763609 ) ) ;
#11350 = VERTEX_POINT ( 'NONE', #635 ) ;
#11351 = PRODUCT_DEFINITION ( 'UNKNOWN', '', #6459, #43167 ) ;
#11352 = AXIS2_PLACEMENT_3D ( 'NONE', #5223, #68739, #29226 ) ;
#11353 = EDGE_CURVE ( 'NONE', #2104, #12353, #70860, .T. ) ;
#11354 = CARTESIAN_POINT ( 'NONE',  ( 92.35000000000006537, -211.5299782133524786, 89.41791666666667027 ) ) ;
#11355 = VERTEX_POINT ( 'NONE', #6252 ) ;
#11356 = CYLINDRICAL_SURFACE ( 'NONE', #17854, 17.50000000000000355 ) ;
#11357 = ORIENTED_EDGE ( 'NONE', *, *, #52746, .F. ) ;
#11358 = CARTESIAN_POINT ( 'NONE',  ( -97.64999999978461176, -209.9999789922612479, 79.91868729551984529 ) ) ;
#11359 = VERTEX_POINT ( 'NONE', #31283 ) ;
#11360 = EDGE_CURVE ( 'NONE', #60498, #28566, #43303, .T. ) ;
#11361 = DIRECTION ( 'NONE',  ( 0.000000000000000000, 0.000000000000000000, 1.000000000000000000 ) ) ;
#11362 = ORIENTED_EDGE ( 'NONE', *, *, #74284, .T. ) ;
#11363 =( BOUNDED_CURVE ( )  B_SPLINE_CURVE ( 2, ( #721, #23612, #48385, #48754, #25086, #48023, #71676, #72052, #70935, #37493, #54401 ),
 .UNSPECIFIED., .F., .F. ) 
 B_SPLINE_CURVE_WITH_KNOTS ( ( 3, 2, 2, 2, 2, 3 ),
 ( 0.6985206468843488947, 0.6985207885473545542, 0.7055765540882368292, 0.7126323196291192152, 0.7196880851700017123, 0.7196881748034550386 ),
 .UNSPECIFIED. ) 
 CURVE ( )  GEOMETRIC_REPRESENTATION_ITEM ( )  RATIONAL_B_SPLINE_CURVE ( ( 0.9999946203249505672, 0.9999973101084687066, 1.000000000000000000, 0.8660254037844387076, 1.000000000000000000, 0.8660254037844387076, 1.000000000000000000, 0.8660254037844387076, 1.000000000000000000, 0.9999982980435435653, 0.9999965961303289852 ) ) 
 REPRESENTATION_ITEM ( '' )  );
#11364 = ORIENTED_EDGE ( 'NONE', *, *, #17720, .T. ) ;
#11365 = DIRECTION ( 'NONE',  ( 0.000000000000000000, 0.000000000000000000, 1.000000000000000000 ) ) ;
#11366 = EDGE_CURVE ( 'NONE', #63788, #70934, #6607, .T. ) ;
#11367 = ORIENTED_EDGE ( 'NONE', *, *, #28083, .T. ) ;
#11368 = EDGE_LOOP ( 'NONE', ( #17884, #53164, #13834, #73111 ) ) ;
#11369 = CARTESIAN_POINT ( 'NONE',  ( 11.99999999999999822, 55.38113227695783536, 54.21277698773694453 ) ) ;
#11370 = EDGE_CURVE ( 'NONE', #68271, #62567, #52452, .T. ) ;
#11371 = DIRECTION ( 'NONE',  ( -1.000000000000000000, 0.000000000000000000, -0.000000000000000000 ) ) ;
#11372 = VERTEX_POINT ( 'NONE', #59499 ) ;
#11373 = ORIENTED_EDGE ( 'NONE', *, *, #14407, .F. ) ;
#11374 = CARTESIAN_POINT ( 'NONE',  ( 94.99999999999998579, 87.33691857156068750, 83.45156250086714067 ) ) ;
#11375 = VERTEX_POINT ( 'NONE', #3121 ) ;
#11376 = CARTESIAN_POINT ( 'NONE',  ( 92.69370383062501162, -208.6684592857803011, 86.41489583420047893 ) ) ;
#11377 = AXIS2_PLACEMENT_3D ( 'NONE', #21639, #33279, #22388 ) ;
#11378 = APPLICATION_PROTOCOL_DEFINITION ( 'draft international standard', 'automotive_design', 1998, #56092 ) ;
#11379 = CARTESIAN_POINT ( 'NONE',  ( -97.64999999999996305, -211.5299782133524218, 81.24229166840096639 ) ) ;
#11380 = DIRECTION ( 'NONE',  ( -1.000000000000000000, -0.000000000000000000, 0.000000000000000000 ) ) ;
#11381 = DIRECTION ( 'NONE',  ( -0.000000000000000000, -0.000000000000000000, -1.000000000000000000 ) ) ;
#11382 = FACE_OUTER_BOUND ( 'NONE', #53895, .T. ) ;
#11383 = CYLINDRICAL_SURFACE ( 'NONE', #56456, 31.99999999999998579 ) ;
#11384 = DIRECTION ( 'NONE',  ( 0.000000000000000000, 0.000000000000000000, 1.000000000000000000 ) ) ;
#11385 = CARTESIAN_POINT ( 'NONE',  ( -97.30629616937497417, -208.6684592857803011, 88.95489583420048518 ) ) ;
#11386 = EDGE_CURVE ( 'NONE', #35978, #3451, #25648, .T. ) ;
#11387 = CARTESIAN_POINT ( 'NONE',  ( -92.69370383062502583, 88.66845928578038638, 85.62114583420047609 ) ) ;
#11388 = EDGE_CURVE ( 'NONE', #37645, #1535, #44475, .T. ) ;
#11389 = ORIENTED_EDGE ( 'NONE', *, *, #6525, .F. ) ;
#11391 = CARTESIAN_POINT ( 'NONE',  ( -92.69370383062504004, 90.00000000000004263, 83.61031250086713840 ) ) ;
#11390 = CARTESIAN_POINT ( 'NONE',  ( 94.99999999999998579, 87.33691857156068750, 85.99156250086714692 ) ) ;
#11392 = B_SPLINE_CURVE_WITH_KNOTS ( 'NONE', 3,
 ( #31864, #20213, #20598, #43549 ),
 .UNSPECIFIED., .F., .F.,
 ( 4, 4 ),
 ( 2.446487931514449005E-06, 1.000000000000000000 ),
 .UNSPECIFIED. ) ;
#11393 = ORIENTED_EDGE ( 'NONE', *, *, #11360, .F. ) ;
#11394 = CARTESIAN_POINT ( 'NONE',  ( -92.35000000000003695, 90.00000000000004263, 87.77749999999998920 ) ) ;
#11395 = CARTESIAN_POINT ( 'NONE',  ( -97.30629616937501680, 90.00000000000004263, 89.80156250086714920 ) ) ;
#11396 = AXIS2_PLACEMENT_3D ( 'NONE', #27560, #21167, #10642 ) ;
#11397 = CARTESIAN_POINT ( 'NONE',  ( 100.0010000000000900, 64.99999999999997158, -290.0000000000000568 ) ) ;
#11398 = CARTESIAN_POINT ( 'NONE',  ( -5.000000000000000000, 0.000000000000000000, -6.000000000000000000 ) ) ;
#11399 = CARTESIAN_POINT ( 'NONE',  ( -93.84685191531247028, -211.9973110713294489, 87.94947916753380923 ) ) ;
#11400 = DIRECTION ( 'NONE',  ( -1.000000000000000000, 0.000000000000000000, -0.000000000000000000 ) ) ;
#11401 = DIRECTION ( 'NONE',  ( 0.000000000000000000, 0.000000000000000000, 1.000000000000000000 ) ) ;
#11402 = CYLINDRICAL_SURFACE ( 'NONE', #12158, 82.00000000000000000 ) ;
#11403 = AXIS2_PLACEMENT_3D ( 'NONE', #14396, #8762, #3146 ) ;
#11404 = DIRECTION ( 'NONE',  ( 0.000000000000000000, 0.000000000000000000, 1.000000000000000000 ) ) ;
#11405 = VERTEX_POINT ( 'NONE', #57748 ) ;
#11406 = EDGE_LOOP ( 'NONE', ( #38025, #56497, #22933, #69550 ) ) ;
#11407 = CARTESIAN_POINT ( 'NONE',  ( -92.35000000000005116, 88.47002178664754979, 78.19958333333332234 ) ) ;
#11408 = CARTESIAN_POINT ( 'NONE',  ( 11.99999999999999822, -31.46837873494930093, -68.27212725128309501 ) ) ;
#11409 = LINE ( 'NONE', #6883, #38169 ) ;
#11410 = CARTESIAN_POINT ( 'NONE',  ( -92.34999999999999432, -209.9999999999999716, 88.41249999999999432 ) ) ;
#11411 = CARTESIAN_POINT ( 'NONE',  ( 0.000000000000000000, -27.74655509720725988, 77.16300072079653205 ) ) ;
#11412 = CARTESIAN_POINT ( 'NONE',  ( -93.67500000000003979, 87.70503267997129626, 86.48104166840096241 ) ) ;
#11413 = CARTESIAN_POINT ( 'NONE',  ( 10.00000000000000000, 20.40083707022987625, -72.35432306680462489 ) ) ;
#11414 = VERTEX_POINT ( 'NONE', #2398 ) ;
#11415 = CARTESIAN_POINT ( 'NONE',  ( -97.30629616937501680, 90.00000000000004263, 77.57781250086713953 ) ) ;
#11416 = VECTOR ( 'NONE', #67154, 1000.000000000000000 ) ;
#11417 = CYLINDRICAL_SURFACE ( 'NONE', #1951, 42.00000000000000000 ) ;
#11418 = CARTESIAN_POINT ( 'NONE',  ( 11.99999999999999822, -12.93880638057369659, 76.41127070299266677 ) ) ;
#11419 = DIRECTION ( 'NONE',  ( -1.000000000000000000, 0.000000000000000000, 0.000000000000000000 ) ) ;
#11420 = FACE_OUTER_BOUND ( 'NONE', #57743, .T. ) ;
#11421 = AXIS2_PLACEMENT_3D ( 'NONE', #50532, #32118, #67456 ) ;
#11422 = DIRECTION ( 'NONE',  ( -0.5000000000000042188, 0.000000000000000000, 0.8660254037844361541 ) ) ;
#11423 = DIRECTION ( 'NONE',  ( 2.603472992746261562E-14, 2.546204323184492723E-14, -1.000000000000000000 ) ) ;
#11424 = AXIS2_PLACEMENT_3D ( 'NONE', #71706, #37149, #55169 ) ;
#11425 = CARTESIAN_POINT ( 'NONE',  ( 92.69370383062498320, 91.33154071421968467, 77.04864583420048518 ) ) ;
#11426 = EDGE_CURVE ( 'NONE', #13869, #73989, #19996, .T. ) ;
#11427 = CARTESIAN_POINT ( 'NONE',  ( -97.30629616937495996, -209.9999999999999716, 78.37156250086715659 ) ) ;
#11428 = DIRECTION ( 'NONE',  ( -7.962523111839282146E-16, 1.065814103640130873E-14, 1.000000000000000000 ) ) ;
#11429 = ORIENTED_EDGE ( 'NONE', *, *, #36655, .F. ) ;
#11430 = CARTESIAN_POINT ( 'NONE',  ( 0.000000000000000000, 0.000000000000000000, 0.000000000000000000 ) ) ;
#11431 = DIRECTION ( 'NONE',  ( -1.000000000000000000, 0.000000000000000000, 0.000000000000000000 ) ) ;
#11432 = CARTESIAN_POINT ( 'NONE',  ( 0.000000000000000000, 8.840884882376133902, -74.65374052328640175 ) ) ;
#11433 = AXIS2_PLACEMENT_3D ( 'NONE', #31714, #2823, #49008 ) ;
#11434 = ADVANCED_FACE ( 'NONE', ( #25288 ), #31649, .F. ) ;
#11435 = CARTESIAN_POINT ( 'NONE',  ( -96.15314808468752972, 91.99731107132950569, 75.09072916753380866 ) ) ;
#11436 = CARTESIAN_POINT ( 'NONE',  ( 97.30629616937498838, -209.9999999999999716, 81.70531250086713726 ) ) ;
#11437 = ORIENTED_EDGE ( 'NONE', *, *, #49071, .F. ) ;
#11438 = EDGE_CURVE ( 'NONE', #46185, #3104, #67279, .T. ) ;
#11439 = CARTESIAN_POINT ( 'NONE',  ( 10.00000000000000000, 35.92658777277511462, 10.74501242461295014 ) ) ;
#11440 = ORIENTED_EDGE ( 'NONE', *, *, #31852, .F. ) ;
#11441 = AXIS2_PLACEMENT_3D ( 'NONE', #43874, #66796, #15285 ) ;
#11442 = CARTESIAN_POINT ( 'NONE',  ( -94.99999999999997158, -209.9999999999999716, 90.00000000000000000 ) ) ;
#11443 = CIRCLE ( 'NONE', #45057, 82.00000000000000000 ) ;
#11444 = EDGE_LOOP ( 'NONE', ( #7661, #54568, #68630, #73101 ) ) ;
#11445 = ADVANCED_FACE ( 'NONE', ( #29515 ), #2022, .T. ) ;
#11446 = CARTESIAN_POINT ( 'NONE',  ( -94.99999999999997158, -206.9400435732949575, 83.49125000000000796 ) ) ;
#11447 = CIRCLE ( 'NONE', #52234, 5.000000000000000000 ) ;
#11448 = ORIENTED_EDGE ( 'NONE', *, *, #19451, .T. ) ;
#11449 = ORIENTED_EDGE ( 'NONE', *, *, #15375, .T. ) ;
#11450 = AXIS2_PLACEMENT_3D ( 'NONE', #34817, #23531, #5521 ) ;
#11451 = ORIENTED_EDGE ( 'NONE', *, *, #65686, .F. ) ;
#11452 = DIRECTION ( 'NONE',  ( -1.000000000000000000, 0.000000000000000000, -0.000000000000000000 ) ) ;
#11453 = ORIENTED_EDGE ( 'NONE', *, *, #62752, .F. ) ;
#11454 = VERTEX_POINT ( 'NONE', #9462 ) ;
#11455 =( BOUNDED_CURVE ( )  B_SPLINE_CURVE ( 2, ( #24691, #64932, #70532, #19042, #63451, #28857, #51786 ),
 .UNSPECIFIED., .F., .F. ) 
 B_SPLINE_CURVE_WITH_KNOTS ( ( 3, 2, 2, 3 ),
 ( 0.3958333333333330373, 0.4027777777777774570, 0.4097222222222218768, 0.4166666666666662966 ),
 .UNSPECIFIED. ) 
 CURVE ( )  GEOMETRIC_REPRESENTATION_ITEM ( )  RATIONAL_B_SPLINE_CURVE ( ( 1.000000000000005329, 0.8660254037844333785, 1.000000000000000000, 0.8660254037844387076, 1.000000000000000000, 0.8660254037844462571, 0.9999999999999924505 ) ) 
 REPRESENTATION_ITEM ( '' )  );
#11456 = CARTESIAN_POINT ( 'NONE',  ( 92.69370383062498320, 88.66845928578037217, 82.23447916753383424 ) ) ;
#11457 = ADVANCED_FACE ( 'NONE', ( #32019 ), #73350, .F. ) ;
#11458 = CARTESIAN_POINT ( 'NONE',  ( 93.67500000000001137, -212.2949673200287179, 77.40583333333331950 ) ) ;
#11459 = CIRCLE ( 'NONE', #26912, 31.99999999999999289 ) ;
#11460 = ORIENTED_EDGE ( 'NONE', *, *, #48377, .T. ) ;
#11461 = ORIENTED_EDGE ( 'NONE', *, *, #48718, .F. ) ;
#11462 = ORIENTED_EDGE ( 'NONE', *, *, #66893, .T. ) ;
#11463 = VERTEX_POINT ( 'NONE', #4963 ) ;
#11464 = CARTESIAN_POINT ( 'NONE',  ( 0.000000000000000000, -2.446882695291883605E-15, -2.499999999999983569 ) ) ;
#11465 = DIRECTION ( 'NONE',  ( -0.9675294772147033928, 0.2527582060401658559, 0.000000000000000000 ) ) ;
#11466 = CARTESIAN_POINT ( 'NONE',  ( -96.32499999999996021, -207.7050326799711968, 75.36854166840096525 ) ) ;
#11467 = PRESENTATION_LAYER_ASSIGNMENT (  '', '', ( #10299 ) ) ;
#11468 = DIRECTION ( 'NONE',  ( 0.000000000000000000, 0.000000000000000000, 1.000000000000000000 ) ) ;
#11469 = LINE ( 'NONE', #73504, #19441 ) ;
#11470 = CARTESIAN_POINT ( 'NONE',  ( 10.00000000000000000, 26.08949754953062694, -27.05870788708203989 ) ) ;
#11471 = DIRECTION ( 'NONE',  ( -0.000000000000000000, -0.000000000000000000, 1.000000000000000000 ) ) ;
#11472 = DIRECTION ( 'NONE',  ( -0.000000000000000000, -0.000000000000000000, 1.000000000000000000 ) ) ;
#11473 = ORIENTED_EDGE ( 'NONE', *, *, #70773, .T. ) ;
#11474 = CARTESIAN_POINT ( 'NONE',  ( -92.34999999999999432, -211.5299782133524502, 82.08895833506764461 ) ) ;
#11476 = ORIENTED_EDGE ( 'NONE', *, *, #39083, .T. ) ;
#11475 = EDGE_CURVE ( 'NONE', #45880, #46053, #55703, .T. ) ;
#11477 = CYLINDRICAL_SURFACE ( 'NONE', #15866, 31.99999999999998579 ) ;
#11478 = ADVANCED_FACE ( 'NONE', ( #20746 ), #27110, .T. ) ;
#11479 = ORIENTED_EDGE ( 'NONE', *, *, #70861, .T. ) ;
#11481 = CARTESIAN_POINT ( 'NONE',  ( -92.35000000000005116, 91.52997821335253548, 80.92479166840098515 ) ) ;
#11480 = CARTESIAN_POINT ( 'NONE',  ( 94.99999999999998579, 86.94004357329500010, 78.17312500173430578 ) ) ;
#11483 = EDGE_CURVE ( 'NONE', #53012, #32056, #61719, .T. ) ;
#11482 = ORIENTED_EDGE ( 'NONE', *, *, #36488, .F. ) ;
#11484 = CARTESIAN_POINT ( 'NONE',  ( 96.15314808468748708, 88.00268892867053694, 79.21822916753382060 ) ) ;
#11485 = CARTESIAN_POINT ( 'NONE',  ( 4.903647372192503795, -146.0423547792665886, 2.500000000000000000 ) ) ;
#11486 = DIRECTION ( 'NONE',  ( 0.000000000000000000, 0.000000000000000000, 1.000000000000000000 ) ) ;
#11487 = CARTESIAN_POINT ( 'NONE',  ( 97.65000000000000568, -211.5299782133524218, 79.54895833506762415 ) ) ;
#11488 = LINE ( 'NONE', #44610, #55849 ) ;
#11489 = ORIENTED_EDGE ( 'NONE', *, *, #20102, .T. ) ;
#11490 = CARTESIAN_POINT ( 'NONE',  ( -12.00000000000000000, 0.000000000000000000, 0.000000000000000000 ) ) ;
#11491 = CARTESIAN_POINT ( 'NONE',  ( 97.65000000000000568, -208.4700217866474645, 77.03541666666666288 ) ) ;
#11492 = CARTESIAN_POINT ( 'NONE',  ( 0.000000000000000000, 0.000000000000000000, 0.000000000000000000 ) ) ;
#11493 = ORIENTED_EDGE ( 'NONE', *, *, #46879, .T. ) ;
#11494 = VERTEX_POINT ( 'NONE', #3847 ) ;
#11495 = CARTESIAN_POINT ( 'NONE',  ( -10.00000000000000000, 0.000000000000000000, 0.000000000000000000 ) ) ;
#11496 = CARTESIAN_POINT ( 'NONE',  ( -2.739742549670663330, -4.191711593333635300, -0.5197061503823270368 ) ) ;
#11497 = DIRECTION ( 'NONE',  ( -0.1276937514489679404, -0.9918136447140103451, 0.000000000000000000 ) ) ;
#11498 = CARTESIAN_POINT ( 'NONE',  ( -92.69370383062498320, -211.3315407142195852, 82.44614583420049314 ) ) ;
#11499 = ORIENTED_EDGE ( 'NONE', *, *, #10899, .T. ) ;
#11500 = ORIENTED_EDGE ( 'NONE', *, *, #72401, .F. ) ;
#11501 = DIRECTION ( 'NONE',  ( 2.603472992746261562E-14, 2.546204323184492723E-14, -1.000000000000000000 ) ) ;
#11502 = CIRCLE ( 'NONE', #48697, 23.50000000000000355 ) ;
#11503 = CARTESIAN_POINT ( 'NONE',  ( -97.51367041768831712, -210.0000000000000284, 74.91808492278045151 ) ) ;
#11504 = DIRECTION ( 'NONE',  ( 0.000000000000000000, 0.000000000000000000, -1.000000000000000000 ) ) ;
#11505 = CIRCLE ( 'NONE', #65560, 16.00000000000000000 ) ;
#11506 = CARTESIAN_POINT ( 'NONE',  ( 10.00000000000000000, 0.000000000000000000, 0.000000000000000000 ) ) ;
#11507 = CARTESIAN_POINT ( 'NONE',  ( 11.99999999999999822, -65.59268652807237743, 36.72794159290217664 ) ) ;
#11508 = DIRECTION ( 'NONE',  ( -1.000000000000000000, -0.000000000000000000, -0.000000000000000000 ) ) ;
#11509 = AXIS2_PLACEMENT_3D ( 'NONE', #68583, #63687, #33983 ) ;
#11510 = PLANE ( 'NONE',  #24122 ) ;
#11511 = CARTESIAN_POINT ( 'NONE',  ( 6.000000000000000000, 3.894527615419050903, -81.90746397400384637 ) ) ;
#11512 = CARTESIAN_POINT ( 'NONE',  ( -92.34999999999999432, -209.9999999999999716, 90.00000000000000000 ) ) ;
#11513 = CARTESIAN_POINT ( 'NONE',  ( 10.00000000000000000, 55.38113227695858143, -54.21277698773617715 ) ) ;
#11514 = AXIS2_PLACEMENT_3D ( 'NONE', #63678, #40357, #28700 ) ;
#11515 = AXIS2_PLACEMENT_3D ( 'NONE', #7255, #6876, #64034 ) ;
#11516 = CARTESIAN_POINT ( 'NONE',  ( 97.30629616937498838, 90.00000000000002842, 88.21406250086714351 ) ) ;
#11517 = CARTESIAN_POINT ( 'NONE',  ( -97.30629616937497417, -211.3315407142195852, 88.58447916753382856 ) ) ;
#11518 = LINE ( 'NONE', #62303, #9798 ) ;
#11520 = EDGE_CURVE ( 'NONE', #40918, #30770, #73276, .T. ) ;
#11519 = EDGE_LOOP ( 'NONE', ( #26173, #60326, #17755, #27328 ) ) ;
#11521 = CARTESIAN_POINT ( 'NONE',  ( -93.84685191531254134, 91.99731107132950569, 81.17614583420048291 ) ) ;
#11522 = AXIS2_PLACEMENT_3D ( 'NONE', #51858, #68428, #16917 ) ;
#11523 = EDGE_CURVE ( 'NONE', #7257, #57225, #68473, .T. ) ;
#11524 = CARTESIAN_POINT ( 'NONE',  ( 0.000000000000000000, 0.000000000000000000, 0.000000000000000000 ) ) ;
#11525 = EDGE_CURVE ( 'NONE', #24794, #12008, #3478, .T. ) ;
#11526 = VERTEX_POINT ( 'NONE', #26748 ) ;
#11527 = DIRECTION ( 'NONE',  ( -1.000000000000000000, 0.000000000000000000, 0.000000000000000000 ) ) ;
#11528 = CARTESIAN_POINT ( 'NONE',  ( 0.000000000000000000, 0.000000000000000000, -275.0000000000000000 ) ) ;
#11529 = PLANE ( 'NONE',  #40824 ) ;
#11530 = EDGE_CURVE ( 'NONE', #8427, #21255, #20485, .T. ) ;
#11531 = CARTESIAN_POINT ( 'NONE',  ( 0.000000000000000000, 0.000000000000000000, 0.000000000000000000 ) ) ;
#11532 = CARTESIAN_POINT ( 'NONE',  ( 97.30629616937498838, -209.9999999999999716, 74.87906250086714977 ) ) ;
#11533 = ORIENTED_EDGE ( 'NONE', *, *, #7917, .T. ) ;
#11534 = ORIENTED_EDGE ( 'NONE', *, *, #38642, .T. ) ;
#11535 = CARTESIAN_POINT ( 'NONE',  ( 96.15314808468750130, -211.9973110713294489, 84.93322916753382401 ) ) ;
#11536 = CARTESIAN_POINT ( 'NONE',  ( -97.65000000000004832, -208.4700217866474929, 81.05708333333332405 ) ) ;
#11537 = CARTESIAN_POINT ( 'NONE',  ( 0.000000000000000000, 0.000000000000000000, 0.000000000000000000 ) ) ;
#11538 = DIRECTION ( 'NONE',  ( 0.000000000000000000, 0.000000000000000000, 1.000000000000000000 ) ) ;
#11539 = LINE ( 'NONE', #57420, #20683 ) ;
#11540 = EDGE_CURVE ( 'NONE', #64759, #61415, #39157, .T. ) ;
#11541 = AXIS2_PLACEMENT_3D ( 'NONE', #27189, #61807, #33208 ) ;
#11542 = DIRECTION ( 'NONE',  ( 0.000000000000000000, 0.000000000000000000, 1.000000000000000000 ) ) ;
#11543 = CARTESIAN_POINT ( 'NONE',  ( 92.35000000000002274, -208.4700217866474645, 89.31208333333333371 ) ) ;
#11544 = ORIENTED_EDGE ( 'NONE', *, *, #2239, .T. ) ;
#11545 = ORIENTED_EDGE ( 'NONE', *, *, #32759, .F. ) ;
#11546 = VERTEX_POINT ( 'NONE', #61353 ) ;
#11547 = ORIENTED_EDGE ( 'NONE', *, *, #60377, .T. ) ;
#11548 = SHAPE_REPRESENTATION_RELATIONSHIP ( 'NONE' , 'NONE' ,  #51769, #4129 ) ;
#11549 = AXIS2_PLACEMENT_3D ( 'NONE', #15547, #56141, #4660 ) ;
#11550 = DIRECTION ( 'NONE',  ( -1.000000000000000000, -0.000000000000000000, -0.000000000000000000 ) ) ;
#11551 = VECTOR ( 'NONE', #49836, 1000.000000000000000 ) ;
#11552 = DIRECTION ( 'NONE',  ( 1.000000000000000000, -3.061616997868382648E-16, -0.000000000000000000 ) ) ;
#11553 = CARTESIAN_POINT ( 'NONE',  ( 96.32499999999998863, -212.2949673200287179, 76.95604166840095672 ) ) ;
#11554 = CARTESIAN_POINT ( 'NONE',  ( 92.34999999999999432, 91.52997821335252127, 79.15208333333332291 ) ) ;
#11555 = ORIENTED_EDGE ( 'NONE', *, *, #8247, .F. ) ;
#11556 = CARTESIAN_POINT ( 'NONE',  ( 0.000000000000000000, 0.000000000000000000, -20.00000000000000000 ) ) ;
#11557 = VERTEX_POINT ( 'NONE', #72241 ) ;
#11558 = ADVANCED_FACE ( 'NONE', ( #33126 ), #38039, .F. ) ;
#11559 = DIRECTION ( 'NONE',  ( -1.000000000000000000, 0.000000000000000000, 0.000000000000000000 ) ) ;
#11560 = ADVANCED_FACE ( 'NONE', ( #26385, #43337, #10569 ), #49312, .T. ) ;
#11561 = AXIS2_PLACEMENT_3D ( 'NONE', #63588, #63952, #34619 ) ;
#11562 = VERTEX_POINT ( 'NONE', #66616 ) ;
#11563 = CARTESIAN_POINT ( 'NONE',  ( -93.84685191531252713, 88.00268892867056536, 81.12322916753382174 ) ) ;
#11564 = CARTESIAN_POINT ( 'NONE',  ( 97.30629616937498838, 90.00000000000002842, 79.80031250086713612 ) ) ;
#11565 = VERTEX_POINT ( 'NONE', #66257 ) ;
#11566 = CARTESIAN_POINT ( 'NONE',  ( 0.000000000000000000, 76.41127070299273782, 12.93880638057342836 ) ) ;
#11567 = DIRECTION ( 'NONE',  ( 1.000000000000000000, 0.000000000000000000, 0.000000000000000000 ) ) ;
#11568 = DIRECTION ( 'NONE',  ( 0.000000000000000000, -0.9723699203976789995, 0.2334453638558956767 ) ) ;
#11569 = CARTESIAN_POINT ( 'NONE',  ( 0.000000000000000000, -34.94270380257693631, 74.18225833017875459 ) ) ;
#11570 = ORIENTED_EDGE ( 'NONE', *, *, #38959, .T. ) ;
#11571 = LINE ( 'NONE', #29589, #37497 ) ;
#11572 = CARTESIAN_POINT ( 'NONE',  ( -93.84685191531247028, -211.9973110713294489, 77.78947916753381264 ) ) ;
#11573 = ORIENTED_EDGE ( 'NONE', *, *, #34441, .F. ) ;
#11574 = ORIENTED_EDGE ( 'NONE', *, *, #37944, .F. ) ;
#11575 = CARTESIAN_POINT ( 'NONE',  ( -62.50000000000000000, 7.654042494670957804E-15, -184.9999999999999432 ) ) ;
#11576 = VERTEX_POINT ( 'NONE', #21858 ) ;
#11577 = DIRECTION ( 'NONE',  ( -1.000000000000000000, -0.000000000000000000, -0.000000000000000000 ) ) ;
#11578 = CARTESIAN_POINT ( 'NONE',  ( -92.34999999999999432, -209.9999999999999716, 78.25249999999999773 ) ) ;
#11579 = VERTEX_POINT ( 'NONE', #60616 ) ;
#11580 = CARTESIAN_POINT ( 'NONE',  ( -96.15314808468747287, -208.0026889286704943, 77.47197916753380298 ) ) ;
#11581 = EDGE_LOOP ( 'NONE', ( #36283, #61980, #49377, #3449 ) ) ;
#11582 = DIRECTION ( 'NONE',  ( 0.000000000000000000, 0.9876883405951381034, -0.1564344650402276216 ) ) ;
#11583 = LINE ( 'NONE', #17243, #74062 ) ;
#11584 = DIRECTION ( 'NONE',  ( -1.000000000000000000, -1.343011723336883198E-16, 0.000000000000000000 ) ) ;
#11585 = ORIENTED_EDGE ( 'NONE', *, *, #73993, .T. ) ;
#11586 = CARTESIAN_POINT ( 'NONE',  ( 10.00000000000000000, 21.32104025579158701, -30.84782396557194772 ) ) ;
#11587 = CLOSED_SHELL ( 'NONE', ( #54893, #46543, #73347, #56205, #72733, #44152, #49656, #69832, #10426, #16377, #47424, #31562, #45234, #72280, #17641, #63496, #8301, #70527, #54217, #22752, #25823, #3154, #42387, #17499, #45374, #22535, #32315, #64955, #70601, #46203, #317, #44578, #29512, #60801, #11043 ) ) ;
#11588 = CARTESIAN_POINT ( 'NONE',  ( 92.69370383062498320, 90.00000000000002842, 84.56281250086713897 ) ) ;
#11589 = LINE ( 'NONE', #34168, #12361 ) ;
#11590 = CARTESIAN_POINT ( 'NONE',  ( -93.67500000000003979, 87.70503267997129626, 88.30666666666665776 ) ) ;
#11591 = CARTESIAN_POINT ( 'NONE',  ( 0.000000000000000000, -29.81001611431024045, 22.74946021919122430 ) ) ;
#11592 = CARTESIAN_POINT ( 'NONE',  ( -4.999999999999999112, 1.831554690317574341, -1.158389257021580576 ) ) ;
#11593 = FACE_BOUND ( 'NONE', #62231, .T. ) ;
#11594 = CARTESIAN_POINT ( 'NONE',  ( 3.101151694651712809, 3.983051926191225611, -0.6020238742160355372 ) ) ;
#11595 = DIRECTION ( 'NONE',  ( 0.000000000000000000, -0.4067366430758009854, 0.9135454576426004225 ) ) ;
#11596 = CIRCLE ( 'NONE', #33163, 12.50000000000000000 ) ;
#11597 = CARTESIAN_POINT ( 'NONE',  ( 94.99999999999998579, 86.94004357329502852, 78.72875000000001933 ) ) ;
#11598 = EDGE_CURVE ( 'NONE', #16867, #56779, #15473, .T. ) ;
#11599 = AXIS2_PLACEMENT_3D ( 'NONE', #51592, #1252, #69980 ) ;
#11600 = DIRECTION ( 'NONE',  ( 1.000000000000000000, -0.000000000000000000, -0.000000000000000000 ) ) ;
#11601 = CARTESIAN_POINT ( 'NONE',  ( -96.15314808468751551, 88.00268892867056536, 88.47864583420047779 ) ) ;
#11602 = DIRECTION ( 'NONE',  ( -0.000000000000000000, -0.000000000000000000, -1.000000000000000000 ) ) ;
#11603 = ADVANCED_FACE ( 'NONE', ( #9837 ), #67351, .T. ) ;
#11604 = AXIS2_PLACEMENT_3D ( 'NONE', #10778, #10402, #57382 ) ;
#11605 = ADVANCED_FACE ( 'NONE', ( #67728 ), #16216, .T. ) ;
#11606 = CARTESIAN_POINT ( 'NONE',  ( 10.00000000000000000, 0.000000000000000000, 0.000000000000000000 ) ) ;
#11607 = PRODUCT_DEFINITION_SHAPE ( 'NONE', 'NONE',  #74360 ) ;
#11608 = DIRECTION ( 'NONE',  ( 1.000000000000000000, 0.000000000000000000, 0.000000000000000000 ) ) ;
#11609 = DIRECTION ( 'NONE',  ( -1.000000000000000000, -0.000000000000000000, -0.000000000000000000 ) ) ;
#11610 = FILL_AREA_STYLE_COLOUR ( '', #38310 ) ;
#11611 = DIRECTION ( 'NONE',  ( 0.000000000000000000, 0.000000000000000000, 1.000000000000000000 ) ) ;
#11612 = EDGE_CURVE ( 'NONE', #43494, #1463, #36031, .T. ) ;
#11613 = DIRECTION ( 'NONE',  ( -1.000000000000000000, 0.000000000000000000, 0.000000000000000000 ) ) ;
#11614 = CARTESIAN_POINT ( 'NONE',  ( 97.30629616937498838, -209.9999999999999716, 86.94406250086716170 ) ) ;
#11615 = CIRCLE ( 'NONE', #38081, 32.00000000000000000 ) ;
#11616 = ORIENTED_EDGE ( 'NONE', *, *, #63442, .T. ) ;
#11617 = EDGE_LOOP ( 'NONE', ( #7884, #69963, #23591, #45824 ) ) ;
#11618 = AXIS2_PLACEMENT_3D ( 'NONE', #74136, #10994, #57966 ) ;
#11619 = CARTESIAN_POINT ( 'NONE',  ( 92.34999999999999432, 90.00000000000002842, 90.00000000000000000 ) ) ;
#11620 = ORIENTED_EDGE ( 'NONE', *, *, #60544, .F. ) ;
#11621 = ADVANCED_FACE ( 'NONE', ( #5333 ), #33880, .T. ) ;
#11622 = CARTESIAN_POINT ( 'NONE',  ( 10.00000000000000000, -37.01155633439053361, -6.555932627142825986 ) ) ;
#11623 = CARTESIAN_POINT ( 'NONE',  ( 93.84685191531251292, -211.9973110713294489, 79.58864583420047722 ) ) ;
#11625 = EDGE_LOOP ( 'NONE', ( #69829, #68459, #13767, #64291, #68604, #10932, #28489, #60152, #25452, #61000, #7114, #63933, #21051, #41615, #33359, #30341, #53639, #64074, #62983, #16200, #135, #62453, #16758, #50826, #3871, #65365, #48809, #41419, #56696, #36976, #73571, #29929, #10710, #7019, #51069, #46147, #67338, #1741, #30296, #72460, #40167, #31792, #11048, #41782, #26718, #33387, #64919, #41004, #47835, #70325 ) ) ;
#11624 = ADVANCED_FACE ( 'NONE', ( #28231 ), #11674, .F. ) ;
#11626 = CARTESIAN_POINT ( 'NONE',  ( 95.00000000000000000, -207.3369185715606307, 82.65781250086715204 ) ) ;
#11627 = ORIENTED_EDGE ( 'NONE', *, *, #35030, .F. ) ;
#11628 = DIRECTION ( 'NONE',  ( -1.000000000000000000, -1.427937372958405461E-15, -7.962523111839130290E-16 ) ) ;
#11629 = ORIENTED_EDGE ( 'NONE', *, *, #46112, .T. ) ;
#11630 = EDGE_CURVE ( 'NONE', #23395, #55194, #45920, .T. ) ;
#11631 = EDGE_CURVE ( 'NONE', #7862, #19038, #3702, .T. ) ;
#11632 = EDGE_LOOP ( 'NONE', ( #73612, #69824, #60299 ) ) ;
#11633 = DIRECTION ( 'NONE',  ( 1.000000000000000000, 0.000000000000000000, 0.000000000000000000 ) ) ;
#11634 = CARTESIAN_POINT ( 'NONE',  ( 10.00000000000000000, 36.88895765772642932, -6.736453364083163642 ) ) ;
#11635 = ORIENTED_EDGE ( 'NONE', *, *, #12276, .T. ) ;
#11636 = PLANE ( 'NONE',  #55714 ) ;
#11637 = CARTESIAN_POINT ( 'NONE',  ( 96.32499999999998863, -212.2949673200287179, 87.75104166840095843 ) ) ;
#11638 = VERTEX_POINT ( 'NONE', #12057 ) ;
#11639 = FACE_OUTER_BOUND ( 'NONE', #63348, .T. ) ;
#11640 = EDGE_CURVE ( 'NONE', #23659, #13520, #43100, .T. ) ;
#11641 = EDGE_LOOP ( 'NONE', ( #29931, #23328, #26687, #73212 ) ) ;
#11642 = CARTESIAN_POINT ( 'NONE',  ( 11.99999999999999822, 0.000000000000000000, 0.000000000000000000 ) ) ;
#11643 = AXIS2_PLACEMENT_3D ( 'NONE', #34520, #57467, #5608 ) ;
#11644 = ORIENTED_EDGE ( 'NONE', *, *, #53135, .F. ) ;
#11645 = AXIS2_PLACEMENT_3D ( 'NONE', #44314, #66508, #38676 ) ;
#11646 = ADVANCED_FACE ( 'NONE', ( #46644 ), #17700, .T. ) ;
#11647 = VERTEX_POINT ( 'NONE', #45174 ) ;
#11648 = VERTEX_POINT ( 'NONE', #6436 ) ;
#11649 = PLANE ( 'NONE',  #63311 ) ;
#11650 = DIRECTION ( 'NONE',  ( -1.000000000000000000, -0.000000000000000000, 0.000000000000000000 ) ) ;
#11651 = ORIENTED_EDGE ( 'NONE', *, *, #27940, .T. ) ;
#11652 = ORIENTED_EDGE ( 'NONE', *, *, #57732, .F. ) ;
#11653 = VECTOR ( 'NONE', #57559, 1000.000000000000000 ) ;
#11654 = ORIENTED_EDGE ( 'NONE', *, *, #17745, .T. ) ;
#11655 = CIRCLE ( 'NONE', #8075, 35.50000000000000711 ) ;
#11656 = DIRECTION ( 'NONE',  ( 0.000000000000000000, 0.000000000000000000, 1.000000000000000000 ) ) ;
#11657 = DIRECTION ( 'NONE',  ( 0.000000000000000000, 0.000000000000000000, 1.000000000000000000 ) ) ;
#11658 = CARTESIAN_POINT ( 'NONE',  ( -92.35000000000005116, 91.52997821335253548, 87.19541666666667368 ) ) ;
#11659 = ORIENTED_EDGE ( 'NONE', *, *, #71967, .F. ) ;
#11660 = CARTESIAN_POINT ( 'NONE',  ( 97.30629616937497417, 89.06968361095755427, 74.68334086212732359 ) ) ;
#11661 = AXIS2_PLACEMENT_3D ( 'NONE', #57214, #41038, #29356 ) ;
#11662 =( BOUNDED_CURVE ( )  B_SPLINE_CURVE ( 2, ( #72430, #44629, #33701, #10025, #38608, #55148, #56655, #49867, #22052 ),
 .UNSPECIFIED., .F., .F. ) 
 B_SPLINE_CURVE_WITH_KNOTS ( ( 3, 2, 2, 2, 3 ),
 ( 0.4868478063929146393, 0.4939035878617654141, 0.5009593534026473005, 0.5080151189435291315, 0.5080151867253831499 ),
 .UNSPECIFIED. ) 
 CURVE ( )  GEOMETRIC_REPRESENTATION_ITEM ( )  RATIONAL_B_SPLINE_CURVE ( ( 1.000000000000000000, 0.8660254037844387076, 1.000000000000000000, 0.8660254037844387076, 1.000000000000000000, 0.8660254037844387076, 1.000000000000000000, 0.9999987129608440828, 0.9999974259464162740 ) ) 
 REPRESENTATION_ITEM ( '' )  );
#11663 = ORIENTED_EDGE ( 'NONE', *, *, #46683, .T. ) ;
#11664 = DIRECTION ( 'NONE',  ( -1.000000000000000000, -0.000000000000000000, -0.000000000000000000 ) ) ;
#11665 = CARTESIAN_POINT ( 'NONE',  ( -97.30629616937495996, -209.9999999999999716, 86.46781250086714010 ) ) ;
#11666 = ORIENTED_EDGE ( 'NONE', *, *, #57368, .T. ) ;
#11667 = CARTESIAN_POINT ( 'NONE',  ( 92.35000000006147047, -209.9999881782113107, 76.10900611559200968 ) ) ;
#11668 = DIRECTION ( 'NONE',  ( -1.000000000000000000, 0.000000000000000000, 0.000000000000000000 ) ) ;
#11669 = LINE ( 'NONE', #74090, #3325 ) ;
#11670 = CARTESIAN_POINT ( 'NONE',  ( -96.15314808468745866, -211.9973110713294489, 75.14364583420046984 ) ) ;
#11671 = DIRECTION ( 'NONE',  ( 1.000000000000000000, 0.000000000000000000, 0.000000000000000000 ) ) ;
#11672 = CARTESIAN_POINT ( 'NONE',  ( 11.99999999999999822, 39.47590169984944453, -71.87247863392373404 ) ) ;
#11673 = VECTOR ( 'NONE', #66753, 1000.000000000000114 ) ;
#11674 = PLANE ( 'NONE',  #61273 ) ;
#11675 = DIRECTION ( 'NONE',  ( 0.000000000000000000, -0.9945218953682730678, -0.1045284632676570929 ) ) ;
#11676 = VECTOR ( 'NONE', #70627, 1000.000000000000227 ) ;
#11677 = DIRECTION ( 'NONE',  ( -1.000000000000000000, 0.000000000000000000, -0.000000000000000000 ) ) ;
#11678 = CARTESIAN_POINT ( 'NONE',  ( -93.84685191531252713, 88.00268892867056536, 79.69447916753379957 ) ) ;
#11679 = DIRECTION ( 'NONE',  ( -1.000000000000000000, 0.000000000000000000, -0.000000000000000000 ) ) ;
#11680 = LINE ( 'NONE', #35003, #68672 ) ;
#11681 = ORIENTED_EDGE ( 'NONE', *, *, #50154, .F. ) ;
#11682 = CARTESIAN_POINT ( 'NONE',  ( -96.32499999999996021, -207.7050326799711968, 80.44854166840097776 ) ) ;
#11683 = EDGE_CURVE ( 'NONE', #47235, #12105, #823, .T. ) ;
#11684 = PLANE ( 'NONE',  #67701 ) ;
#11685 = DIRECTION ( 'NONE',  ( 0.7533909544171997208, 0.6575728627325956310, -6.162975822039155825E-32 ) ) ;
#11686 = DIRECTION ( 'NONE',  ( -1.000000000000000000, 0.000000000000000000, 0.000000000000000000 ) ) ;
#11687 = EDGE_CURVE ( 'NONE', #37410, #38445, #58293, .T. ) ;
#11688 = CARTESIAN_POINT ( 'NONE',  ( 97.64999999999999147, -210.0000000024471092, 75.15687493081163950 ) ) ;
#11689 = CARTESIAN_POINT ( 'NONE',  ( -97.65000000000001990, 91.52997821335253548, 85.58145833506763722 ) ) ;
#11690 = CARTESIAN_POINT ( 'NONE',  ( -97.30629616937495996, -209.9999999999999716, 77.73656250086715147 ) ) ;
#11691 = EDGE_CURVE ( 'NONE', #64991, #26264, #58966, .T. ) ;
#11692 = ADVANCED_FACE ( 'NONE', ( #52650 ), #28599, .T. ) ;
#11693 = LINE ( 'NONE', #23371, #8081 ) ;
#11694 = ORIENTED_EDGE ( 'NONE', *, *, #42475, .T. ) ;
#11695 = MECHANICAL_DESIGN_GEOMETRIC_PRESENTATION_REPRESENTATION (  '', ( #51307 ), #56094 ) ;
#11696 = DIRECTION ( 'NONE',  ( 1.000000000000000000, 1.427937372958405461E-15, 7.962523111839130290E-16 ) ) ;
#11697 = DIRECTION ( 'NONE',  ( -1.000000000000000000, -0.000000000000000000, 0.000000000000000000 ) ) ;
#11698 = DIRECTION ( 'NONE',  ( 1.000000000000000000, 0.000000000000000000, 0.000000000000000000 ) ) ;
#11699 = AXIS2_PLACEMENT_3D ( 'NONE', #20577, #43530, #27305 ) ;
#11700 = CARTESIAN_POINT ( 'NONE',  ( 11.99999999999999822, 75.11764819372149304, -2.946379043146603482 ) ) ;
#11701 = VECTOR ( 'NONE', #74002, 1000.000000000000114 ) ;
#11702 = CIRCLE ( 'NONE', #71705, 77.49899999999999523 ) ;
#11703 = DIRECTION ( 'NONE',  ( 1.000000000000000000, 0.000000000000000000, 0.000000000000000000 ) ) ;
#11704 = ADVANCED_FACE ( 'NONE', ( #69575 ), #46278, .T. ) ;
#11705 = VERTEX_POINT ( 'NONE', #10955 ) ;
#11706 = CYLINDRICAL_SURFACE ( 'NONE', #15667, 42.00000000000000000 ) ;
#11707 = FACE_OUTER_BOUND ( 'NONE', #40806, .T. ) ;
#11708 = ORIENTED_EDGE ( 'NONE', *, *, #39297, .T. ) ;
#11709 = PLANE ( 'NONE',  #59214 ) ;
#11710 = CARTESIAN_POINT ( 'NONE',  ( -92.35000000000678710, 90.00000598221780024, 82.14187520865721126 ) ) ;
#11711 = EDGE_LOOP ( 'NONE', ( #67859, #51492, #37051, #59385 ) ) ;
#11712 = DIRECTION ( 'NONE',  ( -1.000000000000000000, -0.000000000000000000, -0.000000000000000000 ) ) ;
#11713 = ORIENTED_EDGE ( 'NONE', *, *, #32433, .F. ) ;
#11714 = CYLINDRICAL_SURFACE ( 'NONE', #59898, 32.00000000000000000 ) ;
#11715 = EDGE_LOOP ( 'NONE', ( #39295, #19957, #20345, #70538 ) ) ;
#11716 = EDGE_CURVE ( 'NONE', #12834, #29431, #14504, .T. ) ;
#11717 = ADVANCED_FACE ( 'NONE', ( #22608 ), #16967, .T. ) ;
#11718 = CARTESIAN_POINT ( 'NONE',  ( 10.00000000000000000, 0.000000000000000000, 0.000000000000000000 ) ) ;
#11719 = VECTOR ( 'NONE', #32154, 1000.000000000000000 ) ;
#11720 = ORIENTED_EDGE ( 'NONE', *, *, #73856, .F. ) ;
#11721 = DIRECTION ( 'NONE',  ( 0.000000000000000000, 0.000000000000000000, 1.000000000000000000 ) ) ;
#11722 = VERTEX_POINT ( 'NONE', #47387 ) ;
#11723 = VERTEX_POINT ( 'NONE', #65427 ) ;
#11724 = DIRECTION ( 'NONE',  ( -0.000000000000000000, -0.000000000000000000, -1.000000000000000000 ) ) ;
#11725 = VECTOR ( 'NONE', #14742, 1000.000000000000000 ) ;
#11726 = ORIENTED_EDGE ( 'NONE', *, *, #72901, .F. ) ;
#11727 = VERTEX_POINT ( 'NONE', #47021 ) ;
#11728 = VECTOR ( 'NONE', #73744, 1000.000000000000000 ) ;
#11729 = CARTESIAN_POINT ( 'NONE',  ( 92.48104893696866213, 89.82936612246388108, 74.92125785461007581 ) ) ;
#11730 = ORIENTED_EDGE ( 'NONE', *, *, #66893, .F. ) ;
#11731 = ORIENTED_EDGE ( 'NONE', *, *, #34449, .T. ) ;
#11732 = CARTESIAN_POINT ( 'NONE',  ( 96.15314808468748708, 91.99731107132950569, 84.35114583420048007 ) ) ;
#11733 = ORIENTED_EDGE ( 'NONE', *, *, #41079, .T. ) ;
#11734 = CARTESIAN_POINT ( 'NONE',  ( 96.15314808468750130, -211.9973110713294489, 82.86947916753379673 ) ) ;
#11735 = APPLICATION_PROTOCOL_DEFINITION ( 'draft international standard', 'automotive_design', 1998, #52686 ) ;
#11736 = CARTESIAN_POINT ( 'NONE',  ( 11.99999999999999822, 62.50329211542435104, 41.76937507738811917 ) ) ;
#11737 = DIRECTION ( 'NONE',  ( 0.000000000000000000, 0.000000000000000000, 1.000000000000000000 ) ) ;
#11738 = CARTESIAN_POINT ( 'NONE',  ( -97.64999999999996305, -209.9999999999999716, 90.00000000000000000 ) ) ;
#11739 = CYLINDRICAL_SURFACE ( 'NONE', #10386, 2.649999999999999467 ) ;
#11740 = DIRECTION ( 'NONE',  ( 1.000000000000000000, -0.000000000000000000, -0.000000000000000000 ) ) ;
#11741 = DIRECTION ( 'NONE',  ( -0.7950889364178796992, 0.6064928550163511956, 0.000000000000000000 ) ) ;
#11742 = CARTESIAN_POINT ( 'NONE',  ( -93.84685191531247028, -211.9973110713294489, 84.13947916753380696 ) ) ;
#11743 = CARTESIAN_POINT ( 'NONE',  ( -96.15314808468751551, 88.00268892867056536, 83.55739583420049144 ) ) ;
#11744 = VERTEX_POINT ( 'NONE', #7533 ) ;
#11746 = CARTESIAN_POINT ( 'NONE',  ( -92.69370383062502583, 91.33154071421968467, 83.66322916753379957 ) ) ;
#11745 = CARTESIAN_POINT ( 'NONE',  ( 92.69370383062498320, 90.00000000000002842, 83.92781250086714806 ) ) ;
#11747 = EDGE_LOOP ( 'NONE', ( #23670, #47518, #39278, #55192 ) ) ;
#11748 = CARTESIAN_POINT ( 'NONE',  ( -97.64999999989197477, 90.00001510551047090, 78.64888723592453346 ) ) ;
#11749 = CIRCLE ( 'NONE', #64576, 42.00000000000000000 ) ;
#11750 = DIRECTION ( 'NONE',  ( 1.000000000000000000, 0.000000000000000000, 0.000000000000000000 ) ) ;
#11751 = DIRECTION ( 'NONE',  ( -1.000000000000000000, -0.000000000000000000, 0.000000000000000000 ) ) ;
#11752 = CARTESIAN_POINT ( 'NONE',  ( 97.64999999999997726, 91.52997821335254969, 87.19541666666667368 ) ) ;
#11753 = CARTESIAN_POINT ( 'NONE',  ( -97.30629616937497417, -208.6684592857803295, 85.77989583420048803 ) ) ;
#11754 = CIRCLE ( 'NONE', #25016, 77.49899999999999523 ) ;
#11755 = CARTESIAN_POINT ( 'NONE',  ( 0.000000000000000000, 8.830959090343430518, -74.65491531819107252 ) ) ;
#11756 = DIRECTION ( 'NONE',  ( -1.000000000000000000, 0.000000000000000000, -0.000000000000000000 ) ) ;
#11757 = CARTESIAN_POINT ( 'NONE',  ( 10.00000000000000000, -33.00180498840060039, 17.80606268964528027 ) ) ;
#11758 = CARTESIAN_POINT ( 'NONE',  ( 97.64999999999999147, 90.00000000000002842, 80.15749999999999886 ) ) ;
#11759 = ORIENTED_EDGE ( 'NONE', *, *, #33183, .T. ) ;
#11760 = VERTEX_POINT ( 'NONE', #54141 ) ;
#11761 = AXIS2_PLACEMENT_3D ( 'NONE', #23367, #6089, #40280 ) ;
#11762 = CARTESIAN_POINT ( 'NONE',  ( -92.35000000000003695, 90.00000000000004263, 76.98250000000000171 ) ) ;
#11763 = CARTESIAN_POINT ( 'NONE',  ( -96.32499999999996021, -212.2949673200287179, 78.67583333333332973 ) ) ;
#11764 = DIRECTION ( 'NONE',  ( 0.000000000000000000, -0.8910065241883723397, 0.4539904997395382003 ) ) ;
#11765 = CYLINDRICAL_SURFACE ( 'NONE', #33776, 82.00000000000000000 ) ;
#11766 = FACE_OUTER_BOUND ( 'NONE', #41171, .T. ) ;
#11767 = CARTESIAN_POINT ( 'NONE',  ( 92.35000000000000853, -208.4700217866474645, 77.96145833506763267 ) ) ;
#11768 = DIRECTION ( 'NONE',  ( -0.6064928550163533050, -0.7950889364178781449, 0.000000000000000000 ) ) ;
#11769 = ORIENTED_EDGE ( 'NONE', *, *, #19014, .T. ) ;
#11770 = CARTESIAN_POINT ( 'NONE',  ( -93.84685191531252713, 88.00268892867056536, 79.69447916753379957 ) ) ;
#11771 = ADVANCED_FACE ( 'NONE', ( #30446 ), #18434, .T. ) ;
#11772 = DIRECTION ( 'NONE',  ( 0.000000000000000000, -0.9945218953682742891, -0.1045284632676436315 ) ) ;
#11773 = EDGE_CURVE ( 'NONE', #15290, #39348, #13891, .T. ) ;
#11774 = DIRECTION ( 'NONE',  ( 1.000000000000000000, -0.000000000000000000, -0.000000000000000000 ) ) ;
#11775 = AXIS2_PLACEMENT_3D ( 'NONE', #19225, #65480, #13217 ) ;
#11776 = CARTESIAN_POINT ( 'NONE',  ( 0.000000000000000000, 0.000000000000000000, 52.00000000000002132 ) ) ;
#11777 = ADVANCED_FACE ( 'NONE', ( #13534 ), #48492, .T. ) ;
#11778 = LINE ( 'NONE', #200, #33278 ) ;
#11779 = AXIS2_PLACEMENT_3D ( 'NONE', #23194, #39749, #22449 ) ;
#11780 = CARTESIAN_POINT ( 'NONE',  ( 0.000000000000000000, 40.65526001592713357, -71.21200624218752750 ) ) ;
#11781 = CARTESIAN_POINT ( 'NONE',  ( -92.69370383062498320, -209.9999999999999716, 88.21406250086714351 ) ) ;
#11782 = CIRCLE ( 'NONE', #34598, 15.70000000000326956 ) ;
#11783 = ADVANCED_FACE ( 'NONE', ( #14270 ), #7894, .F. ) ;
#11784 = ADVANCED_FACE ( 'NONE', ( #42856 ), #71404, .T. ) ;
#11785 = MANIFOLD_SOLID_BREP ( 'EndChamfer', #46382 ) ;
#11786 = CARTESIAN_POINT ( 'NONE',  ( 97.30629616937498838, 91.33154071421968467, 76.20197916753382117 ) ) ;
#11787 = CARTESIAN_POINT ( 'NONE',  ( -92.69370383062498320, -211.3315407142195852, 79.90614583420048689 ) ) ;
#11788 = CYLINDRICAL_SURFACE ( 'NONE', #15814, 77.49899999999999523 ) ;
#11789 = ORIENTED_EDGE ( 'NONE', *, *, #58297, .T. ) ;
#11790 = LINE ( 'NONE', #51663, #66522 ) ;
#11791 = CARTESIAN_POINT ( 'NONE',  ( 5.250000000000000000, -13.95926121303099343, -1.199999999999999956 ) ) ;
#11792 = CARTESIAN_POINT ( 'NONE',  ( 95.00000000000000000, -213.0599564267049857, 78.80812500173429669 ) ) ;
#11793 = CYLINDRICAL_SURFACE ( 'NONE', #36104, 42.00000000000000000 ) ;
#11795 = EDGE_CURVE ( 'NONE', #70536, #62068, #8263, .T. ) ;
#11794 = CARTESIAN_POINT ( 'NONE',  ( 96.15314808468748708, -208.0026889286704943, 75.46114583420047950 ) ) ;
#11796 = ORIENTED_EDGE ( 'NONE', *, *, #16762, .F. ) ;
#11797 = EDGE_CURVE ( 'NONE', #1624, #6579, #30120, .T. ) ;
#11798 = CARTESIAN_POINT ( 'NONE',  ( -97.65000000000001990, 90.00000000000004263, 75.39499999999999602 ) ) ;
#11799 = EDGE_LOOP ( 'NONE', ( #19878, #64626, #27386, #6020 ) ) ;
#11800 = PLANE ( 'NONE',  #71154 ) ;
#11801 = ORIENTED_EDGE ( 'NONE', *, *, #25029, .F. ) ;
#11802 = AXIS2_PLACEMENT_3D ( 'NONE', #3132, #14743, #65903 ) ;
#11803 = CIRCLE ( 'NONE', #3472, 77.49899999999999523 ) ;
#11804 = CARTESIAN_POINT ( 'NONE',  ( -42.50000000000000000, 0.000000000000000000, 0.000000000000000000 ) ) ;
#11805 = EDGE_CURVE ( 'NONE', #42720, #24576, #26488, .T. ) ;
#11806 = EDGE_CURVE ( 'NONE', #65637, #48516, #4933, .T. ) ;
#11807 = AXIS2_PLACEMENT_3D ( 'NONE', #56465, #55334, #27872 ) ;
#11808 = EDGE_LOOP ( 'NONE', ( #3901, #4195, #43087, #31901 ) ) ;
#11809 = EDGE_LOOP ( 'NONE', ( #28088, #18874, #71463, #14028 ) ) ;
#11810 = AXIS2_PLACEMENT_3D ( 'NONE', #63786, #50628, #12261 ) ;
#11811 = VERTEX_POINT ( 'NONE', #42124 ) ;
#11812 = CARTESIAN_POINT ( 'NONE',  ( 10.00000000000000000, 12.42422080174639021, 35.38097989696516521 ) ) ;
#11813 = ORIENTED_EDGE ( 'NONE', *, *, #3119, .T. ) ;
#11814 = ORIENTED_EDGE ( 'NONE', *, *, #12912, .F. ) ;
#11815 = CARTESIAN_POINT ( 'NONE',  ( 97.30629616937498838, 88.66845928578037217, 83.08114583420048405 ) ) ;
#11816 = DIRECTION ( 'NONE',  ( -1.000000000000000000, 0.000000000000000000, 0.000000000000000000 ) ) ;
#11817 = VERTEX_POINT ( 'NONE', #65060 ) ;
#11819 = ORIENTED_EDGE ( 'NONE', *, *, #41908, .T. ) ;
#11818 = AXIS2_PLACEMENT_3D ( 'NONE', #53513, #47141, #36582 ) ;
#11820 = ORIENTED_EDGE ( 'NONE', *, *, #4954, .F. ) ;
#11821 = VERTEX_POINT ( 'NONE', #59407 ) ;
#11822 =( NAMED_UNIT ( * ) SI_UNIT ( $, .STERADIAN. ) SOLID_ANGLE_UNIT ( ) );
#11823 = CIRCLE ( 'NONE', #53863, 31.99999999999998579 ) ;
#11824 = DIRECTION ( 'NONE',  ( -0.3373011080932099559, -0.9413968145681674837, -0.000000000000000000 ) ) ;
#11825 = CARTESIAN_POINT ( 'NONE',  ( -0.0004442498525516064278, 0.001194404164626844313, -64.00000000000000000 ) ) ;
#11826 = CARTESIAN_POINT ( 'NONE',  ( -3.000000000000000000, 8.688484142254221609, -21.88630264137359660 ) ) ;
#11827 = CARTESIAN_POINT ( 'NONE',  ( 2.426025403784448642, 2.168404344971008868E-16, 0.000000000000000000 ) ) ;
#11828 = PLANE ( 'NONE',  #17451 ) ;
#11829 = DIRECTION ( 'NONE',  ( 1.000000000000000000, 0.000000000000000000, 0.000000000000000000 ) ) ;
#11830 = VECTOR ( 'NONE', #1607, 1000.000000000000000 ) ;
#11831 = CARTESIAN_POINT ( 'NONE',  ( 5.999999999999999112, -55.16347631942998930, -60.67117009219195722 ) ) ;
#11832 = CIRCLE ( 'NONE', #69491, 4.750000000000000000 ) ;
#11833 = VERTEX_POINT ( 'NONE', #44337 ) ;
#11834 = CARTESIAN_POINT ( 'NONE',  ( -96.32499999999996021, -207.7050326799711968, 79.17854166840096752 ) ) ;
#11835 = VERTEX_POINT ( 'NONE', #44719 ) ;
#11836 = FACE_OUTER_BOUND ( 'NONE', #54127, .T. ) ;
#11837 = ORIENTED_EDGE ( 'NONE', *, *, #24751, .T. ) ;
#11839 = CARTESIAN_POINT ( 'NONE',  ( -97.65000000000001990, 88.47002178664754979, 80.60729166840097548 ) ) ;
#11838 = CARTESIAN_POINT ( 'NONE',  ( 94.99999999999998579, 93.05995642670504253, 78.49062500173430124 ) ) ;
#11840 = VECTOR ( 'NONE', #3245, 1000.000000000000000 ) ;
#11841 = ORIENTED_EDGE ( 'NONE', *, *, #3857, .T. ) ;
#11842 = CARTESIAN_POINT ( 'NONE',  ( 94.99999999999998579, 92.66308142843935514, 81.38781250086715602 ) ) ;
#11843 = DIRECTION ( 'NONE',  ( 0.000000000000000000, 0.8090169943749498938, 0.5877852522924696954 ) ) ;
#11845 = ADVANCED_FACE ( 'NONE', ( #67637 ), #66530, .F. ) ;
#11844 = FACE_OUTER_BOUND ( 'NONE', #29116, .T. ) ;
#11846 = DIRECTION ( 'NONE',  ( 0.000000000000000000, -9.787530781167598712E-16, -1.000000000000000000 ) ) ;
#11847 = CARTESIAN_POINT ( 'NONE',  ( 10.00000000000000000, 37.01155633439059756, 6.555932627142549762 ) ) ;
#11848 = ORIENTED_EDGE ( 'NONE', *, *, #61730, .T. ) ;
#11849 = DIRECTION ( 'NONE',  ( 0.000000000000000000, 0.4539904997395479702, -0.8910065241883673437 ) ) ;
#11850 = CARTESIAN_POINT ( 'NONE',  ( 19.12409105625795291, -101.5943176906707919, 5.500000000000000000 ) ) ;
#11851 = DIRECTION ( 'NONE',  ( -1.000000000000000000, 0.000000000000000000, -0.000000000000000000 ) ) ;
#11852 = ORIENTED_EDGE ( 'NONE', *, *, #18104, .F. ) ;
#11853 = ORIENTED_EDGE ( 'NONE', *, *, #45769, .F. ) ;
#11854 = ADVANCED_FACE ( 'NONE', ( #15010 ), #21377, .F. ) ;
#11855 = EDGE_CURVE ( 'NONE', #15073, #69736, #68518, .T. ) ;
#11856 = CARTESIAN_POINT ( 'NONE',  ( 10.00000000000000000, -27.05870788708213226, -26.08949754953053102 ) ) ;
#11857 = EDGE_CURVE ( 'NONE', #63185, #50665, #26288, .T. ) ;
#11858 = DIRECTION ( 'NONE',  ( -1.000000000000000000, 0.000000000000000000, -0.000000000000000000 ) ) ;
#11859 = CARTESIAN_POINT ( 'NONE',  ( -93.09170270117142820, -211.8387227684682159, 74.99954709728268654 ) ) ;
#11860 = CARTESIAN_POINT ( 'NONE',  ( -94.99999999999997158, -207.3369185715606307, 78.21281250086717307 ) ) ;
#11861 = AXIS2_PLACEMENT_3D ( 'NONE', #45256, #16673, #39611 ) ;
#11862 = VERTEX_POINT ( 'NONE', #38697 ) ;
#11863 = CIRCLE ( 'NONE', #74292, 20.20000000000036522 ) ;
#11864 = AXIS2_PLACEMENT_3D ( 'NONE', #38713, #4516, #27414 ) ;
#11865 = EDGE_CURVE ( 'NONE', #60856, #22572, #37951, .T. ) ;
#11866 = DIRECTION ( 'NONE',  ( -1.000000000000000000, -0.000000000000000000, -0.000000000000000000 ) ) ;
#11867 = CARTESIAN_POINT ( 'NONE',  ( -96.91066463016758803, -211.7387787020483358, 74.95660481729511559 ) ) ;
#11868 = CIRCLE ( 'NONE', #15471, 16.00000000000000000 ) ;
#11869 = CARTESIAN_POINT ( 'NONE',  ( 0.000000000000000000, -74.74816331893404708, -33.71516098798818462 ) ) ;
#11870 = ADVANCED_FACE ( 'NONE', ( #16133 ), #60888, .T. ) ;
#11871 = CARTESIAN_POINT ( 'NONE',  ( 96.15314808468748708, 88.00268892867053694, 75.88447916753381151 ) ) ;
#11872 = VECTOR ( 'NONE', #478, 1000.000000000000227 ) ;
#11873 = FACE_OUTER_BOUND ( 'NONE', #29497, .T. ) ;
#11874 = CARTESIAN_POINT ( 'NONE',  ( 15.07208474345548055, -141.7963818439230010, -2.500000000000000000 ) ) ;
#11875 = DIRECTION ( 'NONE',  ( 1.000000000000000000, 0.000000000000000000, 0.000000000000000000 ) ) ;
#11876 = PLANE ( 'NONE',  #67656 ) ;
#11877 = CARTESIAN_POINT ( 'NONE',  ( -10.00000000000000000, 0.000000000000000000, 0.000000000000000000 ) ) ;
#11878 = CARTESIAN_POINT ( 'NONE',  ( -97.64999999999996305, -209.9999999999999716, 89.36499999999999488 ) ) ;
#11879 = EDGE_CURVE ( 'NONE', #71554, #43361, #32291, .T. ) ;
#11880 = CARTESIAN_POINT ( 'NONE',  ( 93.84685191531248449, 91.99731107132950569, 86.52072916753382970 ) ) ;
#11881 = VECTOR ( 'NONE', #44800, 1000.000000000000000 ) ;
#11882 = CARTESIAN_POINT ( 'NONE',  ( 10.00000000000000000, 0.000000000000000000, 0.000000000000000000 ) ) ;
#11883 = DIRECTION ( 'NONE',  ( 0.000000000000000000, -1.000000000000000000, -1.047444401652940007E-14 ) ) ;
#11884 = CIRCLE ( 'NONE', #53915, 16.00000000000000000 ) ;
#11885 = ORIENTED_EDGE ( 'NONE', *, *, #36425, .T. ) ;
#11886 = FACE_OUTER_BOUND ( 'NONE', #35700, .T. ) ;
#11887 = CARTESIAN_POINT ( 'NONE',  ( -97.30629616937501680, 91.33154071421968467, 81.33489583420048064 ) ) ;
#11888 = CIRCLE ( 'NONE', #44315, 16.00000000000000355 ) ;
#11889 = AXIS2_PLACEMENT_3D ( 'NONE', #24061, #48088, #70255 ) ;
#11890 = AXIS2_PLACEMENT_3D ( 'NONE', #8960, #72830, #21332 ) ;
#11891 = CIRCLE ( 'NONE', #53932, 13.90444123027096879 ) ;
#11893 = EDGE_CURVE ( 'NONE', #63185, #9070, #9932, .T. ) ;
#11892 = DIRECTION ( 'NONE',  ( 0.000000000000000000, 0.000000000000000000, 1.000000000000000000 ) ) ;
#11894 = EDGE_CURVE ( 'NONE', #70823, #8033, #55979, .T. ) ;
#11895 = ORIENTED_EDGE ( 'NONE', *, *, #64245, .T. ) ;
#11896 = AXIS2_PLACEMENT_3D ( 'NONE', #21703, #67574, #39008 ) ;
#11897 =( BOUNDED_CURVE ( )  B_SPLINE_CURVE ( 2, ( #47310, #70213, #59325, #7818, #35874, #41164, #52813 ),
 .UNSPECIFIED., .F., .F. ) 
 B_SPLINE_CURVE_WITH_KNOTS ( ( 3, 2, 2, 3 ),
 ( 0.3958333333333330373, 0.4027777777777774570, 0.4097222222222218768, 0.4166666666666662966 ),
 .UNSPECIFIED. ) 
 CURVE ( )  GEOMETRIC_REPRESENTATION_ITEM ( )  RATIONAL_B_SPLINE_CURVE ( ( 1.000000000000005329, 0.8660254037844333785, 1.000000000000000000, 0.8660254037844387076, 1.000000000000000000, 0.8660254037844462571, 0.9999999999999924505 ) ) 
 REPRESENTATION_ITEM ( '' )  );
#11898 = DIRECTION ( 'NONE',  ( -0.000000000000000000, -0.000000000000000000, 1.000000000000000000 ) ) ;
#11899 = EDGE_CURVE ( 'NONE', #34985, #56906, #27396, .T. ) ;
#11900 = CARTESIAN_POINT ( 'NONE',  ( 15.00000000000000000, -22.67460108101774452, 6.353146135318220367 ) ) ;
#11901 = CYLINDRICAL_SURFACE ( 'NONE', #17999, 82.00000000000000000 ) ;
#11902 = CARTESIAN_POINT ( 'NONE',  ( 0.000000000000000000, 25.88420570971438650, -27.13269053701069566 ) ) ;
#11903 = DIRECTION ( 'NONE',  ( -1.000000000000000000, 0.000000000000000000, 0.000000000000000000 ) ) ;
#11904 = ORIENTED_EDGE ( 'NONE', *, *, #55762, .T. ) ;
#11905 = ORIENTED_EDGE ( 'NONE', *, *, #41117, .F. ) ;
#11906 = VECTOR ( 'NONE', #48921, 1000.000000000000000 ) ;
#11907 = CARTESIAN_POINT ( 'NONE',  ( 96.15314808468750130, -211.9973110713294489, 80.48822916753381662 ) ) ;
#11908 = LINE ( 'NONE', #6650, #41232 ) ;
#11909 = CARTESIAN_POINT ( 'NONE',  ( -94.99999999999997158, -206.9400435732949575, 77.22062500173429100 ) ) ;
#11910 = CARTESIAN_POINT ( 'NONE',  ( 92.34999999999999432, 91.52997821335252127, 83.67645833506763609 ) ) ;
#11911 = AXIS2_PLACEMENT_3D ( 'NONE', #12044, #5687, #443 ) ;
#11912 = CARTESIAN_POINT ( 'NONE',  ( 11.99999999999999822, -8.840884882375609877, 74.65374052328647281 ) ) ;
#11913 = CARTESIAN_POINT ( 'NONE',  ( 97.64999999999997726, -211.5299782133524502, 85.18458333333332178 ) ) ;
#11914 = VECTOR ( 'NONE', #25850, 1000.000000000000000 ) ;
#11915 = EDGE_LOOP ( 'NONE', ( #23061, #58936, #29942, #69887 ) ) ;
#11916 = ORIENTED_EDGE ( 'NONE', *, *, #22670, .T. ) ;
#11917 = VECTOR ( 'NONE', #2009, 1000.000000000000000 ) ;
#11918 = ORIENTED_EDGE ( 'NONE', *, *, #61696, .T. ) ;
#11919 = EDGE_LOOP ( 'NONE', ( #12846, #50425, #51123, #45232 ) ) ;
#11920 = FACE_OUTER_BOUND ( 'NONE', #33954, .T. ) ;
#11921 = CIRCLE ( 'NONE', #20183, 16.00000000000000000 ) ;
#11922 = CARTESIAN_POINT ( 'NONE',  ( -92.69370383062504004, 90.00000000000004263, 88.21406250086714351 ) ) ;
#11923 = CARTESIAN_POINT ( 'NONE',  ( 10.00000000000000000, -33.00180498840060039, 17.80606268964528027 ) ) ;
#11924 = VECTOR ( 'NONE', #71334, 1000.000000000000000 ) ;
#11925 = LINE ( 'NONE', #52513, #49738 ) ;
#11926 = CARTESIAN_POINT ( 'NONE',  ( 97.64999999999997726, -208.4700217866474645, 78.38479166840096468 ) ) ;
#11927 = CARTESIAN_POINT ( 'NONE',  ( 93.67499999999998295, 92.29496732002878900, 77.19416666666666060 ) ) ;
#11928 = VERTEX_POINT ( 'NONE', #14642 ) ;
#11929 = LINE ( 'NONE', #51048, #65951 ) ;
#11930 = EDGE_CURVE ( 'NONE', #57622, #6059, #25313, .T. ) ;
#11931 = VERTEX_POINT ( 'NONE', #10485 ) ;
#11932 = LINE ( 'NONE', #5582, #55419 ) ;
#11933 = ORIENTED_EDGE ( 'NONE', *, *, #60017, .F. ) ;
#11934 = CARTESIAN_POINT ( 'NONE',  ( -93.67500000000003979, 87.70503267997129626, 88.38604166840097776 ) ) ;
#11935 = CARTESIAN_POINT ( 'NONE',  ( -92.69370383062505425, 91.33154071421968467, 81.28197916753381946 ) ) ;
#11936 = CARTESIAN_POINT ( 'NONE',  ( 93.84685191531248449, 88.00268892867053694, 88.63739583420048973 ) ) ;
#11937 = ORIENTED_EDGE ( 'NONE', *, *, #9614, .F. ) ;
#11938 = DIRECTION ( 'NONE',  ( 0.8896955516311735312, 0.000000000000000000, -0.4565542962317865050 ) ) ;
#11939 = DIRECTION ( 'NONE',  ( 0.000000000000000000, 0.000000000000000000, 1.000000000000000000 ) ) ;
#11940 = CARTESIAN_POINT ( 'NONE',  ( 0.000000000000000000, 26.79245525562714292, 32.34446384429980981 ) ) ;
#11941 = CARTESIAN_POINT ( 'NONE',  ( -92.69370383062502583, 90.00000000000007105, 74.79348190356851944 ) ) ;
#11942 = ORIENTED_EDGE ( 'NONE', *, *, #39201, .F. ) ;
#11943 = CARTESIAN_POINT ( 'NONE',  ( 0.000000000000000000, -13.04903810567647682, -19.60159698893442481 ) ) ;
#11944 = AXIS2_PLACEMENT_3D ( 'NONE', #16756, #15640, #38574 ) ;
#11946 = AXIS2_PLACEMENT_3D ( 'NONE', #41616, #59657, #29216 ) ;
#11945 = CARTESIAN_POINT ( 'NONE',  ( -97.30629616937495996, -209.9999999999999716, 76.94281250086713442 ) ) ;
#11947 = VERTEX_POINT ( 'NONE', #3034 ) ;
#11948 = ORIENTED_EDGE ( 'NONE', *, *, #51071, .F. ) ;
#11949 = EDGE_CURVE ( 'NONE', #19312, #2794, #54868, .T. ) ;
#11950 = DIRECTION ( 'NONE',  ( -0.000000000000000000, 0.000000000000000000, 1.000000000000000000 ) ) ;
#11951 = VECTOR ( 'NONE', #15531, 1000.000000000000000 ) ;
#11952 = CIRCLE ( 'NONE', #31154, 37.49900000000000233 ) ;
#11953 = EDGE_CURVE ( 'NONE', #63551, #54039, #37589, .T. ) ;
#11954 = EDGE_LOOP ( 'NONE', ( #4942, #64743, #36065, #52696, #7058, #27917 ) ) ;
#11955 = CARTESIAN_POINT ( 'NONE',  ( 0.000000000000000000, 81.50828551894240093, -8.966570791699810528 ) ) ;
#11956 = CARTESIAN_POINT ( 'NONE',  ( -93.67499999999998295, -212.2949673200287179, 78.14666666666667538 ) ) ;
#11957 = VERTEX_POINT ( 'NONE', #72151 ) ;
#11958 = CARTESIAN_POINT ( 'NONE',  ( -97.30629616937495996, -209.9999999999999716, 75.67281250086713840 ) ) ;
#11959 = ORIENTED_EDGE ( 'NONE', *, *, #63581, .T. ) ;
#11960 = DIRECTION ( 'NONE',  ( -1.000000000000000000, 0.000000000000000000, 0.000000000000000000 ) ) ;
#11961 = DIRECTION ( 'NONE',  ( -1.000000000000000000, -0.000000000000000000, -0.000000000000000000 ) ) ;
#11962 = CARTESIAN_POINT ( 'NONE',  ( -97.65000000000000568, 89.99997747911959323, 86.26937578065384571 ) ) ;
#11963 = VERTEX_POINT ( 'NONE', #49588 ) ;
#11964 = EDGE_CURVE ( 'NONE', #2629, #25433, #12345, .T. ) ;
#11965 = EDGE_CURVE ( 'NONE', #18479, #44748, #27714, .T. ) ;
#11966 = ORIENTED_EDGE ( 'NONE', *, *, #45018, .F. ) ;
#11967 = PLANE ( 'NONE',  #56002 ) ;
#11968 = DIRECTION ( 'NONE',  ( -1.000000000000000000, 0.000000000000000000, -0.000000000000000000 ) ) ;
#11969 = CARTESIAN_POINT ( 'NONE',  ( 92.69370383062498320, 91.33154071421968467, 84.50989583420049200 ) ) ;
#11970 = CARTESIAN_POINT ( 'NONE',  ( 6.000000000000000000, -78.73519480814971416, 22.90783923731599359 ) ) ;
#11971 = CARTESIAN_POINT ( 'NONE',  ( 10.00000000000000000, 20.40083707022882820, 72.35432306680490910 ) ) ;
#11972 = CARTESIAN_POINT ( 'NONE',  ( 12.00000000000000000, -23.29833615347104470, 3.418703333116808629 ) ) ;
#11973 = DIRECTION ( 'NONE',  ( 1.000000000000000000, 0.000000000000000000, 0.000000000000000000 ) ) ;
#11974 = DIRECTION ( 'NONE',  ( 0.000000000000000000, 0.000000000000000000, 1.000000000000000000 ) ) ;
#11975 = LINE ( 'NONE', #62395, #32310 ) ;
#11976 = CYLINDRICAL_SURFACE ( 'NONE', #47090, 82.00000000000000000 ) ;
#11977 = CIRCLE ( 'NONE', #63621, 77.49899999999999523 ) ;
#11978 = EDGE_CURVE ( 'NONE', #12324, #63432, #17615, .T. ) ;
#11979 = CARTESIAN_POINT ( 'NONE',  ( 97.65000000000000568, -208.4700217866474645, 85.36979166840096411 ) ) ;
#11980 = VECTOR ( 'NONE', #16249, 1000.000000000000000 ) ;
#11981 = CARTESIAN_POINT ( 'NONE',  ( 0.000000000000000000, -120.0000000000000000, 125.0000000000000000 ) ) ;
#11982 = AXIS2_PLACEMENT_3D ( 'NONE', #67076, #4320, #27205 ) ;
#11983 = CARTESIAN_POINT ( 'NONE',  ( -96.15314808468752972, 91.99731107132950569, 89.53697916753381492 ) ) ;
#11984 = LINE ( 'NONE', #34928, #19057 ) ;
#11985 = VECTOR ( 'NONE', #62319, 1000.000000000000000 ) ;
#11987 = ADVANCED_FACE ( 'NONE', ( #40544 ), #51449, .T. ) ;
#11986 = CARTESIAN_POINT ( 'NONE',  ( 10.00000000000000000, -3.925862922256464493, 41.81611651403861174 ) ) ;
#11988 = ADVANCED_FACE ( 'NONE', ( #34166 ), #57110, .T. ) ;
#11989 = ORIENTED_EDGE ( 'NONE', *, *, #41656, .T. ) ;
#11990 = EDGE_CURVE ( 'NONE', #26052, #43117, #22147, .T. ) ;
#11991 = CARTESIAN_POINT ( 'NONE',  ( 11.99999999999999822, 59.03961581697465277, -46.53671651293886669 ) ) ;
#11992 = CARTESIAN_POINT ( 'NONE',  ( 10.00000000000000000, 10.96151621346487914, 35.95386929396260456 ) ) ;
#11993 = DIRECTION ( 'NONE',  ( -1.000000000000000000, -0.000000000000000000, 0.000000000000000000 ) ) ;
#11994 = DIRECTION ( 'NONE',  ( 0.000000000000000000, 0.1045284632676459491, -0.9945218953682741780 ) ) ;
#11995 = CIRCLE ( 'NONE', #44425, 82.00000000000000000 ) ;
#11996 = LINE ( 'NONE', #34936, #35593 ) ;
#11997 = VECTOR ( 'NONE', #11740, 1000.000000000000000 ) ;
#11998 = VECTOR ( 'NONE', #55417, 1000.000000000000000 ) ;
#11999 = CARTESIAN_POINT ( 'NONE',  ( 92.69370383062501162, -209.9999999999999716, 84.08656250086716000 ) ) ;
#12000 = ORIENTED_EDGE ( 'NONE', *, *, #6199, .F. ) ;
#12001 = AXIS2_PLACEMENT_3D ( 'NONE', #22201, #67319, #22575 ) ;
#12002 = ORIENTED_EDGE ( 'NONE', *, *, #62602, .T. ) ;
#12003 = CIRCLE ( 'NONE', #54041, 16.00000000000000000 ) ;
#12004 = FACE_OUTER_BOUND ( 'NONE', #22481, .T. ) ;
#12005 = ORIENTED_EDGE ( 'NONE', *, *, #25310, .F. ) ;
#12006 = DIRECTION ( 'NONE',  ( -0.000000000000000000, 0.000000000000000000, 1.000000000000000000 ) ) ;
#12007 = DIRECTION ( 'NONE',  ( -1.000000000000000000, -0.000000000000000000, -0.000000000000000000 ) ) ;
#12008 = VERTEX_POINT ( 'NONE', #28512 ) ;
#12009 = CARTESIAN_POINT ( 'NONE',  ( 95.00000000000000000, -212.6630814284392557, 82.34031250086714238 ) ) ;
#12010 = VERTEX_POINT ( 'NONE', #69484 ) ;
#12011 = CARTESIAN_POINT ( 'NONE',  ( 5.000000000000000000, -64.81221759200306565, -50.23322058963418613 ) ) ;
#12012 = ORIENTED_EDGE ( 'NONE', *, *, #12716, .T. ) ;
#12013 = ORIENTED_EDGE ( 'NONE', *, *, #1852, .F. ) ;
#12014 = DIRECTION ( 'NONE',  ( 0.000000000000000000, 0.000000000000000000, 1.000000000000000000 ) ) ;
#12015 = DIRECTION ( 'NONE',  ( 1.000000000000000000, 0.000000000000000000, 0.000000000000000000 ) ) ;
#12016 = ORIENTED_EDGE ( 'NONE', *, *, #58938, .F. ) ;
#12017 = CARTESIAN_POINT ( 'NONE',  ( -97.65000000000006253, 91.52997821335252127, 84.23208333333334963 ) ) ;
#12018 = CARTESIAN_POINT ( 'NONE',  ( 95.00000000000000000, -206.9400435732949575, 87.38062500173430180 ) ) ;
#12019 = ORIENTED_EDGE ( 'NONE', *, *, #11230, .T. ) ;
#12020 = CARTESIAN_POINT ( 'NONE',  ( 5.999999999999998224, 0.000000000000000000, 0.000000000000000000 ) ) ;
#12021 = EDGE_CURVE ( 'NONE', #57727, #53203, #46558, .T. ) ;
#12022 = ORIENTED_EDGE ( 'NONE', *, *, #8196, .F. ) ;
#12023 = LINE ( 'NONE', #57166, #43316 ) ;
#12024 = VECTOR ( 'NONE', #59259, 1000.000000000000000 ) ;
#12025 = ORIENTED_EDGE ( 'NONE', *, *, #60638, .F. ) ;
#12026 = AXIS2_PLACEMENT_3D ( 'NONE', #24370, #2216, #70572 ) ;
#12027 = EDGE_LOOP ( 'NONE', ( #65850, #23882, #58885, #40031 ) ) ;
#12028 = FILL_AREA_STYLE ('',( #57907 ) ) ;
#12029 = EDGE_LOOP ( 'NONE', ( #8225, #28832, #23306, #68172 ) ) ;
#12030 = CIRCLE ( 'NONE', #54067, 16.00000000000000000 ) ;
#12031 = CARTESIAN_POINT ( 'NONE',  ( -5.000000000000000000, -0.9645339558193164464, -0.6919071587033235327 ) ) ;
#12033 = EDGE_CURVE ( 'NONE', #36560, #47180, #51084, .T. ) ;
#12032 = VERTEX_POINT ( 'NONE', #5613 ) ;
#12034 = VERTEX_POINT ( 'NONE', #9 ) ;
#12035 = AXIS2_PLACEMENT_3D ( 'NONE', #37224, #7167, #19540 ) ;
#12036 = ORIENTED_EDGE ( 'NONE', *, *, #17345, .F. ) ;
#12037 = DIRECTION ( 'NONE',  ( 0.000000000000000000, -0.1564344650402168801, -0.9876883405951399908 ) ) ;
#12038 = EDGE_CURVE ( 'NONE', #72759, #55034, #57848, .T. ) ;
#12039 = DIRECTION ( 'NONE',  ( -1.000000000000000000, 0.000000000000000000, 0.000000000000000000 ) ) ;
#12040 = CARTESIAN_POINT ( 'NONE',  ( -93.67500000000003979, 92.29496732002878900, 89.15333333333333599 ) ) ;
#12041 = ORIENTED_EDGE ( 'NONE', *, *, #37367, .F. ) ;
#12042 = CARTESIAN_POINT ( 'NONE',  ( 96.15314808468748708, 91.99731107132950569, 74.82614583420047438 ) ) ;
#12043 = EDGE_LOOP ( 'NONE', ( #55470, #29108, #10545, #73290 ) ) ;
#12044 = CARTESIAN_POINT ( 'NONE',  ( -0.0004442498525516064278, 0.001194404164626844313, 127.4927882439603195 ) ) ;
#12045 = CARTESIAN_POINT ( 'NONE',  ( -97.30629616937497417, -211.3315407142195852, 87.15572916753380639 ) ) ;
#12046 = ORIENTED_EDGE ( 'NONE', *, *, #46857, .T. ) ;
#12047 = MANIFOLD_SOLID_BREP ( 'Cut-Extrude1', #22384 ) ;
#12048 = CARTESIAN_POINT ( 'NONE',  ( 10.00000000000000000, 25.88420570971400991, 27.13269053701105449 ) ) ;
#12049 = DIRECTION ( 'NONE',  ( 0.000000000000000000, 1.000000000000000000, 3.491481338843133355E-15 ) ) ;
#12050 = CARTESIAN_POINT ( 'NONE',  ( 0.000000000000000000, 0.000000000000000000, -5.624496230895140947 ) ) ;
#12051 = CARTESIAN_POINT ( 'NONE',  ( -97.30629616937495996, -209.9999999999999716, 76.30781250086714351 ) ) ;
#12052 = VECTOR ( 'NONE', #20381, 999.9999999999998863 ) ;
#12053 = EDGE_CURVE ( 'NONE', #15157, #8951, #45776, .T. ) ;
#12054 = CARTESIAN_POINT ( 'NONE',  ( 5.000000000000000000, -21.40280677340398086, 36.13751322684410638 ) ) ;
#12055 = CARTESIAN_POINT ( 'NONE',  ( 10.00000000000000000, 58.39081064771751528, 50.95692526931350841 ) ) ;
#12056 = CIRCLE ( 'NONE', #46894, 31.99999999999999289 ) ;
#12057 = CARTESIAN_POINT ( 'NONE',  ( -11.59999999999999964, -0.8299999999999986278, -1.199999999999999956 ) ) ;
#12058 = CARTESIAN_POINT ( 'NONE',  ( 0.000000000000000000, 59.03961581697399907, 46.53671651293969802 ) ) ;
#12059 = AXIS2_PLACEMENT_3D ( 'NONE', #42609, #60284, #59534 ) ;
#12060 = CIRCLE ( 'NONE', #4845, 16.00000000000000000 ) ;
#12061 = CARTESIAN_POINT ( 'NONE',  ( 10.00000000000000000, -33.79645857604501913, -16.45098606841161626 ) ) ;
#12062 = CARTESIAN_POINT ( 'NONE',  ( 92.34999999999999432, 90.00000000000002842, 88.09499999999999886 ) ) ;
#12063 = CARTESIAN_POINT ( 'NONE',  ( -97.30629616937501680, 91.33154071421968467, 76.88989583420047325 ) ) ;
#12064 = DIRECTION ( 'NONE',  ( -1.000000000000000000, -0.000000000000000000, 0.000000000000000000 ) ) ;
#12065 = CARTESIAN_POINT ( 'NONE',  ( 0.000000000000000000, 44.99326035066051332, 68.55367621811160461 ) ) ;
#12066 = EDGE_CURVE ( 'NONE', #10923, #1624, #51761, .T. ) ;
#12067 = VERTEX_POINT ( 'NONE', #12336 ) ;
#12068 = EDGE_CURVE ( 'NONE', #54039, #46823, #57779, .T. ) ;
#12069 = CARTESIAN_POINT ( 'NONE',  ( -97.64999999990722301, -209.9999861897314304, 80.55392363651652943 ) ) ;
#12070 = ADVANCED_FACE ( 'NONE', ( #36008 ), #41645, .T. ) ;
#12071 = CARTESIAN_POINT ( 'NONE',  ( -13.05994868825747446, -139.5943292883446532, -2.500000000000000000 ) ) ;
#12072 = CARTESIAN_POINT ( 'NONE',  ( 97.65000000000000568, -211.5299782133524218, 86.53395833506763779 ) ) ;
#12073 = CARTESIAN_POINT ( 'NONE',  ( -10.00000000000000000, 0.000000000000000000, 0.000000000000000000 ) ) ;
#12074 = CARTESIAN_POINT ( 'NONE',  ( -3.000000000000000000, 14.60985201121729737, -18.46759930825687945 ) ) ;
#12075 = CARTESIAN_POINT ( 'NONE',  ( 10.00000000000000000, 22.74946021919133088, 29.81001611431016229 ) ) ;
#12076 = CARTESIAN_POINT ( 'NONE',  ( -93.67499999999998295, -207.7050326799711968, 89.78833333333332689 ) ) ;
#12077 = DIRECTION ( 'NONE',  ( -0.000000000000000000, -0.000000000000000000, 1.000000000000000000 ) ) ;
#12078 = ADVANCED_FACE ( 'NONE', ( #41289 ), #55352, .F. ) ;
#12079 = VERTEX_POINT ( 'NONE', #70949 ) ;
#12080 = EDGE_CURVE ( 'NONE', #44189, #54372, #12700, .T. ) ;
#12081 = PLANE ( 'NONE',  #13078 ) ;
#12082 = CARTESIAN_POINT ( 'NONE',  ( -2.459674775249762302, -3.512261536895417911E-15, -1.958521724548552858E-15 ) ) ;
#12083 = DIRECTION ( 'NONE',  ( -1.000000000000000000, -0.000000000000000000, 0.000000000000000000 ) ) ;
#12084 = LINE ( 'NONE', #69958, #58140 ) ;
#12085 = AXIS2_PLACEMENT_3D ( 'NONE', #22058, #51001, #11875 ) ;
#12086 = AXIS2_PLACEMENT_3D ( 'NONE', #52373, #23085, #40361 ) ;
#12087 = CARTESIAN_POINT ( 'NONE',  ( -94.99999999999997158, -209.9999999999999716, 90.00000000000000000 ) ) ;
#12088 = ORIENTED_EDGE ( 'NONE', *, *, #9953, .F. ) ;
#12089 = DIRECTION ( 'NONE',  ( -1.000000000000000000, 0.000000000000000000, 0.000000000000000000 ) ) ;
#12090 = SURFACE_SIDE_STYLE ('',( #41407 ) ) ;
#12091 = ORIENTED_EDGE ( 'NONE', *, *, #52112, .F. ) ;
#12092 = CARTESIAN_POINT ( 'NONE',  ( 92.69370383062501162, -211.3315407142195852, 86.52072916753381548 ) ) ;
#12093 = CARTESIAN_POINT ( 'NONE',  ( -92.35000000000005116, 91.52997821335253548, 82.19479166840095274 ) ) ;
#12094 = ORIENTED_EDGE ( 'NONE', *, *, #7454, .T. ) ;
#12095 = DIRECTION ( 'NONE',  ( -1.000000000000000000, 0.000000000000000000, -0.000000000000000000 ) ) ;
#12096 = ORIENTED_EDGE ( 'NONE', *, *, #59610, .F. ) ;
#12097 = DIRECTION ( 'NONE',  ( -1.000000000000000000, -0.000000000000000000, -0.000000000000000000 ) ) ;
#12098 = EDGE_LOOP ( 'NONE', ( #38294, #64366 ) ) ;
#12099 = AXIS2_PLACEMENT_3D ( 'NONE', #32102, #48669, #9179 ) ;
#12100 = CARTESIAN_POINT ( 'NONE',  ( -97.30629616937501680, 88.66845928578038638, 79.69447916753381378 ) ) ;
#12101 = VECTOR ( 'NONE', #1182, 1000.000000000000000 ) ;
#12102 = ORIENTED_EDGE ( 'NONE', *, *, #23929, .F. ) ;
#12103 = ORIENTED_EDGE ( 'NONE', *, *, #48145, .F. ) ;
#12104 = AXIS2_PLACEMENT_3D ( 'NONE', #20944, #43168, #27319 ) ;
#12105 = VERTEX_POINT ( 'NONE', #58568 ) ;
#12106 = CARTESIAN_POINT ( 'NONE',  ( 0.000000000000000000, -70.53064760720297954, -26.01480285779911839 ) ) ;
#12107 = ORIENTED_EDGE ( 'NONE', *, *, #16066, .T. ) ;
#12108 = ORIENTED_EDGE ( 'NONE', *, *, #27304, .T. ) ;
#12109 =( BOUNDED_CURVE ( )  B_SPLINE_CURVE ( 2, ( #35080, #22700, #45645, #5784, #41458, #68565, #63295 ),
 .UNSPECIFIED., .F., .F. ) 
 B_SPLINE_CURVE_WITH_KNOTS ( ( 3, 2, 2, 3 ),
 ( 0.02116741234826251261, 0.02822306216352946096, 0.03527882770441181925, 0.04233441017594418571 ),
 .UNSPECIFIED. ) 
 CURVE ( )  GEOMETRIC_REPRESENTATION_ITEM ( )  RATIONAL_B_SPLINE_CURVE ( ( 0.9999956052852916333, 0.8660276011778336169, 1.000000000000000000, 0.8660254037844387076, 1.000000000000000000, 0.8660288798979943747, 0.9999930479532715966 ) ) 
 REPRESENTATION_ITEM ( '' )  );
#12110 = DIRECTION ( 'NONE',  ( -1.000000000000000000, -0.000000000000000000, 0.000000000000000000 ) ) ;
#12111 = ORIENTED_EDGE ( 'NONE', *, *, #41841, .F. ) ;
#12112 = ADVANCED_FACE ( 'NONE', ( #7445 ), #30726, .T. ) ;
#12113 = ORIENTED_EDGE ( 'NONE', *, *, #11197, .T. ) ;
#12114 = CARTESIAN_POINT ( 'NONE',  ( 96.15314808468748708, 91.99731107132950569, 86.25614583420048120 ) ) ;
#12115 = ORIENTED_EDGE ( 'NONE', *, *, #26545, .F. ) ;
#12116 = CARTESIAN_POINT ( 'NONE',  ( 95.00000000000000000, -212.6630814284392557, 83.45156250086714067 ) ) ;
#12117 = APPLICATION_PROTOCOL_DEFINITION ( 'draft international standard', 'automotive_design', 1998, #8564 ) ;
#12118 = DIRECTION ( 'NONE',  ( 0.000000000000000000, 0.000000000000000000, 1.000000000000000000 ) ) ;
#12119 = EDGE_CURVE ( 'NONE', #55893, #44231, #7809, .T. ) ;
#12120 = CARTESIAN_POINT ( 'NONE',  ( -23.54415474984308787, -120.4156646670583086, 5.500000000000000000 ) ) ;
#12121 = CARTESIAN_POINT ( 'NONE',  ( 97.64999999999999147, -209.9999999999999716, 78.88750000000000284 ) ) ;
#12122 = DIRECTION ( 'NONE',  ( -1.000000000000000000, -0.000000000000000000, -0.000000000000000000 ) ) ;
#12123 = ADVANCED_FACE ( 'NONE', ( #1842 ), #19083, .F. ) ;
#12124 = CARTESIAN_POINT ( 'NONE',  ( 2.499999999999979572, -90.00000000000000000, -280.0000000000000000 ) ) ;
#12125 = CARTESIAN_POINT ( 'NONE',  ( -92.69370383062498320, -211.3315407142195852, 84.19239583420046813 ) ) ;
#12126 = CARTESIAN_POINT ( 'NONE',  ( -95.00000000000002842, 92.66308142843932671, 81.38781250086715602 ) ) ;
#12127 = VERTEX_POINT ( 'NONE', #36370 ) ;
#12128 = CARTESIAN_POINT ( 'NONE',  ( 97.30629616937498838, 90.00000000000002842, 84.88031250086713442 ) ) ;
#12129 = EDGE_CURVE ( 'NONE', #39032, #60096, #24731, .T. ) ;
#12130 = VERTEX_POINT ( 'NONE', #47659 ) ;
#12131 = DIRECTION ( 'NONE',  ( 1.000000000000000000, 0.000000000000000000, 0.000000000000000000 ) ) ;
#12132 = DIRECTION ( 'NONE',  ( -0.000000000000000000, -1.000000000000000000, -0.000000000000000000 ) ) ;
#12133 = CARTESIAN_POINT ( 'NONE',  ( 6.000000000000000000, 68.55367621811204515, -44.99326035065983120 ) ) ;
#12134 = LINE ( 'NONE', #74180, #22459 ) ;
#12135 = CARTESIAN_POINT ( 'NONE',  ( -94.99999999999997158, -207.3369185715606307, 85.67406250086715147 ) ) ;
#12136 = CARTESIAN_POINT ( 'NONE',  ( 11.99999999999999822, 62.20884554314085335, -46.21855187248562657 ) ) ;
#12137 = CIRCLE ( 'NONE', #13314, 16.00000000000000000 ) ;
#12138 = DIRECTION ( 'NONE',  ( -1.000000000000000000, -0.000000000000000000, -0.000000000000000000 ) ) ;
#12139 = CARTESIAN_POINT ( 'NONE',  ( 11.99999999999999822, -75.16055320797043748, 18.89407956138231270 ) ) ;
#12140 = AXIS2_PLACEMENT_3D ( 'NONE', #21772, #72519, #10118 ) ;
#12141 = CARTESIAN_POINT ( 'NONE',  ( 93.67499999999998295, 92.29496732002878900, 80.36916666666665776 ) ) ;
#12142 = VERTEX_POINT ( 'NONE', #70567 ) ;
#12143 = ORIENTED_EDGE ( 'NONE', *, *, #5398, .F. ) ;
#12144 = CARTESIAN_POINT ( 'NONE',  ( -97.65000000000001990, 88.47002178664754979, 77.35291666666665833 ) ) ;
#12145 = CARTESIAN_POINT ( 'NONE',  ( 0.000000000000000000, 0.000000000000000000, 0.000000000000000000 ) ) ;
#12146 = CARTESIAN_POINT ( 'NONE',  ( -92.69370383062502583, 91.33154071421968467, 88.74322916753379786 ) ) ;
#12147 = CARTESIAN_POINT ( 'NONE',  ( 97.65000000000009095, -208.4700217866474929, 80.84541666666663673 ) ) ;
#12148 = CARTESIAN_POINT ( 'NONE',  ( -7.500000000000015099, -73.00000000000001421, -204.9999999999999716 ) ) ;
#12149 = DIRECTION ( 'NONE',  ( 0.000000000000000000, 0.000000000000000000, 1.000000000000000000 ) ) ;
#12150 = CARTESIAN_POINT ( 'NONE',  ( -93.67499999999998295, -207.7050326799711968, 78.35833333333333428 ) ) ;
#12151 = ORIENTED_EDGE ( 'NONE', *, *, #404, .F. ) ;
#12152 = CARTESIAN_POINT ( 'NONE',  ( -93.84685191531254134, 91.99731107132950569, 78.63614583420047666 ) ) ;
#12153 = CARTESIAN_POINT ( 'NONE',  ( 15.00000000000000000, 26.49999999999999645, 1.499999999999995781 ) ) ;
#12154 = AXIS2_PLACEMENT_3D ( 'NONE', #48299, #32839, #56158 ) ;
#12155 = ADVANCED_FACE ( 'NONE', ( #29991 ), #2212, .T. ) ;
#12156 = ADVANCED_FACE ( 'NONE', ( #64970 ), #52937, .T. ) ;
#12157 = CARTESIAN_POINT ( 'NONE',  ( 0.000000000000000000, 5.202137450156389953, 37.22597642581160216 ) ) ;
#12158 = AXIS2_PLACEMENT_3D ( 'NONE', #51250, #62944, #23073 ) ;
#12159 = DIRECTION ( 'NONE',  ( -0.4279312458752990711, -0.9038112904824846527, 0.000000000000000000 ) ) ;
#12160 = DIRECTION ( 'NONE',  ( -1.000000000000000000, 0.000000000000000000, -0.000000000000000000 ) ) ;
#12161 = DIRECTION ( 'NONE',  ( 0.7273375899149793211, -0.6862798483830554463, 0.000000000000000000 ) ) ;
#12162 = CARTESIAN_POINT ( 'NONE',  ( -93.84685191531248449, -208.0026889286704943, 87.68489583420048916 ) ) ;
#12163 =( NAMED_UNIT ( * ) PLANE_ANGLE_UNIT ( ) SI_UNIT ( $, .RADIAN. ) );
#12164 = VECTOR ( 'NONE', #49432, 1000.000000000000000 ) ;
#12165 = PLANE ( 'NONE',  #42061 ) ;
#12166 = EDGE_CURVE ( 'NONE', #57064, #20511, #15351, .T. ) ;
#12167 = VECTOR ( 'NONE', #66550, 1000.000000000000000 ) ;
#12168 = MANIFOLD_SOLID_BREP ( 'Fillet2', #72805 ) ;
#12169 = CARTESIAN_POINT ( 'NONE',  ( 96.15314808468748708, 91.99731107132950569, 76.88989583420048746 ) ) ;
#12170 = CARTESIAN_POINT ( 'NONE',  ( -97.30629616937497417, -211.3315407142195852, 75.88447916753382572 ) ) ;
#12171 = DIRECTION ( 'NONE',  ( 0.4415113423096792000, 5.406954521468000113E-17, -0.8972556684757725387 ) ) ;
#12172 = VERTEX_POINT ( 'NONE', #20188 ) ;
#12173 = DIRECTION ( 'NONE',  ( 0.000000000000000000, 0.000000000000000000, 1.000000000000000000 ) ) ;
#12174 = DIRECTION ( 'NONE',  ( 0.000000000000000000, 0.000000000000000000, 1.000000000000000000 ) ) ;
#12175 = FACE_OUTER_BOUND ( 'NONE', #28138, .T. ) ;
#12176 = CARTESIAN_POINT ( 'NONE',  ( -95.00000000000002842, 87.33691857156074434, 75.99031250086716227 ) ) ;
#12177 = CARTESIAN_POINT ( 'NONE',  ( 96.15314808468748708, -208.0026889286704943, 78.00114583420048575 ) ) ;
#12178 = ORIENTED_EDGE ( 'NONE', *, *, #28844, .T. ) ;
#12179 = DIRECTION ( 'NONE',  ( 0.000000000000000000, 0.5877852522924684742, 0.8090169943749506709 ) ) ;
#12180 = EDGE_LOOP ( 'NONE', ( #40819, #8888, #42795, #20428 ) ) ;
#12181 = FACE_OUTER_BOUND ( 'NONE', #4097, .T. ) ;
#12182 = ORIENTED_EDGE ( 'NONE', *, *, #16752, .T. ) ;
#12183 = AXIS2_PLACEMENT_3D ( 'NONE', #3836, #49664, #50413 ) ;
#12185 = AXIS2_PLACEMENT_3D ( 'NONE', #24369, #13073, #25103 ) ;
#12184 = CARTESIAN_POINT ( 'NONE',  ( 12.00000000000000000, 23.49999999999999645, -1.500000000000003997 ) ) ;
#12186 = VECTOR ( 'NONE', #53857, 1000.000000000000000 ) ;
#12187 = EDGE_LOOP ( 'NONE', ( #67244, #67704, #24399, #63357 ) ) ;
#12188 = ORIENTED_EDGE ( 'NONE', *, *, #29684, .T. ) ;
#12189 = VERTEX_POINT ( 'NONE', #25100 ) ;
#12190 = CARTESIAN_POINT ( 'NONE',  ( 10.00000000000000000, 0.000000000000000000, 0.000000000000000000 ) ) ;
#12191 = VECTOR ( 'NONE', #34050, 1000.000000000000000 ) ;
#12192 = ORIENTED_EDGE ( 'NONE', *, *, #67022, .F. ) ;
#12193 = ORIENTED_EDGE ( 'NONE', *, *, #71220, .F. ) ;
#12194 = CARTESIAN_POINT ( 'NONE',  ( 96.15314808468748708, 91.99731107132950569, 83.87489583420048689 ) ) ;
#12195 = CARTESIAN_POINT ( 'NONE',  ( 96.90829729882592858, -211.8387227684709444, 74.99909419456535886 ) ) ;
#12196 = EDGE_LOOP ( 'NONE', ( #12644, #52800, #48430, #32386 ) ) ;
#12197 = EDGE_LOOP ( 'NONE', ( #34593, #18579, #60758, #27088 ) ) ;
#12198 = ADVANCED_FACE ( 'NONE', ( #72066 ), #49509, .T. ) ;
#12199 = ORIENTED_EDGE ( 'NONE', *, *, #45524, .T. ) ;
#12200 = VERTEX_POINT ( 'NONE', #15294 ) ;
#12201 = DIRECTION ( 'NONE',  ( 0.6862798483830533369, 0.7273375899149812085, -0.000000000000000000 ) ) ;
#12202 = AXIS2_PLACEMENT_3D ( 'NONE', #18071, #74093, #57929 ) ;
#12203 = ORIENTED_EDGE ( 'NONE', *, *, #38643, .T. ) ;
#12204 = AXIS2_PLACEMENT_3D ( 'NONE', #51710, #40058, #27274 ) ;
#12205 = SURFACE_SIDE_STYLE ('',( #24246 ) ) ;
#12206 = DIRECTION ( 'NONE',  ( 0.000000000000000000, -0.8090169943749402348, -0.5877852522924830181 ) ) ;
#12207 = EDGE_CURVE ( 'NONE', #71079, #63717, #15199, .T. ) ;
#12208 = LINE ( 'NONE', #34779, #6362 ) ;
#12209 = CARTESIAN_POINT ( 'NONE',  ( 23.50000000000260414, -119.9999999999999716, -64.99999999999938893 ) ) ;
#12210 = AXIS2_PLACEMENT_3D ( 'NONE', #52020, #56578, #68961 ) ;
#12211 = CARTESIAN_POINT ( 'NONE',  ( 96.32499999999998863, -212.2949673200287179, 87.11604166840096752 ) ) ;
#12212 = CARTESIAN_POINT ( 'NONE',  ( 1.243286885786405054E-17, -120.0000000000000000, -80.00000000000001421 ) ) ;
#12213 = DIRECTION ( 'NONE',  ( 0.000000000000000000, 0.3090169943749412340, 0.9510565162951556406 ) ) ;
#12215 = ORIENTED_EDGE ( 'NONE', *, *, #9675, .T. ) ;
#12214 = EDGE_CURVE ( 'NONE', #11744, #1159, #59751, .T. ) ;
#12216 = CARTESIAN_POINT ( 'NONE',  ( -97.64999999999994884, -208.4700217866474645, 79.23145833506762870 ) ) ;
#12217 = ORIENTED_EDGE ( 'NONE', *, *, #30558, .F. ) ;
#12218 = DIRECTION ( 'NONE',  ( 0.7533909544171998318, 0.6575728627325954090, 0.000000000000000000 ) ) ;
#12219 = ORIENTED_EDGE ( 'NONE', *, *, #12280, .F. ) ;
#12221 = CARTESIAN_POINT ( 'NONE',  ( -92.35000000000005116, 88.47002178664754979, 78.27895833506762813 ) ) ;
#12220 = CARTESIAN_POINT ( 'NONE',  ( 96.32499999999997442, 92.29496732002878900, 79.07270833506763097 ) ) ;
#12222 = ADVANCED_FACE ( 'NONE', ( #37505 ), #14927, .T. ) ;
#12223 = VERTEX_POINT ( 'NONE', #8921 ) ;
#12224 = CARTESIAN_POINT ( 'NONE',  ( 94.99999999999998579, 92.66308142843935514, 78.84781250086714977 ) ) ;
#12225 = CARTESIAN_POINT ( 'NONE',  ( 97.64999999999999147, 90.00000000000002842, 75.71250000000000568 ) ) ;
#12226 = DIRECTION ( 'NONE',  ( -1.000000000000000000, -0.000000000000000000, 0.000000000000000000 ) ) ;
#12227 = FACE_OUTER_BOUND ( 'NONE', #52042, .T. ) ;
#12228 = PLANE ( 'NONE',  #17436 ) ;
#12229 = ORIENTED_EDGE ( 'NONE', *, *, #40948, .T. ) ;
#12230 = EDGE_CURVE ( 'NONE', #19685, #26052, #29726, .T. ) ;
#12231 = DIRECTION ( 'NONE',  ( 0.000000000000000000, 0.000000000000000000, 1.000000000000000000 ) ) ;
#12232 = CARTESIAN_POINT ( 'NONE',  ( -10.00000000000000000, 0.000000000000000000, 0.000000000000000000 ) ) ;
#12233 = ORIENTED_EDGE ( 'NONE', *, *, #39839, .F. ) ;
#12234 = ORIENTED_EDGE ( 'NONE', *, *, #18906, .F. ) ;
#12235 = EDGE_CURVE ( 'NONE', #16429, #58346, #73821, .T. ) ;
#12236 = ADVANCED_FACE ( 'NONE', ( #9283 ), #25835, .T. ) ;
#12237 = PRODUCT_DEFINITION_SHAPE ( 'NONE', 'NONE',  #74363 ) ;
#12238 = LINE ( 'NONE', #54235, #50467 ) ;
#12239 = CARTESIAN_POINT ( 'NONE',  ( -2.981146944884250694, -4.052336700773510714, -0.5666985376598571156 ) ) ;
#12240 = DIRECTION ( 'NONE',  ( -1.000000000000000000, 0.000000000000000000, 0.000000000000000000 ) ) ;
#12241 = CARTESIAN_POINT ( 'NONE',  ( -96.15314808468747287, -208.0026889286704943, 76.99572916753382401 ) ) ;
#12242 = CIRCLE ( 'NONE', #47080, 82.00000000000000000 ) ;
#12243 = ORIENTED_EDGE ( 'NONE', *, *, #26040, .F. ) ;
#12244 = AXIS2_PLACEMENT_3D ( 'NONE', #32660, #72865, #55229 ) ;
#12245 = CARTESIAN_POINT ( 'NONE',  ( 0.000000000000000000, 0.000000000000000000, -43.79999999999998295 ) ) ;
#12246 = EDGE_CURVE ( 'NONE', #48900, #58054, #72915, .T. ) ;
#12247 = EDGE_CURVE ( 'NONE', #62825, #64440, #35741, .T. ) ;
#12248 = DIRECTION ( 'NONE',  ( 1.000000000000000000, 0.000000000000000000, 0.000000000000000000 ) ) ;
#12249 = CIRCLE ( 'NONE', #73471, 12.49999999999999645 ) ;
#12250 = DIRECTION ( 'NONE',  ( -1.000000000000000000, -0.000000000000000000, -0.000000000000000000 ) ) ;
#12251 = LINE ( 'NONE', #25008, #39271 ) ;
#12252 = DIRECTION ( 'NONE',  ( 0.000000000000000000, 0.000000000000000000, 1.000000000000000000 ) ) ;
#12253 = CYLINDRICAL_SURFACE ( 'NONE', #38500, 42.00000000000000000 ) ;
#12254 = CARTESIAN_POINT ( 'NONE',  ( 5.000000000000000000, 81.96053171279902472, -2.543863470248670211 ) ) ;
#12255 = CARTESIAN_POINT ( 'NONE',  ( -92.34999999999999432, -211.5299782133524218, 85.26395833506762756 ) ) ;
#12256 = CARTESIAN_POINT ( 'NONE',  ( 0.000000000000000000, 41.76937507738788469, 62.50329211542452157 ) ) ;
#12257 = LINE ( 'NONE', #65257, #28550 ) ;
#12258 = VECTOR ( 'NONE', #20827, 1000.000000000000000 ) ;
#12259 = VECTOR ( 'NONE', #21637, 1000.000000000000000 ) ;
#12260 = CARTESIAN_POINT ( 'NONE',  ( 92.69370383062498320, 91.33154071421968467, 86.57364583420047666 ) ) ;
#12261 = DIRECTION ( 'NONE',  ( 0.000000000000000000, 0.000000000000000000, 1.000000000000000000 ) ) ;
#12262 = CARTESIAN_POINT ( 'NONE',  ( -97.64998576286770060, -211.5299864331645665, 75.52729223699085992 ) ) ;
#12263 = EDGE_LOOP ( 'NONE', ( #59382, #34660, #16257, #46040 ) ) ;
#12264 = LINE ( 'NONE', #23552, #31613 ) ;
#12265 = CARTESIAN_POINT ( 'NONE',  ( -92.69370383062505425, 88.66845928578038638, 75.30239583420048177 ) ) ;
#12266 = AXIS2_PLACEMENT_3D ( 'NONE', #66027, #36697, #8121 ) ;
#12267 = AXIS2_PLACEMENT_3D ( 'NONE', #39323, #50586, #5495 ) ;
#12268 = CARTESIAN_POINT ( 'NONE',  ( 96.15314808468748708, -208.0026889286704943, 87.52614583420047722 ) ) ;
#12269 = ORIENTED_EDGE ( 'NONE', *, *, #53324, .F. ) ;
#12270 = CARTESIAN_POINT ( 'NONE',  ( 0.000000000000000000, 80.28980883073758434, 16.65972982744962749 ) ) ;
#12271 = ORIENTED_EDGE ( 'NONE', *, *, #30817, .T. ) ;
#12272 = CARTESIAN_POINT ( 'NONE',  ( 0.000000000000000000, 0.000000000000000000, -54.99999999999998579 ) ) ;
#12273 = DIRECTION ( 'NONE',  ( 0.000000000000000000, 0.000000000000000000, 1.000000000000000000 ) ) ;
#12274 = ORIENTED_EDGE ( 'NONE', *, *, #61713, .F. ) ;
#12275 = EDGE_LOOP ( 'NONE', ( #755, #19788, #41213, #62907 ) ) ;
#12276 = EDGE_CURVE ( 'NONE', #59175, #17352, #47770, .T. ) ;
#12277 = CARTESIAN_POINT ( 'NONE',  ( 97.30629616937498838, -211.3315407142195852, 83.08114583420048405 ) ) ;
#12278 = CARTESIAN_POINT ( 'NONE',  ( 92.34999999999999432, 91.52997821335252127, 89.94708333333332462 ) ) ;
#12279 = FACE_OUTER_BOUND ( 'NONE', #6064, .T. ) ;
#12280 = EDGE_CURVE ( 'NONE', #42081, #61582, #52551, .T. ) ;
#12281 = CARTESIAN_POINT ( 'NONE',  ( 11.99999999999999822, 0.000000000000000000, 0.000000000000000000 ) ) ;
#12282 = CARTESIAN_POINT ( 'NONE',  ( 0.000000000000000000, 0.000000000000000000, 0.000000000000000000 ) ) ;
#12283 = CARTESIAN_POINT ( 'NONE',  ( 0.000000000000000000, -22.90783923731686045, 78.73519480814945837 ) ) ;
#12284 = CARTESIAN_POINT ( 'NONE',  ( 97.64999999999997726, -211.5299782133524502, 83.91458333333333997 ) ) ;
#12285 = ADVANCED_FACE ( 'NONE', ( #28806 ), #52102, .T. ) ;
#12286 = EDGE_LOOP ( 'NONE', ( #30026, #50422, #39105, #7565 ) ) ;
#12287 = MECHANICAL_DESIGN_GEOMETRIC_PRESENTATION_REPRESENTATION (  '', ( #1501 ), #48311 ) ;
#12288 = ORIENTED_EDGE ( 'NONE', *, *, #41402, .F. ) ;
#12289 = EDGE_LOOP ( 'NONE', ( #26646, #64260, #16529, #73487 ) ) ;
#12290 = ORIENTED_EDGE ( 'NONE', *, *, #16027, .T. ) ;
#12291 = LINE ( 'NONE', #46893, #32196 ) ;
#12292 = VECTOR ( 'NONE', #1357, 1000.000000000000000 ) ;
#12293 = CARTESIAN_POINT ( 'NONE',  ( -95.00000000000002842, 87.33691857156074434, 88.05531250086716000 ) ) ;
#12294 = ADVANCED_FACE ( 'NONE', ( #61918, #644 ), #69038, .T. ) ;
#12295 = DIRECTION ( 'NONE',  ( -1.000000000000000000, 0.000000000000000000, 0.000000000000000000 ) ) ;
#12296 = DIRECTION ( 'NONE',  ( 2.603472992746261562E-14, 2.546204323184492723E-14, -1.000000000000000000 ) ) ;
#12297 = CARTESIAN_POINT ( 'NONE',  ( 92.35000000000002274, -208.4700217866474645, 76.69145833506763665 ) ) ;
#12298 = CARTESIAN_POINT ( 'NONE',  ( 94.99999999999998579, 93.05995642670504253, 78.41125000000000966 ) ) ;
#12299 = ORIENTED_EDGE ( 'NONE', *, *, #60105, .T. ) ;
#12300 = CARTESIAN_POINT ( 'NONE',  ( 92.35000000000000853, 91.52997821335253548, 79.78708333333331382 ) ) ;
#12301 = VECTOR ( 'NONE', #25742, 1000.000000000000000 ) ;
#12302 = EDGE_LOOP ( 'NONE', ( #47372, #39568, #73380, #55596 ) ) ;
#12303 = DIRECTION ( 'NONE',  ( 0.000000000000000000, -0.9781476007338040235, -0.2079116908177671419 ) ) ;
#12304 = ORIENTED_EDGE ( 'NONE', *, *, #53815, .T. ) ;
#12305 = CARTESIAN_POINT ( 'NONE',  ( -92.35000000000005116, 91.52997821335253548, 88.54479166840097548 ) ) ;
#12306 = AXIS2_PLACEMENT_3D ( 'NONE', #29229, #41270, #35254 ) ;
#12307 = CARTESIAN_POINT ( 'NONE',  ( -96.15314808468752972, 91.99731107132950569, 82.07572916753382231 ) ) ;
#12308 = ADVANCED_FACE ( 'NONE', ( #44631 ), #73918, .T. ) ;
#12309 = CARTESIAN_POINT ( 'NONE',  ( 97.30629616937498838, 90.00000000000002842, 75.35531250086714294 ) ) ;
#12310 = ORIENTED_EDGE ( 'NONE', *, *, #10335, .T. ) ;
#12311 = CARTESIAN_POINT ( 'NONE',  ( 3.000000000000000000, 0.000000000000000000, 0.000000000000000000 ) ) ;
#12312 = CARTESIAN_POINT ( 'NONE',  ( 0.000000000000000000, -76.69515212746036070, 29.01471420065536932 ) ) ;
#12313 = CARTESIAN_POINT ( 'NONE',  ( 12.49999999999999822, -120.0000000000000000, -125.0000000000000000 ) ) ;
#12314 = DIRECTION ( 'NONE',  ( -1.427937372958396784E-15, 1.000000000000000000, -1.078060571631604545E-14 ) ) ;
#12315 = ORIENTED_EDGE ( 'NONE', *, *, #34357, .T. ) ;
#12316 = DIRECTION ( 'NONE',  ( 1.000000000000000000, -0.000000000000000000, -0.000000000000000000 ) ) ;
#12317 = CIRCLE ( 'NONE', #53159, 2.650000000000540812 ) ;
#12318 = CIRCLE ( 'NONE', #38726, 82.00000000000000000 ) ;
#12319 = CARTESIAN_POINT ( 'NONE',  ( -97.30629616937497417, -208.6684592857803011, 74.98489583420048632 ) ) ;
#12320 = ORIENTED_EDGE ( 'NONE', *, *, #16668, .F. ) ;
#12321 = ORIENTED_EDGE ( 'NONE', *, *, #35555, .F. ) ;
#12322 = DIRECTION ( 'NONE',  ( 0.000000000000000000, 0.000000000000000000, 1.000000000000000000 ) ) ;
#12323 = EDGE_CURVE ( 'NONE', #3905, #7045, #28055, .T. ) ;
#12324 = VERTEX_POINT ( 'NONE', #34073 ) ;
#12325 = ADVANCED_FACE ( 'NONE', ( #10401 ), #17522, .T. ) ;
#12326 = DIRECTION ( 'NONE',  ( -1.000000000000000000, -0.000000000000000000, -0.000000000000000000 ) ) ;
#12327 = DIRECTION ( 'NONE',  ( -1.000000000000000000, 0.000000000000000000, 0.000000000000000000 ) ) ;
#12328 = ORIENTED_EDGE ( 'NONE', *, *, #44729, .T. ) ;
#12329 = CARTESIAN_POINT ( 'NONE',  ( -92.69370383062498320, -209.9999999999999716, 86.94406250086716170 ) ) ;
#12330 = ORIENTED_EDGE ( 'NONE', *, *, #27570, .F. ) ;
#12331 = DIRECTION ( 'NONE',  ( 1.000000000000000000, 0.000000000000000000, -0.000000000000000000 ) ) ;
#12332 = FACE_OUTER_BOUND ( 'NONE', #15832, .T. ) ;
#12333 = EDGE_LOOP ( 'NONE', ( #28636, #35490, #11547, #71538 ) ) ;
#12334 = ORIENTED_EDGE ( 'NONE', *, *, #73461, .F. ) ;
#12335 = CARTESIAN_POINT ( 'NONE',  ( 0.000000000000000000, 6.555932627142952995, -37.01155633439051940 ) ) ;
#12336 = CARTESIAN_POINT ( 'NONE',  ( 0.000000000000000000, -30.84782396557201878, -21.32104025579148399 ) ) ;
#12337 = CARTESIAN_POINT ( 'NONE',  ( 96.15314808468748708, 88.00268892867053694, 84.13947916753380696 ) ) ;
#12338 = CARTESIAN_POINT ( 'NONE',  ( 10.00000000000000000, 10.74501242461282757, 35.92658777277515014 ) ) ;
#12339 = DIRECTION ( 'NONE',  ( 0.000000000000000000, -0.6494480483301739993, -0.7604059656000392575 ) ) ;
#12340 = DIRECTION ( 'NONE',  ( 2.628368902995164490E-16, 1.000000000000000000, 0.000000000000000000 ) ) ;
#12341 = DIRECTION ( 'NONE',  ( -1.000000000000000000, 0.000000000000000000, 0.000000000000000000 ) ) ;
#12342 = LINE ( 'NONE', #46938, #41619 ) ;
#12343 = CARTESIAN_POINT ( 'NONE',  ( -96.32500000000001705, 92.29496732002878900, 84.25854166840096582 ) ) ;
#12344 = DIRECTION ( 'NONE',  ( 0.000000000000000000, 0.9969173337331276308, 0.07845909572784873220 ) ) ;
#12345 =( BOUNDED_CURVE ( )  B_SPLINE_CURVE ( 2, ( #9749, #55611, #4133, #27024, #72876, #62387, #69132 ),
 .UNSPECIFIED., .F., .F. ) 
 B_SPLINE_CURVE_WITH_KNOTS ( ( 3, 2, 2, 3 ),
 ( 0.4656806970056959760, 0.4727362912391188665, 0.4797920567800012526, 0.4868478063929145838 ),
 .UNSPECIFIED. ) 
 CURVE ( )  GEOMETRIC_REPRESENTATION_ITEM ( )  RATIONAL_B_SPLINE_CURVE ( ( 0.9999934945994550795, 0.8660286565636856615, 1.000000000000000000, 0.8660254037844387076, 1.000000000000000000, 0.8660254037844387076, 1.000000000000000000 ) ) 
 REPRESENTATION_ITEM ( '' )  );
#12346 = CARTESIAN_POINT ( 'NONE',  ( -10.43921258969510824, -98.89258801967538659, 5.500000000000000000 ) ) ;
#12347 = DIRECTION ( 'NONE',  ( -0.000000000000000000, -0.000000000000000000, 1.000000000000000000 ) ) ;
#12348 = CARTESIAN_POINT ( 'NONE',  ( -97.30629616937501680, 90.00000000000004263, 89.00781250086714635 ) ) ;
#12349 = DIRECTION ( 'NONE',  ( -0.000000000000000000, -0.000000000000000000, 1.000000000000000000 ) ) ;
#12350 = VECTOR ( 'NONE', #39665, 999.9999999999998863 ) ;
#12351 = ADVANCED_FACE ( 'NONE', ( #23178 ), #16040, .T. ) ;
#12352 = DIRECTION ( 'NONE',  ( 0.000000000000000000, -1.224646799147353207E-16, 1.000000000000000000 ) ) ;
#12353 = VERTEX_POINT ( 'NONE', #62677 ) ;
#12354 = AXIS2_PLACEMENT_3D ( 'NONE', #20781, #33535, #73009 ) ;
#12355 = CARTESIAN_POINT ( 'NONE',  ( 11.99999999999999822, 36.73666225445988687, -65.58780272294035285 ) ) ;
#12356 = CARTESIAN_POINT ( 'NONE',  ( 0.000000000000000000, -12.93880638057258814, -76.41127070299285151 ) ) ;
#12357 = CARTESIAN_POINT ( 'NONE',  ( 97.65000000000000568, 91.52997821335252127, 77.03541666666666288 ) ) ;
#12358 = CARTESIAN_POINT ( 'NONE',  ( 92.35000000000000853, -209.9999999999999716, 88.73000000000000398 ) ) ;
#12359 = CARTESIAN_POINT ( 'NONE',  ( 0.000000000000000000, -35.92658777277517856, 10.74501242461269257 ) ) ;
#12360 = FACE_OUTER_BOUND ( 'NONE', #30054, .T. ) ;
#12361 = VECTOR ( 'NONE', #57112, 1000.000000000000000 ) ;
#12362 = CARTESIAN_POINT ( 'NONE',  ( 93.84685191531251292, -211.9973110713294489, 85.46239583420047836 ) ) ;
#12363 = ORIENTED_EDGE ( 'NONE', *, *, #57797, .T. ) ;
#12364 = EDGE_CURVE ( 'NONE', #52892, #42621, #2146, .T. ) ;
#12365 = ORIENTED_EDGE ( 'NONE', *, *, #8936, .T. ) ;
#12366 = EDGE_CURVE ( 'NONE', #63593, #18610, #40454, .T. ) ;
#12367 = CARTESIAN_POINT ( 'NONE',  ( -93.67499999999998295, -207.7050326799711968, 85.97833333333332462 ) ) ;
#12368 = EDGE_LOOP ( 'NONE', ( #66122, #19417, #51039, #33268 ) ) ;
#12369 = PLANE ( 'NONE',  #18546 ) ;
#12370 = CARTESIAN_POINT ( 'NONE',  ( 92.69370383062501162, -211.3315407142195852, 75.09072916753380866 ) ) ;
#12371 = ORIENTED_EDGE ( 'NONE', *, *, #11795, .T. ) ;
#12372 = CARTESIAN_POINT ( 'NONE',  ( 95.00000000000000000, -212.6630814284392557, 80.43531250086715545 ) ) ;
#12373 = EDGE_CURVE ( 'NONE', #42450, #53064, #4794, .T. ) ;
#12374 = ORIENTED_EDGE ( 'NONE', *, *, #43581, .T. ) ;
#12375 = CARTESIAN_POINT ( 'NONE',  ( 10.00000000000000000, 0.000000000000000000, 0.000000000000000000 ) ) ;
#12376 = ORIENTED_EDGE ( 'NONE', *, *, #72075, .F. ) ;
#12377 = ORIENTED_EDGE ( 'NONE', *, *, #46328, .T. ) ;
#12378 = DIRECTION ( 'NONE',  ( 1.000000000000000000, 0.000000000000000000, 0.000000000000000000 ) ) ;
#12379 = CARTESIAN_POINT ( 'NONE',  ( 93.67500000000001137, -207.7050326799711968, 80.36916666666665776 ) ) ;
#12380 = VERTEX_POINT ( 'NONE', #16794 ) ;
#12381 = DIRECTION ( 'NONE',  ( 0.000000000000000000, 0.000000000000000000, 1.000000000000000000 ) ) ;
#12382 = CARTESIAN_POINT ( 'NONE',  ( 95.00000000000000000, -213.0599564267049857, 85.79312500173431033 ) ) ;
#12383 = CARTESIAN_POINT ( 'NONE',  ( 97.64999999999999147, 90.00000000000002842, 88.41249999999999432 ) ) ;
#12384 = ORIENTED_EDGE ( 'NONE', *, *, #9097, .F. ) ;
#12385 = DIRECTION ( 'NONE',  ( 0.000000000000000000, -0.07845909572783058006, -0.9969173337331290741 ) ) ;
#12386 = APPLICATION_CONTEXT ( 'automotive_design' ) ;
#12387 = AXIS2_PLACEMENT_3D ( 'NONE', #1848, #48405, #30366 ) ;
#12388 = VERTEX_POINT ( 'NONE', #51358 ) ;
#12389 = EDGE_LOOP ( 'NONE', ( #67681, #59757, #41242, #11663 ) ) ;
#12390 = DIRECTION ( 'NONE',  ( 0.000000000000000000, -0.7071067811865389130, -0.7071067811865561215 ) ) ;
#12391 = EDGE_CURVE ( 'NONE', #56950, #55462, #66922, .T. ) ;
#12392 = VERTEX_POINT ( 'NONE', #63047 ) ;
#12393 = CARTESIAN_POINT ( 'NONE',  ( 97.64999999999999147, 90.00000000000002842, 84.68187500173429783 ) ) ;
#12394 = PRODUCT_DEFINITION_FORMATION_WITH_SPECIFIED_SOURCE ( 'ANY', '', #72776, .NOT_KNOWN. ) ;
#12395 = ORIENTED_EDGE ( 'NONE', *, *, #2441, .F. ) ;
#12396 = ORIENTED_EDGE ( 'NONE', *, *, #21450, .F. ) ;
#12397 = DIRECTION ( 'NONE',  ( 0.000000000000000000, 0.000000000000000000, 1.000000000000000000 ) ) ;
#12398 = CARTESIAN_POINT ( 'NONE',  ( 0.000000000000000000, 0.000000000000000000, 0.000000000000000000 ) ) ;
#12399 = VERTEX_POINT ( 'NONE', #11869 ) ;
#12400 = CIRCLE ( 'NONE', #31601, 31.99999999999998579 ) ;
#12401 = VERTEX_POINT ( 'NONE', #57757 ) ;
#12402 = ORIENTED_EDGE ( 'NONE', *, *, #10162, .T. ) ;
#12403 = DIRECTION ( 'NONE',  ( 0.000000000000000000, 0.5224985647159500202, -0.8526401643540915121 ) ) ;
#12404 = CARTESIAN_POINT ( 'NONE',  ( -96.32500000000001705, 87.70503267997129626, 86.93083333333332519 ) ) ;
#12405 = EDGE_CURVE ( 'NONE', #6672, #18572, #33323, .T. ) ;
#12406 = VERTEX_POINT ( 'NONE', #68673 ) ;
#12407 = EDGE_CURVE ( 'NONE', #65728, #61974, #58564, .T. ) ;
#12408 = DIRECTION ( 'NONE',  ( 0.000000000000000000, 0.000000000000000000, 1.000000000000000000 ) ) ;
#12409 = VECTOR ( 'NONE', #58516, 1000.000000000000000 ) ;
#12410 = LINE ( 'NONE', #6775, #16680 ) ;
#12411 = ORIENTED_EDGE ( 'NONE', *, *, #19614, .F. ) ;
#12412 = CARTESIAN_POINT ( 'NONE',  ( 0.000000000000000000, 23.59884966291521380, 12.14883922797262805 ) ) ;
#12413 = CARTESIAN_POINT ( 'NONE',  ( -94.99999999999997158, -207.3369185715606307, 84.40406250086712703 ) ) ;
#12414 = EDGE_LOOP ( 'NONE', ( #55218, #7510, #59284, #28388 ) ) ;
#12415 = EDGE_CURVE ( 'NONE', #39808, #19228, #39353, .T. ) ;
#12416 = MANIFOLD_SOLID_BREP ( 'Fillet1', #39184 ) ;
#12417 = VECTOR ( 'NONE', #64516, 1000.000000000000000 ) ;
#12418 = DIRECTION ( 'NONE',  ( -0.000000000000000000, -0.000000000000000000, -1.000000000000000000 ) ) ;
#12419 = CARTESIAN_POINT ( 'NONE',  ( 15.00000000000000000, 0.000000000000000000, 0.000000000000000000 ) ) ;
#12420 = DIRECTION ( 'NONE',  ( 1.000000000000000000, 0.000000000000000000, -0.000000000000000000 ) ) ;
#12421 = CARTESIAN_POINT ( 'NONE',  ( -97.30629616937497417, -208.6684592857803295, 74.98489583420048632 ) ) ;
#12422 = CARTESIAN_POINT ( 'NONE',  ( 99.99999999999998579, 95.00000000000002842, 90.00000000000000000 ) ) ;
#12423 = DIRECTION ( 'NONE',  ( -1.000000000000000000, -0.000000000000000000, -0.000000000000000000 ) ) ;
#12424 = VECTOR ( 'NONE', #17892, 1000.000000000000000 ) ;
#12425 = DIRECTION ( 'NONE',  ( -0.000000000000000000, -0.000000000000000000, -1.000000000000000000 ) ) ;
#12426 = DIRECTION ( 'NONE',  ( 0.000000000000000000, 1.224646799147353207E-16, -1.000000000000000000 ) ) ;
#12427 = DIRECTION ( 'NONE',  ( -1.000000000000000000, 0.000000000000000000, 0.000000000000000000 ) ) ;
#12428 = CARTESIAN_POINT ( 'NONE',  ( 96.73972734126404305, -208.4859488783623362, 74.79348190356850523 ) ) ;
#12429 = CARTESIAN_POINT ( 'NONE',  ( -92.69370383062502583, 88.66845928578038638, 79.74739583420047495 ) ) ;
#12430 = DIRECTION ( 'NONE',  ( 0.000000000000000000, 0.000000000000000000, 1.000000000000000000 ) ) ;
#12431 = DIRECTION ( 'NONE',  ( -0.000000000000000000, -0.000000000000000000, -1.000000000000000000 ) ) ;
#12432 = ORIENTED_EDGE ( 'NONE', *, *, #17815, .T. ) ;
#12433 = CARTESIAN_POINT ( 'NONE',  ( 10.00000000000000000, 75.16055320797030959, 18.89407956138283851 ) ) ;
#12434 = AXIS2_PLACEMENT_3D ( 'NONE', #18497, #51974, #69273 ) ;
#12435 = CARTESIAN_POINT ( 'NONE',  ( -3.000000000000000000, 20.85821328998741109, 10.92862929874522315 ) ) ;
#12436 = DIRECTION ( 'NONE',  ( -1.000000000000000000, -0.000000000000000000, -0.000000000000000000 ) ) ;
#12437 = LINE ( 'NONE', #40279, #4649 ) ;
#12438 = DIRECTION ( 'NONE',  ( -1.000000000000000000, 0.000000000000000000, 0.000000000000000000 ) ) ;
#12439 = CARTESIAN_POINT ( 'NONE',  ( -92.35002849302227901, 91.52999466380659044, 87.27479280632984171 ) ) ;
#12440 = CARTESIAN_POINT ( 'NONE',  ( -93.84685191531248449, -208.0026889286704943, 77.52489583420047836 ) ) ;
#12441 = DIRECTION ( 'NONE',  ( 1.000000000000000000, -0.000000000000000000, -0.000000000000000000 ) ) ;
#12442 = ORIENTED_EDGE ( 'NONE', *, *, #43340, .T. ) ;
#12443 = CARTESIAN_POINT ( 'NONE',  ( 10.00000000000000000, 40.98264845739749518, 9.188173127307441845 ) ) ;
#12444 = CARTESIAN_POINT ( 'NONE',  ( 0.000000000000000000, 0.000000000000000000, 0.000000000000000000 ) ) ;
#12445 = FILL_AREA_STYLE ('',( #23732 ) ) ;
#12446 = AXIS2_PLACEMENT_3D ( 'NONE', #32033, #71889, #15119 ) ;
#12447 = FACE_BOUND ( 'NONE', #69296, .T. ) ;
#12448 = CARTESIAN_POINT ( 'NONE',  ( 10.00000000000000000, 0.000000000000000000, 0.000000000000000000 ) ) ;
#12449 = EDGE_CURVE ( 'NONE', #46611, #70418, #45386, .T. ) ;
#12450 = EDGE_CURVE ( 'NONE', #12353, #27755, #59230, .T. ) ;
#12451 = FACE_OUTER_BOUND ( 'NONE', #66302, .T. ) ;
#12452 = ORIENTED_EDGE ( 'NONE', *, *, #63526, .F. ) ;
#12454 = EDGE_CURVE ( 'NONE', #44954, #13102, #7081, .T. ) ;
#12453 = DIRECTION ( 'NONE',  ( -1.000000000000000000, -0.000000000000000000, -0.000000000000000000 ) ) ;
#12455 =( LENGTH_UNIT ( ) NAMED_UNIT ( * ) SI_UNIT ( .MILLI., .METRE. ) );
#12456 = ORIENTED_EDGE ( 'NONE', *, *, #61890, .F. ) ;
#12457 = CIRCLE ( 'NONE', #55665, 77.49900000000002365 ) ;
#12458 = CARTESIAN_POINT ( 'NONE',  ( 96.15314808468748708, -208.0026889286704943, 83.71614583420047495 ) ) ;
#12459 = DIRECTION ( 'NONE',  ( 0.000000000000000000, 0.000000000000000000, 1.000000000000000000 ) ) ;
#12460 = VECTOR ( 'NONE', #34743, 1000.000000000000114 ) ;
#12461 = ORIENTED_EDGE ( 'NONE', *, *, #21923, .F. ) ;
#12462 = FACE_OUTER_BOUND ( 'NONE', #16123, .T. ) ;
#12463 = EDGE_CURVE ( 'NONE', #38967, #23893, #57446, .T. ) ;
#12464 = ORIENTED_EDGE ( 'NONE', *, *, #38356, .T. ) ;
#12465 = AXIS2_PLACEMENT_3D ( 'NONE', #50149, #5071, #9942 ) ;
#12466 = CARTESIAN_POINT ( 'NONE',  ( 0.000000000000000000, 0.000000000000000000, 0.000000000000000000 ) ) ;
#12467 = ORIENTED_EDGE ( 'NONE', *, *, #35205, .F. ) ;
#12468 = AXIS2_PLACEMENT_3D ( 'NONE', #41030, #11325, #6444 ) ;
#12469 = CARTESIAN_POINT ( 'NONE',  ( -92.69370383062502583, 91.33154071421968467, 81.91697916753381037 ) ) ;
#12470 = ORIENTED_EDGE ( 'NONE', *, *, #18350, .F. ) ;
#12471 = ORIENTED_EDGE ( 'NONE', *, *, #21384, .F. ) ;
#12472 = CARTESIAN_POINT ( 'NONE',  ( -100.0000000000000142, 95.00000000000002842, -90.00000000000000000 ) ) ;
#12473 = ORIENTED_EDGE ( 'NONE', *, *, #42427, .F. ) ;
#12474 = CARTESIAN_POINT ( 'NONE',  ( 11.99999999999999822, 0.000000000000000000, 0.000000000000000000 ) ) ;
#12475 = DIRECTION ( 'NONE',  ( 0.000000000000000000, 0.000000000000000000, -1.000000000000000000 ) ) ;
#12476 = ORIENTED_EDGE ( 'NONE', *, *, #20489, .T. ) ;
#12477 = CARTESIAN_POINT ( 'NONE',  ( 94.99999999999998579, 86.94004357329502852, 80.71312500173429783 ) ) ;
#12478 = EDGE_CURVE ( 'NONE', #65118, #21621, #11754, .T. ) ;
#12479 = ORIENTED_EDGE ( 'NONE', *, *, #59881, .T. ) ;
#12480 = CARTESIAN_POINT ( 'NONE',  ( -8.000000000000007105, -1.142349898368590025E-14, -6.370018489464426943E-15 ) ) ;
#12481 = EDGE_CURVE ( 'NONE', #52158, #54849, #31010, .T. ) ;
#12482 = ORIENTED_EDGE ( 'NONE', *, *, #56436, .T. ) ;
#12483 = AXIS2_PLACEMENT_3D ( 'NONE', #53927, #26816, #26452 ) ;
#12484 = VERTEX_POINT ( 'NONE', #65251 ) ;
#12485 = ORIENTED_EDGE ( 'NONE', *, *, #7828, .F. ) ;
#12486 = CARTESIAN_POINT ( 'NONE',  ( 96.15314808468750130, -211.9973110713294489, 80.96447916753380980 ) ) ;
#12487 = APPLICATION_PROTOCOL_DEFINITION ( 'draft international standard', 'automotive_design', 1998, #29621 ) ;
#12488 = CARTESIAN_POINT ( 'NONE',  ( -93.67499999999998295, -207.7050326799711968, 76.45333333333333314 ) ) ;
#12489 = CARTESIAN_POINT ( 'NONE',  ( -93.62329079302905654, -212.2908000246593474, 75.00000000000000000 ) ) ;
#12490 = CARTESIAN_POINT ( 'NONE',  ( 97.64999999999999147, 90.00000000000002842, 85.23749999999999716 ) ) ;
#12491 = CARTESIAN_POINT ( 'NONE',  ( 0.000000000000000000, 0.000000000000000000, -125.0000000000000000 ) ) ;
#12492 = FACE_OUTER_BOUND ( 'NONE', #73046, .T. ) ;
#12493 = CARTESIAN_POINT ( 'NONE',  ( 0.000000000000000000, -14.66109333815410487, -73.73191006444587003 ) ) ;
#12494 = CARTESIAN_POINT ( 'NONE',  ( -97.30629616937497417, -211.3315407142195852, 85.25072916753379104 ) ) ;
#12495 = CARTESIAN_POINT ( 'NONE',  ( -92.69370383062502583, 88.66845928578038638, 83.08114583420048405 ) ) ;
#12496 = EDGE_CURVE ( 'NONE', #31431, #20705, #29900, .T. ) ;
#12497 = VERTEX_POINT ( 'NONE', #53966 ) ;
#12498 = ADVANCED_FACE ( 'NONE', ( #53220 ), #46468, .T. ) ;
#12499 = AXIS2_PLACEMENT_3D ( 'NONE', #69473, #24722, #25088 ) ;
#12500 = CARTESIAN_POINT ( 'NONE',  ( 97.30629616937498838, 91.33154071421968467, 85.56822916753380071 ) ) ;
#12501 = ORIENTED_EDGE ( 'NONE', *, *, #28930, .T. ) ;
#12502 = DIRECTION ( 'NONE',  ( 0.000000000000000000, 0.000000000000000000, -1.000000000000000000 ) ) ;
#12503 = CARTESIAN_POINT ( 'NONE',  ( -3.000000000000000000, 23.59884966291521380, 12.14883922797262805 ) ) ;
#12504 = LINE ( 'NONE', #35440, #28986 ) ;
#12505 = CARTESIAN_POINT ( 'NONE',  ( 10.00000000000000000, 37.22597642581158084, -5.202137450156524068 ) ) ;
#12506 = CARTESIAN_POINT ( 'NONE',  ( 6.000000000000000000, -22.90783923731685334, 78.73519480814945837 ) ) ;
#12507 = CARTESIAN_POINT ( 'NONE',  ( -97.30629616937497417, -208.6684592857803295, 87.68489583420047495 ) ) ;
#12508 = CARTESIAN_POINT ( 'NONE',  ( -92.34999999999999432, -209.9999999999999716, 76.98250000000000171 ) ) ;
#12509 = CARTESIAN_POINT ( 'NONE',  ( 10.00000000000000000, -35.92658777277502935, -10.74501242461320594 ) ) ;
#12510 = CARTESIAN_POINT ( 'NONE',  ( 11.99999999999999822, 41.76937507738788469, 62.50329211542452157 ) ) ;
#12511 = CARTESIAN_POINT ( 'NONE',  ( 11.99999999999999822, 41.76106447765489094, 62.50884508063442269 ) ) ;
#12512 = ORIENTED_EDGE ( 'NONE', *, *, #5474, .F. ) ;
#12513 = CIRCLE ( 'NONE', #52119, 31.99999999999998934 ) ;
#12514 = ORIENTED_EDGE ( 'NONE', *, *, #68793, .T. ) ;
#12515 = CARTESIAN_POINT ( 'NONE',  ( -92.35000000000005116, 88.47002178664754979, 78.83458333333334167 ) ) ;
#12516 = CARTESIAN_POINT ( 'NONE',  ( -96.15314808468751551, 88.00268892867056536, 89.11364583420048291 ) ) ;
#12517 = CARTESIAN_POINT ( 'NONE',  ( 0.000000000000000000, 0.000000000000000000, 40.80000000000001847 ) ) ;
#12518 = DIRECTION ( 'NONE',  ( 0.000000000000000000, 0.000000000000000000, 1.000000000000000000 ) ) ;
#12519 = LINE ( 'NONE', #46375, #18103 ) ;
#12520 = VECTOR ( 'NONE', #65300, 1000.000000000000000 ) ;
#12521 = DIRECTION ( 'NONE',  ( 0.000000000000000000, 0.000000000000000000, 1.000000000000000000 ) ) ;
#12522 = CIRCLE ( 'NONE', #18532, 42.00000000000000000 ) ;
#12523 = ORIENTED_EDGE ( 'NONE', *, *, #21666, .T. ) ;
#12524 = CARTESIAN_POINT ( 'NONE',  ( -21.33958957442910886, -129.9559990355020034, 5.500000000000000000 ) ) ;
#12525 = CARTESIAN_POINT ( 'NONE',  ( -92.35000000000003695, 90.00000000000004263, 90.00000000000000000 ) ) ;
#12526 = AXIS2_PLACEMENT_3D ( 'NONE', #54334, #31385, #8839 ) ;
#12527 = CIRCLE ( 'NONE', #71327, 82.00000000000000000 ) ;
#12528 = CARTESIAN_POINT ( 'NONE',  ( 0.000000000000000000, -120.0000000000000000, -2.500000000000000000 ) ) ;
#12529 = CARTESIAN_POINT ( 'NONE',  ( 0.000000000000000000, 0.000000000000000000, 0.000000000000000000 ) ) ;
#12530 = DIRECTION ( 'NONE',  ( 0.000000000000000000, 0.9510565162951523099, 0.3090169943749515591 ) ) ;
#12531 = CARTESIAN_POINT ( 'NONE',  ( 12.69589495141918611, -96.69089767102708777, 5.500000000000000000 ) ) ;
#12532 = CARTESIAN_POINT ( 'NONE',  ( -94.99999999999997158, -207.3369185715606307, 86.46781250086716852 ) ) ;
#12533 = SURFACE_STYLE_USAGE ( .BOTH. , #47854 ) ;
#12534 = DIRECTION ( 'NONE',  ( -1.000000000000000000, 7.677074106448950501E-15, 2.598394312951952234E-14 ) ) ;
#12535 = CARTESIAN_POINT ( 'NONE',  ( 96.15314808468748708, 88.00268892867053694, 77.31322916753381946 ) ) ;
#12536 = AXIS2_PLACEMENT_3D ( 'NONE', #23603, #17959, #57449 ) ;
#12537 = EDGE_CURVE ( 'NONE', #24073, #11102, #63775, .T. ) ;
#12538 = CARTESIAN_POINT ( 'NONE',  ( -93.84685191531248449, -208.0026889286704943, 77.52489583420047836 ) ) ;
#12539 = DIRECTION ( 'NONE',  ( 0.000000000000000000, 0.07845909572784512398, -0.9969173337331279638 ) ) ;
#12540 = ORIENTED_EDGE ( 'NONE', *, *, #7385, .T. ) ;
#12541 = CARTESIAN_POINT ( 'NONE',  ( -10.00000000000000000, 0.000000000000000000, 0.000000000000000000 ) ) ;
#12542 = CARTESIAN_POINT ( 'NONE',  ( -16.06301359042743115, -102.7814171781257357, -5.500000000000000000 ) ) ;
#12543 = DIRECTION ( 'NONE',  ( 0.000000000000000000, 0.3090169943749560555, 0.9510565162951506446 ) ) ;
#12544 = EDGE_CURVE ( 'NONE', #42337, #34606, #5830, .T. ) ;
#12545 = EDGE_CURVE ( 'NONE', #22221, #32803, #53780, .T. ) ;
#12546 = EDGE_CURVE ( 'NONE', #23968, #69024, #58481, .T. ) ;
#12547 = CARTESIAN_POINT ( 'NONE',  ( -96.15314808468752972, 91.99731107132950569, 76.36072916753381890 ) ) ;
#12548 = CARTESIAN_POINT ( 'NONE',  ( 97.30629616937498838, -209.9999999999999716, 76.62531250086713897 ) ) ;
#12549 = ORIENTED_EDGE ( 'NONE', *, *, #64209, .T. ) ;
#12550 =( NAMED_UNIT ( * ) PLANE_ANGLE_UNIT ( ) SI_UNIT ( $, .RADIAN. ) );
#12551 = ORIENTED_EDGE ( 'NONE', *, *, #48136, .F. ) ;
#12552 = ADVANCED_FACE ( 'NONE', ( #47211 ), #41559, .F. ) ;
#12553 =( BOUNDED_CURVE ( )  B_SPLINE_CURVE ( 2, ( #13019, #19032, #20136, #65287, #37074, #24678, #60022 ),
 .UNSPECIFIED., .F., .F. ) 
 B_SPLINE_CURVE_WITH_KNOTS ( ( 3, 2, 2, 3 ),
 ( 0.8541666666666666297, 0.8611111111111110494, 0.8680555555555554692, 0.8749999999999997780 ),
 .UNSPECIFIED. ) 
 CURVE ( )  GEOMETRIC_REPRESENTATION_ITEM ( )  RATIONAL_B_SPLINE_CURVE ( ( 1.000000000000000000, 0.8660254037844387076, 1.000000000000000000, 0.8660254037844387076, 1.000000000000000000, 0.8660254037844430375, 0.9999999999999956701 ) ) 
 REPRESENTATION_ITEM ( '' )  );
#12554 = CARTESIAN_POINT ( 'NONE',  ( -10.00000000000000000, 0.000000000000000000, 0.000000000000000000 ) ) ;
#12556 = VERTEX_POINT ( 'NONE', #58866 ) ;
#12555 = VECTOR ( 'NONE', #49148, 1000.000000000000000 ) ;
#12557 = EDGE_CURVE ( 'NONE', #69079, #38213, #24643, .T. ) ;
#12558 = CARTESIAN_POINT ( 'NONE',  ( 15.00000000000000000, 23.49999999999999645, -1.500000000000003997 ) ) ;
#12559 = AXIS2_PLACEMENT_3D ( 'NONE', #19867, #8606, #2990 ) ;
#12560 = ORIENTED_EDGE ( 'NONE', *, *, #37881, .F. ) ;
#12561 = EDGE_LOOP ( 'NONE', ( #668, #66677, #65895, #39863 ) ) ;
#12562 = ORIENTED_EDGE ( 'NONE', *, *, #21288, .F. ) ;
#12563 = CARTESIAN_POINT ( 'NONE',  ( 19.12409105625795291, -101.5943176906707919, -5.500000000000000000 ) ) ;
#12564 = VERTEX_POINT ( 'NONE', #42677 ) ;
#12565 = ORIENTED_EDGE ( 'NONE', *, *, #32351, .T. ) ;
#12566 = CARTESIAN_POINT ( 'NONE',  ( 94.99999999999998579, 87.33691857156068750, 82.34031250086714238 ) ) ;
#12567 = VECTOR ( 'NONE', #67290, 1000.000000000000000 ) ;
#12568 = LINE ( 'NONE', #16835, #15549 ) ;
#12569 = EDGE_CURVE ( 'NONE', #26913, #35679, #33378, .T. ) ;
#12571 = CARTESIAN_POINT ( 'NONE',  ( 92.35000000000000853, -209.9999999999999716, 90.00000000000000000 ) ) ;
#12570 = AXIS2_PLACEMENT_3D ( 'NONE', #72663, #44869, #56523 ) ;
#12572 = ORIENTED_EDGE ( 'NONE', *, *, #71960, .T. ) ;
#12573 = ORIENTED_EDGE ( 'NONE', *, *, #1081, .F. ) ;
#12574 = EDGE_LOOP ( 'NONE', ( #28641, #39861, #16083, #61858 ) ) ;
#12575 = CARTESIAN_POINT ( 'NONE',  ( 10.00000000000000000, 55.20638768913760686, 51.02545421589343988 ) ) ;
#12577 = ORIENTED_EDGE ( 'NONE', *, *, #14231, .F. ) ;
#12576 = ADVANCED_FACE ( 'NONE', ( #48315 ), #65615, .T. ) ;
#12579 = EDGE_CURVE ( 'NONE', #46805, #36613, #38225, .T. ) ;
#12578 = CIRCLE ( 'NONE', #17419, 37.49900000000000944 ) ;
#12580 = CARTESIAN_POINT ( 'NONE',  ( -94.99999999999997158, -206.9400435732949575, 85.39624999999998067 ) ) ;
#12581 = LINE ( 'NONE', #6936, #12292 ) ;
#12582 = DIRECTION ( 'NONE',  ( 0.000000000000000000, 0.3090169943749482839, -0.9510565162951533091 ) ) ;
#12583 = CARTESIAN_POINT ( 'NONE',  ( 0.000000000000000000, -63.18004540532994184, -44.88180994100444821 ) ) ;
#12584 = CARTESIAN_POINT ( 'NONE',  ( 0.000000000000000000, 0.000000000000000000, -1.199999999999999956 ) ) ;
#12585 = DIRECTION ( 'NONE',  ( 0.000000000000000000, -0.2334453638559125521, 0.9723699203976750027 ) ) ;
#12586 = CARTESIAN_POINT ( 'NONE',  ( -96.32499999999996021, -212.2949673200287179, 79.39020833506762642 ) ) ;
#12587 = VERTEX_POINT ( 'NONE', #31752 ) ;
#12588 = CARTESIAN_POINT ( 'NONE',  ( -7.572224309238338336, -145.4393675041377492, 2.500000000000000000 ) ) ;
#12589 = EDGE_CURVE ( 'NONE', #2929, #54905, #20101, .T. ) ;
#12590 = VECTOR ( 'NONE', #61790, 1000.000000000000000 ) ;
#12591 = ORIENTED_EDGE ( 'NONE', *, *, #72027, .F. ) ;
#12593 = CARTESIAN_POINT ( 'NONE',  ( -92.35000000000005116, 91.52997821335253548, 77.11479166840095445 ) ) ;
#12592 = CARTESIAN_POINT ( 'NONE',  ( 94.99999999999998579, 86.94004357329500010, 79.44312500173428759 ) ) ;
#12594 = ORIENTED_EDGE ( 'NONE', *, *, #36762, .F. ) ;
#12595 = CARTESIAN_POINT ( 'NONE',  ( 97.30629616937498838, 88.66845928578037217, 81.17614583420048291 ) ) ;
#12596 = FACE_OUTER_BOUND ( 'NONE', #1778, .T. ) ;
#12597 = CARTESIAN_POINT ( 'NONE',  ( 0.000000000000000000, 1.467624384280029837, 2.541999999999997151 ) ) ;
#12598 = CARTESIAN_POINT ( 'NONE',  ( 11.99999999999999822, 0.000000000000000000, 0.000000000000000000 ) ) ;
#12599 = DIRECTION ( 'NONE',  ( 0.000000000000000000, -0.8660254037844427044, -0.4999999999999931166 ) ) ;
#12600 = ORIENTED_EDGE ( 'NONE', *, *, #36812, .F. ) ;
#12601 = DIRECTION ( 'NONE',  ( -1.000000000000000000, 0.000000000000000000, 0.000000000000000000 ) ) ;
#12602 = CARTESIAN_POINT ( 'NONE',  ( -97.65000000000001990, 90.00000000000004263, 90.00000000000000000 ) ) ;
#12603 = EDGE_LOOP ( 'NONE', ( #62496, #62040, #73006, #17716 ) ) ;
#12604 = VERTEX_POINT ( 'NONE', #43443 ) ;
#12605 = FACE_OUTER_BOUND ( 'NONE', #27076, .T. ) ;
#12606 = CARTESIAN_POINT ( 'NONE',  ( -4.828573329308746942, -2.985724580418009921, -1.878862934774787830 ) ) ;
#12607 = CARTESIAN_POINT ( 'NONE',  ( -92.34999999999999432, -209.9999999999999716, 75.71250000000000568 ) ) ;
#12608 = CARTESIAN_POINT ( 'NONE',  ( -92.69370383062498320, -211.3315407142195852, 76.09614583420048461 ) ) ;
#12609 = ORIENTED_EDGE ( 'NONE', *, *, #47855, .T. ) ;
#12610 = CARTESIAN_POINT ( 'NONE',  ( 11.99999999999999822, 36.72794159290241822, 65.59268652807223532 ) ) ;
#12611 = AXIS2_PLACEMENT_3D ( 'NONE', #13029, #34871, #40504 ) ;
#12612 = CARTESIAN_POINT ( 'NONE',  ( 12.00000000000000000, 26.49999999999999645, 1.499999999999995781 ) ) ;
#12613 = DIRECTION ( 'NONE',  ( 0.000000000000000000, 0.000000000000000000, 1.000000000000000000 ) ) ;
#12614 = CARTESIAN_POINT ( 'NONE',  ( -92.34999999999999432, -210.0000000334413528, 87.85687500050293863 ) ) ;
#12615 = DIRECTION ( 'NONE',  ( 0.000000000000000000, 0.000000000000000000, 1.000000000000000000 ) ) ;
#12616 = CARTESIAN_POINT ( 'NONE',  ( 11.99999999999999822, 0.000000000000000000, 0.000000000000000000 ) ) ;
#12617 = FACE_OUTER_BOUND ( 'NONE', #73215, .T. ) ;
#12618 = FACE_OUTER_BOUND ( 'NONE', #20234, .T. ) ;
#12619 = DIRECTION ( 'NONE',  ( 0.000000000000000000, 0.000000000000000000, 1.000000000000000000 ) ) ;
#12620 = LINE ( 'NONE', #35557, #53844 ) ;
#12621 = AXIS2_PLACEMENT_3D ( 'NONE', #51765, #58509, #312 ) ;
#12622 = VECTOR ( 'NONE', #64651, 1000.000000000000000 ) ;
#12623 = CARTESIAN_POINT ( 'NONE',  ( 92.69370383062498320, 90.00000000000002842, 86.62656250086715204 ) ) ;
#12624 = CARTESIAN_POINT ( 'NONE',  ( -97.30629616937497417, -208.6684592857803295, 85.30364583420048064 ) ) ;
#12625 = CARTESIAN_POINT ( 'NONE',  ( 10.00000000000000000, -71.27951684758046724, 30.41916302227088309 ) ) ;
#12626 = ORIENTED_EDGE ( 'NONE', *, *, #476, .T. ) ;
#12627 = LINE ( 'NONE', #35565, #12417 ) ;
#12628 = CARTESIAN_POINT ( 'NONE',  ( -97.64999999999994884, -211.5299782133524502, 80.52791666666665549 ) ) ;
#12629 = EDGE_CURVE ( 'NONE', #58250, #48071, #54697, .T. ) ;
#12630 = CARTESIAN_POINT ( 'NONE',  ( -93.84685191531252713, 88.00268892867056536, 77.78947916753381264 ) ) ;
#12631 = AXIS2_PLACEMENT_3D ( 'NONE', #60821, #4062, #26596 ) ;
#12632 = EDGE_CURVE ( 'NONE', #32195, #54291, #22912, .T. ) ;
#12633 = AXIS2_PLACEMENT_3D ( 'NONE', #54499, #2299, #66886 ) ;
#12634 = EDGE_CURVE ( 'NONE', #10395, #2456, #65815, .T. ) ;
#12635 = EDGE_CURVE ( 'NONE', #7033, #69733, #58607, .T. ) ;
#12636 = CARTESIAN_POINT ( 'NONE',  ( 92.69370383062501162, -209.9999999999999716, 88.37281250086715545 ) ) ;
#12637 = ORIENTED_EDGE ( 'NONE', *, *, #41917, .T. ) ;
#12638 = VERTEX_POINT ( 'NONE', #60352 ) ;
#12639 = ORIENTED_EDGE ( 'NONE', *, *, #6066, .F. ) ;
#12640 = CARTESIAN_POINT ( 'NONE',  ( 15.00000000000000000, 23.59884966291538078, 12.14883922797231008 ) ) ;
#12641 = FACE_OUTER_BOUND ( 'NONE', #50822, .T. ) ;
#12642 = VECTOR ( 'NONE', #4324, 1000.000000000000000 ) ;
#12643 = EDGE_LOOP ( 'NONE', ( #63711, #55104, #22653, #14971 ) ) ;
#12644 = ORIENTED_EDGE ( 'NONE', *, *, #18438, .T. ) ;
#12645 = EDGE_CURVE ( 'NONE', #34836, #11723, #49424, .T. ) ;
#12646 = CARTESIAN_POINT ( 'NONE',  ( 93.84685191531251292, -211.9973110713294489, 80.38239583420048007 ) ) ;
#12647 = CARTESIAN_POINT ( 'NONE',  ( 10.00000000000000000, 71.21200624218852226, -40.65526001592539984 ) ) ;
#12648 = DIRECTION ( 'NONE',  ( 0.000000000000000000, 0.2334453638558990629, 0.9723699203976782224 ) ) ;
#12649 = CARTESIAN_POINT ( 'NONE',  ( -97.64999999999996305, -209.9999999999999716, 77.37937500173428873 ) ) ;
#12650 = CARTESIAN_POINT ( 'NONE',  ( 10.00000000000000000, -58.39081064771713869, -50.95692526931392052 ) ) ;
#12651 = MANIFOLD_SOLID_BREP ( 'Boss-Extrude2', #46426 ) ;
#12652 = CARTESIAN_POINT ( 'NONE',  ( 11.99999999999999822, 71.87247863392413194, 39.47590169984869846 ) ) ;
#12653 = CARTESIAN_POINT ( 'NONE',  ( 95.00000000000000000, -213.0599564267049857, 85.07874999999999943 ) ) ;
#12654 = ORIENTED_EDGE ( 'NONE', *, *, #35333, .T. ) ;
#12655 = ORIENTED_EDGE ( 'NONE', *, *, #56282, .F. ) ;
#12656 = ORIENTED_EDGE ( 'NONE', *, *, #41867, .F. ) ;
#12657 = EDGE_LOOP ( 'NONE', ( #46159, #30625 ) ) ;
#12658 = SURFACE_STYLE_FILL_AREA ( #58162 ) ;
#12659 = EDGE_CURVE ( 'NONE', #37934, #39121, #9574, .T. ) ;
#12660 = EDGE_CURVE ( 'NONE', #31608, #9704, #61457, .T. ) ;
#12661 = AXIS2_PLACEMENT_3D ( 'NONE', #35516, #40050, #63364 ) ;
#12662 = CARTESIAN_POINT ( 'NONE',  ( -92.69370383062502583, 88.66845928578038638, 88.79614583420050167 ) ) ;
#12663 = DIRECTION ( 'NONE',  ( -1.000000000000000000, 0.000000000000000000, 0.000000000000000000 ) ) ;
#12664 = CYLINDRICAL_SURFACE ( 'NONE', #17394, 21.00000000000000000 ) ;
#12665 = CARTESIAN_POINT ( 'NONE',  ( 96.15314808468750130, -211.9973110713294489, 88.58447916753381435 ) ) ;
#12666 = CARTESIAN_POINT ( 'NONE',  ( 97.64999999999997726, 91.52997821335252127, 78.94041666666666401 ) ) ;
#12667 = ORIENTED_EDGE ( 'NONE', *, *, #59580, .F. ) ;
#12668 = CARTESIAN_POINT ( 'NONE',  ( -94.99999999999997158, -206.9400435732949575, 88.01562500173429271 ) ) ;
#12669 = ORIENTED_EDGE ( 'NONE', *, *, #46591, .T. ) ;
#12670 = CARTESIAN_POINT ( 'NONE',  ( -3.000000000000000000, -22.67460108101774807, -6.353146135318215038 ) ) ;
#12671 = ORIENTED_EDGE ( 'NONE', *, *, #16152, .T. ) ;
#12672 = CARTESIAN_POINT ( 'NONE',  ( 92.35000000000000853, -209.9999999999999716, 90.00000000000000000 ) ) ;
#12673 = CARTESIAN_POINT ( 'NONE',  ( 92.69370383062498320, 90.00000000000002842, 89.16656250086715829 ) ) ;
#12674 = VECTOR ( 'NONE', #16302, 1000.000000000000000 ) ;
#12675 = ORIENTED_EDGE ( 'NONE', *, *, #51193, .T. ) ;
#12676 = CARTESIAN_POINT ( 'NONE',  ( 10.00000000000000178, 12.24744871391589385, -2.499999999999995559 ) ) ;
#12677 = CARTESIAN_POINT ( 'NONE',  ( -11.99999999999999645, 0.000000000000000000, 0.000000000000000000 ) ) ;
#12678 = CARTESIAN_POINT ( 'NONE',  ( 26.47460221209471598, -121.8961639463267090, 5.500000000000000000 ) ) ;
#12679 = DIRECTION ( 'NONE',  ( 0.000000000000000000, 0.7071067811865486830, -0.7071067811865463515 ) ) ;
#12680 = EDGE_LOOP ( 'NONE', ( #66462, #56336, #62526, #59386 ) ) ;
#12681 = CARTESIAN_POINT ( 'NONE',  ( 7.468086116107294004, -12.33868914344945189, 0.000000000000000000 ) ) ;
#12682 = CIRCLE ( 'NONE', #36725, 77.49900000000000944 ) ;
#12683 = CARTESIAN_POINT ( 'NONE',  ( -97.30629616937495996, -209.9999999999999716, 75.03781250086713328 ) ) ;
#12684 = ORIENTED_EDGE ( 'NONE', *, *, #15418, .T. ) ;
#12685 = ORIENTED_EDGE ( 'NONE', *, *, #42608, .F. ) ;
#12687 = CARTESIAN_POINT ( 'NONE',  ( 0.000000000000000000, 81.96053171279902472, 2.543863470248670211 ) ) ;
#12686 = AXIS2_PLACEMENT_3D ( 'NONE', #66805, #33310, #38979 ) ;
#12688 = DIRECTION ( 'NONE',  ( 0.000000000000000000, 0.000000000000000000, 1.000000000000000000 ) ) ;
#12689 = VECTOR ( 'NONE', #30175, 999.9999999999998863 ) ;
#12690 = AXIS2_PLACEMENT_3D ( 'NONE', #72235, #60964, #20740 ) ;
#12691 = CARTESIAN_POINT ( 'NONE',  ( 0.000000000000000000, 0.000000000000000000, -184.9999999999999432 ) ) ;
#12692 = VERTEX_POINT ( 'NONE', #62195 ) ;
#12693 = CARTESIAN_POINT ( 'NONE',  ( -94.99999999999997158, -212.6630814284392557, 88.05531250086716000 ) ) ;
#12694 = ORIENTED_EDGE ( 'NONE', *, *, #46121, .F. ) ;
#12695 = PLANE ( 'NONE',  #24916 ) ;
#12696 = EDGE_LOOP ( 'NONE', ( #62991, #44392, #8015, #53052, #44895, #62052, #70984, #10560, #38729, #54278, #21718, #50480, #29243, #18567, #72931, #60583, #65559, #30141, #35211, #37740, #51792, #60706, #48557, #3967, #31054, #273, #17278, #54451, #36862, #37916, #64065, #53168, #16075, #32912, #59133, #702, #69815, #5382, #12757, #67321, #26084, #37060, #44263, #39512, #25598, #67976, #38200, #70563, #1666, #53916 ) ) ;
#12697 = EDGE_LOOP ( 'NONE', ( #60715, #11733, #38784, #37649 ) ) ;
#12698 = LINE ( 'NONE', #13068, #28247 ) ;
#12699 = AXIS2_PLACEMENT_3D ( 'NONE', #33636, #58053, #46043 ) ;
#12700 = LINE ( 'NONE', #13070, #42163 ) ;
#12701 = CARTESIAN_POINT ( 'NONE',  ( 97.30629616937498838, 91.33154071421968467, 79.85322916753379729 ) ) ;
#12702 = DIRECTION ( 'NONE',  ( -1.000000000000000000, -0.000000000000000000, -0.000000000000000000 ) ) ;
#12703 = DIRECTION ( 'NONE',  ( 0.000000000000000000, 0.000000000000000000, 1.000000000000000000 ) ) ;
#12704 = DIRECTION ( 'NONE',  ( -1.000000000000000000, 0.000000000000000000, 0.000000000000000000 ) ) ;
#12705 = FACE_OUTER_BOUND ( 'NONE', #71743, .T. ) ;
#12706 = CARTESIAN_POINT ( 'NONE',  ( 10.00000000000000000, 0.000000000000000000, 0.000000000000000000 ) ) ;
#12707 = DIRECTION ( 'NONE',  ( -0.1850432970638667129, 0.9827303690289281857, 0.000000000000000000 ) ) ;
#12708 = DIRECTION ( 'NONE',  ( 0.4796670183876317051, -0.8774505977381972244, 0.000000000000000000 ) ) ;
#12709 = DIRECTION ( 'NONE',  ( 0.000000000000000000, 0.000000000000000000, 1.000000000000000000 ) ) ;
#12710 = PRODUCT_RELATED_PRODUCT_CATEGORY ( 'part', '', ( #50605 ) ) ;
#12711 = EDGE_CURVE ( 'NONE', #23922, #70598, #26192, .T. ) ;
#12712 = CARTESIAN_POINT ( 'NONE',  ( -48.80839716909612491, -10.37454508288793065, 5.500000000000000000 ) ) ;
#12713 = CARTESIAN_POINT ( 'NONE',  ( -93.84685191531254134, 91.99731107132950569, 85.62114583420046188 ) ) ;
#12714 = CARTESIAN_POINT ( 'NONE',  ( 0.000000000000000000, 81.50828551894227303, 8.966570791700979370 ) ) ;
#12715 = ADVANCED_FACE ( 'NONE', ( #63314 ), #34351, .T. ) ;
#12716 = EDGE_CURVE ( 'NONE', #1281, #3181, #30962, .T. ) ;
#12717 = CARTESIAN_POINT ( 'NONE',  ( 11.99999999999999822, 73.73191006444551476, 14.66109333815590254 ) ) ;
#12718 = ORIENTED_EDGE ( 'NONE', *, *, #35580, .F. ) ;
#12719 = EDGE_CURVE ( 'NONE', #58159, #11705, #28610, .T. ) ;
#12720 = CARTESIAN_POINT ( 'NONE',  ( 95.00000000000000000, -206.9400435732949575, 83.49125000000000796 ) ) ;
#12721 = FACE_BOUND ( 'NONE', #25764, .T. ) ;
#12722 = CIRCLE ( 'NONE', #65553, 37.49900000000000233 ) ;
#12723 = CARTESIAN_POINT ( 'NONE',  ( -9.937067298023309903, 7.583184918921312523, 42.00000000000001421 ) ) ;
#12724 = DIRECTION ( 'NONE',  ( -1.000000000000000000, 0.000000000000000000, 0.000000000000000000 ) ) ;
#12725 = CARTESIAN_POINT ( 'NONE',  ( 92.69370383062501162, -208.6684592857803011, 83.39864583420050792 ) ) ;
#12726 = AXIS2_PLACEMENT_3D ( 'NONE', #35395, #47056, #41046 ) ;
#12727 = ORIENTED_EDGE ( 'NONE', *, *, #29965, .F. ) ;
#12728 = AXIS2_PLACEMENT_3D ( 'NONE', #47942, #42674, #37033 ) ;
#12729 = VERTEX_POINT ( 'NONE', #33610 ) ;
#12730 = EDGE_CURVE ( 'NONE', #54468, #6463, #50173, .T. ) ;
#12731 = ADVANCED_FACE ( 'NONE', ( #5069 ), #27604, .F. ) ;
#12732 = FACE_OUTER_BOUND ( 'NONE', #74105, .T. ) ;
#12733 = VERTEX_POINT ( 'NONE', #39640 ) ;
#12734 = VECTOR ( 'NONE', #26750, 1000.000000000000000 ) ;
#12735 = CARTESIAN_POINT ( 'NONE',  ( 11.99999999999999822, 77.19088730480532945, -6.903761155836932062 ) ) ;
#12736 = CIRCLE ( 'NONE', #22364, 82.00000000000000000 ) ;
#12737 = CARTESIAN_POINT ( 'NONE',  ( 93.84685191531251292, -211.9973110713294489, 75.14364583420046984 ) ) ;
#12738 = VERTEX_POINT ( 'NONE', #46022 ) ;
#12739 = CARTESIAN_POINT ( 'NONE',  ( 92.69370383062501162, -209.9999999999999716, 80.27656250086714351 ) ) ;
#12740 = EDGE_LOOP ( 'NONE', ( #66310, #37633, #28129, #52807 ) ) ;
#12741 = CARTESIAN_POINT ( 'NONE',  ( 10.00000000000000000, -21.53537804866058991, -30.80686688397033635 ) ) ;
#12742 = ORIENTED_EDGE ( 'NONE', *, *, #68374, .T. ) ;
#12743 = ORIENTED_EDGE ( 'NONE', *, *, #4810, .T. ) ;
#12744 = DIRECTION ( 'NONE',  ( 0.000000000000000000, 1.000000000000000000, 3.491481338843133355E-15 ) ) ;
#12745 = EDGE_CURVE ( 'NONE', #56693, #44676, #50534, .T. ) ;
#12746 = CIRCLE ( 'NONE', #21120, 31.99999999999998934 ) ;
#12747 = SURFACE_SIDE_STYLE ('',( #24054 ) ) ;
#12748 = DIRECTION ( 'NONE',  ( -0.4279312458752977388, -0.9038112904824853189, 0.000000000000000000 ) ) ;
#12749 = ORIENTED_EDGE ( 'NONE', *, *, #971, .T. ) ;
#12750 = CARTESIAN_POINT ( 'NONE',  ( 92.34999999999999432, 90.00000000000002842, 90.00000000000000000 ) ) ;
#12751 = CARTESIAN_POINT ( 'NONE',  ( 92.35000000000002274, -211.5299782133524502, 83.14729166840096752 ) ) ;
#12752 = CARTESIAN_POINT ( 'NONE',  ( 97.30629616937498838, 90.00000000000002842, 74.87906250086714977 ) ) ;
#12753 = ORIENTED_EDGE ( 'NONE', *, *, #43722, .T. ) ;
#12754 = CARTESIAN_POINT ( 'NONE',  ( 96.32499999999997442, 92.29496732002878900, 84.78770833506763438 ) ) ;
#12755 = CARTESIAN_POINT ( 'NONE',  ( -34.02017708624681092, -109.8571428571428470, -2.500000000000000000 ) ) ;
#12756 = ORIENTED_EDGE ( 'NONE', *, *, #18478, .T. ) ;
#12757 = ORIENTED_EDGE ( 'NONE', *, *, #9226, .T. ) ;
#12758 = DIRECTION ( 'NONE',  ( 1.000000000000000000, -0.000000000000000000, 0.000000000000000000 ) ) ;
#12759 = VERTEX_POINT ( 'NONE', #22340 ) ;
#12760 = CARTESIAN_POINT ( 'NONE',  ( 94.99999999999998579, 86.94004357329500010, 84.52312500173428589 ) ) ;
#12761 = ORIENTED_EDGE ( 'NONE', *, *, #60130, .T. ) ;
#12762 = SURFACE_STYLE_USAGE ( .BOTH. , #64648 ) ;
#12763 = ORIENTED_EDGE ( 'NONE', *, *, #65170, .F. ) ;
#12764 = DIRECTION ( 'NONE',  ( -0.000000000000000000, -0.000000000000000000, 1.000000000000000000 ) ) ;
#12765 = LINE ( 'NONE', #1542, #25831 ) ;
#12766 = ORIENTED_EDGE ( 'NONE', *, *, #20017, .T. ) ;
#12767 = VERTEX_POINT ( 'NONE', #16327 ) ;
#12768 = ORIENTED_EDGE ( 'NONE', *, *, #69914, .T. ) ;
#12769 = DIRECTION ( 'NONE',  ( 0.8571673007021122226, 0.000000000000000000, 0.5150380749100542666 ) ) ;
#12770 = LINE ( 'NONE', #69192, #24143 ) ;
#12771 = CARTESIAN_POINT ( 'NONE',  ( -93.67500000000003979, 92.29496732002878900, 88.51833333333333087 ) ) ;
#12772 = EDGE_LOOP ( 'NONE', ( #17866, #28213, #15911, #40684 ) ) ;
#12773 = LINE ( 'NONE', #31176, #68368 ) ;
#12774 = CYLINDRICAL_SURFACE ( 'NONE', #15483, 31.99999999999999289 ) ;
#12775 = ORIENTED_EDGE ( 'NONE', *, *, #33979, .T. ) ;
#12776 =( BOUNDED_CURVE ( )  B_SPLINE_CURVE ( 2, ( #6838, #29751, #25973, #59460, #42535, #18848, #71826 ),
 .UNSPECIFIED., .F., .F. ) 
 B_SPLINE_CURVE_WITH_KNOTS ( ( 3, 2, 2, 3 ),
 ( 0.6875000000000000000, 0.6944444444444443088, 0.7013888888888887285, 0.7083333333333331483 ),
 .UNSPECIFIED. ) 
 CURVE ( )  GEOMETRIC_REPRESENTATION_ITEM ( )  RATIONAL_B_SPLINE_CURVE ( ( 1.000000000000000000, 0.8660254037844387076, 1.000000000000000000, 0.8660254037844387076, 1.000000000000000000, 0.8660254037844430375, 0.9999999999999956701 ) ) 
 REPRESENTATION_ITEM ( '' )  );
#12777 = PLANE ( 'NONE',  #57604 ) ;
#12778 = CARTESIAN_POINT ( 'NONE',  ( -94.99999999999997158, -212.6630814284392557, 84.08656250086713158 ) ) ;
#12779 = EDGE_LOOP ( 'NONE', ( #43223, #52931, #15236, #53707 ) ) ;
#12780 = DIRECTION ( 'NONE',  ( 0.000000000000000000, -0.8910065241883626808, -0.4539904997395568520 ) ) ;
#12781 = CYLINDRICAL_SURFACE ( 'NONE', #3217, 77.49899999999999523 ) ;
#12782 = CARTESIAN_POINT ( 'NONE',  ( 10.00000000000000000, -35.95386929396248377, -10.96151621346525751 ) ) ;
#12783 = CARTESIAN_POINT ( 'NONE',  ( 10.00000000000000000, -6.903761155838323837, 77.19088730480521576 ) ) ;
#12784 = ADVANCED_FACE ( 'NONE', ( #45286 ), #61831, .T. ) ;
#12785 = CARTESIAN_POINT ( 'NONE',  ( 0.000000000000000000, 15.48615015657637883, -39.04073710021327770 ) ) ;
#12786 = AXIS2_PLACEMENT_3D ( 'NONE', #22301, #38484, #16285 ) ;
#12787 = DIRECTION ( 'NONE',  ( -1.000000000000000000, 0.000000000000000000, 0.000000000000000000 ) ) ;
#12788 = DIRECTION ( 'NONE',  ( 0.000000000000000000, -0.9969173337331287410, 0.07845909572783489605 ) ) ;
#12789 = ADVANCED_FACE ( 'NONE', ( #55810 ), #10313, .T. ) ;
#12790 = CIRCLE ( 'NONE', #66836, 42.00000000000000000 ) ;
#12791 = CARTESIAN_POINT ( 'NONE',  ( 6.782329983125267248, 10.49999999999999645, -105.0000000000000000 ) ) ;
#12792 = ADVANCED_FACE ( 'NONE', ( #4325 ), #27214, .T. ) ;
#12793 = FACE_OUTER_BOUND ( 'NONE', #19445, .T. ) ;
#12794 = CARTESIAN_POINT ( 'NONE',  ( -92.69370383062502583, 88.66845928578038638, 77.84239583420045960 ) ) ;
#12795 = DIRECTION ( 'NONE',  ( -1.000000000000000000, 0.000000000000000000, 0.000000000000000000 ) ) ;
#12796 = PLANE ( 'NONE',  #59058 ) ;
#12797 = VECTOR ( 'NONE', #27029, 1000.000000000000227 ) ;
#12798 = DIRECTION ( 'NONE',  ( -1.000000000000000000, -0.000000000000000000, 0.000000000000000000 ) ) ;
#12799 = ADVANCED_FACE ( 'NONE', ( #68588 ), #45662, .F. ) ;
#12800 = DIRECTION ( 'NONE',  ( -1.000000000000000000, 0.000000000000000000, -0.000000000000000000 ) ) ;
#12801 = DIRECTION ( 'NONE',  ( -1.000000000000000000, 0.000000000000000000, 0.000000000000000000 ) ) ;
#12802 = DIRECTION ( 'NONE',  ( -1.000000000000000000, 0.000000000000000000, -0.000000000000000000 ) ) ;
#12803 = DIRECTION ( 'NONE',  ( 0.000000000000000000, 0.000000000000000000, 1.000000000000000000 ) ) ;
#12804 = AXIS2_PLACEMENT_3D ( 'NONE', #42432, #14210, #26232 ) ;
#12805 = DIRECTION ( 'NONE',  ( 1.000000000000000000, -0.000000000000000000, -0.000000000000000000 ) ) ;
#12806 = CARTESIAN_POINT ( 'NONE',  ( -92.69370383062498320, -209.9999999999999716, 74.87906250086714977 ) ) ;
#12807 = DIRECTION ( 'NONE',  ( 0.000000000000000000, 0.000000000000000000, -1.000000000000000000 ) ) ;
#12808 = EDGE_LOOP ( 'NONE', ( #49825, #16202, #64207, #68879 ) ) ;
#12809 = ADVANCED_FACE ( 'NONE', ( #74207 ), #22723, .T. ) ;
#12810 = DIRECTION ( 'NONE',  ( -1.000000000000000000, 0.000000000000000000, -0.000000000000000000 ) ) ;
#12811 = CARTESIAN_POINT ( 'NONE',  ( -3.000000000000000000, -22.67460108101783334, 6.353146135317912169 ) ) ;
#12812 = CARTESIAN_POINT ( 'NONE',  ( -9.332068499558246799, 6.890028847512375876, 42.00000000000001421 ) ) ;
#12813 = DIRECTION ( 'NONE',  ( 1.000000000000000000, -0.000000000000000000, -0.000000000000000000 ) ) ;
#12814 = VECTOR ( 'NONE', #59888, 1000.000000000000000 ) ;
#12815 = DIRECTION ( 'NONE',  ( 0.000000000000000000, 0.7071067811865437980, 0.7071067811865512365 ) ) ;
#12816 = ORIENTED_EDGE ( 'NONE', *, *, #55538, .F. ) ;
#12817 = ADVANCED_FACE ( 'NONE', ( #57293 ), #28713, .T. ) ;
#12818 = DIRECTION ( 'NONE',  ( 0.5200609990132993854, 0.8541291221503274356, 0.000000000000000000 ) ) ;
#12819 = EDGE_CURVE ( 'NONE', #5506, #71442, #12989, .T. ) ;
#12820 = CARTESIAN_POINT ( 'NONE',  ( 10.00000000000000000, -18.89407956138310496, 75.16055320797023853 ) ) ;
#12821 = ORIENTED_EDGE ( 'NONE', *, *, #67215, .F. ) ;
#12822 = CARTESIAN_POINT ( 'NONE',  ( 97.30629616937498838, -209.9999999999999716, 85.51531250086713953 ) ) ;
#12823 = CARTESIAN_POINT ( 'NONE',  ( 95.00000000000000000, -212.6630814284392557, 87.42031250086715488 ) ) ;
#12824 = EDGE_CURVE ( 'NONE', #70724, #28823, #35849, .T. ) ;
#12825 = CIRCLE ( 'NONE', #28450, 16.00000000000000355 ) ;
#12826 = ORIENTED_EDGE ( 'NONE', *, *, #29001, .F. ) ;
#12827 = CARTESIAN_POINT ( 'NONE',  ( 92.69370383062501162, -208.6684592857803011, 89.11364583420049712 ) ) ;
#12828 = AXIS2_PLACEMENT_3D ( 'NONE', #67690, #62440, #3812 ) ;
#12829 = ORIENTED_EDGE ( 'NONE', *, *, #53221, .F. ) ;
#12830 = LINE ( 'NONE', #63630, #55089 ) ;
#12831 = ORIENTED_EDGE ( 'NONE', *, *, #39826, .F. ) ;
#12832 = CARTESIAN_POINT ( 'NONE',  ( -97.30629616937501680, 88.66845928578038638, 82.23447916753383424 ) ) ;
#12833 = ORIENTED_EDGE ( 'NONE', *, *, #15169, .F. ) ;
#12834 = VERTEX_POINT ( 'NONE', #65163 ) ;
#12835 = FACE_OUTER_BOUND ( 'NONE', #52882, .T. ) ;
#12836 = ORIENTED_EDGE ( 'NONE', *, *, #6079, .F. ) ;
#12837 = DIRECTION ( 'NONE',  ( -1.000000000000000000, 0.000000000000000000, 0.000000000000000000 ) ) ;
#12838 = DIRECTION ( 'NONE',  ( -1.000000000000000000, -0.000000000000000000, -0.000000000000000000 ) ) ;
#12839 = EDGE_LOOP ( 'NONE', ( #57346, #36186, #61389, #8153 ) ) ;
#12840 = CARTESIAN_POINT ( 'NONE',  ( 10.00000000000000000, 12.93880638057314059, 76.41127070299278046 ) ) ;
#12841 = VECTOR ( 'NONE', #37141, 1000.000000000000000 ) ;
#12842 = CIRCLE ( 'NONE', #68083, 32.00000000000000000 ) ;
#12843 = ORIENTED_EDGE ( 'NONE', *, *, #27689, .T. ) ;
#12844 = CARTESIAN_POINT ( 'NONE',  ( 92.71977365048356035, 88.83725486022242990, 74.94226573542110259 ) ) ;
#12845 = ORIENTED_EDGE ( 'NONE', *, *, #6887, .T. ) ;
#12846 = ORIENTED_EDGE ( 'NONE', *, *, #20547, .T. ) ;
#12847 = ORIENTED_EDGE ( 'NONE', *, *, #33775, .F. ) ;
#12848 = CARTESIAN_POINT ( 'NONE',  ( 92.69370383062501162, -211.3315407142195852, 82.07572916753380809 ) ) ;
#12849 = DIRECTION ( 'NONE',  ( 0.000000000000000000, 0.07845909572783793529, 0.9969173337331285190 ) ) ;
#12850 = PRODUCT_CONTEXT ( 'NONE', #52686, 'mechanical' ) ;
#12851 = DIRECTION ( 'NONE',  ( 0.000000000000000000, 0.9510565162951544194, -0.3090169943749446757 ) ) ;
#12852 = CARTESIAN_POINT ( 'NONE',  ( 10.00000000000000000, 0.000000000000000000, 0.000000000000000000 ) ) ;
#12853 = CYLINDRICAL_SURFACE ( 'NONE', #46146, 31.99999999999998579 ) ;
#12854 = CARTESIAN_POINT ( 'NONE',  ( 10.00000000000000000, 16.23288003029497162, 33.80338159004289622 ) ) ;
#12855 = CARTESIAN_POINT ( 'NONE',  ( -96.32499999999996021, -207.7050326799711968, 88.70354166840097321 ) ) ;
#12856 = CARTESIAN_POINT ( 'NONE',  ( 93.67500000000001137, -207.7050326799711968, 76.55916666666666970 ) ) ;
#12857 = CARTESIAN_POINT ( 'NONE',  ( -94.99999999999997158, -212.6630814284392557, 83.45156250086714067 ) ) ;
#12858 = CIRCLE ( 'NONE', #53660, 15.77977592589476608 ) ;
#12859 = CARTESIAN_POINT ( 'NONE',  ( -93.84685191531252713, 88.00268892867056536, 82.39322916753381776 ) ) ;
#12860 = ORIENTED_EDGE ( 'NONE', *, *, #65401, .T. ) ;
#12861 = CARTESIAN_POINT ( 'NONE',  ( 94.99999999999998579, 87.33691857156068750, 80.27656250086714351 ) ) ;
#12862 = VERTEX_POINT ( 'NONE', #52380 ) ;
#12863 = CARTESIAN_POINT ( 'NONE',  ( 12.00000000000000000, -0.9646360437375368635, -23.52805723605589705 ) ) ;
#12864 = CARTESIAN_POINT ( 'NONE',  ( 0.000000000000000000, -12.42422080174614862, -35.38097989696524337 ) ) ;
#12865 = LINE ( 'NONE', #45995, #55389 ) ;
#12866 = CARTESIAN_POINT ( 'NONE',  ( 0.000000000000000000, 35.38097989696512968, 12.42422080174651100 ) ) ;
#12867 = LINE ( 'NONE', #60245, #53631 ) ;
#12868 = CARTESIAN_POINT ( 'NONE',  ( -92.69370383062498320, -208.6684592857803295, 84.93322916753379559 ) ) ;
#12869 = DIRECTION ( 'NONE',  ( -1.000000000000000000, 0.000000000000000000, 0.000000000000000000 ) ) ;
#12870 = EDGE_CURVE ( 'NONE', #366, #25593, #35102, .T. ) ;
#12871 = CARTESIAN_POINT ( 'NONE',  ( 8.000000000000007105, 1.142349898368116708E-14, 6.370018489481387452E-15 ) ) ;
#12872 = CYLINDRICAL_SURFACE ( 'NONE', #69117, 31.99999999999998579 ) ;
#12873 = DIRECTION ( 'NONE',  ( 0.000000000000000000, 0.000000000000000000, 1.000000000000000000 ) ) ;
#12874 = EDGE_LOOP ( 'NONE', ( #40916, #8253, #12993, #17468 ) ) ;
#12875 = VERTEX_POINT ( 'NONE', #70393 ) ;
#12876 = ADVANCED_FACE ( 'NONE', ( #24558 ), #35466, .T. ) ;
#12877 = DIRECTION ( 'NONE',  ( -0.000000000000000000, 0.1045284632676437703, -0.9945218953682742891 ) ) ;
#12878 = EDGE_CURVE ( 'NONE', #71894, #58524, #23844, .T. ) ;
#12879 = LINE ( 'NONE', #63301, #24721 ) ;
#12880 = FACE_OUTER_BOUND ( 'NONE', #49994, .T. ) ;
#12881 = CARTESIAN_POINT ( 'NONE',  ( 10.00000000000000000, 0.000000000000000000, 0.000000000000000000 ) ) ;
#12882 = DIRECTION ( 'NONE',  ( -1.000000000000000000, 0.000000000000000000, 0.000000000000000000 ) ) ;
#12883 = PLANE ( 'NONE',  #66193 ) ;
#12884 = DIRECTION ( 'NONE',  ( -1.000000000000000000, -0.000000000000000000, -0.000000000000000000 ) ) ;
#12885 = VECTOR ( 'NONE', #6882, 1000.000000000000000 ) ;
#12886 = ORIENTED_EDGE ( 'NONE', *, *, #959, .F. ) ;
#12887 = CARTESIAN_POINT ( 'NONE',  ( -95.00000000000002842, 87.33691857156074434, 76.46656250086712703 ) ) ;
#12888 = AXIS2_PLACEMENT_3D ( 'NONE', #22580, #32721, #15070 ) ;
#12889 = EDGE_CURVE ( 'NONE', #21827, #26934, #12892, .T. ) ;
#12890 = EDGE_CURVE ( 'NONE', #39717, #58054, #24198, .T. ) ;
#12891 = DIRECTION ( 'NONE',  ( -1.000000000000000000, -0.000000000000000000, -0.000000000000000000 ) ) ;
#12892 = LINE ( 'NONE', #40747, #56266 ) ;
#12893 = VECTOR ( 'NONE', #26005, 1000.000000000000114 ) ;
#12894 = CARTESIAN_POINT ( 'NONE',  ( 10.00000000000000000, 28.89263327155746097, 71.91182617369197771 ) ) ;
#12895 = CARTESIAN_POINT ( 'NONE',  ( 10.00000000000000000, -33.79645857604525361, 16.45098606841114730 ) ) ;
#12896 = CARTESIAN_POINT ( 'NONE',  ( -92.69370383062498320, -208.6684592857803011, 86.99697916753382287 ) ) ;
#12897 = AXIS2_PLACEMENT_3D ( 'NONE', #8471, #20492, #49049 ) ;
#12898 = FILL_AREA_STYLE_COLOUR ( '', #14550 ) ;
#12899 = CARTESIAN_POINT ( 'NONE',  ( 0.000000000000000000, 0.000000000000000000, 0.000000000000000000 ) ) ;
#12900 = EDGE_CURVE ( 'NONE', #60196, #10397, #37047, .T. ) ;
#12901 = CARTESIAN_POINT ( 'NONE',  ( 96.66135172262724495, 88.39919842643632819, 74.79754476654878204 ) ) ;
#12902 = CARTESIAN_POINT ( 'NONE',  ( -93.84685191531248449, -208.0026889286704943, 74.98489583420048632 ) ) ;
#12903 = FACE_OUTER_BOUND ( 'NONE', #64721, .T. ) ;
#12904 = ORIENTED_EDGE ( 'NONE', *, *, #60093, .T. ) ;
#12905 = LINE ( 'NONE', #29086, #37705 ) ;
#12906 = CARTESIAN_POINT ( 'NONE',  ( 0.000000000000000000, 0.000000000000000000, 0.000000000000000000 ) ) ;
#12907 = CIRCLE ( 'NONE', #71713, 77.49900000000000944 ) ;
#12908 = DIRECTION ( 'NONE',  ( -1.000000000000000000, 0.000000000000000000, 0.000000000000000000 ) ) ;
#12909 = CARTESIAN_POINT ( 'NONE',  ( 97.30629616937498838, -211.3315407142195852, 75.93739583420047268 ) ) ;
#12910 = VERTEX_POINT ( 'NONE', #47130 ) ;
#12911 = AXIS2_PLACEMENT_3D ( 'NONE', #4646, #22665, #9890 ) ;
#12912 = EDGE_CURVE ( 'NONE', #7708, #7152, #42233, .T. ) ;
#12913 = EDGE_CURVE ( 'NONE', #38975, #48180, #44285, .T. ) ;
#12914 = CARTESIAN_POINT ( 'NONE',  ( 10.00000000000000000, 0.000000000000000000, 0.000000000000000000 ) ) ;
#12915 = ORIENTED_EDGE ( 'NONE', *, *, #52327, .F. ) ;
#12916 = CYLINDRICAL_SURFACE ( 'NONE', #387, 31.99999999999998579 ) ;
#12917 = EDGE_LOOP ( 'NONE', ( #7646, #54638, #3950, #43540, #11545, #9327, #31467, #25828, #63835, #54569, #40420, #68137, #61697, #67777, #45173, #68648, #37097, #37637, #15158, #60929, #41463, #74217, #55669, #8578, #26634, #7498, #20391, #57813, #48679, #18002, #5015, #33561, #63548, #3446, #15695, #12831, #1544, #64833, #52411, #40644, #18338, #10254, #30697, #3432, #29188, #2272, #10352, #38680, #54665, #4100, #62063, #19690, #40363, #29387, #5738, #73408, #30944, #899, #34036, #17100, #73242, #950, #52598, #18557, #56804, #62079, #34848, #41221, #14583, #48925, #27195, #4848, #29591, #23886, #37176, #48355, #24256, #4116, #67250, #14866, #61012, #53698, #4909, #31602, #46485, #14978, #33686, #54747, #60740, #26679, #18928, #39890, #37285, #34876, #20256, #35588, #11272, #7970, #27910, #55043, #23606, #34372, #15179, #47721, #51525, #4175, #69622, #65683, #28569, #72831, #12562, #26514, #73228, #4566, #66653, #23424, #8779, #14598, #14456, #35240, #6738, #48998, #37164, #14041, #27300, #12932, #68116, #6454, #72784, #1468, #27809, #48802, #48752, #28572, #239, #36600, #20687, #49274, #44327, #23522, #42440, #73297, #25817, #52045, #51877, #64224, #23439, #5100, #57923, #63268, #35417, #29016, #63850, #18694, #58332, #20157, #27615, #28007, #7919, #70283, #1699, #21248, #2652, #50661, #57279, #14505, #33157, #35531, #47010, #68429, #49991, #24848, #31647, #5286, #71098, #65826, #40671, #50177, #20326, #13309, #47926, #33270, #68624, #69254, #46906, #5122, #30317, #28089, #48645, #11905, #12288, #37648, #59886, #23997, #1911, #70708, #42927, #3321, #64404, #23101, #69451, #11652, #30233, #13823, #11726, #39789, #21060, #16637, #56628, #33849, #12115, #9680, #26056, #34964, #31986, #4225, #33307, #49271, #38754, #69903, #43224, #44768, #66521, #20973, #26035, #36003, #67318, #39204, #8499, #10265, #29485, #46753, #18387, #57709, #46099, #48610, #29471, #67079, #65886, #30778, #37499, #53080, #9341, #427, #38844, #13582, #33326, #62275, #59091, #12000, #2530, #24411, #40144, #59746, #19980, #59732, #29875, #32786, #68224, #33437, #46693, #15975, #10850, #29922, #29833, #55215, #72934, #5021, #22391, #52823, #58142, #13208, #34861, #10440, #61231, #53904, #16572, #4295, #13380, #62934, #29148, #36330, #36050, #74074, #50271, #45723, #52355, #51898, #68695, #19680, #3153, #13048, #69532, #8542, #43225, #39407, #29172, #41999, #36806, #26827, #35119, #8789, #34468, #32706, #67699, #27473, #15175, #61143, #10525, #46792, #18580, #17936, #58655, #4161, #55105, #53484, #65094, #23687, #69200, #489, #32649, #21664, #5788, #41244, #15130 ) ) ;
#12918 = CARTESIAN_POINT ( 'NONE',  ( 0.000000000000000000, -19.89357724624987256, -12.59942793731086041 ) ) ;
#12919 = ORIENTED_EDGE ( 'NONE', *, *, #11893, .T. ) ;
#12920 = ORIENTED_EDGE ( 'NONE', *, *, #64847, .F. ) ;
#12921 = ORIENTED_EDGE ( 'NONE', *, *, #38636, .F. ) ;
#12922 = CARTESIAN_POINT ( 'NONE',  ( -92.34999999999999432, -209.9999999999999716, 77.61749999999999261 ) ) ;
#12923 = ORIENTED_EDGE ( 'NONE', *, *, #71899, .F. ) ;
#12924 = EDGE_LOOP ( 'NONE', ( #52614, #31377, #9885, #27634 ) ) ;
#12925 = CARTESIAN_POINT ( 'NONE',  ( 97.30629616937498838, 88.66845928578037217, 79.27114583420048177 ) ) ;
#12926 = CARTESIAN_POINT ( 'NONE',  ( 2.500000000000034639, 89.99999999999998579, -279.9999999999999432 ) ) ;
#12927 = CIRCLE ( 'NONE', #21348, 42.00000000000000000 ) ;
#12928 = CARTESIAN_POINT ( 'NONE',  ( 97.65000000000000568, -211.0689551420226451, 75.04052853044679239 ) ) ;
#12929 = AXIS2_PLACEMENT_3D ( 'NONE', #11151, #12250, #13721 ) ;
#12930 = ORIENTED_EDGE ( 'NONE', *, *, #33183, .F. ) ;
#12931 = ORIENTED_EDGE ( 'NONE', *, *, #61024, .T. ) ;
#12932 = ORIENTED_EDGE ( 'NONE', *, *, #57472, .F. ) ;
#12933 = DIRECTION ( 'NONE',  ( -1.000000000000000000, -0.000000000000000000, 0.000000000000000000 ) ) ;
#12934 = ORIENTED_EDGE ( 'NONE', *, *, #12964, .T. ) ;
#12935 = DIRECTION ( 'NONE',  ( 0.000000000000000000, 0.000000000000000000, 1.000000000000000000 ) ) ;
#12936 = CARTESIAN_POINT ( 'NONE',  ( -97.65000000000001990, 90.00000000000004263, 87.45999999999999375 ) ) ;
#12937 = CIRCLE ( 'NONE', #58567, 31.99999999999999289 ) ;
#12938 = CARTESIAN_POINT ( 'NONE',  ( 92.34999999999999432, 90.00000000000002842, 90.00000000000000000 ) ) ;
#12939 = CARTESIAN_POINT ( 'NONE',  ( 10.00000000000000000, -30.41916302227164337, 71.27951684758015460 ) ) ;
#12940 = AXIS2_PLACEMENT_3D ( 'NONE', #36568, #72612, #21119 ) ;
#12941 = FACE_OUTER_BOUND ( 'NONE', #15536, .T. ) ;
#12942 = DIRECTION ( 'NONE',  ( -1.000000000000000000, -0.000000000000000000, 0.000000000000000000 ) ) ;
#12943 = CYLINDRICAL_SURFACE ( 'NONE', #4439, 82.00000000000000000 ) ;
#12944 = CARTESIAN_POINT ( 'NONE',  ( -92.34999999999999432, -209.9999999999999716, 80.23687500173429044 ) ) ;
#12945 = CARTESIAN_POINT ( 'NONE',  ( 11.99999999999999822, 8.966570791700714693, 81.50828551894230145 ) ) ;
#12946 = VERTEX_POINT ( 'NONE', #57675 ) ;
#12947 = EDGE_CURVE ( 'NONE', #60509, #56683, #4647, .T. ) ;
#12949 = CARTESIAN_POINT ( 'NONE',  ( -97.65000000000001990, 88.47002178664754979, 76.16229166840095388 ) ) ;
#12948 = CARTESIAN_POINT ( 'NONE',  ( 94.99999999999998579, 86.94004357329500010, 76.26812500173430465 ) ) ;
#12950 = ORIENTED_EDGE ( 'NONE', *, *, #66392, .F. ) ;
#12951 = CARTESIAN_POINT ( 'NONE',  ( 94.99999999999998579, 87.33691857156068750, 81.70531250086715147 ) ) ;
#12952 = CARTESIAN_POINT ( 'NONE',  ( 92.34999999999990905, 88.47002178664757821, 75.44791666666667140 ) ) ;
#12953 = DIRECTION ( 'NONE',  ( -0.000000000000000000, -0.000000000000000000, -1.000000000000000000 ) ) ;
#12954 = EDGE_CURVE ( 'NONE', #68357, #73369, #11863, .T. ) ;
#12955 = CARTESIAN_POINT ( 'NONE',  ( 92.35000000000000853, -209.9999999999999716, 79.28437500173430408 ) ) ;
#12956 = CARTESIAN_POINT ( 'NONE',  ( -1.200000000000000030E-05, 16.95692799528845640, -2.500000000000000000 ) ) ;
#12957 = ORIENTED_EDGE ( 'NONE', *, *, #40479, .T. ) ;
#12958 = CARTESIAN_POINT ( 'NONE',  ( 0.000000000000000000, -3.948201729842348850, 23.21447184625293048 ) ) ;
#12959 = CYLINDRICAL_SURFACE ( 'NONE', #56398, 42.00000000000000000 ) ;
#12960 = ORIENTED_EDGE ( 'NONE', *, *, #52301, .F. ) ;
#12961 = EDGE_CURVE ( 'NONE', #25068, #49041, #30553, .T. ) ;
#12962 = AXIS2_PLACEMENT_3D ( 'NONE', #52500, #36326, #34855 ) ;
#12963 = VERTEX_POINT ( 'NONE', #18176 ) ;
#12964 = EDGE_CURVE ( 'NONE', #35320, #12946, #52660, .T. ) ;
#12965 = VECTOR ( 'NONE', #8775, 1000.000000000000000 ) ;
#12966 = CIRCLE ( 'NONE', #14141, 35.50000000000000711 ) ;
#12967 = CARTESIAN_POINT ( 'NONE',  ( 0.000000000000000000, 0.000000000000000000, 0.000000000000000000 ) ) ;
#12968 = DIRECTION ( 'NONE',  ( -1.000000000000000000, 0.000000000000000000, 0.000000000000000000 ) ) ;
#12969 = CARTESIAN_POINT ( 'NONE',  ( 10.00000000000000000, -60.67117009219097667, -55.16347631943105512 ) ) ;
#12970 = CARTESIAN_POINT ( 'NONE',  ( -94.99999999999997158, -207.3369185715606307, 78.84781250086714977 ) ) ;
#12971 = AXIS2_PLACEMENT_3D ( 'NONE', #27889, #11698, #21880 ) ;
#12972 = ORIENTED_EDGE ( 'NONE', *, *, #23448, .F. ) ;
#12973 = ADVANCED_FACE ( 'NONE', ( #18539 ), #41476, .T. ) ;
#12974 = DIRECTION ( 'NONE',  ( -1.000000000000000000, 0.000000000000000000, 0.000000000000000000 ) ) ;
#12975 = DIRECTION ( 'NONE',  ( 0.000000000000000000, 0.000000000000000000, 1.000000000000000000 ) ) ;
#12976 = DIRECTION ( 'NONE',  ( -0.000000000000000000, -0.000000000000000000, -1.000000000000000000 ) ) ;
#12977 = CARTESIAN_POINT ( 'NONE',  ( -12.75000000000000000, -120.0000000000000000, 127.5000000000000000 ) ) ;
#12978 = CARTESIAN_POINT ( 'NONE',  ( 10.00000000000000000, 37.58145647212453611, 0.6853352020791767529 ) ) ;
#12979 = DIRECTION ( 'NONE',  ( 0.000000000000000000, 0.000000000000000000, 1.000000000000000000 ) ) ;
#12980 = CARTESIAN_POINT ( 'NONE',  ( 19.12409105625795291, -101.5943176906707919, 5.500000000000000000 ) ) ;
#12981 = CARTESIAN_POINT ( 'NONE',  ( 92.35000000019410038, 89.99998015720535705, 86.27002759516707897 ) ) ;
#12982 = DIRECTION ( 'NONE',  ( -0.8896955516311735312, 0.000000000000000000, 0.4565542962317865050 ) ) ;
#12983 = DIRECTION ( 'NONE',  ( 0.000000000000000000, 0.000000000000000000, -1.000000000000000000 ) ) ;
#12984 = EDGE_CURVE ( 'NONE', #24796, #54007, #560, .T. ) ;
#12985 =( BOUNDED_CURVE ( )  B_SPLINE_CURVE ( 2, ( #45642, #34331, #69657, #22695, #39614, #11752, #28312 ),
 .UNSPECIFIED., .F., .F. ) 
 B_SPLINE_CURVE_WITH_KNOTS ( ( 3, 2, 2, 3 ),
 ( 0.1666666666666666852, 0.1736111111111111049, 0.1805555555555554970, 0.1874999999999999167 ),
 .UNSPECIFIED. ) 
 CURVE ( )  GEOMETRIC_REPRESENTATION_ITEM ( )  RATIONAL_B_SPLINE_CURVE ( ( 0.9999999999999994449, 0.8660254037844392627, 1.000000000000000000, 0.8660254037844387076, 1.000000000000000000, 0.8660254037844402619, 0.9999999999999984457 ) ) 
 REPRESENTATION_ITEM ( '' )  );
#12986 = AXIS2_PLACEMENT_3D ( 'NONE', #63091, #37831, #49094 ) ;
#12987 = EDGE_CURVE ( 'NONE', #29474, #72004, #73026, .T. ) ;
#12988 = CARTESIAN_POINT ( 'NONE',  ( 94.99999999999998579, 92.66308142843932671, 82.65781250086715204 ) ) ;
#12989 = CIRCLE ( 'NONE', #43071, 77.49900000000002365 ) ;
#12990 = CIRCLE ( 'NONE', #16650, 16.00000000000000000 ) ;
#12991 = CARTESIAN_POINT ( 'NONE',  ( -96.15314808468747287, -208.0026889286704943, 87.15572916753382060 ) ) ;
#12992 = CARTESIAN_POINT ( 'NONE',  ( 93.67499999999998295, 92.29496732002878900, 79.17854166840096752 ) ) ;
#12993 = ORIENTED_EDGE ( 'NONE', *, *, #9275, .T. ) ;
#12994 = DIRECTION ( 'NONE',  ( 0.000000000000000000, -0.7071067811865389130, -0.7071067811865561215 ) ) ;
#12995 = CARTESIAN_POINT ( 'NONE',  ( -93.67499999999998295, -212.2949673200287179, 81.95666666666666345 ) ) ;
#12996 = CARTESIAN_POINT ( 'NONE',  ( -97.30629616937501680, 90.00000000000004263, 75.03781250086713328 ) ) ;
#12997 = EDGE_CURVE ( 'NONE', #61868, #53859, #30188, .T. ) ;
#12998 = AXIS2_PLACEMENT_3D ( 'NONE', #3945, #62183, #50891 ) ;
#12999 = VECTOR ( 'NONE', #21687, 1000.000000000000000 ) ;
#13000 = CARTESIAN_POINT ( 'NONE',  ( 93.84685191531251292, -211.9973110713294489, 88.47864583420047779 ) ) ;
#13001 = EDGE_LOOP ( 'NONE', ( #22021, #60424, #18945, #26340 ) ) ;
#13002 = ADVANCED_FACE ( 'NONE', ( #23816 ), #17796, .T. ) ;
#13003 = ORIENTED_EDGE ( 'NONE', *, *, #55454, .T. ) ;
#13004 = ORIENTED_EDGE ( 'NONE', *, *, #23092, .T. ) ;
#13005 = EDGE_CURVE ( 'NONE', #12406, #51690, #20225, .T. ) ;
#13006 = CIRCLE ( 'NONE', #44262, 32.00000000000000000 ) ;
#13007 = DIRECTION ( 'NONE',  ( -1.000000000000000000, 0.000000000000000000, 0.000000000000000000 ) ) ;
#13008 = CYLINDRICAL_SURFACE ( 'NONE', #73850, 35.50000000000000711 ) ;
#13009 = AXIS2_PLACEMENT_3D ( 'NONE', #44769, #25976, #48904 ) ;
#13010 = CIRCLE ( 'NONE', #72999, 16.00000000000000355 ) ;
#13011 = ORIENTED_EDGE ( 'NONE', *, *, #10015, .F. ) ;
#13012 = VERTEX_POINT ( 'NONE', #48948 ) ;
#13013 = CARTESIAN_POINT ( 'NONE',  ( 21.07894319797337701, -103.8699611390234878, 5.500000000000000000 ) ) ;
#13014 = CARTESIAN_POINT ( 'NONE',  ( 92.69370383062501162, -208.6684592857803295, 81.49364583420049257 ) ) ;
#13015 = CARTESIAN_POINT ( 'NONE',  ( 93.67499999999998295, 92.29496732002878900, 89.89416666666666345 ) ) ;
#13016 = CARTESIAN_POINT ( 'NONE',  ( 94.99999999999998579, 93.05995642670504253, 80.95125000000000171 ) ) ;
#13017 = AXIS2_PLACEMENT_3D ( 'NONE', #5271, #28172, #62415 ) ;
#13018 = DIRECTION ( 'NONE',  ( -0.1850432970638667129, 0.9827303690289281857, 0.000000000000000000 ) ) ;
#13019 = CARTESIAN_POINT ( 'NONE',  ( 97.64999999999999147, 90.00000000000002842, 76.98250000000000171 ) ) ;
#13020 = LINE ( 'NONE', #58155, #5805 ) ;
#13021 = CARTESIAN_POINT ( 'NONE',  ( 93.67500000000001137, -212.2949673200287179, 83.75583333333332803 ) ) ;
#13022 = ORIENTED_EDGE ( 'NONE', *, *, #47979, .F. ) ;
#13023 = ORIENTED_EDGE ( 'NONE', *, *, #27984, .T. ) ;
#13024 = ORIENTED_EDGE ( 'NONE', *, *, #34814, .T. ) ;
#13025 = ORIENTED_EDGE ( 'NONE', *, *, #63003, .F. ) ;
#13026 = DIRECTION ( 'NONE',  ( 0.000000000000000000, -0.2079116908177653100, 0.9781476007338044676 ) ) ;
#13027 = CARTESIAN_POINT ( 'NONE',  ( -92.69370383062502583, 88.66845928578038638, 86.89114583420050053 ) ) ;
#13028 = DIRECTION ( 'NONE',  ( 0.000000000000000000, -0.9876883405951393247, 0.1564344650402205161 ) ) ;
#13029 = CARTESIAN_POINT ( 'NONE',  ( -94.99999999999997158, -209.9999999999999716, 90.00000000000000000 ) ) ;
#13030 = CARTESIAN_POINT ( 'NONE',  ( 93.84685191531251292, -211.9973110713294489, 88.47864583420047779 ) ) ;
#13031 = CARTESIAN_POINT ( 'NONE',  ( 97.64999999999999147, 90.00000000000002842, 79.52249999999999375 ) ) ;
#13032 = VERTEX_POINT ( 'NONE', #43710 ) ;
#13033 = CARTESIAN_POINT ( 'NONE',  ( -93.67499999999998295, -207.7050326799711968, 87.96270833506763154 ) ) ;
#13034 = ORIENTED_EDGE ( 'NONE', *, *, #19683, .T. ) ;
#13035 = CARTESIAN_POINT ( 'NONE',  ( 92.34999999999999432, -211.5299782133524502, 79.89291666666666458 ) ) ;
#13036 = ORIENTED_EDGE ( 'NONE', *, *, #8906, .T. ) ;
#13037 = CARTESIAN_POINT ( 'NONE',  ( -92.35000000000005116, 88.47002178664754979, 85.89895833506764689 ) ) ;
#13038 = CIRCLE ( 'NONE', #51472, 82.00000000000000000 ) ;
#13039 = CARTESIAN_POINT ( 'NONE',  ( 92.69370383062498320, 88.66845928578037217, 75.09072916753382287 ) ) ;
#13040 = ORIENTED_EDGE ( 'NONE', *, *, #16728, .T. ) ;
#13041 = DIRECTION ( 'NONE',  ( 0.4565542962317865050, 0.000000000000000000, 0.8896955516311735312 ) ) ;
#13042 = AXIS2_PLACEMENT_3D ( 'NONE', #69678, #58396, #929 ) ;
#13043 = VECTOR ( 'NONE', #18359, 1000.000000000000114 ) ;
#13044 = CARTESIAN_POINT ( 'NONE',  ( 11.99999999999999822, -3.894527615418461153, 81.90746397400387480 ) ) ;
#13045 = LINE ( 'NONE', #36352, #5374 ) ;
#13046 = EDGE_CURVE ( 'NONE', #24083, #7138, #70671, .T. ) ;
#13047 = DIRECTION ( 'NONE',  ( -1.000000000000000000, 0.000000000000000000, -0.000000000000000000 ) ) ;
#13048 = ORIENTED_EDGE ( 'NONE', *, *, #24682, .F. ) ;
#13049 = DIRECTION ( 'NONE',  ( 0.000000000000000000, 0.3090169943749442316, 0.9510565162951545304 ) ) ;
#13050 = LINE ( 'NONE', #35614, #46741 ) ;
#13051 = ORIENTED_EDGE ( 'NONE', *, *, #60023, .F. ) ;
#13052 = AXIS2_PLACEMENT_3D ( 'NONE', #57197, #23717, #35374 ) ;
#13053 = ADVANCED_FACE ( 'NONE', ( #25303, #8748 ), #8002, .F. ) ;
#13054 = EDGE_LOOP ( 'NONE', ( #54407, #11362, #62530, #44600 ) ) ;
#13055 = AXIS2_PLACEMENT_3D ( 'NONE', #17718, #70315, #40663 ) ;
#13056 = CARTESIAN_POINT ( 'NONE',  ( 11.99999999999999822, 0.000000000000000000, 0.000000000000000000 ) ) ;
#13057 = EDGE_CURVE ( 'NONE', #39711, #46797, #29834, .T. ) ;
#13058 = EDGE_CURVE ( 'NONE', #50178, #61657, #37329, .T. ) ;
#13059 = CARTESIAN_POINT ( 'NONE',  ( 5.000000000000000000, 2.419979747126332903, -5.688163366729713566 ) ) ;
#13060 = CARTESIAN_POINT ( 'NONE',  ( 0.000000000000000000, 73.44644590900061587, 24.73286445877730699 ) ) ;
#13061 = CARTESIAN_POINT ( 'NONE',  ( -97.30629616937495996, -209.9999999999999716, 87.26156250086715715 ) ) ;
#13062 = ORIENTED_EDGE ( 'NONE', *, *, #51000, .T. ) ;
#13063 = CARTESIAN_POINT ( 'NONE',  ( 10.00000000000000000, 77.32052557432841411, 5.256550761633138613 ) ) ;
#13064 = ORIENTED_EDGE ( 'NONE', *, *, #20208, .F. ) ;
#13065 = AXIS2_PLACEMENT_3D ( 'NONE', #40726, #2018, #34705 ) ;
#13066 = VECTOR ( 'NONE', #14760, 1000.000000000000000 ) ;
#13067 = ORIENTED_EDGE ( 'NONE', *, *, #17980, .T. ) ;
#13068 = CARTESIAN_POINT ( 'NONE',  ( 5.000000000000000000, -68.55367621811112144, -44.99326035066125939 ) ) ;
#13069 = CARTESIAN_POINT ( 'NONE',  ( 97.64999999999992042, 91.52997821335257811, 86.56041666666668277 ) ) ;
#13070 = CARTESIAN_POINT ( 'NONE',  ( 90.00000000000001421, -204.9999999999999147, 90.00000000000000000 ) ) ;
#13071 = CARTESIAN_POINT ( 'NONE',  ( 97.30629616937498838, 91.33154071421968467, 81.12322916753380753 ) ) ;
#13072 = FACE_OUTER_BOUND ( 'NONE', #55270, .T. ) ;
#13073 = DIRECTION ( 'NONE',  ( -1.000000000000000000, 0.000000000000000000, -0.000000000000000000 ) ) ;
#13074 = CARTESIAN_POINT ( 'NONE',  ( -92.34999999999995168, 91.52997821335249284, 80.84541666666663673 ) ) ;
#13075 = AXIS2_PLACEMENT_3D ( 'NONE', #33833, #49626, #21059 ) ;
#13076 = CARTESIAN_POINT ( 'NONE',  ( 0.000000000000000000, 72.35160999960844208, -20.41045688087747223 ) ) ;
#13077 = EDGE_CURVE ( 'NONE', #25431, #25593, #71856, .T. ) ;
#13078 = AXIS2_PLACEMENT_3D ( 'NONE', #34267, #45198, #68869 ) ;
#13079 = CARTESIAN_POINT ( 'NONE',  ( -97.64999999960629395, 90.00002930740643592, 76.74344264317980446 ) ) ;
#13080 = CARTESIAN_POINT ( 'NONE',  ( 19.29194287201271862, -133.5026271600380880, 5.500000000000000000 ) ) ;
#13081 = DIRECTION ( 'NONE',  ( 0.000000000000000000, -0.07845909572785224328, 0.9969173337331274087 ) ) ;
#13082 = DIRECTION ( 'NONE',  ( -1.000000000000000000, 0.000000000000000000, 0.000000000000000000 ) ) ;
#13083 = DIRECTION ( 'NONE',  ( 0.000000000000000000, 1.000000000000000000, 3.469446951953614978E-15 ) ) ;
#13084 = CARTESIAN_POINT ( 'NONE',  ( -96.15314808468751551, 88.00268892867056536, 86.57364583420047666 ) ) ;
#13085 = EDGE_CURVE ( 'NONE', #73031, #2581, #47880, .T. ) ;
#13086 = ADVANCED_FACE ( 'NONE', ( #66633 ), #25663, .T. ) ;
#13087 = CARTESIAN_POINT ( 'NONE',  ( -9.055038557894883766, -98.31460683512894150, 2.500000000000000000 ) ) ;
#13088 = VECTOR ( 'NONE', #37663, 1000.000000000000000 ) ;
#13089 = DIRECTION ( 'NONE',  ( -1.000000000000000000, 0.000000000000000000, -0.000000000000000000 ) ) ;
#13090 = VERTEX_POINT ( 'NONE', #48598 ) ;
#13092 = DIRECTION ( 'NONE',  ( -1.000000000000000000, -0.000000000000000000, -0.000000000000000000 ) ) ;
#13091 = AXIS2_PLACEMENT_3D ( 'NONE', #29778, #6867, #52732 ) ;
#13093 = CARTESIAN_POINT ( 'NONE',  ( 96.32499999999998863, -207.7050326799711968, 75.89770833506763381 ) ) ;
#13094 = DIRECTION ( 'NONE',  ( -1.000000000000000000, -0.000000000000000000, 0.000000000000000000 ) ) ;
#13095 = VECTOR ( 'NONE', #70813, 1000.000000000000114 ) ;
#13096 = VECTOR ( 'NONE', #13905, 1000.000000000000000 ) ;
#13097 = AXIS2_PLACEMENT_3D ( 'NONE', #58182, #64206, #35611 ) ;
#13098 = CARTESIAN_POINT ( 'NONE',  ( 11.99999999999999822, -73.95703589263990807, 23.16143007188399139 ) ) ;
#13099 = CARTESIAN_POINT ( 'NONE',  ( 97.30629616937498838, -208.6684592857803011, 82.55197916753382970 ) ) ;
#13100 = AXIS2_PLACEMENT_3D ( 'NONE', #49594, #20285, #14647 ) ;
#13101 = AXIS2_PLACEMENT_3D ( 'NONE', #56299, #55549, #4065 ) ;
#13102 = VERTEX_POINT ( 'NONE', #15113 ) ;
#13103 = ORIENTED_EDGE ( 'NONE', *, *, #16225, .T. ) ;
#13104 = CARTESIAN_POINT ( 'NONE',  ( -0.0004442498525516064278, 0.001194404164626844313, 127.4927882439603195 ) ) ;
#13105 = ORIENTED_EDGE ( 'NONE', *, *, #60393, .F. ) ;
#13106 = CYLINDRICAL_SURFACE ( 'NONE', #19723, 16.00000000000000000 ) ;
#13107 = CARTESIAN_POINT ( 'NONE',  ( 92.69370383062501162, -209.9999999999999716, 76.30781250086714351 ) ) ;
#13108 = ORIENTED_EDGE ( 'NONE', *, *, #30225, .T. ) ;
#13109 = CARTESIAN_POINT ( 'NONE',  ( 96.15314808468750130, -211.9973110713294489, 79.85322916753381151 ) ) ;
#13110 = AXIS2_PLACEMENT_3D ( 'NONE', #36086, #25179, #8250 ) ;
#13111 = EDGE_LOOP ( 'NONE', ( #11451, #31224, #37533, #44924 ) ) ;
#13112 = CARTESIAN_POINT ( 'NONE',  ( -26.29030328629083968, -123.6496510949466341, 5.500000000000000000 ) ) ;
#13113 = ORIENTED_EDGE ( 'NONE', *, *, #64585, .T. ) ;
#13114 = ORIENTED_EDGE ( 'NONE', *, *, #62936, .F. ) ;
#13115 = CARTESIAN_POINT ( 'NONE',  ( 10.00000000000000000, 32.34446384429971744, 26.79245525562727082 ) ) ;
#13116 = VECTOR ( 'NONE', #9781, 1000.000000000000000 ) ;
#13117 = CARTESIAN_POINT ( 'NONE',  ( 0.000000000000000000, 0.000000000000000000, 0.000000000000000000 ) ) ;
#13118 = CIRCLE ( 'NONE', #2334, 4.749999999999999112 ) ;
#13119 = ORIENTED_EDGE ( 'NONE', *, *, #10059, .T. ) ;
#13120 = CARTESIAN_POINT ( 'NONE',  ( -97.64999999999996305, -209.9999999999999716, 90.00000000000000000 ) ) ;
#13121 = CARTESIAN_POINT ( 'NONE',  ( 93.67500000000001137, -212.2949673200287179, 81.93020833506763267 ) ) ;
#13123 = VECTOR ( 'NONE', #17636, 1000.000000000000000 ) ;
#13122 = CARTESIAN_POINT ( 'NONE',  ( 97.64999999999997726, 88.47002178664753558, 88.99458333333333826 ) ) ;
#13124 = ORIENTED_EDGE ( 'NONE', *, *, #44652, .F. ) ;
#13125 = CARTESIAN_POINT ( 'NONE',  ( 10.00000000000000000, -8.840884882375609877, 74.65374052328647281 ) ) ;
#13126 = CARTESIAN_POINT ( 'NONE',  ( 97.64999999999999147, -209.9999999999999716, 90.00000000000000000 ) ) ;
#13127 = ORIENTED_EDGE ( 'NONE', *, *, #22226, .T. ) ;
#13128 = ORIENTED_EDGE ( 'NONE', *, *, #68405, .F. ) ;
#13129 = CARTESIAN_POINT ( 'NONE',  ( -93.84685191531254134, 91.99731107132950569, 87.04989583420048405 ) ) ;
#13130 = ORIENTED_EDGE ( 'NONE', *, *, #36913, .F. ) ;
#13131 = CARTESIAN_POINT ( 'NONE',  ( 97.64999999999999147, 90.00000000000002842, 85.31687500173428873 ) ) ;
#13132 = EDGE_CURVE ( 'NONE', #28736, #20120, #48231, .T. ) ;
#13133 =( NAMED_UNIT ( * ) SI_UNIT ( $, .STERADIAN. ) SOLID_ANGLE_UNIT ( ) );
#13134 = EDGE_LOOP ( 'NONE', ( #34069, #71804, #12088, #41925 ) ) ;
#13135 = FACE_BOUND ( 'NONE', #22881, .T. ) ;
#13136 = LINE ( 'NONE', #43863, #66671 ) ;
#13137 = VERTEX_POINT ( 'NONE', #20398 ) ;
#13138 = VERTEX_POINT ( 'NONE', #66271 ) ;
#13139 = ADVANCED_FACE ( 'NONE', ( #54968 ), #65528, .T. ) ;
#13140 = VERTEX_POINT ( 'NONE', #59892 ) ;
#13141 = DIRECTION ( 'NONE',  ( 1.000000000000000000, 0.000000000000000000, 0.000000000000000000 ) ) ;
#13142 = CARTESIAN_POINT ( 'NONE',  ( 93.67499999999998295, 92.29496732002878900, 81.63916666666666799 ) ) ;
#13143 = EDGE_CURVE ( 'NONE', #37625, #73517, #16648, .T. ) ;
#13144 = CARTESIAN_POINT ( 'NONE',  ( -92.35000000000005116, 91.52997821335253548, 85.29041666666665833 ) ) ;
#13145 = VERTEX_POINT ( 'NONE', #32029 ) ;
#13146 = CARTESIAN_POINT ( 'NONE',  ( -10.90473778262209414, 0.000000000000000000, 0.000000000000000000 ) ) ;
#13147 = DIRECTION ( 'NONE',  ( 0.000000000000000000, 0.5224985647159440250, 0.8526401643540951758 ) ) ;
#13148 = ORIENTED_EDGE ( 'NONE', *, *, #52870, .F. ) ;
#13149 = CARTESIAN_POINT ( 'NONE',  ( 0.000000000000000000, 77.49459641780886443, -0.8261519478433788644 ) ) ;
#13150 = CARTESIAN_POINT ( 'NONE',  ( -94.99999999999997158, -212.6630814284392557, 81.54656250086715374 ) ) ;
#13152 = EDGE_LOOP ( 'NONE', ( #54825, #10834, #34222, #55206 ) ) ;
#13151 = EDGE_CURVE ( 'NONE', #55839, #59860, #14752, .T. ) ;
#13153 = AXIS2_PLACEMENT_3D ( 'NONE', #24806, #70649, #37211 ) ;
#13154 = CARTESIAN_POINT ( 'NONE',  ( 10.00000000000000000, -77.49459641780886443, 0.8261519478428377417 ) ) ;
#13155 = DIRECTION ( 'NONE',  ( -1.000000000000000000, -0.000000000000000000, 0.000000000000000000 ) ) ;
#13156 = CYLINDRICAL_SURFACE ( 'NONE', #4497, 37.49900000000000233 ) ;
#13157 = FACE_OUTER_BOUND ( 'NONE', #62614, .T. ) ;
#13158 = CIRCLE ( 'NONE', #55176, 42.00000000000000000 ) ;
#13159 = CIRCLE ( 'NONE', #69572, 31.99999999999998579 ) ;
#13160 = EDGE_CURVE ( 'NONE', #53011, #70414, #57227, .T. ) ;
#13161 = CYLINDRICAL_SURFACE ( 'NONE', #33134, 77.49899999999999523 ) ;
#13162 = DIRECTION ( 'NONE',  ( -0.000000000000000000, -0.000000000000000000, -1.000000000000000000 ) ) ;
#13164 = AXIS2_PLACEMENT_3D ( 'NONE', #41868, #74321, #5920 ) ;
#13163 = CARTESIAN_POINT ( 'NONE',  ( 0.000000000000000000, 0.000000000000000000, 0.000000000000000000 ) ) ;
#13165 = DIRECTION ( 'NONE',  ( -0.000000000000000000, -0.000000000000000000, 1.000000000000000000 ) ) ;
#13166 = DIRECTION ( 'NONE',  ( -1.000000000000000000, 0.000000000000000000, 0.000000000000000000 ) ) ;
#13167 = EDGE_CURVE ( 'NONE', #66514, #39991, #10992, .T. ) ;
#13168 = FACE_OUTER_BOUND ( 'NONE', #7473, .T. ) ;
#13169 = ADVANCED_FACE ( 'NONE', ( #5372 ), #46685, .F. ) ;
#13170 = CARTESIAN_POINT ( 'NONE',  ( -93.84685191531254134, 91.99731107132950569, 75.46114583420047950 ) ) ;
#13171 = CARTESIAN_POINT ( 'NONE',  ( 16.30584220631899228, -140.9432449716519784, -2.500000000000000000 ) ) ;
#13172 = LINE ( 'NONE', #42135, #282 ) ;
#13173 = LINE ( 'NONE', #12433, #49768 ) ;
#13174 = CIRCLE ( 'NONE', #35981, 77.49899999999999523 ) ;
#13175 = DIRECTION ( 'NONE',  ( 0.000000000000000000, 0.3090169943749412895, 0.9510565162951556406 ) ) ;
#13177 = DIRECTION ( 'NONE',  ( 0.000000000000000000, 0.000000000000000000, 1.000000000000000000 ) ) ;
#13176 = CIRCLE ( 'NONE', #23983, 1.500000000000000000 ) ;
#13178 = EDGE_CURVE ( 'NONE', #32525, #37548, #56860, .T. ) ;
#13179 = EDGE_CURVE ( 'NONE', #986, #16639, #40646, .T. ) ;
#13180 = CIRCLE ( 'NONE', #2449, 26.50000000000552092 ) ;
#13181 = CARTESIAN_POINT ( 'NONE',  ( -11.70000000000000107, 0.000000000000000000, 17.45460580326810174 ) ) ;
#13182 = DIRECTION ( 'NONE',  ( -1.000000000000000000, 0.000000000000000000, 0.000000000000000000 ) ) ;
#13183 = CYLINDRICAL_SURFACE ( 'NONE', #70043, 77.49899999999999523 ) ;
#13184 = CARTESIAN_POINT ( 'NONE',  ( -92.69370383062498320, -211.3315407142195852, 77.36614583420048064 ) ) ;
#13185 = CIRCLE ( 'NONE', #32388, 82.00000000000000000 ) ;
#13186 = AXIS2_PLACEMENT_3D ( 'NONE', #59342, #30745, #1498 ) ;
#13187 = DIRECTION ( 'NONE',  ( 0.000000000000000000, 0.000000000000000000, 1.000000000000000000 ) ) ;
#13188 = ORIENTED_EDGE ( 'NONE', *, *, #50042, .F. ) ;
#13189 = CARTESIAN_POINT ( 'NONE',  ( 10.00000000000000000, 21.53537804866126137, -30.80686688396986028 ) ) ;
#13190 = CARTESIAN_POINT ( 'NONE',  ( -97.64999999978466860, 90.00002100773832581, 79.91868729552945183 ) ) ;
#13191 = SURFACE_STYLE_USAGE ( .BOTH. , #28999 ) ;
#13192 = CARTESIAN_POINT ( 'NONE',  ( 0.000000000000000000, -54.21277698773713638, 55.38113227695764351 ) ) ;
#13193 = DIRECTION ( 'NONE',  ( 0.000000000000000000, 0.000000000000000000, -1.000000000000000000 ) ) ;
#13194 = ORIENTED_EDGE ( 'NONE', *, *, #10776, .T. ) ;
#13195 = CARTESIAN_POINT ( 'NONE',  ( -2.977765906491215642, 0.000000000000000000, 0.000000000000000000 ) ) ;
#13196 = DIRECTION ( 'NONE',  ( 0.000000000000000000, 0.000000000000000000, 1.000000000000000000 ) ) ;
#13197 = VERTEX_POINT ( 'NONE', #6469 ) ;
#13198 =( BOUNDED_CURVE ( )  B_SPLINE_CURVE ( 2, ( #6230, #38943, #16376, #5119, #56984, #33664, #39319 ),
 .UNSPECIFIED., .F., .F. ) 
 B_SPLINE_CURVE_WITH_KNOTS ( ( 3, 2, 2, 3 ),
 ( 0.3598440426530882807, 0.3668998081258831867, 0.3739555736667655728, 0.3810111478265181262 ),
 .UNSPECIFIED. ) 
 CURVE ( )  GEOMETRIC_REPRESENTATION_ITEM ( )  RATIONAL_B_SPLINE_CURVE ( ( 1.000000000000000000, 0.8660254037844387076, 1.000000000000000000, 0.8660254037844387076, 1.000000000000000000, 0.8660290377217400026, 0.9999927323225317188 ) ) 
 REPRESENTATION_ITEM ( '' )  );
#13199 = VECTOR ( 'NONE', #74168, 1000.000000000000000 ) ;
#13200 = CARTESIAN_POINT ( 'NONE',  ( 95.00000000000000000, -207.3369185715606307, 86.30906250086714238 ) ) ;
#13201 = CARTESIAN_POINT ( 'NONE',  ( 97.30629616937498838, -211.3315407142195852, 89.43114583420049257 ) ) ;
#13202 = VERTEX_POINT ( 'NONE', #47063 ) ;
#13203 = CIRCLE ( 'NONE', #20413, 31.99999999999999289 ) ;
#13204 = ORIENTED_EDGE ( 'NONE', *, *, #32351, .F. ) ;
#13205 = DIRECTION ( 'NONE',  ( 1.000000000000000000, 0.000000000000000000, 0.000000000000000000 ) ) ;
#13206 = ORIENTED_EDGE ( 'NONE', *, *, #30615, .T. ) ;
#13207 = CARTESIAN_POINT ( 'NONE',  ( -97.30629616937501680, 90.00000000000004263, 81.54656250086715374 ) ) ;
#13208 = ORIENTED_EDGE ( 'NONE', *, *, #47865, .F. ) ;
#13209 = ORIENTED_EDGE ( 'NONE', *, *, #31672, .F. ) ;
#13210 = CIRCLE ( 'NONE', #2491, 42.00000000000000000 ) ;
#13211 = FACE_OUTER_BOUND ( 'NONE', #69917, .T. ) ;
#13212 = EDGE_CURVE ( 'NONE', #56853, #35138, #32241, .T. ) ;
#13213 = ORIENTED_EDGE ( 'NONE', *, *, #63262, .F. ) ;
#13214 = CARTESIAN_POINT ( 'NONE',  ( 0.000000000000000000, 67.80270845531956070, -46.11716303203111522 ) ) ;
#13215 = EDGE_CURVE ( 'NONE', #60769, #69147, #28267, .T. ) ;
#13216 = ORIENTED_EDGE ( 'NONE', *, *, #6471, .T. ) ;
#13217 = DIRECTION ( 'NONE',  ( 0.000000000000000000, 0.5877852522924744694, -0.8090169943749465631 ) ) ;
#13218 = EDGE_CURVE ( 'NONE', #20502, #14677, #59869, .T. ) ;
#13219 = ORIENTED_EDGE ( 'NONE', *, *, #73737, .F. ) ;
#13220 =( BOUNDED_CURVE ( )  B_SPLINE_CURVE ( 2, ( #1730, #24617, #57356, #23512, #621, #46445, #69372 ),
 .UNSPECIFIED., .F., .F. ) 
 B_SPLINE_CURVE_WITH_KNOTS ( ( 3, 2, 2, 3 ),
 ( 0.5000000000000000000, 0.5069444444444444198, 0.5138888888888887285, 0.5208333333333332593 ),
 .UNSPECIFIED. ) 
 CURVE ( )  GEOMETRIC_REPRESENTATION_ITEM ( )  RATIONAL_B_SPLINE_CURVE ( ( 1.000000000000000000, 0.8660254037844387076, 1.000000000000000000, 0.8660254037844387076, 1.000000000000000000, 0.8660254037844408170, 0.9999999999999978906 ) ) 
 REPRESENTATION_ITEM ( '' )  );
#13221 = CARTESIAN_POINT ( 'NONE',  ( 92.35000000000000853, -211.5299782133524218, 80.60729166840097548 ) ) ;
#13222 = ORIENTED_EDGE ( 'NONE', *, *, #51624, .T. ) ;
#13223 = ADVANCED_FACE ( 'NONE', ( #40299 ), #41052, .T. ) ;
#13224 = AXIS2_PLACEMENT_3D ( 'NONE', #37317, #36927, #36550 ) ;
#13225 = ORIENTED_EDGE ( 'NONE', *, *, #67849, .F. ) ;
#13226 = ORIENTED_EDGE ( 'NONE', *, *, #21116, .F. ) ;
#13227 = AXIS2_PLACEMENT_3D ( 'NONE', #41655, #13082, #12709 ) ;
#13228 = CARTESIAN_POINT ( 'NONE',  ( 97.30629616937498838, -209.9999999999999716, 79.16531250086714522 ) ) ;
#13229 = AXIS2_PLACEMENT_3D ( 'NONE', #57261, #45986, #8341 ) ;
#13230 = PLANE ( 'NONE',  #67674 ) ;
#13231 = VECTOR ( 'NONE', #42948, 1000.000000000000000 ) ;
#13232 = CARTESIAN_POINT ( 'NONE',  ( 11.99999999999999822, -35.91791733033428358, -68.67312586195033930 ) ) ;
#13233 = DIRECTION ( 'NONE',  ( -1.000000000000000000, 0.000000000000000000, 0.000000000000000000 ) ) ;
#13234 = CARTESIAN_POINT ( 'NONE',  ( 97.64999999999994884, 88.47002178664752137, 85.18458333333332178 ) ) ;
#13235 = EDGE_CURVE ( 'NONE', #50602, #54476, #25074, .T. ) ;
#13236 = CARTESIAN_POINT ( 'NONE',  ( 10.00000000000000000, 72.35432306680485226, -20.40083707022909110 ) ) ;
#13237 = FACE_OUTER_BOUND ( 'NONE', #35134, .T. ) ;
#13238 = DIRECTION ( 'NONE',  ( -1.000000000000000000, -0.000000000000000000, -0.000000000000000000 ) ) ;
#13239 = VECTOR ( 'NONE', #32049, 1000.000000000000000 ) ;
#13240 = CARTESIAN_POINT ( 'NONE',  ( -92.69370383062498320, -211.3315407142195852, 82.92239583420045790 ) ) ;
#13241 = CARTESIAN_POINT ( 'NONE',  ( -93.84685191531254134, 91.99731107132950569, 83.23989583420049598 ) ) ;
#13242 = ORIENTED_EDGE ( 'NONE', *, *, #39213, .T. ) ;
#13243 = CARTESIAN_POINT ( 'NONE',  ( 93.84685191531248449, 88.00268892867053694, 80.22364583420046813 ) ) ;
#13244 = ORIENTED_EDGE ( 'NONE', *, *, #49197, .T. ) ;
#13245 = DIRECTION ( 'NONE',  ( -1.000000000000000000, 0.000000000000000000, 0.000000000000000000 ) ) ;
#13246 = DIRECTION ( 'NONE',  ( -0.000000000000000000, -0.000000000000000000, 1.000000000000000000 ) ) ;
#13247 = EDGE_CURVE ( 'NONE', #4586, #11727, #65929, .T. ) ;
#13248 = CARTESIAN_POINT ( 'NONE',  ( 1.692257445284848207E-12, 0.000000000000000000, -65.00000000000000000 ) ) ;
#13249 = CARTESIAN_POINT ( 'NONE',  ( 11.99999999999999822, 44.88180994100466847, -63.18004540532978552 ) ) ;
#13250 = DIRECTION ( 'NONE',  ( 0.000000000000000000, -0.9238795325112822976, -0.3826834323651008285 ) ) ;
#13251 = CARTESIAN_POINT ( 'NONE',  ( -96.15314808468747287, -208.0026889286704943, 83.82197916753381151 ) ) ;
#13252 = CARTESIAN_POINT ( 'NONE',  ( 6.000000000000000000, 71.21200624218852226, -40.65526001592539984 ) ) ;
#13253 = DIRECTION ( 'NONE',  ( 1.000000000000000000, 0.000000000000000000, 0.000000000000000000 ) ) ;
#13254 = DIRECTION ( 'NONE',  ( -1.000000000000000000, 0.000000000000000000, 0.000000000000000000 ) ) ;
#13255 = DIRECTION ( 'NONE',  ( 0.000000000000000000, -0.7431448254773954654, 0.6691306063588569053 ) ) ;
#13256 = ORIENTED_EDGE ( 'NONE', *, *, #50505, .T. ) ;
#13257 = ORIENTED_EDGE ( 'NONE', *, *, #46851, .F. ) ;
#13258 = LINE ( 'NONE', #24541, #67489 ) ;
#13259 = EDGE_CURVE ( 'NONE', #52158, #16575, #26301, .T. ) ;
#13260 = CARTESIAN_POINT ( 'NONE',  ( -97.64999999999986358, -211.5299782133524502, 78.62291666666668277 ) ) ;
#13261 = EDGE_CURVE ( 'NONE', #30694, #70056, #53896, .T. ) ;
#13262 = CARTESIAN_POINT ( 'NONE',  ( -96.15314808468751551, 88.00268892867056536, 87.84364583420047268 ) ) ;
#13263 = CARTESIAN_POINT ( 'NONE',  ( 11.99999999999999822, -71.21200624218766961, -40.65526001592688488 ) ) ;
#13264 = CYLINDRICAL_SURFACE ( 'NONE', #32581, 31.99999999999998579 ) ;
#13265 = CARTESIAN_POINT ( 'NONE',  ( 10.00000000000000000, 75.16055320797030959, 18.89407956138283851 ) ) ;
#13266 = DIRECTION ( 'NONE',  ( 0.000000000000000000, 0.000000000000000000, 1.000000000000000000 ) ) ;
#13267 = ORIENTED_EDGE ( 'NONE', *, *, #69323, .F. ) ;
#13268 = CARTESIAN_POINT ( 'NONE',  ( -92.69370383062504004, 90.00000000000004263, 76.62531250086713897 ) ) ;
#13269 = AXIS2_PLACEMENT_3D ( 'NONE', #5618, #34915, #376 ) ;
#13270 = CIRCLE ( 'NONE', #33658, 5.000000000000000888 ) ;
#13271 = DIRECTION ( 'NONE',  ( -0.000000000000000000, -0.000000000000000000, -1.000000000000000000 ) ) ;
#13272 = DIRECTION ( 'NONE',  ( 0.000000000000000000, 0.9876883405951383255, -0.1564344650402277048 ) ) ;
#13273 = CARTESIAN_POINT ( 'NONE',  ( 97.64999999999999147, -210.0000000983658026, 80.23687499810812085 ) ) ;
#13274 = AXIS2_PLACEMENT_3D ( 'NONE', #40522, #46171, #58935 ) ;
#13275 = CARTESIAN_POINT ( 'NONE',  ( 92.35000000000000853, -209.9999999999999716, 82.37999999999999545 ) ) ;
#13276 = CARTESIAN_POINT ( 'NONE',  ( -92.69370383062498320, -209.9999999999999716, 86.94406250086716170 ) ) ;
#13277 = CYLINDRICAL_SURFACE ( 'NONE', #61667, 82.00000000000000000 ) ;
#13278 = CARTESIAN_POINT ( 'NONE',  ( 96.66078148566039374, 88.39974787049349914, 74.80065602173002048 ) ) ;
#13279 = CARTESIAN_POINT ( 'NONE',  ( -96.15314808468745866, -211.9973110713294489, 76.57239583420049200 ) ) ;
#13280 = CARTESIAN_POINT ( 'NONE',  ( 92.34999999999999432, 90.00000000000002842, 88.73000000000000398 ) ) ;
#13281 = VERTEX_POINT ( 'NONE', #46314 ) ;
#13282 = CARTESIAN_POINT ( 'NONE',  ( -92.35000000000005116, 91.52997821335253548, 82.82979166840095786 ) ) ;
#13283 = DIRECTION ( 'NONE',  ( -1.000000000000000000, 0.000000000000000000, 0.000000000000000000 ) ) ;
#13284 = DIRECTION ( 'NONE',  ( 2.603472992746261562E-14, 2.546204323184492723E-14, -1.000000000000000000 ) ) ;
#13285 = AXIS2_PLACEMENT_3D ( 'NONE', #42195, #25994, #69998 ) ;
#13286 = AXIS2_PLACEMENT_3D ( 'NONE', #31538, #20259, #25536 ) ;
#13287 = CIRCLE ( 'NONE', #12059, 82.00000000000000000 ) ;
#13288 = CARTESIAN_POINT ( 'NONE',  ( 0.000000000000000000, 37.16516213103285082, -4.992566952384588141 ) ) ;
#13289 = CARTESIAN_POINT ( 'NONE',  ( 97.30629616937498838, -209.9999999999999716, 75.99031250086714806 ) ) ;
#13290 = ORIENTED_EDGE ( 'NONE', *, *, #51398, .T. ) ;
#13291 = EDGE_CURVE ( 'NONE', #21733, #32740, #30114, .T. ) ;
#13292 = CYLINDRICAL_SURFACE ( 'NONE', #37161, 77.49899999999999523 ) ;
#13293 =( LENGTH_UNIT ( ) NAMED_UNIT ( * ) SI_UNIT ( .MILLI., .METRE. ) );
#13294 = ORIENTED_EDGE ( 'NONE', *, *, #32642, .T. ) ;
#13295 = DIRECTION ( 'NONE',  ( 0.000000000000000000, 0.000000000000000000, 1.000000000000000000 ) ) ;
#13296 = ORIENTED_EDGE ( 'NONE', *, *, #71336, .T. ) ;
#13297 = CARTESIAN_POINT ( 'NONE',  ( -3.000000000000000000, -18.13022148937243472, -15.02647892043568767 ) ) ;
#13298 = ORIENTED_EDGE ( 'NONE', *, *, #1499, .T. ) ;
#13299 = ORIENTED_EDGE ( 'NONE', *, *, #58326, .T. ) ;
#13300 = EDGE_CURVE ( 'NONE', #15455, #37544, #51944, .T. ) ;
#13301 = ORIENTED_EDGE ( 'NONE', *, *, #37358, .F. ) ;
#13302 = DIRECTION ( 'NONE',  ( -0.000000000000000000, -0.000000000000000000, -1.000000000000000000 ) ) ;
#13303 = ADVANCED_FACE ( 'NONE', ( #63623 ), #25961, .T. ) ;
#13304 = ORIENTED_EDGE ( 'NONE', *, *, #29714, .F. ) ;
#13305 = ORIENTED_EDGE ( 'NONE', *, *, #49197, .F. ) ;
#13306 = CARTESIAN_POINT ( 'NONE',  ( 92.69370383062498320, 88.66845928578037217, 80.32947916753381890 ) ) ;
#13307 = CARTESIAN_POINT ( 'NONE',  ( -0.2999999999999964362, 1.567547902908612184E-15, 12.80000000000000071 ) ) ;
#13308 = LINE ( 'NONE', #1707, #46475 ) ;
#13309 = ORIENTED_EDGE ( 'NONE', *, *, #46330, .F. ) ;
#13310 = EDGE_CURVE ( 'NONE', #57603, #26180, #32304, .T. ) ;
#13311 = ORIENTED_EDGE ( 'NONE', *, *, #46371, .F. ) ;
#13312 = EDGE_CURVE ( 'NONE', #14612, #53174, #37822, .T. ) ;
#13313 = AXIS2_PLACEMENT_3D ( 'NONE', #55154, #4048, #48771 ) ;
#13314 = AXIS2_PLACEMENT_3D ( 'NONE', #3565, #66340, #30612 ) ;
#13315 = ORIENTED_EDGE ( 'NONE', *, *, #12364, .F. ) ;
#13316 = CARTESIAN_POINT ( 'NONE',  ( 94.99999999999998579, 90.00000000000002842, 90.00000000000000000 ) ) ;
#13317 = VECTOR ( 'NONE', #40830, 1000.000000000000000 ) ;
#13318 = EDGE_LOOP ( 'NONE', ( #70335, #53626, #35354, #36132 ) ) ;
#13319 = DIRECTION ( 'NONE',  ( 0.000000000000000000, 0.000000000000000000, -1.000000000000000000 ) ) ;
#13320 = CARTESIAN_POINT ( 'NONE',  ( -2.500000000000014655, -69.70000000000003126, -255.0000000000000000 ) ) ;
#13321 = CARTESIAN_POINT ( 'NONE',  ( -97.30599797242227567, 90.94645204372872627, 74.89836836546780319 ) ) ;
#13322 = CARTESIAN_POINT ( 'NONE',  ( 10.00000000000000000, -30.00120703465222149, 22.64427369931158296 ) ) ;
#13323 = CARTESIAN_POINT ( 'NONE',  ( -93.67499999999998295, -207.7050326799711968, 84.15270833506762926 ) ) ;
#13324 = CARTESIAN_POINT ( 'NONE',  ( -6.880223345695647197, -142.5202692415819854, -5.500000000000000000 ) ) ;
#13325 = DIRECTION ( 'NONE',  ( 0.000000000000000000, 0.4539904997395479702, -0.8910065241883673437 ) ) ;
#13326 = CARTESIAN_POINT ( 'NONE',  ( -96.32499999999996021, -207.7050326799711968, 78.54354166840096241 ) ) ;
#13327 = CARTESIAN_POINT ( 'NONE',  ( 6.000000000000000000, 39.47590169984846398, 71.87247863392427405 ) ) ;
#13329 = CARTESIAN_POINT ( 'NONE',  ( -96.32500000000001705, 92.29496732002878900, 76.63854166840096127 ) ) ;
#13328 = CARTESIAN_POINT ( 'NONE',  ( 97.64999999999997726, 91.52997821335252127, 74.57479166840096241 ) ) ;
#13330 = ORIENTED_EDGE ( 'NONE', *, *, #17986, .F. ) ;
#13331 = CARTESIAN_POINT ( 'NONE',  ( 97.30629616937498838, 91.33154071421968467, 78.10697916753383652 ) ) ;
#13332 = EDGE_CURVE ( 'NONE', #26331, #36342, #25130, .T. ) ;
#13333 = DIRECTION ( 'NONE',  ( 0.000000000000000000, 0.5877852522924696954, -0.8090169943749498938 ) ) ;
#13334 = DIRECTION ( 'NONE',  ( -1.000000000000000000, 0.000000000000000000, 0.000000000000000000 ) ) ;
#13335 = DIRECTION ( 'NONE',  ( -1.000000000000000000, 0.000000000000000000, 0.000000000000000000 ) ) ;
#13336 = CARTESIAN_POINT ( 'NONE',  ( 0.000000000000000000, 39.04073710021344112, 15.48615015657596672 ) ) ;
#13337 = PLANE ( 'NONE',  #41412 ) ;
#13338 = VERTEX_POINT ( 'NONE', #9967 ) ;
#13339 = CARTESIAN_POINT ( 'NONE',  ( 0.000000000000000000, 0.000000000000000000, 0.000000000000000000 ) ) ;
#13340 = CIRCLE ( 'NONE', #22965, 2.500000000000000000 ) ;
#13341 = CARTESIAN_POINT ( 'NONE',  ( 15.00000000000000000, 8.688484142254226938, 21.88630264137359305 ) ) ;
#13342 = ORIENTED_EDGE ( 'NONE', *, *, #5174, .F. ) ;
#13343 = AXIS2_PLACEMENT_3D ( 'NONE', #36731, #49125, #25822 ) ;
#13344 = EDGE_LOOP ( 'NONE', ( #50314, #20792, #28938, #67780 ) ) ;
#13345 = CIRCLE ( 'NONE', #66172, 31.99999999999998934 ) ;
#13346 =( BOUNDED_CURVE ( )  B_SPLINE_CURVE ( 2, ( #5379, #68523, #73394, #28274, #44480, #73768, #73014 ),
 .UNSPECIFIED., .F., .F. ) 
 B_SPLINE_CURVE_WITH_KNOTS ( ( 3, 2, 2, 3 ),
 ( 0.5208333333333332593, 0.5277777777777776791, 0.5347222222222220989, 0.5416666666666665186 ),
 .UNSPECIFIED. ) 
 CURVE ( )  GEOMETRIC_REPRESENTATION_ITEM ( )  RATIONAL_B_SPLINE_CURVE ( ( 1.000000000000002220, 0.8660254037844365982, 1.000000000000000000, 0.8660254037844387076, 1.000000000000000000, 0.8660254037844408170, 0.9999999999999978906 ) ) 
 REPRESENTATION_ITEM ( '' )  );
#13347 = EDGE_CURVE ( 'NONE', #42089, #968, #70723, .T. ) ;
#13348 = DIRECTION ( 'NONE',  ( -1.000000000000000000, 0.000000000000000000, 0.000000000000000000 ) ) ;
#13349 = CARTESIAN_POINT ( 'NONE',  ( -97.65000000000001990, 90.00000000000004263, 86.26937500173430351 ) ) ;
#13350 = DIRECTION ( 'NONE',  ( -2.628368902995175337E-16, -1.000000000000000000, 0.000000000000000000 ) ) ;
#13351 = CARTESIAN_POINT ( 'NONE',  ( -3.000000000000000000, -23.29833615347109443, 3.418703333116492438 ) ) ;
#13352 = CARTESIAN_POINT ( 'NONE',  ( -96.15314808468747287, -208.0026889286704943, 78.26572916753382003 ) ) ;
#13353 = ADVANCED_FACE ( 'NONE', ( #72736 ), #26885, .T. ) ;
#13354 = ORIENTED_EDGE ( 'NONE', *, *, #23420, .F. ) ;
#13355 = LINE ( 'NONE', #19728, #54768 ) ;
#13356 = CARTESIAN_POINT ( 'NONE',  ( 12.00000000000000000, -22.67460108101774452, 6.353146135318220367 ) ) ;
#13357 = CARTESIAN_POINT ( 'NONE',  ( 93.67499999999999716, 87.70503267997126784, 85.74020833506763495 ) ) ;
#13358 = CARTESIAN_POINT ( 'NONE',  ( 0.000000000000000000, 79.10210256391368944, 21.60688246758614284 ) ) ;
#13359 = FACE_OUTER_BOUND ( 'NONE', #42431, .T. ) ;
#13360 = DIRECTION ( 'NONE',  ( -1.000000000000000000, 0.000000000000000000, 0.000000000000000000 ) ) ;
#13361 = FACE_OUTER_BOUND ( 'NONE', #21997, .T. ) ;
#13362 = CARTESIAN_POINT ( 'NONE',  ( 10.00000000000000000, 0.000000000000000000, 0.000000000000000000 ) ) ;
#13363 = LINE ( 'NONE', #24649, #54463 ) ;
#13364 = CARTESIAN_POINT ( 'NONE',  ( -43.60332556124591719, -107.0000000000000000, 2.500000000000002220 ) ) ;
#13365 = CARTESIAN_POINT ( 'NONE',  ( 93.84685191531248449, 88.00268892867053694, 82.28739583420048120 ) ) ;
#13366 = CARTESIAN_POINT ( 'NONE',  ( -93.84685191531248449, -208.0026889286704943, 85.14489583420048291 ) ) ;
#13367 = CARTESIAN_POINT ( 'NONE',  ( 10.00000000000000000, 37.58145647212453611, 0.6853352020791767529 ) ) ;
#13368 = EDGE_LOOP ( 'NONE', ( #31491, #57818, #19504, #3732 ) ) ;
#13369 = CIRCLE ( 'NONE', #55388, 82.00000000000000000 ) ;
#13370 = LINE ( 'NONE', #30652, #60461 ) ;
#13371 = VECTOR ( 'NONE', #23427, 1000.000000000000114 ) ;
#13372 = CARTESIAN_POINT ( 'NONE',  ( -94.99999999999997158, -213.0599564267049857, 79.99874999999998693 ) ) ;
#13373 = CARTESIAN_POINT ( 'NONE',  ( -92.69370383062505425, 88.66845928578038638, 77.84239583420047381 ) ) ;
#13374 = AXIS2_PLACEMENT_3D ( 'NONE', #55982, #49591, #26291 ) ;
#13375 = VECTOR ( 'NONE', #42225, 1000.000000000000000 ) ;
#13376 = CARTESIAN_POINT ( 'NONE',  ( 96.15314808468750130, -211.9973110713294489, 86.67947916753381321 ) ) ;
#13377 = VERTEX_POINT ( 'NONE', #32887 ) ;
#13378 = AXIS2_PLACEMENT_3D ( 'NONE', #16015, #22790, #38960 ) ;
#13379 =( REPRESENTATION_RELATIONSHIP ('NONE','NONE', #31117, #51769 ) REPRESENTATION_RELATIONSHIP_WITH_TRANSFORMATION ( #43309 )SHAPE_REPRESENTATION_RELATIONSHIP( ) );
#13380 = ORIENTED_EDGE ( 'NONE', *, *, #33145, .F. ) ;
#13381 = ORIENTED_EDGE ( 'NONE', *, *, #69082, .F. ) ;
#13382 = VECTOR ( 'NONE', #23072, 1000.000000000000000 ) ;
#13383 = DIRECTION ( 'NONE',  ( -1.000000000000000000, 0.000000000000000000, 0.000000000000000000 ) ) ;
#13385 = LINE ( 'NONE', #24668, #36666 ) ;
#13384 = VECTOR ( 'NONE', #4010, 1000.000000000000000 ) ;
#13386 = VERTEX_POINT ( 'NONE', #39299 ) ;
#13387 = VECTOR ( 'NONE', #40853, 999.9999999999998863 ) ;
#13388 = EDGE_CURVE ( 'NONE', #13338, #24878, #44572, .T. ) ;
#13389 = VERTEX_POINT ( 'NONE', #56215 ) ;
#13390 = CARTESIAN_POINT ( 'NONE',  ( -42.50000000000000000, 2.571758278209441267E-15, 20.99999999999999645 ) ) ;
#13391 = CARTESIAN_POINT ( 'NONE',  ( 96.15314808468750130, -211.9973110713294489, 81.75822916753382685 ) ) ;
#13392 = EDGE_CURVE ( 'NONE', #34044, #24357, #27636, .T. ) ;
#13393 = DIRECTION ( 'NONE',  ( 0.000000000000000000, 0.000000000000000000, 1.000000000000000000 ) ) ;
#13394 = DIRECTION ( 'NONE',  ( 1.000000000000000000, 0.000000000000000000, -0.000000000000000000 ) ) ;
#13395 = DIRECTION ( 'NONE',  ( -1.000000000000000000, 0.000000000000000000, -0.000000000000000000 ) ) ;
#13396 = DIRECTION ( 'NONE',  ( -1.000000000000000000, -0.000000000000000000, -0.000000000000000000 ) ) ;
#13397 = DIRECTION ( 'NONE',  ( 0.000000000000000000, 0.9723699203976773342, -0.2334453638559024213 ) ) ;
#13398 = CARTESIAN_POINT ( 'NONE',  ( 95.00000000000000000, -213.0599564267049857, 83.80875000000000341 ) ) ;
#13399 = ORIENTED_EDGE ( 'NONE', *, *, #25028, .T. ) ;
#13400 = EDGE_CURVE ( 'NONE', #73994, #26896, #21994, .T. ) ;
#13401 = ORIENTED_EDGE ( 'NONE', *, *, #61612, .T. ) ;
#13402 = ORIENTED_EDGE ( 'NONE', *, *, #54399, .F. ) ;
#13403 = ORIENTED_EDGE ( 'NONE', *, *, #71382, .F. ) ;
#13404 = CARTESIAN_POINT ( 'NONE',  ( 96.32499999999998863, -212.2949673200287179, 87.03666666666666174 ) ) ;
#13405 = CARTESIAN_POINT ( 'NONE',  ( -93.84685191531252713, 88.00268892867056536, 83.02822916753380866 ) ) ;
#13406 = CARTESIAN_POINT ( 'NONE',  ( 0.000000000000000000, 37.58145647212453611, 0.6853352020791767529 ) ) ;
#13407 = DIRECTION ( 'NONE',  ( -1.000000000000000000, 0.000000000000000000, 0.000000000000000000 ) ) ;
#13408 = CARTESIAN_POINT ( 'NONE',  ( 93.84685191531251292, -211.9973110713294489, 89.11364583420048291 ) ) ;
#13409 = LINE ( 'NONE', #2175, #2332 ) ;
#13410 = ORIENTED_EDGE ( 'NONE', *, *, #3528, .T. ) ;
#13411 = DIRECTION ( 'NONE',  ( 0.000000000000000000, 0.000000000000000000, 1.000000000000000000 ) ) ;
#13412 = ORIENTED_EDGE ( 'NONE', *, *, #65183, .F. ) ;
#13413 = CARTESIAN_POINT ( 'NONE',  ( 0.3000000000000016542, 6.123233995736766282E-16, -5.000000000000000000 ) ) ;
#13414 = EDGE_CURVE ( 'NONE', #69389, #66054, #31073, .T. ) ;
#13415 = VERTEX_POINT ( 'NONE', #6921 ) ;
#13416 = CARTESIAN_POINT ( 'NONE',  ( -96.32500000000001705, 92.29496732002878900, 85.52854166840096184 ) ) ;
#13417 = CARTESIAN_POINT ( 'NONE',  ( 92.69370383062498320, 88.66845928578037217, 86.67947916753382742 ) ) ;
#13418 = EDGE_CURVE ( 'NONE', #43453, #55469, #18934, .T. ) ;
#13419 = EDGE_CURVE ( 'NONE', #34204, #39425, #7094, .T. ) ;
#13420 = LINE ( 'NONE', #1454, #32164 ) ;
#13421 = DIRECTION ( 'NONE',  ( -1.000000000000000000, 0.000000000000000000, 0.000000000000000000 ) ) ;
#13422 = CARTESIAN_POINT ( 'NONE',  ( -93.67499999999998295, -207.7050326799711968, 78.43770833506764006 ) ) ;
#13423 =( GEOMETRIC_REPRESENTATION_CONTEXT ( 3 ) GLOBAL_UNCERTAINTY_ASSIGNED_CONTEXT ( ( #50455 ) ) GLOBAL_UNIT_ASSIGNED_CONTEXT ( ( #48956, #2416, #59522 ) ) REPRESENTATION_CONTEXT ( 'NONE', 'WORKASPACE' ) );
#13424 = VECTOR ( 'NONE', #12331, 1000.000000000000000 ) ;
#13425 = FACE_OUTER_BOUND ( 'NONE', #51047, .T. ) ;
#13426 = ORIENTED_EDGE ( 'NONE', *, *, #8249, .F. ) ;
#13427 = DIRECTION ( 'NONE',  ( -1.000000000000000000, 0.000000000000000000, -0.000000000000000000 ) ) ;
#13428 = EDGE_CURVE ( 'NONE', #28262, #16918, #33487, .T. ) ;
#13429 = FACE_OUTER_BOUND ( 'NONE', #53169, .T. ) ;
#13430 = ORIENTED_EDGE ( 'NONE', *, *, #59532, .T. ) ;
#13431 = VECTOR ( 'NONE', #37597, 1000.000000000000000 ) ;
#13432 = ORIENTED_EDGE ( 'NONE', *, *, #73653, .F. ) ;
#13433 = CARTESIAN_POINT ( 'NONE',  ( -92.69370383062498320, -210.0000000000000568, 74.79348190356851944 ) ) ;
#13434 = VECTOR ( 'NONE', #7699, 1000.000000000000000 ) ;
#13435 = EDGE_CURVE ( 'NONE', #53644, #69813, #30561, .T. ) ;
#13436 = CARTESIAN_POINT ( 'NONE',  ( 10.00000000000000000, 46.21855187248719687, -62.20884554313968806 ) ) ;
#13437 = CARTESIAN_POINT ( 'NONE',  ( 10.00000000000000000, 6.555932627142418312, 37.01155633439060466 ) ) ;
#13438 = VECTOR ( 'NONE', #72392, 1000.000000000000000 ) ;
#13439 =( BOUNDED_CURVE ( )  B_SPLINE_CURVE ( 2, ( #55556, #44664, #49902, #40124, #5560, #5188, #28090 ),
 .UNSPECIFIED., .F., .F. ) 
 B_SPLINE_CURVE_WITH_KNOTS ( ( 3, 2, 2, 3 ),
 ( 0.5080151867278726030, 0.5150708844869413827, 0.5221266500278589628, 0.5291824299534890752 ),
 .UNSPECIFIED. ) 
 CURVE ( )  GEOMETRIC_REPRESENTATION_ITEM ( )  RATIONAL_B_SPLINE_CURVE ( ( 0.9999974259466133386, 0.8660266908234961480, 1.000000000000000000, 0.8660254037844387076, 1.000000000000000000, 0.8660254037844387076, 1.000000000000000000 ) ) 
 REPRESENTATION_ITEM ( '' )  );
#13440 = CARTESIAN_POINT ( 'NONE',  ( -92.69370383062498320, -209.9999999999999716, 86.30906250086715659 ) ) ;
#13441 = VERTEX_POINT ( 'NONE', #51685 ) ;
#13442 = ORIENTED_EDGE ( 'NONE', *, *, #58136, .T. ) ;
#13443 = ORIENTED_EDGE ( 'NONE', *, *, #37797, .F. ) ;
#13444 = LINE ( 'NONE', #25833, #19821 ) ;
#13445 = AXIS2_PLACEMENT_3D ( 'NONE', #19265, #53119, #42577 ) ;
#13446 = CARTESIAN_POINT ( 'NONE',  ( 92.69370383062498320, 90.00000000000002842, 89.16656250086715829 ) ) ;
#13447 = DIRECTION ( 'NONE',  ( 1.000000000000000000, 0.000000000000000000, 0.000000000000000000 ) ) ;
#13448 = CARTESIAN_POINT ( 'NONE',  ( 96.15314808468748708, 88.00268892867053694, 82.86947916753379673 ) ) ;
#13449 = DIRECTION ( 'NONE',  ( 0.000000000000000000, 0.3090169943749480619, -0.9510565162951533091 ) ) ;
#13450 = CIRCLE ( 'NONE', #55471, 77.49900000000000944 ) ;
#13451 = CARTESIAN_POINT ( 'NONE',  ( -100.0000000000260485, 95.00000000000001421, -65.00000000000001421 ) ) ;
#13452 = DIRECTION ( 'NONE',  ( 0.000000000000000000, -0.9945218953682730678, -0.1045284632676570929 ) ) ;
#13453 = DIRECTION ( 'NONE',  ( 0.000000000000000000, 0.000000000000000000, -1.000000000000000000 ) ) ;
#13454 = CARTESIAN_POINT ( 'NONE',  ( -3.000000000000000000, 8.688484142253939169, 21.88630264137371029 ) ) ;
#13455 = DIRECTION ( 'NONE',  ( 0.000000000000000000, 0.000000000000000000, -1.000000000000000000 ) ) ;
#13456 = CARTESIAN_POINT ( 'NONE',  ( 11.99999999999999822, 34.44570377933598593, 69.42325613327452061 ) ) ;
#13457 = CARTESIAN_POINT ( 'NONE',  ( 0.000000000000000000, 0.000000000000000000, 0.000000000000000000 ) ) ;
#13458 = CARTESIAN_POINT ( 'NONE',  ( 5.999999999999999112, -67.80270845531855173, -46.11716303203260736 ) ) ;
#13459 = ORIENTED_EDGE ( 'NONE', *, *, #47109, .T. ) ;
#13460 = CARTESIAN_POINT ( 'NONE',  ( -92.69370383062505425, 88.66845928578038638, 84.82739583420048746 ) ) ;
#13461 = DIRECTION ( 'NONE',  ( -1.000000000000000000, 0.000000000000000000, 0.000000000000000000 ) ) ;
#13462 = DIRECTION ( 'NONE',  ( -0.000000000000000000, 1.000000000000000000, 1.224646799147353207E-16 ) ) ;
#13463 = PRODUCT_DEFINITION_SHAPE ( 'NONE', 'NONE',  #74372 ) ;
#13464 = ORIENTED_EDGE ( 'NONE', *, *, #31251, .F. ) ;
#13465 = DIRECTION ( 'NONE',  ( 0.000000000000000000, -0.1564344650402170744, -0.9876883405951399908 ) ) ;
#13466 = CARTESIAN_POINT ( 'NONE',  ( 10.00000000000000000, -6.903761155837252694, -77.19088730480530103 ) ) ;
#13467 = DIRECTION ( 'NONE',  ( -1.000000000000000000, -0.000000000000000000, -0.000000000000000000 ) ) ;
#13468 = EDGE_CURVE ( 'NONE', #32997, #22617, #29895, .T. ) ;
#13469 = PRESENTATION_LAYER_ASSIGNMENT (  '', '', ( #62718 ) ) ;
#13470 = VECTOR ( 'NONE', #26101, 1000.000000000000000 ) ;
#13471 = DIRECTION ( 'NONE',  ( -1.000000000000000000, 0.000000000000000000, 0.000000000000000000 ) ) ;
#13472 = CARTESIAN_POINT ( 'NONE',  ( 97.30629616937498838, -211.3315407142195852, 81.81114583420048803 ) ) ;
#13473 = EDGE_CURVE ( 'NONE', #6773, #57738, #1340, .T. ) ;
#13474 = CIRCLE ( 'NONE', #33879, 82.00000000000000000 ) ;
#13475 = EDGE_CURVE ( 'NONE', #35978, #32156, #21464, .T. ) ;
#13476 = ORIENTED_EDGE ( 'NONE', *, *, #47444, .T. ) ;
#13477 = EDGE_CURVE ( 'NONE', #7050, #74311, #56494, .T. ) ;
#13478 = ORIENTED_EDGE ( 'NONE', *, *, #49318, .T. ) ;
#13479 = CIRCLE ( 'NONE', #38716, 31.99999999999999645 ) ;
#13480 = VERTEX_POINT ( 'NONE', #11812 ) ;
#13481 = CARTESIAN_POINT ( 'NONE',  ( 10.00000000000000000, 0.000000000000000000, 0.000000000000000000 ) ) ;
#13482 = CIRCLE ( 'NONE', #55519, 3.000000000000000000 ) ;
#13483 = EDGE_CURVE ( 'NONE', #27765, #16367, #52712, .T. ) ;
#13484 = CARTESIAN_POINT ( 'NONE',  ( -95.00000000002611955, 90.00000000000007105, -65.00000000000000000 ) ) ;
#13485 = ORIENTED_EDGE ( 'NONE', *, *, #51929, .T. ) ;
#13486 = CARTESIAN_POINT ( 'NONE',  ( 97.30629616937498838, -208.6684592857803011, 80.64697916753382856 ) ) ;
#13487 = EDGE_CURVE ( 'NONE', #65774, #17672, #15514, .T. ) ;
#13488 = ORIENTED_EDGE ( 'NONE', *, *, #5144, .T. ) ;
#13489 = CARTESIAN_POINT ( 'NONE',  ( 0.000000000000000000, -73.44644590900043113, -24.73286445877782924 ) ) ;
#13490 = ORIENTED_EDGE ( 'NONE', *, *, #23709, .F. ) ;
#13491 = AXIS2_PLACEMENT_3D ( 'NONE', #15325, #33742, #22468 ) ;
#13492 = ORIENTED_EDGE ( 'NONE', *, *, #3407, .T. ) ;
#13493 = CYLINDRICAL_SURFACE ( 'NONE', #15348, 77.49899999999999523 ) ;
#13494 = VECTOR ( 'NONE', #53397, 1000.000000000000000 ) ;
#13495 = CARTESIAN_POINT ( 'NONE',  ( 97.64999999999999147, -209.9999999999999716, 80.15749999999999886 ) ) ;
#13496 = ORIENTED_EDGE ( 'NONE', *, *, #50920, .F. ) ;
#13497 = DIRECTION ( 'NONE',  ( -1.000000000000000000, -0.000000000000000000, -0.000000000000000000 ) ) ;
#13498 = CARTESIAN_POINT ( 'NONE',  ( 97.64999999999999147, -209.9999999999999716, 84.04687500173430692 ) ) ;
#13499 = CARTESIAN_POINT ( 'NONE',  ( 92.34999999999999432, 91.52997821335252127, 89.31208333333333371 ) ) ;
#13500 = ORIENTED_EDGE ( 'NONE', *, *, #18270, .T. ) ;
#13501 = CARTESIAN_POINT ( 'NONE',  ( 15.70000000000286455, -120.0000000000000568, -74.99999999999958789 ) ) ;
#13502 = DIRECTION ( 'NONE',  ( -0.000000000000000000, -0.000000000000000000, -1.000000000000000000 ) ) ;
#13503 = ORIENTED_EDGE ( 'NONE', *, *, #52611, .F. ) ;
#13504 = VERTEX_POINT ( 'NONE', #41509 ) ;
#13505 = CARTESIAN_POINT ( 'NONE',  ( -95.00000000000002842, 87.33691857156074434, 88.69031250086716511 ) ) ;
#13506 = CARTESIAN_POINT ( 'NONE',  ( 93.84685191531248449, 88.00268892867053694, 84.66864583420047552 ) ) ;
#13507 = ADVANCED_FACE ( 'NONE', ( #58063 ), #52409, .T. ) ;
#13508 = ORIENTED_EDGE ( 'NONE', *, *, #68261, .T. ) ;
#13509 = CARTESIAN_POINT ( 'NONE',  ( 92.34999999999999432, 90.00000000000002842, 86.90437500173429441 ) ) ;
#13510 = ORIENTED_EDGE ( 'NONE', *, *, #25557, .F. ) ;
#13511 = CARTESIAN_POINT ( 'NONE',  ( 11.99999999999999822, 0.000000000000000000, 0.000000000000000000 ) ) ;
#13512 = EDGE_CURVE ( 'NONE', #61999, #58994, #64177, .T. ) ;
#13513 = EDGE_CURVE ( 'NONE', #72913, #72132, #51537, .T. ) ;
#13514 = VERTEX_POINT ( 'NONE', #29842 ) ;
#13515 = ORIENTED_EDGE ( 'NONE', *, *, #11855, .T. ) ;
#13516 = VERTEX_POINT ( 'NONE', #58809 ) ;
#13517 = DIRECTION ( 'NONE',  ( -0.000000000000000000, -0.000000000000000000, 1.000000000000000000 ) ) ;
#13518 = DIRECTION ( 'NONE',  ( -1.000000000000000000, -0.000000000000000000, 0.000000000000000000 ) ) ;
#13519 = CARTESIAN_POINT ( 'NONE',  ( -97.65000000000001990, 88.47002178664754979, 85.60791666666665378 ) ) ;
#13520 = VERTEX_POINT ( 'NONE', #1701 ) ;
#13521 = EDGE_CURVE ( 'NONE', #21663, #62600, #38334, .T. ) ;
#13522 = CARTESIAN_POINT ( 'NONE',  ( 97.25633982090072038, 90.55049048501746256, 74.79348190356850523 ) ) ;
#13523 = DIRECTION ( 'NONE',  ( -1.000000000000000000, 0.000000000000000000, 0.000000000000000000 ) ) ;
#13524 = ORIENTED_EDGE ( 'NONE', *, *, #36941, .T. ) ;
#13525 = DIRECTION ( 'NONE',  ( 1.000000000000000000, 0.000000000000000000, 0.000000000000000000 ) ) ;
#13526 = CARTESIAN_POINT ( 'NONE',  ( -92.69370383062498320, -208.6684592857803011, 83.66322916753379957 ) ) ;
#13527 = EDGE_LOOP ( 'NONE', ( #43473, #50398, #72933, #69546 ) ) ;
#13528 = CYLINDRICAL_SURFACE ( 'NONE', #31451, 16.00000000000000000 ) ;
#13529 = FACE_OUTER_BOUND ( 'NONE', #59311, .T. ) ;
#13530 = FACE_OUTER_BOUND ( 'NONE', #17130, .T. ) ;
#13531 =( GEOMETRIC_REPRESENTATION_CONTEXT ( 3 ) GLOBAL_UNCERTAINTY_ASSIGNED_CONTEXT ( ( #8474 ) ) GLOBAL_UNIT_ASSIGNED_CONTEXT ( ( #32161, #3634, #59647 ) ) REPRESENTATION_CONTEXT ( 'NONE', 'WORKASPACE' ) );
#13532 = CARTESIAN_POINT ( 'NONE',  ( 10.00000000000000000, -16.45098606841102651, -33.79645857604531045 ) ) ;
#13533 = CIRCLE ( 'NONE', #8763, 42.00000000000000000 ) ;
#13534 = FACE_OUTER_BOUND ( 'NONE', #15831, .T. ) ;
#13535 = DIRECTION ( 'NONE',  ( -1.000000000000000000, 0.000000000000000000, 0.000000000000000000 ) ) ;
#13536 = CARTESIAN_POINT ( 'NONE',  ( 2.874421927457452952, -143.3717286177755739, 5.500000000000000000 ) ) ;
#13537 = CARTESIAN_POINT ( 'NONE',  ( 0.000000000000000000, -13.04903810567647682, -19.60159698893442481 ) ) ;
#13538 = CARTESIAN_POINT ( 'NONE',  ( 18.80329974962065265, -105.8248132807389084, -5.500000000000000000 ) ) ;
#13539 = CARTESIAN_POINT ( 'NONE',  ( -97.30629616937501680, 88.66845928578038638, 75.09072916753382287 ) ) ;
#13540 = CARTESIAN_POINT ( 'NONE',  ( 1.560000000000000053, 1.732050807568878747, 7.017607234860990640E-28 ) ) ;
#13541 = DIRECTION ( 'NONE',  ( 0.02332147558787931590, 0.9997280174009348652, -0.000000000000000000 ) ) ;
#13542 = VECTOR ( 'NONE', #51030, 1000.000000000000000 ) ;
#13543 = CARTESIAN_POINT ( 'NONE',  ( 10.00000000000000000, 38.55633173627034438, -16.65560815589369881 ) ) ;
#13544 = LINE ( 'NONE', #59418, #46133 ) ;
#13545 = DIRECTION ( 'NONE',  ( 0.000000000000000000, 0.4067366430757989870, 0.9135454576426015327 ) ) ;
#13546 = VECTOR ( 'NONE', #56750, 1000.000000000000114 ) ;
#13547 = LINE ( 'NONE', #19917, #40699 ) ;
#13548 = CARTESIAN_POINT ( 'NONE',  ( 11.99999999999999822, -81.96053171279903893, 2.543863470248101333 ) ) ;
#13549 = LINE ( 'NONE', #54521, #35220 ) ;
#13550 = CARTESIAN_POINT ( 'NONE',  ( -94.99999999999997158, -206.9400435732949575, 88.57124999999999204 ) ) ;
#13551 = LINE ( 'NONE', #6808, #22465 ) ;
#13552 = ORIENTED_EDGE ( 'NONE', *, *, #9921, .T. ) ;
#13553 = CARTESIAN_POINT ( 'NONE',  ( 92.35000000005783249, 89.99998877583867340, 75.47473230081648410 ) ) ;
#13554 = CARTESIAN_POINT ( 'NONE',  ( 97.64999999999999147, -209.9999999999999716, 88.41249999999999432 ) ) ;
#13555 = PLANE ( 'NONE',  #14202 ) ;
#13556 = LINE ( 'NONE', #36861, #7748 ) ;
#13557 = EDGE_CURVE ( 'NONE', #11086, #54488, #43000, .T. ) ;
#13558 = DIRECTION ( 'NONE',  ( 0.000000000000000000, -0.2334453638558922628, -0.9723699203976798877 ) ) ;
#13559 = ORIENTED_EDGE ( 'NONE', *, *, #51162, .F. ) ;
#13560 = EDGE_CURVE ( 'NONE', #22617, #54538, #30585, .T. ) ;
#13561 = CARTESIAN_POINT ( 'NONE',  ( 10.00000000000000000, 10.74501242461282757, 35.92658777277515014 ) ) ;
#13562 = FILL_AREA_STYLE ('',( #41770 ) ) ;
#13563 = ORIENTED_EDGE ( 'NONE', *, *, #40248, .F. ) ;
#13564 = CARTESIAN_POINT ( 'NONE',  ( 93.84685191531249870, -208.0026889286704943, 84.45697916753380241 ) ) ;
#13565 = CARTESIAN_POINT ( 'NONE',  ( 96.15314808468750130, -211.9973110713294489, 89.37822916753381719 ) ) ;
#13566 = ORIENTED_EDGE ( 'NONE', *, *, #1687, .F. ) ;
#13567 = CARTESIAN_POINT ( 'NONE',  ( 0.000000000000000000, -59.75363087400035056, -56.15606465355021015 ) ) ;
#13568 = AXIS2_PLACEMENT_3D ( 'NONE', #18222, #11465, #69351 ) ;
#13569 = ORIENTED_EDGE ( 'NONE', *, *, #15432, .T. ) ;
#13570 = CARTESIAN_POINT ( 'NONE',  ( -96.32499999999996021, -212.2949673200287179, 80.58083333333331666 ) ) ;
#13571 = ORIENTED_EDGE ( 'NONE', *, *, #35543, .T. ) ;
#13572 = CARTESIAN_POINT ( 'NONE',  ( -95.00000000000002842, 92.66308142843932671, 82.02281250086714692 ) ) ;
#13573 = VECTOR ( 'NONE', #60475, 1000.000000000000000 ) ;
#13574 = VERTEX_POINT ( 'NONE', #48988 ) ;
#13575 = ORIENTED_EDGE ( 'NONE', *, *, #56899, .T. ) ;
#13576 = CARTESIAN_POINT ( 'NONE',  ( 10.00000000000000000, 0.000000000000000000, 0.000000000000000000 ) ) ;
#13577 = ORIENTED_EDGE ( 'NONE', *, *, #4530, .T. ) ;
#13578 = CARTESIAN_POINT ( 'NONE',  ( -100.0000000000000142, 85.00000000000002842, -79.99999999999998579 ) ) ;
#13579 = LINE ( 'NONE', #20335, #53623 ) ;
#13580 = EDGE_CURVE ( 'NONE', #7432, #75, #39527, .T. ) ;
#13581 = EDGE_CURVE ( 'NONE', #38472, #7584, #49363, .T. ) ;
#13582 = ORIENTED_EDGE ( 'NONE', *, *, #34062, .F. ) ;
#13583 = CARTESIAN_POINT ( 'NONE',  ( 10.00000000000000000, -71.87247863392384772, -39.47590169984921005 ) ) ;
#13584 = VECTOR ( 'NONE', #21622, 1000.000000000000000 ) ;
#13585 = ORIENTED_EDGE ( 'NONE', *, *, #65187, .F. ) ;
#13586 = CARTESIAN_POINT ( 'NONE',  ( 92.35000000000000853, -211.5299782133524218, 81.24229166840096639 ) ) ;
#13587 = AXIS2_PLACEMENT_3D ( 'NONE', #45939, #69592, #33899 ) ;
#13588 = EDGE_LOOP ( 'NONE', ( #11174, #40881, #17153, #73782 ) ) ;
#13589 = CIRCLE ( 'NONE', #38958, 82.00000000000000000 ) ;
#13590 = EDGE_LOOP ( 'NONE', ( #62819, #69121 ) ) ;
#13591 = AXIS2_PLACEMENT_3D ( 'NONE', #30361, #12702, #53307 ) ;
#13592 = ORIENTED_EDGE ( 'NONE', *, *, #35560, .T. ) ;
#13593 = CARTESIAN_POINT ( 'NONE',  ( 93.84685191531249870, -208.0026889286704943, 77.47197916753380298 ) ) ;
#13594 = AXIS2_PLACEMENT_3D ( 'NONE', #9847, #8744, #55711 ) ;
#13596 = ADVANCED_FACE ( 'NONE', ( #59549 ), #72294, .F. ) ;
#13595 = CARTESIAN_POINT ( 'NONE',  ( -92.35000000000003695, 90.00000000000004263, 83.33250000000001023 ) ) ;
#13597 = ADVANCED_FACE ( 'NONE', ( #2071 ), #20434, .F. ) ;
#13598 = CONTEXT_DEPENDENT_SHAPE_REPRESENTATION ( #73864, #42753 ) ;
#13599 = CARTESIAN_POINT ( 'NONE',  ( -0.8815729230226008184, -93.47222532549339746, 2.500000000000000000 ) ) ;
#13600 = VERTEX_POINT ( 'NONE', #54639 ) ;
#13601 = CARTESIAN_POINT ( 'NONE',  ( 92.35000000000000853, -209.9999999999999716, 75.00000000000000000 ) ) ;
#13602 = DIRECTION ( 'NONE',  ( 0.000000000000000000, 0.000000000000000000, -1.000000000000000000 ) ) ;
#13603 = DIRECTION ( 'NONE',  ( 0.000000000000000000, 0.3826834323650842862, 0.9238795325112890700 ) ) ;
#13604 = LINE ( 'NONE', #48193, #51724 ) ;
#13605 = PLANE ( 'NONE',  #9496 ) ;
#13606 = CARTESIAN_POINT ( 'NONE',  ( -97.30629616937497417, -211.3315407142195852, 81.44072916753381719 ) ) ;
#13607 = CARTESIAN_POINT ( 'NONE',  ( -97.30629616937501680, 90.00000000000004263, 80.27656250086714351 ) ) ;
#13608 = ORIENTED_EDGE ( 'NONE', *, *, #9185, .F. ) ;
#13609 = CARTESIAN_POINT ( 'NONE',  ( 96.15314808468748708, 88.00268892867053694, 80.32947916753380468 ) ) ;
#13610 = ORIENTED_EDGE ( 'NONE', *, *, #32341, .T. ) ;
#13611 = DIRECTION ( 'NONE',  ( 0.000000000000000000, -0.9781476007338070211, -0.2079116908177532363 ) ) ;
#13612 = CARTESIAN_POINT ( 'NONE',  ( 0.000000000000000000, 20.40083707022882820, 72.35432306680490910 ) ) ;
#13613 = CARTESIAN_POINT ( 'NONE',  ( 93.67499999999999716, 87.70503267997126784, 77.48520833506763950 ) ) ;
#13614 = CARTESIAN_POINT ( 'NONE',  ( 15.00000000000000000, 9.615535125379096826, 24.73947219025905042 ) ) ;
#13615 = DIRECTION ( 'NONE',  ( -1.000000000000000000, 0.000000000000000000, 0.000000000000000000 ) ) ;
#13616 = CARTESIAN_POINT ( 'NONE',  ( -93.84685191531247028, -211.9973110713294489, 82.86947916753379673 ) ) ;
#13617 = CARTESIAN_POINT ( 'NONE',  ( -97.64999999999990621, -211.5299782133524786, 89.41791666666667027 ) ) ;
#13618 = DIRECTION ( 'NONE',  ( 0.000000000000000000, 0.07845909572784512398, -0.9969173337331279638 ) ) ;
#13619 = DIRECTION ( 'NONE',  ( -1.000000000000000000, -0.000000000000000000, 0.000000000000000000 ) ) ;
#13620 = ORIENTED_EDGE ( 'NONE', *, *, #17255, .T. ) ;
#13621 = ORIENTED_EDGE ( 'NONE', *, *, #47689, .T. ) ;
#13622 = DIRECTION ( 'NONE',  ( 0.000000000000000000, 0.000000000000000000, -1.000000000000000000 ) ) ;
#13623 = DIRECTION ( 'NONE',  ( -1.000000000000000000, 0.000000000000000000, 0.000000000000000000 ) ) ;
#13624 = CARTESIAN_POINT ( 'NONE',  ( -97.30629616937501680, 90.00000000000004263, 84.56281250086713897 ) ) ;
#13625 = CARTESIAN_POINT ( 'NONE',  ( -12.50000000000000000, -107.5000000000000000, 2.500000000000000000 ) ) ;
#13626 = FACE_OUTER_BOUND ( 'NONE', #10160, .T. ) ;
#13627 = CIRCLE ( 'NONE', #64045, 12.85999999999999943 ) ;
#13628 = DIRECTION ( 'NONE',  ( 0.000000000000000000, 0.000000000000000000, -1.000000000000000000 ) ) ;
#13629 = DIRECTION ( 'NONE',  ( 1.000000000000000000, 0.000000000000000000, 0.000000000000000000 ) ) ;
#13630 = B_SPLINE_CURVE_WITH_KNOTS ( 'NONE', 1,
 ( #59159, #47142 ),
 .UNSPECIFIED., .F., .F.,
 ( 2, 2 ),
 ( 0.000000000000000000, 1.000000000000000000 ),
 .UNSPECIFIED. ) ;
#13631 = ORIENTED_EDGE ( 'NONE', *, *, #6248, .T. ) ;
#13632 = CARTESIAN_POINT ( 'NONE',  ( -97.30629616937501680, 91.33154071421968467, 76.25489583420049655 ) ) ;
#13633 = CARTESIAN_POINT ( 'NONE',  ( 15.00000000000000000, 14.60985201121729737, 18.46759930825687235 ) ) ;
#13634 = CARTESIAN_POINT ( 'NONE',  ( -10.00000000000000000, 0.000000000000000000, 0.000000000000000000 ) ) ;
#13635 = DIRECTION ( 'NONE',  ( -0.000000000000000000, -0.000000000000000000, -1.000000000000000000 ) ) ;
#13636 = CARTESIAN_POINT ( 'NONE',  ( 10.00000000000000000, 41.76937507738788469, 62.50329211542452157 ) ) ;
#13637 = CARTESIAN_POINT ( 'NONE',  ( -97.30629616937497417, -208.6684592857803011, 87.84364583420048689 ) ) ;
#13638 = PRESENTATION_STYLE_ASSIGNMENT (( #53869 ) ) ;
#13639 = DIRECTION ( 'NONE',  ( 0.000000000000000000, -0.8910065241883722287, 0.4539904997395382558 ) ) ;
#13640 =( BOUNDED_CURVE ( )  B_SPLINE_CURVE ( 2, ( #46570, #51467, #11983, #22163, #45853, #23, #22917, #6718, #28164, #68775, #69499, #40941, #12348, #46210, #17263, #35290, #58217, #50720, #68408, #73646, #63145, #45102, #11601, #16515, #57488, #62405, #6005, #51840, #10885, #1122, #7824, #2602, #1492, #25118, #18722, #48050, #41659, #30740, #42411, #25483, #36384, #19468, #70964, #36759, #53320, #14194, #1859, #42781, #30003, #52951, #53684, #24018, #2224, #48415, #24378, #65351, #64600, #13818, #13084, #59707, #8185, #24743, #19830, #31114, #54066, #71326, #70582, #65716, #37147, #7458, #46946, #30373, #47673, #42048, #60090, #29626, #12713, #52571, #69860, #36023, #18358, #41302, #58968, #19100, #64242, #35643, #58582, #7085, #47318, #70217, #64985, #13460, #59334, #4057, #26954, #66820, #55543, #38627, #67191, #44264, #49884, #54426, #9297, #8570, #44647, #67566, #43541, #49520, #27321, #73192, #55910, #71703, #20202, #15690, #72803, #20589, #15308, #32597, #61186, #32961, #61560, #14567, #66456, #10042, #31855, #3690, #60453, #66096, #2961, #43171, #72445, #21304, #4423, #60816, #50255, #14943, #54794, #21691, #16058, #25849, #38998, #20947, #37886, #48779, #9676, #31487, #26214, #37517, #32214, #8935, #3322, #26589, #55167, #43902, #49154, #72080, #38243, #11887, #28821, #298, #11521, #57772, #69407, #661, #56672, #62694, #51375, #5912, #17538, #33328, #68315, #33720, #27710, #23192, #40108, #16808, #39747, #63419, #34838, #6276, #29174, #73936, #56289, #17909, #10413, #22447, #4808, #61933, #52118, #34455, #5172, #28072, #74313, #46119, #50632, #11165, #73559, #23553, #46482, #45391, #28442, #69054, #22073, #57396, #10795, #34088, #45015, #40469, #67942, #16431, #39369, #22826, #62307, #51015, #57034, #5545, #45766, #68689, #17174, #63062, #51753, #64897, #6993, #13373, #12630, #36304, #42332, #35567, #59247, #48332, #24659, #53236, #69778, #6631, #30292, #1408, #35198, #41960, #7739, #58497, #47966, #31027, #29917, #52869, #58882, #19008, #29543, #2524, #53981, #46866, #19382, #25406, #1772, #30654, #64154, #63792, #18279, #70137, #71241, #41578, #47590, #70882, #70495, #65265, #53600, #18637, #2139, #40856, #24300, #25024, #13738, #12265, #47227, #36675, #64518, #59621, #12996, #58132, #8104, #35934, #52482, #41216, #1033 ),
 .UNSPECIFIED., .F., .F. ) 
 B_SPLINE_CURVE_WITH_KNOTS ( ( 3, 2, 2, 2, 2, 2, 2, 2, 2, 2, 2, 2, 2, 2, 2, 2, 2, 2, 2, 2, 2, 2, 2, 2, 2, 2, 2, 2, 2, 2, 2, 2, 2, 2, 2, 2, 2, 2, 2, 2, 2, 2, 2, 2, 2, 2, 2, 2, 2, 2, 2, 2, 2, 2, 2, 2, 2, 2, 2, 2, 2, 2, 2, 2, 2, 2, 2, 2, 2, 2, 2, 2, 2, 2, 2, 2, 2, 2, 2, 2, 2, 2, 2, 2, 2, 2, 2, 2, 2, 2, 2, 2, 2, 2, 2, 2, 2, 2, 2, 2, 2, 2, 2, 2, 2, 2, 2, 2, 2, 2, 2, 2, 2, 2, 2, 2, 2, 2, 2, 2, 2, 2, 2, 2, 2, 2, 2, 2, 2, 2, 2, 2, 2, 2, 2, 2, 2, 2, 2, 2, 2, 3 ),
 ( 0.000000000000000000, 0.007055765384978174640, 0.01411153076995634928, 0.02116729615493452218, 0.02822306153991269856, 0.03527882692489087840, 0.04233459230986904437, 0.04939035769484722421, 0.05644612307982539712, 0.06350188846480357696, 0.07055765384978175681, 0.07761341923475993665, 0.08466918461973808874, 0.09172495000471626858, 0.09878071538969444843, 0.1058364807746726144, 0.1128922461596507942, 0.1199480115446289741, 0.1270037769296071539, 0.1340595423145853338, 0.1411153076995635136, 0.1481710730845416935, 0.1552268384695198733, 0.1622826038544979976, 0.1693383692394761775, 0.1763941346244543573, 0.1834499000094325372, 0.1905056653944107170, 0.1975614307793888969, 0.2046171961643670489, 0.2116729615493452288, 0.2187287269343234364, 0.2257844923193015885, 0.2328402577042797683, 0.2398960230892579482, 0.2469517884742361002, 0.2540075538592143078, 0.2610633192441924599, 0.2681190846291706675, 0.2751748500141487641, 0.2822306153991270272, 0.2892863807841051238, 0.2963421461690833869, 0.3033979115540614835, 0.3104536769390397466, 0.3175094423240178432, 0.3245652077089959953, 0.3316209730939742029, 0.3386767384789523549, 0.3457325038639306181, 0.3527882692489087146, 0.3598440346338869222, 0.3668998000188650743, 0.3739555654038432819, 0.3810113307888214340, 0.3880670961737995861, 0.3951228615587777937, 0.4021786269437559458, 0.4092343923287340979, 0.4162901577137123055, 0.4233459230986904576, 0.4304016884836686652, 0.4374574538686468728, 0.4445132192536250249, 0.4515689846386031769, 0.4586247500235813290, 0.4656805154085595366, 0.4727362807935376887, 0.4797920461785158963, 0.4868478115634940484, 0.4939035769484722005, 0.5009593423334504081, 0.5080151077184286157, 0.5150708731034067123, 0.5221266384883849199, 0.5291824038733631275, 0.5362381692583413351, 0.5432939346433194316, 0.5503497000282975282, 0.5574054654132758468, 0.5644612307982540544, 0.5715169961832321510, 0.5785727615682102476, 0.5856285269531883442, 0.5926842923381667738, 0.5997400577231448704, 0.6067958231081229670, 0.6138515884931011746, 0.6209073538780794932, 0.6279631192630575898, 0.6350188846480356863, 0.6420746500330138939, 0.6491304154179919905, 0.6561861808029703091, 0.6632419461879484057, 0.6702977115729266133, 0.6773534769579047099, 0.6844092423428829175, 0.6914650077278612361, 0.6985207731128393327, 0.7055765384978174293, 0.7126323038827955259, 0.7196880692677738445, 0.7267438346527520521, 0.7337996000377301486, 0.7408553654227082452, 0.7479111308076865638, 0.7549668961926647714, 0.7620226615776428680, 0.7690784269626210756, 0.7761341923475991722, 0.7831899577325773798, 0.7902457231175555874, 0.7973014885025337950, 0.8043572538875118916, 0.8114130192724900992, 0.8184687846574681958, 0.8255245500424465144, 0.8325803154274246110, 0.8396360808124027075, 0.8466918461973809151, 0.8537476115823591227, 0.8608033769673373303, 0.8678591423523154269, 0.8749149077372937455, 0.8819706731222718421, 0.8890264385072500497, 0.8960822038922281463, 0.9031379692772063539, 0.9101937346621845615, 0.9172495000471626581, 0.9243052654321408657, 0.9313610308171190733, 0.9384167962020972809, 0.9454725615870753774, 0.9525283269720535850, 0.9595840923570317926, 0.9666398577420098892, 0.9736956231269880968, 0.9807513885119663044, 0.9878071538969444010, 0.9900635123082154321 ),
 .UNSPECIFIED. ) 
 CURVE ( )  GEOMETRIC_REPRESENTATION_ITEM ( )  RATIONAL_B_SPLINE_CURVE ( ( 1.000000000000000000, 0.8660254037844387076, 1.000000000000000000, 0.8660254037844387076, 1.000000000000000000, 0.8660254037844387076, 1.000000000000000000, 0.8660254037844387076, 1.000000000000000000, 0.8660254037844387076, 1.000000000000000000, 0.8660254037844387076, 1.000000000000000000, 0.8660254037844387076, 1.000000000000000000, 0.8660254037844387076, 1.000000000000000000, 0.8660254037844387076, 1.000000000000000000, 0.8660254037844387076, 1.000000000000000000, 0.8660254037844387076, 1.000000000000000000, 0.8660254037844387076, 1.000000000000000000, 0.8660254037844387076, 1.000000000000000000, 0.8660254037844387076, 1.000000000000000000, 0.8660254037844387076, 1.000000000000000000, 0.8660254037844387076, 1.000000000000000000, 0.8660254037844387076, 1.000000000000000000, 0.8660254037844387076, 1.000000000000000000, 0.8660254037844387076, 1.000000000000000000, 0.8660254037844387076, 1.000000000000000000, 0.8660254037844387076, 1.000000000000000000, 0.8660254037844387076, 1.000000000000000000, 0.8660254037844387076, 1.000000000000000000, 0.8660254037844387076, 1.000000000000000000, 0.8660254037844387076, 1.000000000000000000, 0.8660254037844387076, 1.000000000000000000, 0.8660254037844387076, 1.000000000000000000, 0.8660254037844387076, 1.000000000000000000, 0.8660254037844387076, 1.000000000000000000, 0.8660254037844387076, 1.000000000000000000, 0.8660254037844387076, 1.000000000000000000, 0.8660254037844387076, 1.000000000000000000, 0.8660254037844387076, 1.000000000000000000, 0.8660254037844387076, 1.000000000000000000, 0.8660254037844387076, 1.000000000000000000, 0.8660254037844387076, 1.000000000000000000, 0.8660254037844387076, 1.000000000000000000, 0.8660254037844387076, 1.000000000000000000, 0.8660254037844387076, 1.000000000000000000, 0.8660254037844387076, 1.000000000000000000, 0.8660254037844387076, 1.000000000000000000, 0.8660254037844387076, 1.000000000000000000, 0.8660254037844387076, 1.000000000000000000, 0.8660254037844387076, 1.000000000000000000, 0.8660254037844387076, 1.000000000000000000, 0.8660254037844387076, 1.000000000000000000, 0.8660254037844387076, 1.000000000000000000, 0.8660254037844387076, 1.000000000000000000, 0.8660254037844387076, 1.000000000000000000, 0.8660254037844387076, 1.000000000000000000, 0.8660254037844387076, 1.000000000000000000, 0.8660254037844387076, 1.000000000000000000, 0.8660254037844387076, 1.000000000000000000, 0.8660254037844387076, 1.000000000000000000, 0.8660254037844387076, 1.000000000000000000, 0.8660254037844387076, 1.000000000000000000, 0.8660254037844387076, 1.000000000000000000, 0.8660254037844387076, 1.000000000000000000, 0.8660254037844387076, 1.000000000000000000, 0.8660254037844387076, 1.000000000000000000, 0.8660254037844387076, 1.000000000000000000, 0.8660254037844387076, 1.000000000000000000, 0.8660254037844387076, 1.000000000000000000, 0.8660254037844387076, 1.000000000000000000, 0.8660254037844387076, 1.000000000000000000, 0.8660254037844387076, 1.000000000000000000, 0.8660254037844387076, 1.000000000000000000, 0.8660254037844387076, 1.000000000000000000, 0.8660254037844387076, 1.000000000000000000, 0.8660254037844387076, 1.000000000000000000, 0.8660254037844387076, 1.000000000000000000, 0.8660254037844387076, 1.000000000000000000, 0.8660254037844387076, 1.000000000000000000, 0.8660254037844387076, 1.000000000000000000, 0.8660254037844387076, 1.000000000000000000, 0.8660254037844387076, 1.000000000000000000, 0.8660254037844387076, 1.000000000000000000, 0.8660254037844387076, 1.000000000000000000, 0.8660254037844387076, 1.000000000000000000, 0.8660254037844387076, 1.000000000000000000, 0.8660254037844387076, 1.000000000000000000, 0.8660254037844387076, 1.000000000000000000, 0.8660254037844387076, 1.000000000000000000, 0.8660254037844387076, 1.000000000000000000, 0.8660254037844387076, 1.000000000000000000, 0.8660254037844387076, 1.000000000000000000, 0.8660254037844387076, 1.000000000000000000, 0.8660254037844387076, 1.000000000000000000, 0.8660254037844387076, 1.000000000000000000, 0.8660254037844387076, 1.000000000000000000, 0.8660254037844387076, 1.000000000000000000, 0.8660254037844387076, 1.000000000000000000, 0.8660254037844387076, 1.000000000000000000, 0.8660254037844387076, 1.000000000000000000, 0.8660254037844387076, 1.000000000000000000, 0.8660254037844387076, 1.000000000000000000, 0.8660254037844387076, 1.000000000000000000, 0.8660254037844387076, 1.000000000000000000, 0.8660254037844387076, 1.000000000000000000, 0.8660254037844387076, 1.000000000000000000, 0.8660254037844387076, 1.000000000000000000, 0.8660254037844387076, 1.000000000000000000, 0.8660254037844387076, 1.000000000000000000, 0.8660254037844387076, 1.000000000000000000, 0.8660254037844387076, 1.000000000000000000, 0.8660254037844387076, 1.000000000000000000, 0.8660254037844387076, 1.000000000000000000, 0.8660254037844387076, 1.000000000000000000, 0.8660254037844387076, 1.000000000000000000, 0.8660254037844387076, 1.000000000000000000, 0.8660254037844387076, 1.000000000000000000, 0.8660254037844387076, 1.000000000000000000, 0.8660254037844387076, 1.000000000000000000, 0.8660254037844387076, 1.000000000000000000, 0.8660254037844387076, 1.000000000000000000, 0.8660254037844387076, 1.000000000000000000, 0.8660254037844387076, 1.000000000000000000, 0.8660254037844387076, 1.000000000000000000, 0.8660254037844387076, 1.000000000000000000, 0.8660254037844387076, 1.000000000000000000, 0.8660254037844387076, 1.000000000000000000, 0.8660254037844387076, 1.000000000000000000, 0.8660254037844387076, 1.000000000000000000, 0.8660254037844387076, 1.000000000000000000, 0.8660254037844387076, 1.000000000000000000, 0.8660254037844387076, 1.000000000000000000, 0.8660254037844387076, 1.000000000000000000, 0.8660254037844387076, 1.000000000000000000, 0.8660254037844387076, 1.000000000000000000, 0.8660254037844387076, 1.000000000000000000, 0.8660254037844387076, 1.000000000000000000, 0.8660254037844387076, 1.000000000000000000, 0.8660254037844387076, 1.000000000000000000, 0.8660254037844387076, 1.000000000000000000, 0.8660254037844387076, 1.000000000000000000, 0.8660254037844387076, 1.000000000000000000, 0.8660254037844387076, 1.000000000000000000, 0.8660254037844387076, 1.000000000000000000, 0.8660254037844387076, 1.000000000000000000, 0.8660254037844387076, 1.000000000000000000, 0.9571563550410552290, 0.9417145902178747363 ) ) 
 REPRESENTATION_ITEM ( '' )  );
#13641 = CIRCLE ( 'NONE', #55668, 82.00000000000000000 ) ;
#13642 = DIRECTION ( 'NONE',  ( -0.000000000000000000, 0.1045284632676437703, -0.9945218953682742891 ) ) ;
#13643 = PRODUCT_RELATED_PRODUCT_CATEGORY ( 'part', '', ( #49976 ) ) ;
#13644 = ADVANCED_FACE ( 'NONE', ( #30955 ), #8781, .F. ) ;
#13645 = CARTESIAN_POINT ( 'NONE',  ( -92.69370383062498320, -211.3315407142195852, 76.09614583420048461 ) ) ;
#13646 = DIRECTION ( 'NONE',  ( -1.000000000000000000, -0.000000000000000000, 0.000000000000000000 ) ) ;
#13647 = EDGE_LOOP ( 'NONE', ( #8618, #56121, #21425, #24502 ) ) ;
#13648 = FACE_OUTER_BOUND ( 'NONE', #6912, .T. ) ;
#13649 = FACE_OUTER_BOUND ( 'NONE', #26360, .T. ) ;
#13650 = CARTESIAN_POINT ( 'NONE',  ( 10.00000000000000000, 31.52238457039599595, 27.75498641678753842 ) ) ;
#13651 = EDGE_CURVE ( 'NONE', #51512, #30764, #2454, .T. ) ;
#13652 = DIRECTION ( 'NONE',  ( -1.000000000000000000, 0.000000000000000000, 0.000000000000000000 ) ) ;
#13653 = CARTESIAN_POINT ( 'NONE',  ( 97.30629616937498838, -211.3315407142195852, 75.30239583420048177 ) ) ;
#13654 = ORIENTED_EDGE ( 'NONE', *, *, #51533, .T. ) ;
#13655 = ADVANCED_FACE ( 'NONE', ( #25336 ), #59930, .T. ) ;
#13656 = CARTESIAN_POINT ( 'NONE',  ( 92.34999999999999432, 90.00000000000002842, 86.90437500173429441 ) ) ;
#13657 = CARTESIAN_POINT ( 'NONE',  ( 0.000000000000000000, 34.94270380257741238, -74.18225833017852722 ) ) ;
#13658 = CARTESIAN_POINT ( 'NONE',  ( 5.000000000000000000, 26.79245525562714292, 32.34446384429980981 ) ) ;
#13659 = ORIENTED_EDGE ( 'NONE', *, *, #38596, .F. ) ;
#13660 = EDGE_CURVE ( 'NONE', #10255, #17228, #57561, .T. ) ;
#13661 = CARTESIAN_POINT ( 'NONE',  ( 32.50000000000000000, -120.0000000000000000, -2.500000000000000000 ) ) ;
#13662 = ORIENTED_EDGE ( 'NONE', *, *, #7664, .F. ) ;
#13663 = AXIS2_PLACEMENT_3D ( 'NONE', #35980, #29584, #19058 ) ;
#13664 = CARTESIAN_POINT ( 'NONE',  ( 11.99999999999999822, 14.67089635893713684, 73.72996012237443608 ) ) ;
#13665 = ORIENTED_EDGE ( 'NONE', *, *, #26968, .F. ) ;
#13666 = ORIENTED_EDGE ( 'NONE', *, *, #22417, .F. ) ;
#13667 = ORIENTED_EDGE ( 'NONE', *, *, #51726, .F. ) ;
#13668 = CARTESIAN_POINT ( 'NONE',  ( 95.00000000000000000, -206.9400435732949575, 76.58562500173430010 ) ) ;
#13669 = EDGE_CURVE ( 'NONE', #57350, #63128, #37731, .T. ) ;
#13670 = EDGE_CURVE ( 'NONE', #35666, #68796, #45551, .T. ) ;
#13671 = VERTEX_POINT ( 'NONE', #48632 ) ;
#13672 = VECTOR ( 'NONE', #53089, 1000.000000000000000 ) ;
#13673 = ORIENTED_EDGE ( 'NONE', *, *, #20403, .F. ) ;
#13674 = CARTESIAN_POINT ( 'NONE',  ( 96.15314808468748708, 88.00268892867053694, 78.58322916753382970 ) ) ;
#13675 = CARTESIAN_POINT ( 'NONE',  ( 92.35003969675446456, -211.5300011322842977, 88.86229325377448163 ) ) ;
#13676 = CARTESIAN_POINT ( 'NONE',  ( 10.00000000000000000, 0.000000000000000000, 0.000000000000000000 ) ) ;
#13677 = VERTEX_POINT ( 'NONE', #9140 ) ;
#13678 = ORIENTED_EDGE ( 'NONE', *, *, #61789, .F. ) ;
#13679 = VERTEX_POINT ( 'NONE', #32066 ) ;
#13680 = DIRECTION ( 'NONE',  ( -1.000000000000000000, 0.000000000000000000, -0.000000000000000000 ) ) ;
#13681 = VERTEX_POINT ( 'NONE', #64825 ) ;
#13682 = DIRECTION ( 'NONE',  ( 0.9599519036180297338, 0.2801648492229545928, -5.514559048157468323E-17 ) ) ;
#13683 = DIRECTION ( 'NONE',  ( 0.000000000000000000, 0.000000000000000000, 1.000000000000000000 ) ) ;
#13684 = CARTESIAN_POINT ( 'NONE',  ( 5.000000000000000000, 3.925862922256160736, 41.81611651403863306 ) ) ;
#13685 = CARTESIAN_POINT ( 'NONE',  ( 92.34999999999999432, 91.52997821335252127, 77.96145833506763267 ) ) ;
#13686 = CARTESIAN_POINT ( 'NONE',  ( 11.99999999999999822, 30.41916302227114599, 71.27951684758035356 ) ) ;
#13687 = DIRECTION ( 'NONE',  ( 1.000000000000000000, 0.000000000000000000, 0.000000000000000000 ) ) ;
#13688 = CYLINDRICAL_SURFACE ( 'NONE', #41663, 16.00000000000000000 ) ;
#13689 = CARTESIAN_POINT ( 'NONE',  ( -97.64999999999996305, -209.9999999999999716, 74.83937500173429669 ) ) ;
#13690 = CARTESIAN_POINT ( 'NONE',  ( -95.00000000000002842, 92.66308142843932671, 88.37281250086715545 ) ) ;
#13692 = CARTESIAN_POINT ( 'NONE',  ( -92.35000000000003695, 90.00000000000004263, 77.06187500173429328 ) ) ;
#13691 = CARTESIAN_POINT ( 'NONE',  ( 96.32499999999998863, 87.70503267997126784, 76.32104166840096582 ) ) ;
#13693 = AXIS2_PLACEMENT_3D ( 'NONE', #34487, #5945, #51785 ) ;
#13694 = ORIENTED_EDGE ( 'NONE', *, *, #10868, .F. ) ;
#13695 = CARTESIAN_POINT ( 'NONE',  ( 96.15314808468748708, 88.00268892867053694, 75.40822916753381833 ) ) ;
#13696 = AXIS2_PLACEMENT_3D ( 'NONE', #4713, #62209, #34364 ) ;
#13697 = CARTESIAN_POINT ( 'NONE',  ( -10.00000000000000000, 0.000000000000000000, 0.000000000000000000 ) ) ;
#13698 = CARTESIAN_POINT ( 'NONE',  ( 0.000000000000000000, 80.00000000000000000, -90.00000000000000000 ) ) ;
#13699 = CYLINDRICAL_SURFACE ( 'NONE', #43242, 2.649999999999985700 ) ;
#13700 = FACE_OUTER_BOUND ( 'NONE', #1343, .T. ) ;
#13701 = CARTESIAN_POINT ( 'NONE',  ( 10.00000000000000000, -68.27212725128254078, -31.46837873495049465 ) ) ;
#13702 = EDGE_LOOP ( 'NONE', ( #6734, #10999, #15978, #68990 ) ) ;
#13704 = CARTESIAN_POINT ( 'NONE',  ( -0.8815729230226008184, -93.47222532549339746, 5.500000000000000000 ) ) ;
#13703 = AXIS2_PLACEMENT_3D ( 'NONE', #35468, #69312, #34353 ) ;
#13705 = CIRCLE ( 'NONE', #30551, 37.49900000000000944 ) ;
#13706 = DIRECTION ( 'NONE',  ( -0.000000000000000000, 6.938893903907229364E-16, 1.000000000000000000 ) ) ;
#13707 = EDGE_LOOP ( 'NONE', ( #46436, #37742, #68291, #35110 ) ) ;
#13708 = ORIENTED_EDGE ( 'NONE', *, *, #18464, .T. ) ;
#13709 = DIRECTION ( 'NONE',  ( -1.000000000000000000, -0.000000000000000000, 0.000000000000000000 ) ) ;
#13710 = DIRECTION ( 'NONE',  ( 0.000000000000000000, 0.3826834323650841752, 0.9238795325112891810 ) ) ;
#13711 = FACE_OUTER_BOUND ( 'NONE', #1436, .T. ) ;
#13712 = AXIS2_PLACEMENT_3D ( 'NONE', #4308, #22318, #61810 ) ;
#13713 = DIRECTION ( 'NONE',  ( 0.000000000000000000, 0.2334453638558990907, 0.9723699203976781114 ) ) ;
#13714 = DIRECTION ( 'NONE',  ( 0.000000000000000000, 0.6691306063588675634, -0.7431448254773856954 ) ) ;
#13715 = CARTESIAN_POINT ( 'NONE',  ( 12.00000000000000000, 14.60985201121703980, -18.46759930825707841 ) ) ;
#13716 = ORIENTED_EDGE ( 'NONE', *, *, #24856, .F. ) ;
#13717 = EDGE_CURVE ( 'NONE', #39802, #41314, #42624, .T. ) ;
#13718 = AXIS2_PLACEMENT_3D ( 'NONE', #24516, #47452, #70356 ) ;
#13719 = CYLINDRICAL_SURFACE ( 'NONE', #22357, 82.00000000000000000 ) ;
#13720 = CARTESIAN_POINT ( 'NONE',  ( 10.00000000000000000, 62.50329211542494789, -41.76937507738723099 ) ) ;
#13721 = DIRECTION ( 'NONE',  ( 0.000000000000000000, 0.000000000000000000, -1.000000000000000000 ) ) ;
#13722 = DIRECTION ( 'NONE',  ( 0.000000000000000000, 0.000000000000000000, 1.000000000000000000 ) ) ;
#13723 = DIRECTION ( 'NONE',  ( -0.000000000000000000, -0.000000000000000000, 1.000000000000000000 ) ) ;
#13724 = CARTESIAN_POINT ( 'NONE',  ( 0.000000000000000000, -26.08949754953044220, 27.05870788708222818 ) ) ;
#13725 = EDGE_CURVE ( 'NONE', #69920, #63641, #22730, .T. ) ;
#13726 = DIRECTION ( 'NONE',  ( 0.5200609990133008287, 0.8541291221503266584, -0.000000000000000000 ) ) ;
#13727 = DIRECTION ( 'NONE',  ( -1.000000000000000000, 0.000000000000000000, 0.000000000000000000 ) ) ;
#13728 = EDGE_CURVE ( 'NONE', #60757, #428, #38251, .T. ) ;
#13729 = DIRECTION ( 'NONE',  ( 0.000000000000000000, 0.000000000000000000, -1.000000000000000000 ) ) ;
#13730 = VECTOR ( 'NONE', #16785, 1000.000000000000000 ) ;
#13731 = CARTESIAN_POINT ( 'NONE',  ( 96.15314808468748708, 91.99731107132950569, 82.60489583420049087 ) ) ;
#13732 = ADVANCED_FACE ( 'NONE', ( #11002 ), #5011, .T. ) ;
#13733 = CARTESIAN_POINT ( 'NONE',  ( -97.30629616937497417, -208.6684592857803295, 87.20864583420048177 ) ) ;
#13734 = CARTESIAN_POINT ( 'NONE',  ( 32.50000000000000000, -120.0000000000000000, -2.500000000000000000 ) ) ;
#13735 = ORIENTED_EDGE ( 'NONE', *, *, #30918, .T. ) ;
#13736 = CARTESIAN_POINT ( 'NONE',  ( -97.64999999999996305, -209.9999999999999716, 81.10999999999999943 ) ) ;
#13737 = CARTESIAN_POINT ( 'NONE',  ( -97.64999999999994884, -208.4700217866474645, 80.42208333333331893 ) ) ;
#13738 = CARTESIAN_POINT ( 'NONE',  ( -92.69370383062504004, 90.00000000000004263, 75.35531250086714294 ) ) ;
#13739 = AXIS2_PLACEMENT_3D ( 'NONE', #70622, #59367, #46607 ) ;
#13740 = CARTESIAN_POINT ( 'NONE',  ( 97.30629616937498838, -208.6684592857803011, 86.20322916753382003 ) ) ;
#13741 = ORIENTED_EDGE ( 'NONE', *, *, #17675, .T. ) ;
#13742 = FACE_OUTER_BOUND ( 'NONE', #19885, .T. ) ;
#13743 = ORIENTED_EDGE ( 'NONE', *, *, #24362, .T. ) ;
#13744 = VECTOR ( 'NONE', #26036, 1000.000000000000114 ) ;
#13745 = ADVANCED_FACE ( 'NONE', ( #20794 ), #15147, .T. ) ;
#13746 = ORIENTED_EDGE ( 'NONE', *, *, #2671, .T. ) ;
#13747 = CARTESIAN_POINT ( 'NONE',  ( -92.35000000000003695, 90.00000015433754186, 79.60187500750917877 ) ) ;
#13748 = VECTOR ( 'NONE', #45302, 1000.000000000000000 ) ;
#13749 = DIRECTION ( 'NONE',  ( -1.000000000000000000, -0.000000000000000000, 0.000000000000000000 ) ) ;
#13750 = ORIENTED_EDGE ( 'NONE', *, *, #45768, .F. ) ;
#13751 = VECTOR ( 'NONE', #55337, 999.9999999999998863 ) ;
#13752 = CARTESIAN_POINT ( 'NONE',  ( 2.874421927457452952, -143.3717286177755739, 5.500000000000000000 ) ) ;
#13753 = CARTESIAN_POINT ( 'NONE',  ( 97.30629616937498838, -211.3315407142195852, 79.27114583420048177 ) ) ;
#13754 = EDGE_CURVE ( 'NONE', #73125, #32561, #20340, .T. ) ;
#13755 = DIRECTION ( 'NONE',  ( -1.000000000000000000, 0.000000000000000000, 0.000000000000000000 ) ) ;
#13756 = EDGE_CURVE ( 'NONE', #70963, #23395, #65991, .T. ) ;
#13758 = CARTESIAN_POINT ( 'NONE',  ( -95.00000000000002842, 90.00000000000004263, 90.00000000000000000 ) ) ;
#13757 = CIRCLE ( 'NONE', #55801, 21.00000000000000000 ) ;
#13759 = DIRECTION ( 'NONE',  ( -1.000000000000000000, 0.000000000000000000, -0.000000000000000000 ) ) ;
#13760 = LINE ( 'NONE', #54732, #50688 ) ;
#13761 = EDGE_CURVE ( 'NONE', #39587, #44855, #69570, .T. ) ;
#13762 = DIRECTION ( 'NONE',  ( 0.000000000000000000, 0.000000000000000000, 1.000000000000000000 ) ) ;
#13763 = CARTESIAN_POINT ( 'NONE',  ( 96.32499999999998863, -212.2949673200287179, 81.95666666666666345 ) ) ;
#13764 = ORIENTED_EDGE ( 'NONE', *, *, #6940, .F. ) ;
#13765 = ORIENTED_EDGE ( 'NONE', *, *, #13669, .F. ) ;
#13766 = ORIENTED_EDGE ( 'NONE', *, *, #8450, .T. ) ;
#13767 = ORIENTED_EDGE ( 'NONE', *, *, #38528, .F. ) ;
#13768 = CARTESIAN_POINT ( 'NONE',  ( -1.250000000000000444, -16.78109714094927085, 0.000000000000000000 ) ) ;
#13769 = CARTESIAN_POINT ( 'NONE',  ( -96.15314808468751551, 88.00268892867056536, 84.19239583420049655 ) ) ;
#13770 = CARTESIAN_POINT ( 'NONE',  ( 5.000000000000002665, 81.50828551894227303, 8.966570791700979370 ) ) ;
#13771 = LINE ( 'NONE', #30688, #64254 ) ;
#13772 =( BOUNDED_CURVE ( )  B_SPLINE_CURVE ( 2, ( #5531, #74303, #45755, #16421, #68303, #16798, #39735 ),
 .UNSPECIFIED., .F., .F. ) 
 B_SPLINE_CURVE_WITH_KNOTS ( ( 3, 2, 2, 3 ),
 ( 0.7083333333333331483, 0.7152777777777775681, 0.7222222222222220989, 0.7291666666666665186 ),
 .UNSPECIFIED. ) 
 CURVE ( )  GEOMETRIC_REPRESENTATION_ITEM ( )  RATIONAL_B_SPLINE_CURVE ( ( 1.000000000000004219, 0.8660254037844343777, 1.000000000000000000, 0.8660254037844387076, 1.000000000000000000, 0.8660254037844408170, 0.9999999999999978906 ) ) 
 REPRESENTATION_ITEM ( '' )  );
#13773 = CARTESIAN_POINT ( 'NONE',  ( 94.99999999999998579, 86.94004357329500010, 75.55375000000000796 ) ) ;
#13774 = VERTEX_POINT ( 'NONE', #32802 ) ;
#13775 = CARTESIAN_POINT ( 'NONE',  ( 94.99999999999998579, 93.05995642670504253, 79.68124999999999147 ) ) ;
#13776 = EDGE_LOOP ( 'NONE', ( #14176, #35760, #5499, #20793 ) ) ;
#13777 = CYLINDRICAL_SURFACE ( 'NONE', #47054, 31.99999999999999289 ) ;
#13778 = ORIENTED_EDGE ( 'NONE', *, *, #15692, .T. ) ;
#13779 = CARTESIAN_POINT ( 'NONE',  ( -93.67500000000003979, 87.70503267997129626, 85.84604166840097150 ) ) ;
#13780 = CARTESIAN_POINT ( 'NONE',  ( 92.69370383062498320, 90.00000000000002842, 85.35656250086715602 ) ) ;
#13781 = CARTESIAN_POINT ( 'NONE',  ( 0.000000000000000000, 0.000000000000000000, -270.0000000000000000 ) ) ;
#13782 = CARTESIAN_POINT ( 'NONE',  ( -16.06301359042743115, -102.7814171781257357, 5.500000000000000000 ) ) ;
#13783 = CARTESIAN_POINT ( 'NONE',  ( -94.99999999999997158, -206.9400435732949575, 78.49062500173430124 ) ) ;
#13784 = CARTESIAN_POINT ( 'NONE',  ( 0.000000000000000000, 74.18225833017937987, -34.94270380257560049 ) ) ;
#13785 = ORIENTED_EDGE ( 'NONE', *, *, #62650, .F. ) ;
#13786 = DIRECTION ( 'NONE',  ( -1.000000000000000000, 0.000000000000000000, 0.000000000000000000 ) ) ;
#13787 = CARTESIAN_POINT ( 'NONE',  ( -0.9515373497862389396, -96.47140937769621871, 2.500000000000000000 ) ) ;
#13788 = VECTOR ( 'NONE', #15998, 1000.000000000000000 ) ;
#13789 = ORIENTED_EDGE ( 'NONE', *, *, #32218, .F. ) ;
#13790 = ORIENTED_EDGE ( 'NONE', *, *, #29617, .F. ) ;
#13791 = FACE_OUTER_BOUND ( 'NONE', #37463, .T. ) ;
#13792 = CYLINDRICAL_SURFACE ( 'NONE', #31202, 16.00000000000000000 ) ;
#13793 = CARTESIAN_POINT ( 'NONE',  ( -96.32500000000001705, 92.29496732002878900, 75.36854166840096525 ) ) ;
#13794 = CARTESIAN_POINT ( 'NONE',  ( -92.69370383062498320, -208.6684592857803011, 83.18697916753382060 ) ) ;
#13795 = ORIENTED_EDGE ( 'NONE', *, *, #51192, .T. ) ;
#13796 = AXIS2_PLACEMENT_3D ( 'NONE', #45113, #68037, #66911 ) ;
#13797 = DIRECTION ( 'NONE',  ( -1.000000000000000000, -0.000000000000000000, -0.000000000000000000 ) ) ;
#13798 = ORIENTED_EDGE ( 'NONE', *, *, #62661, .F. ) ;
#13799 = ADVANCED_FACE ( 'NONE', ( #21152 ), #39209, .T. ) ;
#13800 = ORIENTED_EDGE ( 'NONE', *, *, #47609, .F. ) ;
#13801 = DIRECTION ( 'NONE',  ( 0.000000000000000000, 0.000000000000000000, 1.000000000000000000 ) ) ;
#13802 = CARTESIAN_POINT ( 'NONE',  ( 97.30629616937498838, 90.00000000000002842, 89.48406250086715374 ) ) ;
#13803 = SURFACE_STYLE_FILL_AREA ( #1477 ) ;
#13804 = CARTESIAN_POINT ( 'NONE',  ( 96.15314808468748708, 88.00268892867053694, 80.32947916753380468 ) ) ;
#13805 = DIRECTION ( 'NONE',  ( 0.000000000000000000, 0.8910065241883688980, -0.4539904997395447506 ) ) ;
#13806 = CARTESIAN_POINT ( 'NONE',  ( 35.50000000000000711, -120.0000000000000000, -5.500000000000000000 ) ) ;
#13807 = ADVANCED_FACE ( 'NONE', ( #39579 ), #50844, .T. ) ;
#13808 = LINE ( 'NONE', #18347, #4879 ) ;
#13809 = DIRECTION ( 'NONE',  ( 0.000000000000000000, 0.000000000000000000, -1.000000000000000000 ) ) ;
#13810 = CARTESIAN_POINT ( 'NONE',  ( 11.99999999999999822, 41.19522573413733113, 65.64334221924924861 ) ) ;
#13811 = EDGE_CURVE ( 'NONE', #48459, #64733, #38087, .T. ) ;
#13812 = DIRECTION ( 'NONE',  ( -0.000000000000000000, -0.000000000000000000, -1.000000000000000000 ) ) ;
#13813 = CARTESIAN_POINT ( 'NONE',  ( -18.24502636017238899, -100.7225776329765665, -5.500000000000000000 ) ) ;
#13814 = VECTOR ( 'NONE', #10005, 1000.000000000000000 ) ;
#13815 = EDGE_CURVE ( 'NONE', #51420, #26020, #61402, .T. ) ;
#13816 = PLANE ( 'NONE',  #6122 ) ;
#13817 = VERTEX_POINT ( 'NONE', #38463 ) ;
#13818 = CARTESIAN_POINT ( 'NONE',  ( -95.00000000000002842, 87.33691857156074434, 86.62656250086713783 ) ) ;
#13819 = CARTESIAN_POINT ( 'NONE',  ( 97.64999999999999147, 90.00000000000002842, 79.52249999999999375 ) ) ;
#13820 = AXIS2_PLACEMENT_3D ( 'NONE', #57292, #17794, #29076 ) ;
#13821 = FACE_OUTER_BOUND ( 'NONE', #21044, .T. ) ;
#13822 = VECTOR ( 'NONE', #3328, 1000.000000000000000 ) ;
#13823 = ORIENTED_EDGE ( 'NONE', *, *, #4625, .F. ) ;
#13824 = CARTESIAN_POINT ( 'NONE',  ( -3.000000000000000000, 0.000000000000000000, -5.974599999999999689 ) ) ;
#13825 = CARTESIAN_POINT ( 'NONE',  ( 0.000000000000000000, -18.13022148937263012, 15.02647892043544608 ) ) ;
#13826 = EDGE_CURVE ( 'NONE', #22970, #72597, #50090, .T. ) ;
#13827 = FACE_OUTER_BOUND ( 'NONE', #32175, .T. ) ;
#13828 = AXIS2_PLACEMENT_3D ( 'NONE', #72315, #73420, #55772 ) ;
#13829 = CARTESIAN_POINT ( 'NONE',  ( 93.84685191531251292, -211.9973110713294489, 82.92239583420048632 ) ) ;
#13830 = ORIENTED_EDGE ( 'NONE', *, *, #829, .F. ) ;
#13831 = VERTEX_POINT ( 'NONE', #44100 ) ;
#13832 = EDGE_CURVE ( 'NONE', #32827, #54022, #50478, .T. ) ;
#13833 = LINE ( 'NONE', #66113, #22430 ) ;
#13834 = ORIENTED_EDGE ( 'NONE', *, *, #66190, .T. ) ;
#13835 = ADVANCED_FACE ( 'NONE', ( #68146 ), #56123, .F. ) ;
#13836 = CYLINDRICAL_SURFACE ( 'NONE', #31743, 31.99999999999998579 ) ;
#13837 = DIRECTION ( 'NONE',  ( 0.000000000000000000, -0.3090169943749548342, 0.9510565162951510887 ) ) ;
#13838 = VECTOR ( 'NONE', #27533, 1000.000000000000000 ) ;
#13839 = ORIENTED_EDGE ( 'NONE', *, *, #24140, .T. ) ;
#13840 = AXIS2_PLACEMENT_3D ( 'NONE', #69373, #40814, #6953 ) ;
#13841 = CARTESIAN_POINT ( 'NONE',  ( 95.00000000000000000, -207.3369185715606307, 80.11781250086714579 ) ) ;
#13842 = VERTEX_POINT ( 'NONE', #5383 ) ;
#13843 = CYLINDRICAL_SURFACE ( 'NONE', #25105, 31.99999999999999289 ) ;
#13844 = ORIENTED_EDGE ( 'NONE', *, *, #30619, .F. ) ;
#13845 = AXIS2_PLACEMENT_3D ( 'NONE', #10049, #14577, #38252 ) ;
#13846 = ORIENTED_EDGE ( 'NONE', *, *, #9395, .T. ) ;
#13847 = CARTESIAN_POINT ( 'NONE',  ( -14.87942725330654348, -141.9795960975983178, 5.500000000000000000 ) ) ;
#13848 = SURFACE_STYLE_FILL_AREA ( #72108 ) ;
#13849 = CYLINDRICAL_SURFACE ( 'NONE', #46076, 82.00000000000000000 ) ;
#13850 = ORIENTED_EDGE ( 'NONE', *, *, #7997, .F. ) ;
#13851 = FACE_OUTER_BOUND ( 'NONE', #3210, .T. ) ;
#13852 = CARTESIAN_POINT ( 'NONE',  ( 92.35000000000000853, -209.9999999999999716, 84.99937500173429328 ) ) ;
#13853 = CARTESIAN_POINT ( 'NONE',  ( 93.67499999999999716, 87.70503267997126784, 83.75583333333332803 ) ) ;
#13854 = VERTEX_POINT ( 'NONE', #33175 ) ;
#13855 = DIRECTION ( 'NONE',  ( -1.000000000000000000, -0.000000000000000000, -0.000000000000000000 ) ) ;
#13856 = DIRECTION ( 'NONE',  ( -1.000000000000000000, 0.000000000000000000, -0.000000000000000000 ) ) ;
#13857 = VERTEX_POINT ( 'NONE', #28279 ) ;
#13858 = VECTOR ( 'NONE', #8728, 1000.000000000000000 ) ;
#13859 = ORIENTED_EDGE ( 'NONE', *, *, #25612, .F. ) ;
#13860 =( BOUNDED_CURVE ( )  B_SPLINE_CURVE ( 2, ( #10610, #129, #10237, #45590, #62127, #22643, #17367, #34656, #74133, #63246, #51575, #44470, #34283, #57605, #16626, #6106, #11348, #33161, #68880, #27529, #17005, #33534, #21893, #4998, #57226, #62513, #67387, #27900, #56110, #39565, #39939, #29013, #73758, #5371, #4630, #51943, #491, #23023, #15886, #50462, #38820, #45956, #68513, #44839, #61759, #67767, #22272, #10991, #16253, #39191, #62890, #45210, #68130, #28266, #51202, #6821, #52688, #47420, #1964, #12092, #29734, #64350, #1237, #13200, #18830, #35031, #24131, #47062, #53792, #36130, #1600, #7568, #69240, #64717, #69964, #59080, #18467, #17731, #12822, #47781, #23742, #23388, #30844, #46313, #57963, #65092, #41409, #40678, #30116, #30483, #59444, #63981, #53428, #63622, #24486, #41051, #70326, #70701, #13564, #53065, #42159, #35750, #58701, #29373, #52315, #24850, #7930, #69610, #41772, #35400, #19209, #36494, #12458, #856, #58329, #6468, #7198, #46684, #18111, #65462, #48886, #8681, #2341, #19571, #44004, #9406, #37985, #20692, #14311, #9040, #32332, #25233, #55276, #26333, #71070, #2707, #9785, #3425, #60197, #66917, #21053, #72185, #3064, #25588, #26691, #31592, #49259, #42520, #15412, #25960, #59817, #36867, #54535, #15046, #42896, #3796, #31228, #48160, #20322, #8305, #61296, #48521, #60562, #38360, #32698, #43643, #31961, #54180, #66566, #49618, #19940, #43280, #13927, #71440, #60916, #71809, #65824, #37258, #72547, #66203, #14678, #37627, #54902, #40214, #45501, #57147, #68044, #38734, #56776, #44753, #11623, #45125, #39481, #56016, #68431, #44374, #10148, #16920, #11267, #67301, #21414, #27059, #16534, #5654, #4536, #72910, #67677, #16165, #28183, #51120, #27435, #4914, #15799, #28546, #61663, #62805, #33072, #62429, #10517, #62042, #55644, #51486, #22938, #10906, #47, #34200, #4162, #39858, #68800, #27814, #45879, #22554, #50372, #17281, #73293, #74044, #50743, #49992, #63167, #39104, #33829, #21806, #33444, #56407, #73666, #22182, #5285, #40963, #24043, #408, #53339, #19123, #13107, #1876, #17653, #47695, #42071, #40582, #52226, #58990, #58241, #35665, #18023, #24765, #70605, #58603, #7105, #6742, #773, #36044, #30029, #46967, #29648, #47333, #12737, #12370, #65002, #18746, #63530, #46593, #52972, #6025, #52589 ),
 .UNSPECIFIED., .F., .F. ) 
 B_SPLINE_CURVE_WITH_KNOTS ( ( 3, 2, 2, 2, 2, 2, 2, 2, 2, 2, 2, 2, 2, 2, 2, 2, 2, 2, 2, 2, 2, 2, 2, 2, 2, 2, 2, 2, 2, 2, 2, 2, 2, 2, 2, 2, 2, 2, 2, 2, 2, 2, 2, 2, 2, 2, 2, 2, 2, 2, 2, 2, 2, 2, 2, 2, 2, 2, 2, 2, 2, 2, 2, 2, 2, 2, 2, 2, 2, 2, 2, 2, 2, 2, 2, 2, 2, 2, 2, 2, 2, 2, 2, 2, 2, 2, 2, 2, 2, 2, 2, 2, 2, 2, 2, 2, 2, 2, 2, 2, 2, 2, 2, 2, 2, 2, 2, 2, 2, 2, 2, 2, 2, 2, 2, 2, 2, 2, 2, 2, 2, 2, 2, 2, 2, 2, 2, 2, 2, 2, 2, 2, 2, 2, 2, 2, 2, 2, 2, 2, 2, 3 ),
 ( 0.000000000000000000, 0.007055765384978174640, 0.01411153076995634928, 0.02116729615493452565, 0.02822306153991269856, 0.03527882692489087146, 0.04233459230986905131, 0.04939035769484722421, 0.05644612307982539712, 0.06350188846480357696, 0.07055765384978174293, 0.07761341923475992277, 0.08466918461973810262, 0.09172495000471626858, 0.09878071538969444843, 0.1058364807746726144, 0.1128922461596507942, 0.1199480115446289741, 0.1270037769296071539, 0.1340595423145853060, 0.1411153076995634859, 0.1481710730845416657, 0.1552268384695198455, 0.1622826038544980254, 0.1693383692394762052, 0.1763941346244543573, 0.1834499000094325372, 0.1905056653944107170, 0.1975614307793888969, 0.2046171961643670767, 0.2116729615493452288, 0.2187287269343234086, 0.2257844923193015885, 0.2328402577042797683, 0.2398960230892579482, 0.2469517884742361002, 0.2540075538592143078, 0.2610633192441924599, 0.2681190846291706120, 0.2751748500141488196, 0.2822306153991269717, 0.2892863807841051793, 0.2963421461690833314, 0.3033979115540614835, 0.3104536769390396911, 0.3175094423240178432, 0.3245652077089960508, 0.3316209730939742029, 0.3386767384789524105, 0.3457325038639305625, 0.3527882692489087146, 0.3598440346338869222, 0.3668998000188650743, 0.3739555654038432819, 0.3810113307888214340, 0.3880670961737995861, 0.3951228615587777937, 0.4021786269437559458, 0.4092343923287341534, 0.4162901577137123055, 0.4233459230986904576, 0.4304016884836686652, 0.4374574538686468173, 0.4445132192536250249, 0.4515689846386031769, 0.4586247500235813290, 0.4656805154085595366, 0.4727362807935376887, 0.4797920461785158963, 0.4868478115634940484, 0.4939035769484722005, 0.5009593423334504081, 0.5080151077184286157, 0.5150708731034067123, 0.5221266384883849199, 0.5291824038733631275, 0.5362381692583412240, 0.5432939346433194316, 0.5503497000282976392, 0.5574054654132758468, 0.5644612307982539434, 0.5715169961832320400, 0.5785727615682103586, 0.5856285269531884552, 0.5926842923381666628, 0.5997400577231448704, 0.6067958231081229670, 0.6138515884931011746, 0.6209073538780793822, 0.6279631192630575898, 0.6350188846480356863, 0.6420746500330137829, 0.6491304154179921015, 0.6561861808029703091, 0.6632419461879484057, 0.6702977115729265023, 0.6773534769579048209, 0.6844092423428830285, 0.6914650077278611251, 0.6985207731128393327, 0.7055765384978174293, 0.7126323038827956369, 0.7196880692677738445, 0.7267438346527520521, 0.7337996000377301486, 0.7408553654227082452, 0.7479111308076865638, 0.7549668961926647714, 0.7620226615776428680, 0.7690784269626209646, 0.7761341923475991722, 0.7831899577325774908, 0.7902457231175555874, 0.7973014885025336840, 0.8043572538875118916, 0.8114130192724900992, 0.8184687846574683068, 0.8255245500424464034, 0.8325803154274246110, 0.8396360808124027075, 0.8466918461973809151, 0.8537476115823592338, 0.8608033769673373303, 0.8678591423523154269, 0.8749149077372936345, 0.8819706731222718421, 0.8890264385072500497, 0.8960822038922281463, 0.9031379692772063539, 0.9101937346621845615, 0.9172495000471626581, 0.9243052654321408657, 0.9313610308171190733, 0.9384167962020972809, 0.9454725615870753774, 0.9525283269720535850, 0.9595840923570317926, 0.9666398577420098892, 0.9736956231269880968, 0.9807513885119663044, 0.9878071538969444010, 0.9900635123082155431 ),
 .UNSPECIFIED. ) 
 CURVE ( )  GEOMETRIC_REPRESENTATION_ITEM ( )  RATIONAL_B_SPLINE_CURVE ( ( 1.000000000000000000, 0.8660254037844387076, 1.000000000000000000, 0.8660254037844387076, 1.000000000000000000, 0.8660254037844387076, 1.000000000000000000, 0.8660254037844387076, 1.000000000000000000, 0.8660254037844387076, 1.000000000000000000, 0.8660254037844387076, 1.000000000000000000, 0.8660254037844387076, 1.000000000000000000, 0.8660254037844387076, 1.000000000000000000, 0.8660254037844387076, 1.000000000000000000, 0.8660254037844387076, 1.000000000000000000, 0.8660254037844387076, 1.000000000000000000, 0.8660254037844387076, 1.000000000000000000, 0.8660254037844387076, 1.000000000000000000, 0.8660254037844387076, 1.000000000000000000, 0.8660254037844387076, 1.000000000000000000, 0.8660254037844387076, 1.000000000000000000, 0.8660254037844387076, 1.000000000000000000, 0.8660254037844387076, 1.000000000000000000, 0.8660254037844387076, 1.000000000000000000, 0.8660254037844387076, 1.000000000000000000, 0.8660254037844387076, 1.000000000000000000, 0.8660254037844387076, 1.000000000000000000, 0.8660254037844387076, 1.000000000000000000, 0.8660254037844387076, 1.000000000000000000, 0.8660254037844387076, 1.000000000000000000, 0.8660254037844387076, 1.000000000000000000, 0.8660254037844387076, 1.000000000000000000, 0.8660254037844387076, 1.000000000000000000, 0.8660254037844387076, 1.000000000000000000, 0.8660254037844387076, 1.000000000000000000, 0.8660254037844387076, 1.000000000000000000, 0.8660254037844387076, 1.000000000000000000, 0.8660254037844387076, 1.000000000000000000, 0.8660254037844387076, 1.000000000000000000, 0.8660254037844387076, 1.000000000000000000, 0.8660254037844387076, 1.000000000000000000, 0.8660254037844387076, 1.000000000000000000, 0.8660254037844387076, 1.000000000000000000, 0.8660254037844387076, 1.000000000000000000, 0.8660254037844387076, 1.000000000000000000, 0.8660254037844387076, 1.000000000000000000, 0.8660254037844387076, 1.000000000000000000, 0.8660254037844387076, 1.000000000000000000, 0.8660254037844387076, 1.000000000000000000, 0.8660254037844387076, 1.000000000000000000, 0.8660254037844387076, 1.000000000000000000, 0.8660254037844387076, 1.000000000000000000, 0.8660254037844387076, 1.000000000000000000, 0.8660254037844387076, 1.000000000000000000, 0.8660254037844387076, 1.000000000000000000, 0.8660254037844387076, 1.000000000000000000, 0.8660254037844387076, 1.000000000000000000, 0.8660254037844387076, 1.000000000000000000, 0.8660254037844387076, 1.000000000000000000, 0.8660254037844387076, 1.000000000000000000, 0.8660254037844387076, 1.000000000000000000, 0.8660254037844387076, 1.000000000000000000, 0.8660254037844387076, 1.000000000000000000, 0.8660254037844387076, 1.000000000000000000, 0.8660254037844387076, 1.000000000000000000, 0.8660254037844387076, 1.000000000000000000, 0.8660254037844387076, 1.000000000000000000, 0.8660254037844387076, 1.000000000000000000, 0.8660254037844387076, 1.000000000000000000, 0.8660254037844387076, 1.000000000000000000, 0.8660254037844387076, 1.000000000000000000, 0.8660254037844387076, 1.000000000000000000, 0.8660254037844387076, 1.000000000000000000, 0.8660254037844387076, 1.000000000000000000, 0.8660254037844387076, 1.000000000000000000, 0.8660254037844387076, 1.000000000000000000, 0.8660254037844387076, 1.000000000000000000, 0.8660254037844387076, 1.000000000000000000, 0.8660254037844387076, 1.000000000000000000, 0.8660254037844387076, 1.000000000000000000, 0.8660254037844387076, 1.000000000000000000, 0.8660254037844387076, 1.000000000000000000, 0.8660254037844387076, 1.000000000000000000, 0.8660254037844387076, 1.000000000000000000, 0.8660254037844387076, 1.000000000000000000, 0.8660254037844387076, 1.000000000000000000, 0.8660254037844387076, 1.000000000000000000, 0.8660254037844387076, 1.000000000000000000, 0.8660254037844387076, 1.000000000000000000, 0.8660254037844387076, 1.000000000000000000, 0.8660254037844387076, 1.000000000000000000, 0.8660254037844387076, 1.000000000000000000, 0.8660254037844387076, 1.000000000000000000, 0.8660254037844387076, 1.000000000000000000, 0.8660254037844387076, 1.000000000000000000, 0.8660254037844387076, 1.000000000000000000, 0.8660254037844387076, 1.000000000000000000, 0.8660254037844387076, 1.000000000000000000, 0.8660254037844387076, 1.000000000000000000, 0.8660254037844387076, 1.000000000000000000, 0.8660254037844387076, 1.000000000000000000, 0.8660254037844387076, 1.000000000000000000, 0.8660254037844387076, 1.000000000000000000, 0.8660254037844387076, 1.000000000000000000, 0.8660254037844387076, 1.000000000000000000, 0.8660254037844387076, 1.000000000000000000, 0.8660254037844387076, 1.000000000000000000, 0.8660254037844387076, 1.000000000000000000, 0.8660254037844387076, 1.000000000000000000, 0.8660254037844387076, 1.000000000000000000, 0.8660254037844387076, 1.000000000000000000, 0.8660254037844387076, 1.000000000000000000, 0.8660254037844387076, 1.000000000000000000, 0.8660254037844387076, 1.000000000000000000, 0.8660254037844387076, 1.000000000000000000, 0.8660254037844387076, 1.000000000000000000, 0.8660254037844387076, 1.000000000000000000, 0.8660254037844387076, 1.000000000000000000, 0.8660254037844387076, 1.000000000000000000, 0.8660254037844387076, 1.000000000000000000, 0.8660254037844387076, 1.000000000000000000, 0.8660254037844387076, 1.000000000000000000, 0.8660254037844387076, 1.000000000000000000, 0.8660254037844387076, 1.000000000000000000, 0.8660254037844387076, 1.000000000000000000, 0.8660254037844387076, 1.000000000000000000, 0.8660254037844387076, 1.000000000000000000, 0.8660254037844387076, 1.000000000000000000, 0.8660254037844387076, 1.000000000000000000, 0.8660254037844387076, 1.000000000000000000, 0.8660254037844387076, 1.000000000000000000, 0.8660254037844387076, 1.000000000000000000, 0.8660254037844387076, 1.000000000000000000, 0.8660254037844387076, 1.000000000000000000, 0.8660254037844387076, 1.000000000000000000, 0.8660254037844387076, 1.000000000000000000, 0.8660254037844387076, 1.000000000000000000, 0.8660254037844387076, 1.000000000000000000, 0.8660254037844387076, 1.000000000000000000, 0.8660254037844387076, 1.000000000000000000, 0.8660254037844387076, 1.000000000000000000, 0.8660254037844387076, 1.000000000000000000, 0.8660254037844387076, 1.000000000000000000, 0.8660254037844387076, 1.000000000000000000, 0.8660254037844387076, 1.000000000000000000, 0.9571563550410531196, 0.9417145902178731820 ) ) 
 REPRESENTATION_ITEM ( '' )  );
#13861 = CARTESIAN_POINT ( 'NONE',  ( -95.00000000000002842, 92.66308142843932671, 87.10281250086715943 ) ) ;
#13862 = CARTESIAN_POINT ( 'NONE',  ( 97.30629616937498838, 90.00000000000002842, 80.43531250086714124 ) ) ;
#13863 = ORIENTED_EDGE ( 'NONE', *, *, #64799, .F. ) ;
#13864 = VECTOR ( 'NONE', #45261, 1000.000000000000000 ) ;
#13865 = CARTESIAN_POINT ( 'NONE',  ( 92.34999999999999432, 88.47002178664753558, 85.05229166840096866 ) ) ;
#13866 = DIRECTION ( 'NONE',  ( 0.4279312458752991266, 0.9038112904824847638, 0.000000000000000000 ) ) ;
#13867 = VERTEX_POINT ( 'NONE', #51217 ) ;
#13868 = CARTESIAN_POINT ( 'NONE',  ( 92.35003236756683975, -208.4700030992239874, 87.48645704240064447 ) ) ;
#13869 = VERTEX_POINT ( 'NONE', #32441 ) ;
#13870 = ORIENTED_EDGE ( 'NONE', *, *, #41853, .F. ) ;
#13871 = AXIS2_PLACEMENT_3D ( 'NONE', #64814, #23839, #14024 ) ;
#13872 = ORIENTED_EDGE ( 'NONE', *, *, #25138, .T. ) ;
#13873 = CARTESIAN_POINT ( 'NONE',  ( -97.65000000000001990, 90.00000000000004263, 76.66499999999999204 ) ) ;
#13874 = CARTESIAN_POINT ( 'NONE',  ( 0.000000000000000000, 0.000000000000000000, 0.000000000000000000 ) ) ;
#13875 = CARTESIAN_POINT ( 'NONE',  ( -93.67500000000003979, 87.70503267997129626, 83.86166666666666458 ) ) ;
#13876 = EDGE_LOOP ( 'NONE', ( #30396, #49612 ) ) ;
#13877 = DIRECTION ( 'NONE',  ( -1.000000000000000000, -0.000000000000000000, -0.000000000000000000 ) ) ;
#13878 = EDGE_CURVE ( 'NONE', #14912, #58263, #23951, .T. ) ;
#13879 = DIRECTION ( 'NONE',  ( -1.000000000000000000, 0.000000000000000000, -0.000000000000000000 ) ) ;
#13880 = ORIENTED_EDGE ( 'NONE', *, *, #28169, .F. ) ;
#13881 = DIRECTION ( 'NONE',  ( -1.000000000000000000, -0.000000000000000000, 0.000000000000000000 ) ) ;
#13882 = CARTESIAN_POINT ( 'NONE',  ( -93.84685191531248449, -208.0026889286704943, 81.81114583420047381 ) ) ;
#13883 = VERTEX_POINT ( 'NONE', #21525 ) ;
#13884 = DIRECTION ( 'NONE',  ( 0.000000000000000000, 0.000000000000000000, 1.000000000000000000 ) ) ;
#13885 = CARTESIAN_POINT ( 'NONE',  ( 11.99999999999999822, -67.80270845531855173, -46.11716303203260736 ) ) ;
#13886 = DIRECTION ( 'NONE',  ( 0.000000000000000000, 0.000000000000000000, 1.000000000000000000 ) ) ;
#13887 = LINE ( 'NONE', #65781, #26627 ) ;
#13888 = EDGE_CURVE ( 'NONE', #66054, #35854, #3897, .T. ) ;
#13889 = LINE ( 'NONE', #59778, #37973 ) ;
#13890 = EDGE_CURVE ( 'NONE', #68271, #14366, #9883, .T. ) ;
#13891 = LINE ( 'NONE', #53394, #49338 ) ;
#13892 = CARTESIAN_POINT ( 'NONE',  ( 10.00000000000000000, 0.000000000000000000, 0.000000000000000000 ) ) ;
#13893 = CARTESIAN_POINT ( 'NONE',  ( -97.64999999999996305, -209.9999999999999716, 85.55499999999999261 ) ) ;
#13894 = ADVANCED_FACE ( 'NONE', ( #874 ), #58715, .T. ) ;
#13895 = CARTESIAN_POINT ( 'NONE',  ( 0.000000000000000000, -4.261787119644969479, -26.19803753235780519 ) ) ;
#13896 = CARTESIAN_POINT ( 'NONE',  ( 7.103376864691351012E-17, -120.0000000000000000, -80.00000000000000000 ) ) ;
#13897 = CARTESIAN_POINT ( 'NONE',  ( -92.69370383062504004, 90.00000000000004263, 75.99031250086714806 ) ) ;
#13898 = CARTESIAN_POINT ( 'NONE',  ( 10.00000000000000000, 31.47745569255140552, 68.26794271651274926 ) ) ;
#13899 = FACE_OUTER_BOUND ( 'NONE', #59553, .T. ) ;
#13900 = DIRECTION ( 'NONE',  ( 0.000000000000000000, 0.000000000000000000, -1.000000000000000000 ) ) ;
#13901 = CARTESIAN_POINT ( 'NONE',  ( 0.000000000000000000, 16.45098606841173705, -33.79645857604496229 ) ) ;
#13902 = ADVANCED_FACE ( 'NONE', ( #47076 ), #6483, .F. ) ;
#13903 = CARTESIAN_POINT ( 'NONE',  ( -92.34999999999999432, -210.0000001167898631, 84.68187499741277691 ) ) ;
#13904 = LINE ( 'NONE', #53770, #32220 ) ;
#13905 = DIRECTION ( 'NONE',  ( -1.000000000000000000, 0.000000000000000000, 0.000000000000000000 ) ) ;
#13906 = CARTESIAN_POINT ( 'NONE',  ( 97.64999999999999147, -209.9999999999999716, 78.88750000000000284 ) ) ;
#13907 = CARTESIAN_POINT ( 'NONE',  ( 11.99999999999999822, 31.46837873494978055, 68.27212725128286763 ) ) ;
#13908 = CARTESIAN_POINT ( 'NONE',  ( -92.34999999999999432, -209.9999999999999716, 86.50750000000000739 ) ) ;
#13909 = VECTOR ( 'NONE', #27211, 1000.000000000000000 ) ;
#13910 = DIRECTION ( 'NONE',  ( 1.000000000000000000, 0.000000000000000000, 0.000000000000000000 ) ) ;
#13911 = PRODUCT_DEFINITION_SHAPE ( 'NONE', 'NONE',  #74346 ) ;
#13912 = AXIS2_PLACEMENT_3D ( 'NONE', #11408, #74195, #62182 ) ;
#13913 = EDGE_CURVE ( 'NONE', #15161, #10181, #32038, .T. ) ;
#13914 = CIRCLE ( 'NONE', #2006, 82.00000000000000000 ) ;
#13915 = EDGE_LOOP ( 'NONE', ( #53850, #49635, #54370, #36643 ) ) ;
#13916 = CARTESIAN_POINT ( 'NONE',  ( 7.399999999999985256, -2.335046931737187547E-13, -22.90000000000041069 ) ) ;
#13917 = EDGE_CURVE ( 'NONE', #66576, #71829, #7215, .T. ) ;
#13918 = CYLINDRICAL_SURFACE ( 'NONE', #58195, 31.99999999999998579 ) ;
#13919 = ADVANCED_FACE ( 'NONE', ( #30133 ), #146, .T. ) ;
#13920 = EDGE_CURVE ( 'NONE', #38741, #56010, #9234, .T. ) ;
#13921 = AXIS2_PLACEMENT_3D ( 'NONE', #66563, #55274, #38358 ) ;
#13922 = VERTEX_POINT ( 'NONE', #23036 ) ;
#13923 = CARTESIAN_POINT ( 'NONE',  ( 0.000000000000000000, -76.41127070299262414, -12.93880638057396304 ) ) ;
#13924 = ADVANCED_FACE ( 'NONE', ( #18485 ), #35766, .F. ) ;
#13925 = CARTESIAN_POINT ( 'NONE',  ( 0.000000000000000000, -74.74816331893404708, -33.71516098798818462 ) ) ;
#13926 = ORIENTED_EDGE ( 'NONE', *, *, #24041, .T. ) ;
#13927 = CARTESIAN_POINT ( 'NONE',  ( 96.15314808468748708, -208.0026889286704943, 80.54114583420046358 ) ) ;
#13928 = CARTESIAN_POINT ( 'NONE',  ( 93.84685191531249870, -208.0026889286704943, 87.15572916753382060 ) ) ;
#13929 = ORIENTED_EDGE ( 'NONE', *, *, #17918, .F. ) ;
#13930 = CARTESIAN_POINT ( 'NONE',  ( 92.69370383062501162, -208.6684592857803011, 88.47864583420047779 ) ) ;
#13931 = ADVANCED_FACE ( 'NONE', ( #52326 ), #41424, .T. ) ;
#13932 = ADVANCED_BREP_SHAPE_REPRESENTATION ( '', ( #38137, #43395 ), #37485 ) ;
#13933 = EDGE_LOOP ( 'NONE', ( #72142, #68001, #54103, #10058 ) ) ;
#13934 = FACE_BOUND ( 'NONE', #48832, .T. ) ;
#13935 = ORIENTED_EDGE ( 'NONE', *, *, #45073, .F. ) ;
#13936 = CARTESIAN_POINT ( 'NONE',  ( -97.30629616937501680, 90.00000000000004263, 75.83156250086716454 ) ) ;
#13937 = ORIENTED_EDGE ( 'NONE', *, *, #37935, .F. ) ;
#13938 = ORIENTED_EDGE ( 'NONE', *, *, #71339, .T. ) ;
#13939 = CARTESIAN_POINT ( 'NONE',  ( -92.34999999999999432, -210.0000000334413528, 87.85687500050293863 ) ) ;
#13940 = ORIENTED_EDGE ( 'NONE', *, *, #24352, .T. ) ;
#13941 = PLANE ( 'NONE',  #59313 ) ;
#13942 = CARTESIAN_POINT ( 'NONE',  ( 97.65000000002596892, 89.99999999999992895, -74.99999999999992895 ) ) ;
#13943 = ORIENTED_EDGE ( 'NONE', *, *, #33731, .T. ) ;
#13944 = DIRECTION ( 'NONE',  ( -1.000000000000000000, -0.000000000000000000, -0.000000000000000000 ) ) ;
#13945 = ORIENTED_EDGE ( 'NONE', *, *, #35419, .F. ) ;
#13946 = CARTESIAN_POINT ( 'NONE',  ( 15.00000000000000000, 18.84667830672579569, -18.68964196561269375 ) ) ;
#13947 = CIRCLE ( 'NONE', #19962, 31.99999999999998579 ) ;
#13948 = ORIENTED_EDGE ( 'NONE', *, *, #42775, .F. ) ;
#13949 = VERTEX_POINT ( 'NONE', #22658 ) ;
#13950 = ORIENTED_EDGE ( 'NONE', *, *, #23203, .T. ) ;
#13951 = CARTESIAN_POINT ( 'NONE',  ( 96.15314808468750130, -211.9973110713294489, 78.42447916753381776 ) ) ;
#13952 = FACE_OUTER_BOUND ( 'NONE', #17844, .T. ) ;
#13953 = CONTEXT_DEPENDENT_SHAPE_REPRESENTATION ( #20070, #54164 ) ;
#13954 = CARTESIAN_POINT ( 'NONE',  ( 11.99999999999999822, -51.02545421589285723, -55.20638768913812555 ) ) ;
#13955 = ORIENTED_EDGE ( 'NONE', *, *, #2828, .T. ) ;
#13956 = CARTESIAN_POINT ( 'NONE',  ( 15.00000000000000000, 6.762365576493647445, 25.66652317338391498 ) ) ;
#13957 = VERTEX_POINT ( 'NONE', #57977 ) ;
#13958 = AXIS2_PLACEMENT_3D ( 'NONE', #67044, #33569, #11022 ) ;
#13959 = DIRECTION ( 'NONE',  ( -1.000000000000000000, 0.000000000000000000, 0.000000000000000000 ) ) ;
#13960 = CARTESIAN_POINT ( 'NONE',  ( -97.65000000000003411, -211.5299782133524502, 75.44791666666667140 ) ) ;
#13961 = CIRCLE ( 'NONE', #43986, 31.99999999999998579 ) ;
#13962 = CARTESIAN_POINT ( 'NONE',  ( 0.000000000000000000, 0.000000000000000000, 0.000000000000000000 ) ) ;
#13963 = LINE ( 'NONE', #65864, #51523 ) ;
#13964 = CARTESIAN_POINT ( 'NONE',  ( -92.69370383062498320, -208.6684592857803011, 81.12322916753382174 ) ) ;
#13965 = CARTESIAN_POINT ( 'NONE',  ( -95.00000000000002842, 92.66308142843932671, 78.84781250086714977 ) ) ;
#13966 = EDGE_LOOP ( 'NONE', ( #58338, #10650, #54833 ) ) ;
#13967 = CIRCLE ( 'NONE', #39211, 12.75000000000000000 ) ;
#13968 = CARTESIAN_POINT ( 'NONE',  ( 92.69370383062498320, 91.33154071421968467, 82.60489583420047666 ) ) ;
#13969 = AXIS2_PLACEMENT_3D ( 'NONE', #22521, #73259, #15758 ) ;
#13970 = ORIENTED_EDGE ( 'NONE', *, *, #18506, .F. ) ;
#13971 = DIRECTION ( 'NONE',  ( 1.000000000000000000, 0.000000000000000000, 0.000000000000000000 ) ) ;
#13972 = CARTESIAN_POINT ( 'NONE',  ( 0.000000000000000000, 0.000000000000000000, 0.000000000000000000 ) ) ;
#13973 = DIRECTION ( 'NONE',  ( -1.000000000000000000, 0.000000000000000000, -0.000000000000000000 ) ) ;
#13974 = CARTESIAN_POINT ( 'NONE',  ( 5.999999999999999112, 44.99326035066149387, -68.55367621811095091 ) ) ;
#13975 = DIRECTION ( 'NONE',  ( 1.000000000000000000, 0.000000000000000000, -0.000000000000000000 ) ) ;
#13976 = CARTESIAN_POINT ( 'NONE',  ( -94.99999999999997158, -212.6630814284392557, 81.54656250086713953 ) ) ;
#13977 = EDGE_CURVE ( 'NONE', #63033, #2062, #47670, .T. ) ;
#13978 = DIRECTION ( 'NONE',  ( -7.728965982074743403E-16, -1.065814103640131188E-14, -1.000000000000000000 ) ) ;
#13979 = DIRECTION ( 'NONE',  ( 0.000000000000000000, 0.000000000000000000, 1.000000000000000000 ) ) ;
#13980 = DIRECTION ( 'NONE',  ( 0.000000000000000000, 0.7071067811865439090, 0.7071067811865512365 ) ) ;
#13981 = VERTEX_POINT ( 'NONE', #39952 ) ;
#13982 = EDGE_CURVE ( 'NONE', #71305, #68580, #68530, .T. ) ;
#13983 = AXIS2_PLACEMENT_3D ( 'NONE', #66477, #71717, #36775 ) ;
#13984 = ORIENTED_EDGE ( 'NONE', *, *, #65311, .T. ) ;
#13985 = DIRECTION ( 'NONE',  ( -0.000000000000000000, -0.000000000000000000, -1.000000000000000000 ) ) ;
#13986 = EDGE_CURVE ( 'NONE', #28379, #42337, #46327, .T. ) ;
#13987 = EDGE_CURVE ( 'NONE', #15802, #21912, #68895, .T. ) ;
#13988 = DIRECTION ( 'NONE',  ( 0.000000000000000000, 0.000000000000000000, -1.000000000000000000 ) ) ;
#13989 = DIRECTION ( 'NONE',  ( 1.000000000000000000, -5.236901059551556403E-15, -2.618450529775778123E-14 ) ) ;
#13990 = CARTESIAN_POINT ( 'NONE',  ( -96.15314808468752972, 91.99731107132950569, 83.82197916753381151 ) ) ;
#13991 = CARTESIAN_POINT ( 'NONE',  ( -97.30599797242217619, -209.0535479562712169, 74.89836836546777477 ) ) ;
#13992 = DIRECTION ( 'NONE',  ( 0.000000000000000000, -0.8526401643540859610, -0.5224985647159591240 ) ) ;
#13993 = DIRECTION ( 'NONE',  ( -1.000000000000000000, -0.000000000000000000, -0.000000000000000000 ) ) ;
#13994 = ORIENTED_EDGE ( 'NONE', *, *, #66737, .F. ) ;
#13995 = CARTESIAN_POINT ( 'NONE',  ( -93.33921309982508774, 88.39975348990192572, 74.64190636928354650 ) ) ;
#13996 = CARTESIAN_POINT ( 'NONE',  ( 11.99999999999999822, 0.000000000000000000, 0.000000000000000000 ) ) ;
#13997 = AXIS2_PLACEMENT_3D ( 'NONE', #37691, #49682, #3486 ) ;
#13998 = CARTESIAN_POINT ( 'NONE',  ( 0.000000000000000000, 0.000000000000000000, 0.000000000000000000 ) ) ;
#13999 = CARTESIAN_POINT ( 'NONE',  ( 0.000000000000000000, 0.000000000000000000, -2.500000000000000000 ) ) ;
#14000 = CARTESIAN_POINT ( 'NONE',  ( 0.000000000000000000, -36.13751322684404244, -21.40280677340410165 ) ) ;
#14001 = ADVANCED_FACE ( 'NONE', ( #5749 ), #45969, .F. ) ;
#14002 = CYLINDRICAL_SURFACE ( 'NONE', #65243, 2.649999999999999467 ) ;
#14003 = CARTESIAN_POINT ( 'NONE',  ( -94.99999999999997158, -212.6630814284392557, 84.24531250086715772 ) ) ;
#14004 = EDGE_CURVE ( 'NONE', #11722, #40784, #40313, .T. ) ;
#14005 = DIRECTION ( 'NONE',  ( -1.000000000000000000, -0.000000000000000000, -0.000000000000000000 ) ) ;
#14006 = CIRCLE ( 'NONE', #47668, 77.49900000000000944 ) ;
#14007 = DIRECTION ( 'NONE',  ( 0.000000000000000000, 0.000000000000000000, 1.000000000000000000 ) ) ;
#14008 = FACE_OUTER_BOUND ( 'NONE', #25611, .T. ) ;
#14009 = DIRECTION ( 'NONE',  ( 0.000000000000000000, 0.7431448254773946882, -0.6691306063588577935 ) ) ;
#14010 = CIRCLE ( 'NONE', #56040, 16.00000000000000000 ) ;
#14011 = EDGE_LOOP ( 'NONE', ( #46535, #36233, #61392, #26433 ) ) ;
#14012 = PLANE ( 'NONE',  #56969 ) ;
#14013 = CYLINDRICAL_SURFACE ( 'NONE', #43148, 31.99999999999998579 ) ;
#14014 = FACE_OUTER_BOUND ( 'NONE', #35026, .T. ) ;
#14015 = EDGE_CURVE ( 'NONE', #232, #61944, #41657, .T. ) ;
#14016 = EDGE_CURVE ( 'NONE', #51621, #4009, #12776, .T. ) ;
#14017 = AXIS2_PLACEMENT_3D ( 'NONE', #2013, #47828, #65508 ) ;
#14018 = VECTOR ( 'NONE', #47575, 1000.000000000000000 ) ;
#14019 = CARTESIAN_POINT ( 'NONE',  ( 11.99999999999999822, -58.39081064771786345, 50.95692526931308919 ) ) ;
#14020 = CARTESIAN_POINT ( 'NONE',  ( 92.69370383062501162, -208.6684592857803011, 88.47864583420047779 ) ) ;
#14021 = VERTEX_POINT ( 'NONE', #65109 ) ;
#14022 = DIRECTION ( 'NONE',  ( -1.000000000000000000, -0.000000000000000000, -0.000000000000000000 ) ) ;
#14023 = CIRCLE ( 'NONE', #24827, 31.99999999999998934 ) ;
#14024 = DIRECTION ( 'NONE',  ( 0.000000000000000000, 0.9876883405951383255, -0.1564344650402276216 ) ) ;
#14025 = VERTEX_POINT ( 'NONE', #65840 ) ;
#14026 = DIRECTION ( 'NONE',  ( -1.000000000000000000, 0.000000000000000000, 0.000000000000000000 ) ) ;
#14027 = VECTOR ( 'NONE', #58590, 1000.000000000000000 ) ;
#14028 = ORIENTED_EDGE ( 'NONE', *, *, #10898, .F. ) ;
#14029 = CARTESIAN_POINT ( 'NONE',  ( 5.000000000000000000, -35.47612816024539484, 22.48208911017487921 ) ) ;
#14030 = AXIS2_PLACEMENT_3D ( 'NONE', #44280, #27726, #28459 ) ;
#14031 = VERTEX_POINT ( 'NONE', #14326 ) ;
#14032 = ORIENTED_EDGE ( 'NONE', *, *, #49389, .F. ) ;
#14033 = ORIENTED_EDGE ( 'NONE', *, *, #53709, .T. ) ;
#14034 = CARTESIAN_POINT ( 'NONE',  ( 92.35003715139268365, -208.4700003372809078, 76.69145685134846246 ) ) ;
#14035 = CIRCLE ( 'NONE', #51293, 31.99999999999999645 ) ;
#14036 = ORIENTED_EDGE ( 'NONE', *, *, #45283, .F. ) ;
#14037 = ORIENTED_EDGE ( 'NONE', *, *, #33979, .F. ) ;
#14038 = CARTESIAN_POINT ( 'NONE',  ( 97.30629616937498838, 88.66845928578037217, 79.90614583420048689 ) ) ;
#14039 = DIRECTION ( 'NONE',  ( -0.000000000000000000, 0.000000000000000000, 1.000000000000000000 ) ) ;
#14040 = DIRECTION ( 'NONE',  ( -1.000000000000000000, -0.000000000000000000, 0.000000000000000000 ) ) ;
#14041 = ORIENTED_EDGE ( 'NONE', *, *, #50820, .F. ) ;
#14042 = EDGE_LOOP ( 'NONE', ( #41220, #835, #63163, #39048 ) ) ;
#14043 = ORIENTED_EDGE ( 'NONE', *, *, #24020, .F. ) ;
#14044 = DIRECTION ( 'NONE',  ( -1.000000000000000000, -0.000000000000000000, 0.000000000000000000 ) ) ;
#14045 = ORIENTED_EDGE ( 'NONE', *, *, #5644, .T. ) ;
#14046 = DIRECTION ( 'NONE',  ( -0.04322280433995023818, -0.9990654579080344710, 7.115633110146689771E-17 ) ) ;
#14047 = DIRECTION ( 'NONE',  ( 1.000000000000000000, -0.000000000000000000, -0.000000000000000000 ) ) ;
#14048 = CARTESIAN_POINT ( 'NONE',  ( 4.749999999999999112, 6.447547231611302361E-16, 0.000000000000000000 ) ) ;
#14049 = DIRECTION ( 'NONE',  ( 1.000000000000000000, -0.000000000000000000, -0.000000000000000000 ) ) ;
#14050 = CARTESIAN_POINT ( 'NONE',  ( -97.64999999999999147, -210.0000225213925660, 84.36437578067156551 ) ) ;
#14051 = DIRECTION ( 'NONE',  ( 1.000000000000000000, -0.000000000000000000, -0.000000000000000000 ) ) ;
#14052 = CARTESIAN_POINT ( 'NONE',  ( 0.000000000000000000, 14.66109333815460225, 73.73191006444577056 ) ) ;
#14053 = CARTESIAN_POINT ( 'NONE',  ( -94.99999999999997158, -206.9400435732949575, 77.22062500173429100 ) ) ;
#14054 = CARTESIAN_POINT ( 'NONE',  ( -95.00000000000002842, 87.33691857156074434, 88.05531250086716000 ) ) ;
#14056 = CARTESIAN_POINT ( 'NONE',  ( -92.35000000000005116, 91.52997821335253548, 75.20979166840096752 ) ) ;
#14055 = CARTESIAN_POINT ( 'NONE',  ( 96.32499999999997442, 92.29496732002878900, 77.16770833506762983 ) ) ;
#14057 = ORIENTED_EDGE ( 'NONE', *, *, #61480, .T. ) ;
#14058 = CARTESIAN_POINT ( 'NONE',  ( 94.99999999999998579, 87.33691857156068750, 77.89531250086714920 ) ) ;
#14059 = CIRCLE ( 'NONE', #2144, 37.49900000000000233 ) ;
#14060 = DIRECTION ( 'NONE',  ( 1.000000000000000000, -0.000000000000000000, -0.000000000000000000 ) ) ;
#14061 = FACE_OUTER_BOUND ( 'NONE', #23975, .T. ) ;
#14062 = CARTESIAN_POINT ( 'NONE',  ( 0.000000000000000000, 22.48208911017500355, 35.47612816024530957 ) ) ;
#14063 = EDGE_CURVE ( 'NONE', #5078, #61762, #18836, .T. ) ;
#14064 = DIRECTION ( 'NONE',  ( -1.000000000000000000, -0.000000000000000000, 0.000000000000000000 ) ) ;
#14065 = CIRCLE ( 'NONE', #53681, 37.49900000000001654 ) ;
#14066 = DIRECTION ( 'NONE',  ( 1.000000000000000000, -0.000000000000000000, -0.000000000000000000 ) ) ;
#14067 = ORIENTED_EDGE ( 'NONE', *, *, #46776, .T. ) ;
#14068 = DIRECTION ( 'NONE',  ( 1.000000000000000000, 0.000000000000000000, -0.000000000000000000 ) ) ;
#14069 = CARTESIAN_POINT ( 'NONE',  ( 10.00000000000000000, -2.956366410621191765, 75.11725578898467859 ) ) ;
#14070 = ORIENTED_EDGE ( 'NONE', *, *, #38007, .F. ) ;
#14071 = CIRCLE ( 'NONE', #50070, 31.99999999999997868 ) ;
#14072 = EDGE_CURVE ( 'NONE', #49109, #36877, #62062, .T. ) ;
#14073 = ORIENTED_EDGE ( 'NONE', *, *, #57984, .T. ) ;
#14074 = VECTOR ( 'NONE', #41121, 1000.000000000000000 ) ;
#14075 = EDGE_CURVE ( 'NONE', #31904, #52407, #13579, .T. ) ;
#14076 = DIRECTION ( 'NONE',  ( 0.000000000000000000, 0.000000000000000000, 1.000000000000000000 ) ) ;
#14077 = DIRECTION ( 'NONE',  ( 0.000000000000000000, 0.4539904997395413644, 0.8910065241883706744 ) ) ;
#14078 = CARTESIAN_POINT ( 'NONE',  ( -92.35000000000003695, 89.99999998014077107, 85.95187500101400246 ) ) ;
#14079 = CIRCLE ( 'NONE', #27275, 12.49999999999999645 ) ;
#14080 = CARTESIAN_POINT ( 'NONE',  ( 10.00000000000000000, -14.67089635893764665, 73.72996012237435082 ) ) ;
#14081 = CARTESIAN_POINT ( 'NONE',  ( 11.99999999999999822, 20.41045688087824317, 72.35160999960824313 ) ) ;
#14082 =( BOUNDED_CURVE ( )  B_SPLINE_CURVE ( 2, ( #19410, #66405, #13404, #36332, #41992, #43487, #42359 ),
 .UNSPECIFIED., .F., .F. ) 
 B_SPLINE_CURVE_WITH_KNOTS ( ( 3, 2, 2, 3 ),
 ( 0.1874999999999999167, 0.1944444444444443365, 0.2013888888888887285, 0.2083333333333331483 ),
 .UNSPECIFIED. ) 
 CURVE ( )  GEOMETRIC_REPRESENTATION_ITEM ( )  RATIONAL_B_SPLINE_CURVE ( ( 1.000000000000001554, 0.8660254037844371533, 1.000000000000000000, 0.8660254037844387076, 1.000000000000000000, 0.8660254037844424824, 0.9999999999999962252 ) ) 
 REPRESENTATION_ITEM ( '' )  );
#14083 = CARTESIAN_POINT ( 'NONE',  ( -93.33922900947476364, -211.6002630214759961, 74.80065534806806227 ) ) ;
#14084 = EDGE_CURVE ( 'NONE', #12862, #12692, #54551, .T. ) ;
#14085 = VERTEX_POINT ( 'NONE', #37276 ) ;
#14086 = FACE_OUTER_BOUND ( 'NONE', #32611, .T. ) ;
#14087 = CARTESIAN_POINT ( 'NONE',  ( 5.000000000000000000, 67.80270845531956070, -46.11716303203112943 ) ) ;
#14088 = AXIS2_PLACEMENT_3D ( 'NONE', #49454, #47984, #7759 ) ;
#14089 = DIRECTION ( 'NONE',  ( 0.000000000000000000, 0.1564344650402312298, -0.9876883405951375483 ) ) ;
#14090 = FACE_OUTER_BOUND ( 'NONE', #63625, .T. ) ;
#14091 = CARTESIAN_POINT ( 'NONE',  ( 10.00000000000000000, 28.89263327155746097, 71.91182617369197771 ) ) ;
#14092 = LINE ( 'NONE', #32499, #52619 ) ;
#14093 = CARTESIAN_POINT ( 'NONE',  ( -94.99999999999997158, -213.0599564267049857, 76.18874999999999886 ) ) ;
#14094 = EDGE_CURVE ( 'NONE', #14025, #28347, #48540, .T. ) ;
#14095 = AXIS2_PLACEMENT_3D ( 'NONE', #67028, #16271, #55759 ) ;
#14096 = CARTESIAN_POINT ( 'NONE',  ( 0.000000000000000000, 68.26794271651262136, 31.47745569255165066 ) ) ;
#14097 = EDGE_CURVE ( 'NONE', #25646, #38932, #35641, .T. ) ;
#14098 = CARTESIAN_POINT ( 'NONE',  ( 93.84685191531248449, 88.00268892867053694, 84.19239583420049655 ) ) ;
#14099 = CARTESIAN_POINT ( 'NONE',  ( -93.84685191531247028, -211.9973110713294489, 86.20322916753382003 ) ) ;
#14100 = CARTESIAN_POINT ( 'NONE',  ( 92.35000000049316782, -210.0000320386632495, 83.73041644179299681 ) ) ;
#14101 = ORIENTED_EDGE ( 'NONE', *, *, #61002, .T. ) ;
#14102 = CARTESIAN_POINT ( 'NONE',  ( -7.999999999999992895, -1.142349898368590025E-14, -6.370018489464426943E-15 ) ) ;
#14103 = CARTESIAN_POINT ( 'NONE',  ( -97.64999999999996305, -209.9999999999999716, 81.74500000000000455 ) ) ;
#14104 = CARTESIAN_POINT ( 'NONE',  ( -97.65000000000001990, 90.00000000000004263, 84.92000000000000171 ) ) ;
#14105 = EDGE_CURVE ( 'NONE', #51481, #7862, #2046, .T. ) ;
#14106 = ADVANCED_FACE ( 'NONE', ( #8694 ), #70715, .T. ) ;
#14107 = CARTESIAN_POINT ( 'NONE',  ( 92.69370383062501162, -209.9999999999999716, 85.19781250086714408 ) ) ;
#14108 = VERTEX_POINT ( 'NONE', #37641 ) ;
#14109 = FACE_OUTER_BOUND ( 'NONE', #67747, .T. ) ;
#14110 = ORIENTED_EDGE ( 'NONE', *, *, #71380, .F. ) ;
#14111 = VECTOR ( 'NONE', #33749, 1000.000000000000000 ) ;
#14112 = ORIENTED_EDGE ( 'NONE', *, *, #31568, .F. ) ;
#14113 = DIRECTION ( 'NONE',  ( -1.000000000000000000, -0.000000000000000000, 0.000000000000000000 ) ) ;
#14114 = AXIS2_PLACEMENT_3D ( 'NONE', #66883, #60158, #31549 ) ;
#14115 = VECTOR ( 'NONE', #32400, 1000.000000000000114 ) ;
#14116 = ORIENTED_EDGE ( 'NONE', *, *, #52036, .T. ) ;
#14117 = CARTESIAN_POINT ( 'NONE',  ( -99.99999999999998579, -124.0000000000000142, -40.00000000000002132 ) ) ;
#14118 = CARTESIAN_POINT ( 'NONE',  ( 92.69370383062501162, -211.3315407142195852, 79.69447916753381378 ) ) ;
#14119 = CARTESIAN_POINT ( 'NONE',  ( -11.99999999999999645, 0.000000000000000000, 0.000000000000000000 ) ) ;
#14120 = CARTESIAN_POINT ( 'NONE',  ( 0.000000000000000000, 64.81221759200342092, 50.23322058963371006 ) ) ;
#14121 = CARTESIAN_POINT ( 'NONE',  ( 95.00000000000000000, -213.0599564267049857, 80.63375000000000625 ) ) ;
#14122 = DIRECTION ( 'NONE',  ( 0.000000000000000000, 0.000000000000000000, 1.000000000000000000 ) ) ;
#14123 = MANIFOLD_SOLID_BREP ( 'InnerRace', #11587 ) ;
#14124 = DIRECTION ( 'NONE',  ( -1.000000000000000000, -0.000000000000000000, 0.000000000000000000 ) ) ;
#14125 = CARTESIAN_POINT ( 'NONE',  ( 97.64999999999997726, -211.5299782133524502, 80.73958333333332860 ) ) ;
#14126 = VERTEX_POINT ( 'NONE', #13942 ) ;
#14127 = ORIENTED_EDGE ( 'NONE', *, *, #5009, .F. ) ;
#14128 = ORIENTED_EDGE ( 'NONE', *, *, #49895, .F. ) ;
#14129 = ORIENTED_EDGE ( 'NONE', *, *, #52454, .T. ) ;
#14130 = DIRECTION ( 'NONE',  ( 0.000000000000000000, 0.000000000000000000, 1.000000000000000000 ) ) ;
#14131 = CIRCLE ( 'NONE', #23752, 20.69999999999999929 ) ;
#14132 = SURFACE_STYLE_FILL_AREA ( #20897 ) ;
#14133 = CARTESIAN_POINT ( 'NONE',  ( -95.00000000000002842, 92.66308142843932671, 85.19781250086714408 ) ) ;
#14134 = DIRECTION ( 'NONE',  ( 1.000000000000000000, 0.000000000000000000, 0.000000000000000000 ) ) ;
#14135 = CIRCLE ( 'NONE', #34594, 37.49900000000000944 ) ;
#14136 = EDGE_CURVE ( 'NONE', #67800, #14697, #69245, .T. ) ;
#14137 = CARTESIAN_POINT ( 'NONE',  ( 11.99999999999999822, 77.19088730480532945, -6.903761155836932062 ) ) ;
#14138 = CARTESIAN_POINT ( 'NONE',  ( 93.67499999999999716, 87.70503267997126784, 75.50083333333331836 ) ) ;
#14139 = CIRCLE ( 'NONE', #53938, 31.99999999999998579 ) ;
#14140 = CARTESIAN_POINT ( 'NONE',  ( 12.49999999999999645, 1.530808498934191127E-15, 125.0000000000000000 ) ) ;
#14142 = EDGE_CURVE ( 'NONE', #59223, #42410, #36883, .T. ) ;
#14141 = AXIS2_PLACEMENT_3D ( 'NONE', #12528, #35464, #6892 ) ;
#14143 = VERTEX_POINT ( 'NONE', #54196 ) ;
#14144 = CARTESIAN_POINT ( 'NONE',  ( -93.67499999999998295, -212.2949673200287179, 84.57604166840096127 ) ) ;
#14145 = ORIENTED_EDGE ( 'NONE', *, *, #48147, .T. ) ;
#14146 = CARTESIAN_POINT ( 'NONE',  ( -8.826826895187510402, -94.96827758698185562, -5.500000000000000000 ) ) ;
#14148 = VERTEX_POINT ( 'NONE', #44767 ) ;
#14147 = EDGE_CURVE ( 'NONE', #2572, #26241, #57231, .T. ) ;
#14149 = CARTESIAN_POINT ( 'NONE',  ( -93.67500000000003979, 87.70503267997129626, 87.11604166840096752 ) ) ;
#14150 = AXIS2_PLACEMENT_3D ( 'NONE', #19653, #26034, #37339 ) ;
#14151 = ORIENTED_EDGE ( 'NONE', *, *, #42274, .F. ) ;
#14152 = CARTESIAN_POINT ( 'NONE',  ( 97.30629616937498838, 91.33154071421968467, 86.99697916753382287 ) ) ;
#14153 = DIRECTION ( 'NONE',  ( -1.000000000000000000, 0.000000000000000000, -0.000000000000000000 ) ) ;
#14154 = PRODUCT_DEFINITION ( 'UNKNOWN', '', #38807, #31111 ) ;
#14155 = EDGE_CURVE ( 'NONE', #31529, #28408, #21067, .T. ) ;
#14156 = CARTESIAN_POINT ( 'NONE',  ( -92.35000000000005116, 88.47002178664754979, 83.99395833506763154 ) ) ;
#14157 = CARTESIAN_POINT ( 'NONE',  ( -3.000000000000000000, -18.13022148937263012, 15.02647892043544608 ) ) ;
#14158 = FACE_OUTER_BOUND ( 'NONE', #54084, .T. ) ;
#14159 = ORIENTED_EDGE ( 'NONE', *, *, #34709, .F. ) ;
#14160 = FACE_OUTER_BOUND ( 'NONE', #62375, .T. ) ;
#14161 = DIRECTION ( 'NONE',  ( -1.000000000000000000, -0.000000000000000000, 0.000000000000000000 ) ) ;
#14162 = ORIENTED_EDGE ( 'NONE', *, *, #41092, .F. ) ;
#14163 = EDGE_CURVE ( 'NONE', #50561, #55514, #20022, .T. ) ;
#14164 = ORIENTED_EDGE ( 'NONE', *, *, #1081, .T. ) ;
#14165 = CARTESIAN_POINT ( 'NONE',  ( 0.000000000000000000, 77.49459641780886443, -0.8261519478433960728 ) ) ;
#14166 = DIRECTION ( 'NONE',  ( -1.000000000000000000, -0.000000000000000000, -0.000000000000000000 ) ) ;
#14167 = CARTESIAN_POINT ( 'NONE',  ( 15.00000000000000000, -19.89357724624986545, 12.59942793731086219 ) ) ;
#14168 = CARTESIAN_POINT ( 'NONE',  ( -94.99999999999997158, -212.6630814284392557, 84.24531250086715772 ) ) ;
#14169 = ORIENTED_EDGE ( 'NONE', *, *, #44246, .F. ) ;
#14170 = EDGE_CURVE ( 'NONE', #58159, #18231, #14010, .T. ) ;
#14171 = VECTOR ( 'NONE', #43571, 1000.000000000000000 ) ;
#14172 = FILL_AREA_STYLE ('',( #25830 ) ) ;
#14173 = ORIENTED_EDGE ( 'NONE', *, *, #32763, .F. ) ;
#14174 = AXIS2_PLACEMENT_3D ( 'NONE', #44540, #62965, #5806 ) ;
#14175 = AXIS2_PLACEMENT_3D ( 'NONE', #46476, #10408, #67932 ) ;
#14176 = ORIENTED_EDGE ( 'NONE', *, *, #26965, .F. ) ;
#14177 = CARTESIAN_POINT ( 'NONE',  ( 5.999999999999999112, -55.16347631943085617, 60.67117009219117563 ) ) ;
#14178 = CARTESIAN_POINT ( 'NONE',  ( 92.34999999999999432, 90.00000000000002842, 86.82500000000000284 ) ) ;
#14179 = AXIS2_PLACEMENT_3D ( 'NONE', #43792, #4686, #10670 ) ;
#14180 = DIRECTION ( 'NONE',  ( -1.000000000000000000, 0.000000000000000000, -0.000000000000000000 ) ) ;
#14181 = CARTESIAN_POINT ( 'NONE',  ( 92.69370383062498320, 91.33154071421968467, 76.88989583420047325 ) ) ;
#14182 = AXIS2_PLACEMENT_3D ( 'NONE', #10410, #2690, #36476 ) ;
#14183 = DIRECTION ( 'NONE',  ( 0.000000000000000000, 0.000000000000000000, -1.000000000000000000 ) ) ;
#14184 = DIRECTION ( 'NONE',  ( -1.000000000000000000, 0.000000000000000000, -0.000000000000000000 ) ) ;
#14185 = DIRECTION ( 'NONE',  ( -1.000000000000000000, 0.000000000000000000, 0.000000000000000000 ) ) ;
#14186 = CARTESIAN_POINT ( 'NONE',  ( 95.29776683160947925, 92.36156954995058754, 74.83035915144989758 ) ) ;
#14187 = CARTESIAN_POINT ( 'NONE',  ( 3.000000000000000000, 0.000000000000000000, 0.000000000000000000 ) ) ;
#14188 = EDGE_CURVE ( 'NONE', #56042, #36390, #27074, .T. ) ;
#14189 = DIRECTION ( 'NONE',  ( 0.000000000000000000, 0.8090169943749445647, 0.5877852522924770229 ) ) ;
#14190 = EDGE_CURVE ( 'NONE', #64128, #20120, #71643, .T. ) ;
#14191 = DIRECTION ( 'NONE',  ( -1.000000000000000000, 0.000000000000000000, 0.000000000000000000 ) ) ;
#14192 = DIRECTION ( 'NONE',  ( -1.000000000000000000, 0.000000000000000000, -0.000000000000000000 ) ) ;
#14193 = EDGE_LOOP ( 'NONE', ( #66569, #53415, #30582, #58879 ) ) ;
#14194 = CARTESIAN_POINT ( 'NONE',  ( -95.00000000000002842, 87.33691857156074434, 87.26156250086714294 ) ) ;
#14195 = DIRECTION ( 'NONE',  ( -0.6064928550163524168, -0.7950889364178789220, 0.000000000000000000 ) ) ;
#14196 = AXIS2_PLACEMENT_3D ( 'NONE', #69982, #53445, #59096 ) ;
#14197 = VECTOR ( 'NONE', #43862, 1000.000000000000000 ) ;
#14198 = AXIS2_PLACEMENT_3D ( 'NONE', #21899, #33168, #16258 ) ;
#14199 = CIRCLE ( 'NONE', #35827, 31.99999999999999289 ) ;
#14200 = DIRECTION ( 'NONE',  ( -1.000000000000000000, 0.000000000000000000, -0.000000000000000000 ) ) ;
#14201 = ORIENTED_EDGE ( 'NONE', *, *, #20686, .F. ) ;
#14202 = AXIS2_PLACEMENT_3D ( 'NONE', #23378, #64340, #40664 ) ;
#14203 = CARTESIAN_POINT ( 'NONE',  ( 26.09152095774781799, -124.8716048804687375, 5.500000000000000000 ) ) ;
#14204 = DIRECTION ( 'NONE',  ( 0.000000000000000000, -0.1564344650402170744, -0.9876883405951398798 ) ) ;
#14205 = CARTESIAN_POINT ( 'NONE',  ( 0.000000000000000000, -46.54456581323762521, -59.03342792756313884 ) ) ;
#14206 = CARTESIAN_POINT ( 'NONE',  ( 97.30629616937498838, -209.9999999999999716, 81.86406250086714920 ) ) ;
#14207 = VERTEX_POINT ( 'NONE', #15061 ) ;
#14208 = ORIENTED_EDGE ( 'NONE', *, *, #1495, .F. ) ;
#14209 = ADVANCED_FACE ( 'NONE', ( #4926 ), #66934, .T. ) ;
#14210 = DIRECTION ( 'NONE',  ( -1.000000000000000000, -0.000000000000000000, -0.000000000000000000 ) ) ;
#14211 = DIRECTION ( 'NONE',  ( 0.000000000000000000, 0.000000000000000000, 1.000000000000000000 ) ) ;
#14212 = DIRECTION ( 'NONE',  ( 1.000000000000000000, 0.000000000000000000, 0.000000000000000000 ) ) ;
#14213 = VECTOR ( 'NONE', #55106, 1000.000000000000000 ) ;
#14214 = VERTEX_POINT ( 'NONE', #9801 ) ;
#14215 = LINE ( 'NONE', #8592, #48916 ) ;
#14216 = CARTESIAN_POINT ( 'NONE',  ( 92.35000000000000853, -209.9999999999999716, 90.00000000000000000 ) ) ;
#14217 = CIRCLE ( 'NONE', #59870, 42.00000000000000000 ) ;
#14218 = ORIENTED_EDGE ( 'NONE', *, *, #54821, .F. ) ;
#14219 = DIRECTION ( 'NONE',  ( -1.000000000000000000, -0.000000000000000000, 0.000000000000000000 ) ) ;
#14220 = VERTEX_POINT ( 'NONE', #56417 ) ;
#14221 = VERTEX_POINT ( 'NONE', #44018 ) ;
#14222 = CIRCLE ( 'NONE', #62289, 77.49899999999999523 ) ;
#14223 =( NAMED_UNIT ( * ) PLANE_ANGLE_UNIT ( ) SI_UNIT ( $, .RADIAN. ) );
#14224 = CARTESIAN_POINT ( 'NONE',  ( 0.000000000000000000, 14.67089635893819377, -73.72996012237423713 ) ) ;
#14225 = AXIS2_PLACEMENT_3D ( 'NONE', #12444, #41759, #52673 ) ;
#14226 = ADVANCED_FACE ( 'NONE', ( #9423 ), #60933, .T. ) ;
#14227 = ORIENTED_EDGE ( 'NONE', *, *, #34645, .F. ) ;
#14228 = CARTESIAN_POINT ( 'NONE',  ( 0.000000000000000000, 55.19960302592141232, -51.03279382321027668 ) ) ;
#14229 = CARTESIAN_POINT ( 'NONE',  ( 95.00000000000000000, -213.0599564267049857, 85.15812500173430521 ) ) ;
#14230 = CARTESIAN_POINT ( 'NONE',  ( 97.64999999999999147, 90.00000000000002842, 85.87249999999998806 ) ) ;
#14231 = EDGE_CURVE ( 'NONE', #3457, #11454, #45281, .T. ) ;
#14232 = ORIENTED_EDGE ( 'NONE', *, *, #32909, .F. ) ;
#14233 = DIRECTION ( 'NONE',  ( 0.000000000000000000, 0.2334453638559060296, -0.9723699203976764460 ) ) ;
#14234 = DIRECTION ( 'NONE',  ( 1.000000000000000000, 0.000000000000000000, 0.000000000000000000 ) ) ;
#14235 = EDGE_LOOP ( 'NONE', ( #57149, #9867 ) ) ;
#14236 = ORIENTED_EDGE ( 'NONE', *, *, #24640, .T. ) ;
#14237 = CARTESIAN_POINT ( 'NONE',  ( -92.69370383062505425, 88.66845928578038638, 87.52614583420049144 ) ) ;
#14238 = CARTESIAN_POINT ( 'NONE',  ( 93.84685191531248449, 91.99731107132950569, 82.55197916753380127 ) ) ;
#14239 = ORIENTED_EDGE ( 'NONE', *, *, #52956, .F. ) ;
#14240 = CARTESIAN_POINT ( 'NONE',  ( 97.64999999999997726, 88.47002178664753558, 81.45395833506763950 ) ) ;
#14241 = EDGE_CURVE ( 'NONE', #69413, #40595, #58506, .T. ) ;
#14242 = VECTOR ( 'NONE', #40010, 1000.000000000000000 ) ;
#14243 = EDGE_CURVE ( 'NONE', #24697, #13883, #6890, .T. ) ;
#14244 = DIRECTION ( 'NONE',  ( 0.000000000000000000, 0.7071067811865487940, -0.7071067811865462405 ) ) ;
#14245 = ORIENTED_EDGE ( 'NONE', *, *, #43894, .F. ) ;
#14246 = FACE_BOUND ( 'NONE', #32230, .T. ) ;
#14247 = EDGE_LOOP ( 'NONE', ( #5910, #53992, #17097, #67385 ) ) ;
#14248 = AXIS2_PLACEMENT_3D ( 'NONE', #23676, #46610, #69542 ) ;
#14249 = ORIENTED_EDGE ( 'NONE', *, *, #12323, .T. ) ;
#14250 = VERTEX_POINT ( 'NONE', #3444 ) ;
#14251 = PLANE ( 'NONE',  #25261 ) ;
#14252 = DIRECTION ( 'NONE',  ( 0.000000000000000000, -0.8526401643540860720, -0.5224985647159590130 ) ) ;
#14253 = VECTOR ( 'NONE', #35755, 1000.000000000000000 ) ;
#14254 = AXIS2_PLACEMENT_3D ( 'NONE', #45944, #50811, #28624 ) ;
#14255 = CARTESIAN_POINT ( 'NONE',  ( -92.35000000000003695, 90.00000000000004263, 83.33250000000001023 ) ) ;
#14256 = ORIENTED_EDGE ( 'NONE', *, *, #44687, .T. ) ;
#14257 = CARTESIAN_POINT ( 'NONE',  ( 10.00000000000000000, 22.74946021919175720, -29.81001611430984255 ) ) ;
#14258 = AXIS2_PLACEMENT_3D ( 'NONE', #26513, #72001, #15231 ) ;
#14259 = CARTESIAN_POINT ( 'NONE',  ( -18.12185313557660038, -104.9634299478706794, 5.500000000000000000 ) ) ;
#14260 = ORIENTED_EDGE ( 'NONE', *, *, #8407, .F. ) ;
#14261 = PLANE ( 'NONE',  #13153 ) ;
#14262 = CARTESIAN_POINT ( 'NONE',  ( -92.69370383062498320, -209.9999999999999716, 80.43531250086714124 ) ) ;
#14263 = ORIENTED_EDGE ( 'NONE', *, *, #7828, .T. ) ;
#14265 = ADVANCED_FACE ( 'NONE', ( #49276 ), #32348, .T. ) ;
#14264 = DIRECTION ( 'NONE',  ( -1.000000000000000000, 0.000000000000000000, 0.000000000000000000 ) ) ;
#14266 = DIRECTION ( 'NONE',  ( -0.000000000000000000, -0.000000000000000000, -1.000000000000000000 ) ) ;
#14267 = CYLINDRICAL_SURFACE ( 'NONE', #30857, 31.99999999999998579 ) ;
#14268 = FACE_OUTER_BOUND ( 'NONE', #53732, .T. ) ;
#14269 = DIRECTION ( 'NONE',  ( -0.000000000000000000, -1.000000000000000000, -0.000000000000000000 ) ) ;
#14270 = FACE_OUTER_BOUND ( 'NONE', #4321, .T. ) ;
#14271 = CARTESIAN_POINT ( 'NONE',  ( 11.99999999999999822, 71.91182617369230456, -28.89263327155667938 ) ) ;
#14272 = CARTESIAN_POINT ( 'NONE',  ( 10.00000000000000000, 16.65972982744934683, 80.28980883073762698 ) ) ;
#14273 = DIRECTION ( 'NONE',  ( 0.000000000000000000, 0.000000000000000000, 1.000000000000000000 ) ) ;
#14274 = CARTESIAN_POINT ( 'NONE',  ( 97.64999999999999147, 89.99999989488613039, 86.58687499784845443 ) ) ;
#14275 = CIRCLE ( 'NONE', #25122, 3.000000000000000000 ) ;
#14276 = ADVANCED_FACE ( 'NONE', ( #73308 ), #17180, .F. ) ;
#14277 = EDGE_CURVE ( 'NONE', #5475, #61574, #54907, .T. ) ;
#14278 = CARTESIAN_POINT ( 'NONE',  ( -93.84685191531252713, 88.00268892867056536, 75.88447916753381151 ) ) ;
#14279 = CYLINDRICAL_SURFACE ( 'NONE', #70676, 16.00000000000000000 ) ;
#14280 = DIRECTION ( 'NONE',  ( -0.000000000000000000, -0.000000000000000000, -1.000000000000000000 ) ) ;
#14281 = DIRECTION ( 'NONE',  ( -1.000000000000000000, 0.000000000000000000, -0.000000000000000000 ) ) ;
#14282 = AXIS2_PLACEMENT_3D ( 'NONE', #63728, #35510, #18218 ) ;
#14283 = EDGE_CURVE ( 'NONE', #57624, #55001, #56098, .T. ) ;
#14284 = LINE ( 'NONE', #8655, #73647 ) ;
#14285 = AXIS2_PLACEMENT_3D ( 'NONE', #47160, #5838, #70427 ) ;
#14286 = AXIS2_PLACEMENT_3D ( 'NONE', #33051, #9763, #43625 ) ;
#14287 = CARTESIAN_POINT ( 'NONE',  ( -3.000000000000000000, 5.835314593368772229, -22.81335362449846826 ) ) ;
#14288 = CARTESIAN_POINT ( 'NONE',  ( 11.99999999999999822, 51.02545421589324803, 55.20638768913779870 ) ) ;
#14289 = LINE ( 'NONE', #13181, #20294 ) ;
#14290 = CARTESIAN_POINT ( 'NONE',  ( -97.64999999999996305, -209.9999999999999716, 75.39499999999999602 ) ) ;
#14291 = PLANE ( 'NONE',  #38822 ) ;
#14292 = CARTESIAN_POINT ( 'NONE',  ( -94.99999999999997158, -206.9400435732949575, 87.93625000000000114 ) ) ;
#14293 = AXIS2_PLACEMENT_3D ( 'NONE', #54077, #37155, #3332 ) ;
#14294 = LINE ( 'NONE', #3411, #64992 ) ;
#14295 = ORIENTED_EDGE ( 'NONE', *, *, #13077, .T. ) ;
#14296 = DIRECTION ( 'NONE',  ( 2.603472992746261562E-14, 2.546204323184492723E-14, -1.000000000000000000 ) ) ;
#14297 = FACE_OUTER_BOUND ( 'NONE', #11617, .T. ) ;
#14299 = CARTESIAN_POINT ( 'NONE',  ( -8.000000000000007105, -1.142349898368590025E-14, -6.370018489464426943E-15 ) ) ;
#14298 = AXIS2_PLACEMENT_3D ( 'NONE', #2393, #9091, #54953 ) ;
#14300 = DIRECTION ( 'NONE',  ( 1.000000000000000000, -0.000000000000000000, -0.000000000000000000 ) ) ;
#14301 = AXIS2_PLACEMENT_3D ( 'NONE', #46265, #51899, #57919 ) ;
#14302 = VECTOR ( 'NONE', #2337, 1000.000000000000000 ) ;
#14303 = VECTOR ( 'NONE', #37545, 1000.000000000000000 ) ;
#14304 = ORIENTED_EDGE ( 'NONE', *, *, #36310, .T. ) ;
#14305 = VECTOR ( 'NONE', #8288, 1000.000000000000000 ) ;
#14306 = DIRECTION ( 'NONE',  ( 0.6575728627325957421, -0.7533909544171994987, 0.000000000000000000 ) ) ;
#14307 = DIRECTION ( 'NONE',  ( 0.000000000000000000, 0.000000000000000000, 1.000000000000000000 ) ) ;
#14308 = ORIENTED_EDGE ( 'NONE', *, *, #71806, .T. ) ;
#14309 = EDGE_CURVE ( 'NONE', #39865, #45184, #14792, .T. ) ;
#14310 =( BOUNDED_CURVE ( )  B_SPLINE_CURVE ( 2, ( #13939, #47434, #59830, #8316, #7940, #70337, #64361, #70712, #42172 ),
 .UNSPECIFIED., .F., .F. ) 
 B_SPLINE_CURVE_WITH_KNOTS ( ( 3, 2, 2, 2, 3 ),
 ( 0.1058364832028025337, 0.1128922486546722892, 0.1199480141955893697, 0.1270037797365064502, 0.1270039290057624060 ),
 .UNSPECIFIED. ) 
 CURVE ( )  GEOMETRIC_REPRESENTATION_ITEM ( )  RATIONAL_B_SPLINE_CURVE ( ( 1.000000000000000000, 0.8660254037844387076, 1.000000000000000000, 0.8660254037844387076, 1.000000000000000000, 0.8660254037844387076, 1.000000000000000000, 0.9999971656812888243, 0.9999943314825013863 ) ) 
 REPRESENTATION_ITEM ( '' )  );
#14311 = CARTESIAN_POINT ( 'NONE',  ( 96.15314808468750130, -211.9973110713294489, 82.86947916753379673 ) ) ;
#14312 = CARTESIAN_POINT ( 'NONE',  ( 95.00000000000000000, -207.3369185715606307, 89.64281250086715147 ) ) ;
#14313 = VERTEX_POINT ( 'NONE', #61326 ) ;
#14314 = CARTESIAN_POINT ( 'NONE',  ( 96.15314808468748708, -208.0026889286704943, 86.41489583420049314 ) ) ;
#14315 = VERTEX_POINT ( 'NONE', #9809 ) ;
#14316 = DIRECTION ( 'NONE',  ( 0.000000000000000000, -0.7071067811865536790, 0.7071067811865413555 ) ) ;
#14317 = ORIENTED_EDGE ( 'NONE', *, *, #13811, .F. ) ;
#14318 = CARTESIAN_POINT ( 'NONE',  ( -92.69370383062502583, 88.66845928578038638, 78.63614583420049087 ) ) ;
#14319 = EDGE_CURVE ( 'NONE', #49855, #47001, #14065, .T. ) ;
#14320 = VERTEX_POINT ( 'NONE', #38756 ) ;
#14321 = VERTEX_POINT ( 'NONE', #10177 ) ;
#14322 = DIRECTION ( 'NONE',  ( 1.000000000000000000, 0.000000000000000000, 0.000000000000000000 ) ) ;
#14323 = EDGE_CURVE ( 'NONE', #1097, #72747, #23681, .T. ) ;
#14324 = ORIENTED_EDGE ( 'NONE', *, *, #73736, .F. ) ;
#14325 = CARTESIAN_POINT ( 'NONE',  ( 10.00000000000000000, -17.28742895386031719, -75.54627589209962935 ) ) ;
#14326 = CARTESIAN_POINT ( 'NONE',  ( 26.50000000000260414, -120.0000000000000000, -64.99999999999930367 ) ) ;
#14327 = ORIENTED_EDGE ( 'NONE', *, *, #44243, .T. ) ;
#14328 = CARTESIAN_POINT ( 'NONE',  ( 3.000000000000000000, 2.935248768560057897, -3.252606517456513302E-15 ) ) ;
#14329 = EDGE_LOOP ( 'NONE', ( #73773, #49284, #62359, #72650 ) ) ;
#14330 = DIRECTION ( 'NONE',  ( 0.000000000000000000, 0.000000000000000000, 1.000000000000000000 ) ) ;
#14331 = AXIS2_PLACEMENT_3D ( 'NONE', #63661, #6508, #35073 ) ;
#14332 = VECTOR ( 'NONE', #61019, 1000.000000000000000 ) ;
#14333 = ORIENTED_EDGE ( 'NONE', *, *, #62045, .T. ) ;
#14334 = AXIS2_PLACEMENT_3D ( 'NONE', #47555, #8811, #53562 ) ;
#14335 = ADVANCED_FACE ( 'NONE', ( #71 ), #18406, .F. ) ;
#14336 = VECTOR ( 'NONE', #48202, 1000.000000000000000 ) ;
#14337 = ORIENTED_EDGE ( 'NONE', *, *, #52262, .F. ) ;
#14338 = ORIENTED_EDGE ( 'NONE', *, *, #66195, .T. ) ;
#14339 = CARTESIAN_POINT ( 'NONE',  ( 96.15314808468748708, -208.0026889286704943, 77.36614583420046642 ) ) ;
#14340 = FACE_OUTER_BOUND ( 'NONE', #52591, .T. ) ;
#14341 = CARTESIAN_POINT ( 'NONE',  ( -96.32500000000001705, 87.70503267997129626, 81.85083333333332689 ) ) ;
#14342 = EDGE_LOOP ( 'NONE', ( #5008, #60947, #43654, #14045 ) ) ;
#14343 = EDGE_LOOP ( 'NONE', ( #19129, #44415, #8061, #41356 ) ) ;
#14344 = DIRECTION ( 'NONE',  ( 0.000000000000000000, 0.000000000000000000, 1.000000000000000000 ) ) ;
#14345 = CARTESIAN_POINT ( 'NONE',  ( 92.34999999999999432, 90.00000000000002842, 76.03000000000000114 ) ) ;
#14346 = ORIENTED_EDGE ( 'NONE', *, *, #65697, .T. ) ;
#14347 = CARTESIAN_POINT ( 'NONE',  ( -92.34999999999999432, -209.9999999999999716, 88.49187500173430010 ) ) ;
#14348 = PLANE ( 'NONE',  #34733 ) ;
#14349 = CARTESIAN_POINT ( 'NONE',  ( -92.69370383062498320, -209.9999999999999716, 81.70531250086713726 ) ) ;
#14350 = CARTESIAN_POINT ( 'NONE',  ( -92.69370383062504004, 90.00000000000004263, 77.41906250086715602 ) ) ;
#14351 = ORIENTED_EDGE ( 'NONE', *, *, #74092, .T. ) ;
#14352 = ADVANCED_FACE ( 'NONE', ( #57539 ), #11649, .F. ) ;
#14353 = CARTESIAN_POINT ( 'NONE',  ( 92.69370383062498320, 90.00000000000002842, 80.75281250086715090 ) ) ;
#14354 = ORIENTED_EDGE ( 'NONE', *, *, #39567, .F. ) ;
#14355 = FACE_OUTER_BOUND ( 'NONE', #73810, .T. ) ;
#14356 = LINE ( 'NONE', #14720, #52779 ) ;
#14358 = EDGE_CURVE ( 'NONE', #35896, #70403, #42901, .T. ) ;
#14357 = DIRECTION ( 'NONE',  ( -0.000000000000000000, -0.000000000000000000, -1.000000000000000000 ) ) ;
#14359 = DIRECTION ( 'NONE',  ( -1.000000000000000000, 0.000000000000000000, -0.000000000000000000 ) ) ;
#14360 = DIRECTION ( 'NONE',  ( -1.000000000000000000, -0.000000000000000000, -0.000000000000000000 ) ) ;
#14361 = CARTESIAN_POINT ( 'NONE',  ( -96.15314808468745866, -211.9973110713294489, 84.03364583420047040 ) ) ;
#14362 = CARTESIAN_POINT ( 'NONE',  ( -23.50044424985086522, 0.001194404165009976208, -65.00000000000061107 ) ) ;
#14363 = CARTESIAN_POINT ( 'NONE',  ( -97.64999999947046661, -209.9999663481462164, 81.18829462297327382 ) ) ;
#14364 = EDGE_CURVE ( 'NONE', #56884, #16859, #27258, .T. ) ;
#14365 = CARTESIAN_POINT ( 'NONE',  ( 12.69589495141918611, -96.69089767102708777, 5.500000000000000000 ) ) ;
#14366 = VERTEX_POINT ( 'NONE', #69907 ) ;
#14367 = CIRCLE ( 'NONE', #39594, 31.99999999999999289 ) ;
#14368 = VECTOR ( 'NONE', #42303, 1000.000000000000000 ) ;
#14369 = ORIENTED_EDGE ( 'NONE', *, *, #7054, .F. ) ;
#14370 = DIRECTION ( 'NONE',  ( -1.000000000000000000, -0.000000000000000000, 0.000000000000000000 ) ) ;
#14371 = CARTESIAN_POINT ( 'NONE',  ( -92.35000000000003695, 90.00000000000004263, 90.00000000000000000 ) ) ;
#14372 = FACE_OUTER_BOUND ( 'NONE', #54780, .T. ) ;
#14373 = EDGE_CURVE ( 'NONE', #11102, #11035, #1541, .T. ) ;
#14374 = CARTESIAN_POINT ( 'NONE',  ( -92.69370383062502583, 88.66845928578038638, 86.73239583420047438 ) ) ;
#14375 = CARTESIAN_POINT ( 'NONE',  ( -97.49696879394605276, -209.7556371990022512, 74.91343443312145212 ) ) ;
#14376 = CARTESIAN_POINT ( 'NONE',  ( 10.00000000000000000, -46.11716303203136391, -67.80270845531937596 ) ) ;
#14377 = CARTESIAN_POINT ( 'NONE',  ( 97.64999999999999147, 90.00000000000002842, 77.61749999999999261 ) ) ;
#14378 = ORIENTED_EDGE ( 'NONE', *, *, #24875, .T. ) ;
#14379 = CARTESIAN_POINT ( 'NONE',  ( 10.00000000000000000, 8.830959090343430518, -74.65491531819107252 ) ) ;
#14380 = FACE_OUTER_BOUND ( 'NONE', #59360, .T. ) ;
#14381 = CARTESIAN_POINT ( 'NONE',  ( -96.32500000000001705, 92.29496732002878900, 82.35354166840096468 ) ) ;
#14382 = CYLINDRICAL_SURFACE ( 'NONE', #42972, 31.99999999999999289 ) ;
#14383 = DIRECTION ( 'NONE',  ( 0.1736481776669309418, -0.9848077530122080203, 0.000000000000000000 ) ) ;
#14384 = DIRECTION ( 'NONE',  ( -0.000000000000000000, -0.000000000000000000, 1.000000000000000000 ) ) ;
#14385 = CARTESIAN_POINT ( 'NONE',  ( -96.15314808468747287, -208.0026889286704943, 82.71072916753381321 ) ) ;
#14386 = FACE_OUTER_BOUND ( 'NONE', #57156, .T. ) ;
#14387 = CIRCLE ( 'NONE', #56422, 77.49899999999999523 ) ;
#14388 = CARTESIAN_POINT ( 'NONE',  ( -10.00000000000000000, 0.000000000000000000, 0.000000000000000000 ) ) ;
#14389 = VECTOR ( 'NONE', #44085, 1000.000000000000000 ) ;
#14390 = DIRECTION ( 'NONE',  ( -0.000000000000000000, -0.000000000000000000, 1.000000000000000000 ) ) ;
#14391 = CARTESIAN_POINT ( 'NONE',  ( -99.99999999999997158, -214.9999999999999716, 90.00000000000000000 ) ) ;
#14392 = ORIENTED_EDGE ( 'NONE', *, *, #53702, .T. ) ;
#14393 = CARTESIAN_POINT ( 'NONE',  ( -7.468086116107294004, -12.33868914344945189, -1.199999999999999956 ) ) ;
#14394 = CARTESIAN_POINT ( 'NONE',  ( -96.32500000000001705, 92.29496732002878900, 78.46416666666667084 ) ) ;
#14395 = VECTOR ( 'NONE', #62957, 999.9999999999998863 ) ;
#14396 = CARTESIAN_POINT ( 'NONE',  ( 10.00000000000000000, 35.95386929396241271, 10.96151621346552751 ) ) ;
#14397 = VECTOR ( 'NONE', #66864, 1000.000000000000000 ) ;
#14398 = LINE ( 'NONE', #14019, #3708 ) ;
#14399 = CARTESIAN_POINT ( 'NONE',  ( 93.84685191531251292, -211.9973110713294489, 75.14364583420046984 ) ) ;
#14400 = ORIENTED_EDGE ( 'NONE', *, *, #52524, .F. ) ;
#14401 = DIRECTION ( 'NONE',  ( 0.000000000000000000, 0.3090169943749461745, -0.9510565162951539753 ) ) ;
#14402 = PLANE ( 'NONE',  #69131 ) ;
#14403 = ORIENTED_EDGE ( 'NONE', *, *, #28881, .T. ) ;
#14404 = DIRECTION ( 'NONE',  ( -1.000000000000000000, -0.000000000000000000, -0.000000000000000000 ) ) ;
#14405 = ORIENTED_EDGE ( 'NONE', *, *, #3770, .F. ) ;
#14406 = EDGE_CURVE ( 'NONE', #71243, #54767, #6764, .T. ) ;
#14407 = EDGE_CURVE ( 'NONE', #35421, #47282, #45528, .T. ) ;
#14408 = LINE ( 'NONE', #31691, #7006 ) ;
#14409 = CIRCLE ( 'NONE', #38412, 82.00000000000000000 ) ;
#14410 = EDGE_CURVE ( 'NONE', #43104, #35072, #33266, .T. ) ;
#14411 = ORIENTED_EDGE ( 'NONE', *, *, #49563, .T. ) ;
#14412 = EDGE_LOOP ( 'NONE', ( #46804, #43486, #8720, #43854 ) ) ;
#14414 = ORIENTED_EDGE ( 'NONE', *, *, #46092, .T. ) ;
#14413 = EDGE_CURVE ( 'NONE', #2294, #39621, #51201, .T. ) ;
#14415 = AXIS2_PLACEMENT_3D ( 'NONE', #57959, #22639, #63242 ) ;
#14416 = EDGE_LOOP ( 'NONE', ( #50515, #58161, #49177, #48301 ) ) ;
#14417 = CARTESIAN_POINT ( 'NONE',  ( 97.65000000000000568, -208.4700217866474645, 76.47979166840096354 ) ) ;
#14418 = ORIENTED_EDGE ( 'NONE', *, *, #30918, .F. ) ;
#14420 = ADVANCED_FACE ( 'NONE', ( #63925 ), #18049, .T. ) ;
#14419 = ORIENTED_EDGE ( 'NONE', *, *, #43238, .T. ) ;
#14421 = CARTESIAN_POINT ( 'NONE',  ( 92.69370383062498320, 88.66845928578037217, 79.69447916753381378 ) ) ;
#14422 = FACE_OUTER_BOUND ( 'NONE', #50569, .T. ) ;
#14423 = DIRECTION ( 'NONE',  ( -8.090853898039828715E-17, 9.269810975720166919E-17, -1.000000000000000000 ) ) ;
#14424 = ORIENTED_EDGE ( 'NONE', *, *, #54405, .T. ) ;
#14425 = ORIENTED_EDGE ( 'NONE', *, *, #39291, .F. ) ;
#14426 = VERTEX_POINT ( 'NONE', #7140 ) ;
#14427 = DIRECTION ( 'NONE',  ( 0.000000000000000000, 0.9781476007338065770, 0.2079116908177544853 ) ) ;
#14428 = ORIENTED_EDGE ( 'NONE', *, *, #55658, .T. ) ;
#14429 = DIRECTION ( 'NONE',  ( 0.8513098556990980059, 0.5246632535156059429, 0.000000000000000000 ) ) ;
#14430 = LINE ( 'NONE', #24971, #7907 ) ;
#14431 = CARTESIAN_POINT ( 'NONE',  ( 10.00000000000000000, 0.000000000000000000, 0.000000000000000000 ) ) ;
#14432 = CYLINDRICAL_SURFACE ( 'NONE', #44921, 2.649999999999985700 ) ;
#14433 = DIRECTION ( 'NONE',  ( 0.000000000000000000, 0.7071067811865437980, 0.7071067811865512365 ) ) ;
#14434 = DIRECTION ( 'NONE',  ( -1.000000000000000000, -0.000000000000000000, 0.000000000000000000 ) ) ;
#14435 = DIRECTION ( 'NONE',  ( -0.000000000000000000, 0.5877852522924796874, 0.8090169943749426773 ) ) ;
#14436 = CARTESIAN_POINT ( 'NONE',  ( -97.64999999999994884, -208.4700217866474645, 75.42145833506764063 ) ) ;
#14437 = DIRECTION ( 'NONE',  ( -1.000000000000000000, -0.000000000000000000, -0.000000000000000000 ) ) ;
#14438 = ORIENTED_EDGE ( 'NONE', *, *, #38173, .T. ) ;
#14440 = CARTESIAN_POINT ( 'NONE',  ( -95.00000000000002842, 87.33691857156074434, 87.89656250086713385 ) ) ;
#14439 = CARTESIAN_POINT ( 'NONE',  ( 93.67499999999999716, 87.70503267997126784, 74.94520833506761903 ) ) ;
#14441 = EDGE_LOOP ( 'NONE', ( #68414, #686, #11629, #48567 ) ) ;
#14442 = CARTESIAN_POINT ( 'NONE',  ( 97.30629616937498838, 88.66845928578037217, 75.46114583420049371 ) ) ;
#14443 = DIRECTION ( 'NONE',  ( 0.000000000000000000, 0.000000000000000000, 1.000000000000000000 ) ) ;
#14444 = CARTESIAN_POINT ( 'NONE',  ( 0.000000000000000000, 30.00120703465205452, 22.64427369931179967 ) ) ;
#14445 = CARTESIAN_POINT ( 'NONE',  ( 14.09999999999999964, 0.000000000000000000, 0.000000000000000000 ) ) ;
#14446 = DIRECTION ( 'NONE',  ( -1.000000000000000000, 0.000000000000000000, 0.000000000000000000 ) ) ;
#14447 = DIRECTION ( 'NONE',  ( 1.000000000000000000, 0.000000000000000000, 0.000000000000000000 ) ) ;
#14448 = AXIS2_PLACEMENT_3D ( 'NONE', #20581, #60442, #32950 ) ;
#14449 = VERTEX_POINT ( 'NONE', #29674 ) ;
#14450 = DIRECTION ( 'NONE',  ( 0.000000000000000000, 0.000000000000000000, 1.000000000000000000 ) ) ;
#14451 = CIRCLE ( 'NONE', #15635, 35.50000000000000711 ) ;
#14452 = ADVANCED_FACE ( 'NONE', ( #24074 ), #30055, .T. ) ;
#14453 = EDGE_CURVE ( 'NONE', #59274, #32004, #69186, .T. ) ;
#14454 = CARTESIAN_POINT ( 'NONE',  ( 94.99999999999998579, 90.00000000000002842, 90.00000000000000000 ) ) ;
#14455 = ORIENTED_EDGE ( 'NONE', *, *, #42612, .T. ) ;
#14456 = ORIENTED_EDGE ( 'NONE', *, *, #38128, .F. ) ;
#14457 = VECTOR ( 'NONE', #67527, 1000.000000000000000 ) ;
#14458 = CARTESIAN_POINT ( 'NONE',  ( 114.1267819554180392, -82.91796067500511924, 5.500000000000000000 ) ) ;
#14459 = EDGE_CURVE ( 'NONE', #420, #12638, #62114, .T. ) ;
#14460 = DIRECTION ( 'NONE',  ( -1.000000000000000000, -0.000000000000000000, -0.000000000000000000 ) ) ;
#14461 = CARTESIAN_POINT ( 'NONE',  ( 97.64999999999999147, -209.9999999999999716, 89.68250000000000455 ) ) ;
#14462 = CARTESIAN_POINT ( 'NONE',  ( -96.32500000000001705, 87.70503267997129626, 76.21520833506762926 ) ) ;
#14463 = DIRECTION ( 'NONE',  ( -1.000000000000000000, -0.000000000000000000, -0.000000000000000000 ) ) ;
#14464 = EDGE_LOOP ( 'NONE', ( #51956, #8044, #6990, #43743 ) ) ;
#14465 = AXIS2_PLACEMENT_3D ( 'NONE', #29152, #46458, #47837 ) ;
#14466 = DIRECTION ( 'NONE',  ( 0.000000000000000000, 0.000000000000000000, 1.000000000000000000 ) ) ;
#14467 = CIRCLE ( 'NONE', #25259, 31.99999999999998579 ) ;
#14468 = AXIS2_PLACEMENT_3D ( 'NONE', #25175, #30426, #71019 ) ;
#14469 = CARTESIAN_POINT ( 'NONE',  ( 11.99999999999999822, 0.000000000000000000, 0.000000000000000000 ) ) ;
#14470 = CARTESIAN_POINT ( 'NONE',  ( 0.000000000000000000, -2.956366410621191765, 75.11725578898467859 ) ) ;
#14471 = DIRECTION ( 'NONE',  ( -1.000000000000000000, 0.000000000000000000, 0.000000000000000000 ) ) ;
#14472 = DIRECTION ( 'NONE',  ( 0.4796670183876317051, -0.8774505977381971134, 0.000000000000000000 ) ) ;
#14473 = CARTESIAN_POINT ( 'NONE',  ( 0.000000000000000000, 0.000000000000000000, -40.00000000000000000 ) ) ;
#14474 = UNCERTAINTY_MEASURE_WITH_UNIT (LENGTH_MEASURE( 1.000000000000000082E-05 ), #49830, 'distance_accuracy_value', 'NONE');
#14475 = CARTESIAN_POINT ( 'NONE',  ( 0.000000000000000000, 0.000000000000000000, 0.000000000000000000 ) ) ;
#14476 = CIRCLE ( 'NONE', #34870, 77.49899999999999523 ) ;
#14477 = DIRECTION ( 'NONE',  ( 0.000000000000000000, 0.5000000000000039968, -0.8660254037844363761 ) ) ;
#14478 = CARTESIAN_POINT ( 'NONE',  ( 92.69370383062498320, 88.66845928578035796, 85.40947916753381719 ) ) ;
#14479 = CARTESIAN_POINT ( 'NONE',  ( -92.69370383062498320, -211.3315407142195852, 81.81114583420048803 ) ) ;
#14480 = CYLINDRICAL_SURFACE ( 'NONE', #20642, 16.00000000000000000 ) ;
#14481 = ORIENTED_EDGE ( 'NONE', *, *, #63107, .F. ) ;
#14482 = CARTESIAN_POINT ( 'NONE',  ( 92.35000000000000853, -209.9999999999999716, 90.00000000000000000 ) ) ;
#14483 = CARTESIAN_POINT ( 'NONE',  ( -92.34999999999999432, -209.9999999999999716, 79.52249999999999375 ) ) ;
#14484 = CARTESIAN_POINT ( 'NONE',  ( 12.74955575014928399, 0.001194404169505926478, -70.59999999999966747 ) ) ;
#14485 = CARTESIAN_POINT ( 'NONE',  ( 96.15314808468748708, -208.0026889286704943, 84.35114583420048007 ) ) ;
#14486 = EDGE_LOOP ( 'NONE', ( #46630, #51730, #45149, #3351 ) ) ;
#14487 = DIRECTION ( 'NONE',  ( -1.000000000000000000, -0.000000000000000000, -0.000000000000000000 ) ) ;
#14488 = VERTEX_POINT ( 'NONE', #63188 ) ;
#14489 = ORIENTED_EDGE ( 'NONE', *, *, #19612, .T. ) ;
#14490 = CIRCLE ( 'NONE', #68563, 77.49899999999999523 ) ;
#14492 = CIRCLE ( 'NONE', #55340, 82.00000000000000000 ) ;
#14491 = DIRECTION ( 'NONE',  ( 1.000000000000000000, -0.000000000000000000, -0.000000000000000000 ) ) ;
#14493 = EDGE_CURVE ( 'NONE', #48711, #41355, #17674, .T. ) ;
#14494 = ORIENTED_EDGE ( 'NONE', *, *, #55798, .T. ) ;
#14495 = EDGE_CURVE ( 'NONE', #21534, #53485, #60920, .T. ) ;
#14496 = CARTESIAN_POINT ( 'NONE',  ( 93.84685191531249870, -208.0026889286704943, 78.90072916753382515 ) ) ;
#14497 = FACE_OUTER_BOUND ( 'NONE', #8510, .T. ) ;
#14498 = LINE ( 'NONE', #47986, #48420 ) ;
#14499 = DIRECTION ( 'NONE',  ( 0.000000000000000000, 0.8090169943749487835, -0.5877852522924713607 ) ) ;
#14500 = CARTESIAN_POINT ( 'NONE',  ( 10.00000000000000000, 0.000000000000000000, 0.000000000000000000 ) ) ;
#14501 = EDGE_CURVE ( 'NONE', #49698, #59084, #36438, .T. ) ;
#14502 = DIRECTION ( 'NONE',  ( -1.000000000000000000, 0.000000000000000000, -0.000000000000000000 ) ) ;
#14503 = CARTESIAN_POINT ( 'NONE',  ( 97.64999999999997726, -208.4700217866474645, 80.21041666666666003 ) ) ;
#14504 = CIRCLE ( 'NONE', #61323, 11.59999999999999787 ) ;
#14505 = ORIENTED_EDGE ( 'NONE', *, *, #46211, .F. ) ;
#14506 = ORIENTED_EDGE ( 'NONE', *, *, #24464, .F. ) ;
#14507 = ORIENTED_EDGE ( 'NONE', *, *, #41446, .T. ) ;
#14508 = ORIENTED_EDGE ( 'NONE', *, *, #70452, .T. ) ;
#14509 = CARTESIAN_POINT ( 'NONE',  ( 0.000000000000000000, 8.830959090342393125, 74.65491531819122883 ) ) ;
#14510 = AXIS2_PLACEMENT_3D ( 'NONE', #27288, #33683, #17140 ) ;
#14511 = AXIS2_PLACEMENT_3D ( 'NONE', #22589, #10551, #28216 ) ;
#14512 = FILL_AREA_STYLE_COLOUR ( '', #15948 ) ;
#14513 = CARTESIAN_POINT ( 'NONE',  ( -97.30629616937501680, 91.33154071421968467, 84.03364583420049883 ) ) ;
#14514 = DIRECTION ( 'NONE',  ( -1.000000000000000000, -0.000000000000000000, -0.000000000000000000 ) ) ;
#14515 = VECTOR ( 'NONE', #39833, 1000.000000000000000 ) ;
#14516 = DIRECTION ( 'NONE',  ( 0.5687579148473752566, -0.8225049752423786442, 0.000000000000000000 ) ) ;
#14517 = CARTESIAN_POINT ( 'NONE',  ( 15.00000000000000000, 16.83928648764945635, 16.46020748918027010 ) ) ;
#14518 = ADVANCED_FACE ( 'NONE', ( #71747 ), #59383, .F. ) ;
#14519 = CARTESIAN_POINT ( 'NONE',  ( 0.000000000000000000, -22.67460108101783334, 6.353146135317912169 ) ) ;
#14520 = ORIENTED_EDGE ( 'NONE', *, *, #52609, .F. ) ;
#14521 = CARTESIAN_POINT ( 'NONE',  ( -96.32499999999996021, -207.7050326799711968, 87.43354166840096298 ) ) ;
#14522 = ORIENTED_EDGE ( 'NONE', *, *, #51676, .T. ) ;
#14523 = ADVANCED_FACE ( 'NONE', ( #20252, #7871, #31908, #65404, #30788, #8238, #59018, #70636, #14246, #8983, #7511, #1908, #13135, #71012, #41712, #54845, #24792 ), #42464, .F. ) ;
#14524 = DIRECTION ( 'NONE',  ( -0.000000000000000000, 0.9945218953682731788, 0.1045284632676559550 ) ) ;
#14525 = ORIENTED_EDGE ( 'NONE', *, *, #25215, .T. ) ;
#14526 = CARTESIAN_POINT ( 'NONE',  ( -95.00000000000002842, 86.94004357329504273, 82.61812500173428475 ) ) ;
#14527 =( BOUNDED_CURVE ( )  B_SPLINE_CURVE ( 2, ( #21505, #9125, #4994, #14765, #3515, #10233, #73004 ),
 .UNSPECIFIED., .F., .F. ) 
 B_SPLINE_CURVE_WITH_KNOTS ( ( 3, 2, 2, 3 ),
 ( 0.8890265259358467453, 0.8960822236920598094, 0.9031379892329426395, 0.9101937466091533091 ),
 .UNSPECIFIED. ) 
 CURVE ( )  GEOMETRIC_REPRESENTATION_ITEM ( )  RATIONAL_B_SPLINE_CURVE ( ( 0.9999974258394870308, 0.8660266908770603012, 1.000000000000000000, 0.8660254037844387076, 1.000000000000000000, 0.8660254037844387076, 1.000000000000000000 ) ) 
 REPRESENTATION_ITEM ( '' )  );
#14528 = VERTEX_POINT ( 'NONE', #31168 ) ;
#14529 = CARTESIAN_POINT ( 'NONE',  ( 94.99999999999998579, 92.66308142843935514, 87.10281250086715943 ) ) ;
#14530 = DIRECTION ( 'NONE',  ( 0.000000000000000000, -0.7071067811865389130, -0.7071067811865563435 ) ) ;
#14531 = CARTESIAN_POINT ( 'NONE',  ( 26.09152095774781799, -124.8716048804687375, 5.500000000000000000 ) ) ;
#14532 = DIRECTION ( 'NONE',  ( -1.000000000000000000, 0.000000000000000000, 0.000000000000000000 ) ) ;
#14533 = CARTESIAN_POINT ( 'NONE',  ( 97.64999999999999147, 90.00000000000002842, 89.04749999999999943 ) ) ;
#14534 = DIRECTION ( 'NONE',  ( -1.000000000000000000, -0.000000000000000000, 0.000000000000000000 ) ) ;
#14535 = ORIENTED_EDGE ( 'NONE', *, *, #2017, .F. ) ;
#14536 = CARTESIAN_POINT ( 'NONE',  ( 93.67500000000001137, -207.7050326799711968, 77.82916666666665151 ) ) ;
#14537 = EDGE_CURVE ( 'NONE', #6061, #44704, #17624, .T. ) ;
#14538 = ADVANCED_FACE ( 'NONE', ( #3008 ), #53366, .T. ) ;
#14539 = CARTESIAN_POINT ( 'NONE',  ( 0.000000000000000000, 65.58780272294076497, 36.73666225445916211 ) ) ;
#14540 = ORIENTED_EDGE ( 'NONE', *, *, #46870, .F. ) ;
#14541 = EDGE_LOOP ( 'NONE', ( #13662, #68437, #51240, #17508 ) ) ;
#14542 = DIRECTION ( 'NONE',  ( 0.000000000000000000, -0.9876883405951359940, -0.1564344650402420822 ) ) ;
#14543 = PRODUCT ( 'ISO 5597-32-4-5_GB_SEALS_TYPE1 32X4X5 L1', 'ISO 5597-32-4-5_GB_SEALS_TYPE1 32X4X5 L1', '', ( #22675 ) ) ;
#14544 = CARTESIAN_POINT ( 'NONE',  ( 10.00000000000000000, -79.10210256391383155, 21.60688246758557796 ) ) ;
#14545 = CARTESIAN_POINT ( 'NONE',  ( -93.67499999999998295, -212.2949673200287179, 83.22666666666665947 ) ) ;
#14546 = CARTESIAN_POINT ( 'NONE',  ( -94.99999999999997158, -207.3369185715606307, 83.92781250086716227 ) ) ;
#14547 = ORIENTED_EDGE ( 'NONE', *, *, #73847, .T. ) ;
#14548 = LINE ( 'NONE', #15288, #65711 ) ;
#14549 = VERTEX_POINT ( 'NONE', #18772 ) ;
#14550 = COLOUR_RGB ( '', 0.40784314, 0.44705882, 0.49803922) ;
#14551 = CIRCLE ( 'NONE', #62561, 15.99999999999999645 ) ;
#14552 = CARTESIAN_POINT ( 'NONE',  ( -8.000000000000021316, -1.510451465605151834E-13, -13.10000000000024301 ) ) ;
#14553 = DIRECTION ( 'NONE',  ( -1.000000000000000000, -0.000000000000000000, -0.000000000000000000 ) ) ;
#14554 = VECTOR ( 'NONE', #60975, 1000.000000000000000 ) ;
#14555 = DIRECTION ( 'NONE',  ( 1.000000000000000000, 0.000000000000000000, 0.000000000000000000 ) ) ;
#14556 = CARTESIAN_POINT ( 'NONE',  ( 96.15314808468748708, 88.00268892867053694, 77.78947916753381264 ) ) ;
#14557 = CARTESIAN_POINT ( 'NONE',  ( 0.000000000000000000, 0.000000000000000000, 0.000000000000000000 ) ) ;
#14558 = FACE_OUTER_BOUND ( 'NONE', #43845, .T. ) ;
#14559 = CARTESIAN_POINT ( 'NONE',  ( 0.000000000000000000, 75.16055320797030959, 18.89407956138283851 ) ) ;
#14560 = FACE_OUTER_BOUND ( 'NONE', #14897, .T. ) ;
#14561 = DIRECTION ( 'NONE',  ( -1.000000000000000000, -0.000000000000000000, -0.000000000000000000 ) ) ;
#14562 = CYLINDRICAL_SURFACE ( 'NONE', #44185, 15.50000000000000000 ) ;
#14563 = DIRECTION ( 'NONE',  ( -1.000000000000000000, -0.000000000000000000, 0.000000000000000000 ) ) ;
#14564 = PRODUCT_DEFINITION_CONTEXT ( 'detailed design', #63796, 'design' ) ;
#14565 = CARTESIAN_POINT ( 'NONE',  ( 11.99999999999999822, 0.000000000000000000, 0.000000000000000000 ) ) ;
#14566 = EDGE_LOOP ( 'NONE', ( #58695, #27286 ) ) ;
#14567 = CARTESIAN_POINT ( 'NONE',  ( -97.30629616937501680, 91.33154071421968467, 83.23989583420048177 ) ) ;
#14568 = VECTOR ( 'NONE', #67437, 1000.000000000000000 ) ;
#14569 = DIRECTION ( 'NONE',  ( 0.000000000000000000, -1.181994176819165452E-15, -1.000000000000000000 ) ) ;
#14570 = CIRCLE ( 'NONE', #24197, 77.49899999999999523 ) ;
#14571 = VECTOR ( 'NONE', #73933, 1000.000000000000114 ) ;
#14572 = EDGE_CURVE ( 'NONE', #1262, #9715, #20482, .T. ) ;
#14573 = DIRECTION ( 'NONE',  ( 0.000000000000000000, -0.9945218953682742891, -0.1045284632676449360 ) ) ;
#14574 = EDGE_CURVE ( 'NONE', #13012, #49856, #42097, .T. ) ;
#14575 = VERTEX_POINT ( 'NONE', #64650 ) ;
#14576 = CIRCLE ( 'NONE', #20595, 16.00000000000000000 ) ;
#14577 = DIRECTION ( 'NONE',  ( 0.000000000000000000, 0.000000000000000000, -1.000000000000000000 ) ) ;
#14578 = CARTESIAN_POINT ( 'NONE',  ( -92.35000000000674447, -209.9999940177768565, 82.14187520865739600 ) ) ;
#14579 = CARTESIAN_POINT ( 'NONE',  ( 50.00005079999999680, 0.000000000000000000, 0.000000000000000000 ) ) ;
#14580 = ADVANCED_FACE ( 'NONE', ( #36807 ), #68121, .T. ) ;
#14581 = CARTESIAN_POINT ( 'NONE',  ( 95.00000000000000000, -207.3369185715606307, 79.48281250086715488 ) ) ;
#14582 = EDGE_CURVE ( 'NONE', #23968, #9432, #71831, .T. ) ;
#14583 = ORIENTED_EDGE ( 'NONE', *, *, #38776, .F. ) ;
#14584 = EDGE_LOOP ( 'NONE', ( #36641, #54995, #32960, #32339 ) ) ;
#14585 = ADVANCED_FACE ( 'NONE', ( #37932 ), #66866, .T. ) ;
#14586 = CARTESIAN_POINT ( 'NONE',  ( 10.00000000000000000, -41.91543099594816368, -2.663952781846588014 ) ) ;
#14587 = DIRECTION ( 'NONE',  ( 0.000000000000000000, -0.3826834323650772363, -0.9238795325112919565 ) ) ;
#14588 = DIRECTION ( 'NONE',  ( 0.000000000000000000, 0.000000000000000000, -1.000000000000000000 ) ) ;
#14589 = EDGE_CURVE ( 'NONE', #13574, #23135, #35686, .T. ) ;
#14590 = EDGE_LOOP ( 'NONE', ( #44751, #44787, #46509, #57175 ) ) ;
#14591 = CARTESIAN_POINT ( 'NONE',  ( 93.84685191531249870, -208.0026889286704943, 75.09072916753380866 ) ) ;
#14592 = PRESENTATION_LAYER_ASSIGNMENT (  '', '', ( #47033 ) ) ;
#14593 = VECTOR ( 'NONE', #60605, 1000.000000000000000 ) ;
#14594 = VERTEX_POINT ( 'NONE', #15355 ) ;
#14595 = B_SPLINE_CURVE_WITH_KNOTS ( 'NONE', 3,
 ( #2926, #18688, #43132, #42013, #48380, #70549, #60058, #59297 ),
 .UNSPECIFIED., .F., .F.,
 ( 4, 2, 2, 4 ),
 ( 0.002921158011986708155, 0.003648658599403065313, 0.004376159186819422037, 0.005831160361652136352 ),
 .UNSPECIFIED. ) ;
#14596 = DIRECTION ( 'NONE',  ( -1.000000000000000000, 0.000000000000000000, 0.000000000000000000 ) ) ;
#14597 = EDGE_LOOP ( 'NONE', ( #20445, #16365, #37571, #54692 ) ) ;
#14598 = ORIENTED_EDGE ( 'NONE', *, *, #40302, .F. ) ;
#14599 = FACE_OUTER_BOUND ( 'NONE', #10074, .T. ) ;
#14600 = VECTOR ( 'NONE', #34622, 1000.000000000000000 ) ;
#14601 = LINE ( 'NONE', #72109, #64159 ) ;
#14602 = EDGE_LOOP ( 'NONE', ( #15250, #46334, #44092, #51040 ) ) ;
#14603 = DIRECTION ( 'NONE',  ( 1.000000000000000000, 0.000000000000000000, 0.000000000000000000 ) ) ;
#14604 = CARTESIAN_POINT ( 'NONE',  ( 97.64999999999997726, -211.5299782133524502, 79.54895833506762415 ) ) ;
#14605 = CARTESIAN_POINT ( 'NONE',  ( 97.64999999999999147, 90.00000000000002842, 84.60249999999999204 ) ) ;
#14606 = ADVANCED_FACE ( 'NONE', ( #55216 ), #32645, .T. ) ;
#14607 = VERTEX_POINT ( 'NONE', #38299 ) ;
#14608 = CARTESIAN_POINT ( 'NONE',  ( 11.99999999999999822, 0.000000000000000000, 0.000000000000000000 ) ) ;
#14609 = VECTOR ( 'NONE', #10004, 1000.000000000000227 ) ;
#14610 = EDGE_CURVE ( 'NONE', #58705, #31970, #39422, .T. ) ;
#14611 = DIRECTION ( 'NONE',  ( 0.000000000000000000, 0.000000000000000000, 1.000000000000000000 ) ) ;
#14612 = VERTEX_POINT ( 'NONE', #73243 ) ;
#14613 = ORIENTED_EDGE ( 'NONE', *, *, #42902, .T. ) ;
#14614 = CARTESIAN_POINT ( 'NONE',  ( -95.00000000000002842, 87.33691857156074434, 88.05531250086714579 ) ) ;
#14615 = CARTESIAN_POINT ( 'NONE',  ( 92.69370383062498320, 88.66845928578037217, 83.34572916753380412 ) ) ;
#14616 = VERTEX_POINT ( 'NONE', #3370 ) ;
#14617 = CARTESIAN_POINT ( 'NONE',  ( 92.34999999999999432, 91.52997821335252127, 82.40645833506762585 ) ) ;
#14618 = CARTESIAN_POINT ( 'NONE',  ( 10.00000000000000000, 0.000000000000000000, 0.000000000000000000 ) ) ;
#14619 = ORIENTED_EDGE ( 'NONE', *, *, #2671, .F. ) ;
#14620 = CARTESIAN_POINT ( 'NONE',  ( 96.32499999999998863, -207.7050326799711968, 87.32770833506762642 ) ) ;
#14621 = VECTOR ( 'NONE', #13253, 1000.000000000000000 ) ;
#14622 = VERTEX_POINT ( 'NONE', #49200 ) ;
#14623 = VECTOR ( 'NONE', #43857, 1000.000000000000114 ) ;
#14624 = EDGE_LOOP ( 'NONE', ( #36265, #56426, #55287, #4108 ) ) ;
#14625 = ORIENTED_EDGE ( 'NONE', *, *, #15694, .F. ) ;
#14626 = LINE ( 'NONE', #38592, #25318 ) ;
#14627 = AXIS2_PLACEMENT_3D ( 'NONE', #60731, #72711, #73093 ) ;
#14628 = CARTESIAN_POINT ( 'NONE',  ( 0.000000000000000000, -32.34446384429951138, -26.79245525562750530 ) ) ;
#14629 = CARTESIAN_POINT ( 'NONE',  ( -93.67500000000003979, 87.70503267997129626, 85.76666666666665151 ) ) ;
#14630 = ORIENTED_EDGE ( 'NONE', *, *, #48541, .F. ) ;
#14631 = DIRECTION ( 'NONE',  ( 0.000000000000000000, 0.000000000000000000, 1.000000000000000000 ) ) ;
#14632 = CARTESIAN_POINT ( 'NONE',  ( 92.34999999999999432, 91.52997821335252127, 88.12145833506762926 ) ) ;
#14633 = ORIENTED_EDGE ( 'NONE', *, *, #56745, .F. ) ;
#14634 = DIRECTION ( 'NONE',  ( 1.000000000000000000, 0.000000000000000000, 0.000000000000000000 ) ) ;
#14635 = CARTESIAN_POINT ( 'NONE',  ( -96.15314808468747287, -208.0026889286704943, 80.01197916753380923 ) ) ;
#14636 = VERTEX_POINT ( 'NONE', #55591 ) ;
#14637 = LINE ( 'NONE', #13154, #71048 ) ;
#14638 = DIRECTION ( 'NONE',  ( 1.000000000000000000, 0.000000000000000000, 0.000000000000000000 ) ) ;
#14639 = CARTESIAN_POINT ( 'NONE',  ( 95.00000000000000000, -209.9999999999999716, 90.00000000000000000 ) ) ;
#14640 = LINE ( 'NONE', #32663, #1508 ) ;
#14641 = DIRECTION ( 'NONE',  ( 0.000000000000000000, -0.3826834323650970537, 0.9238795325112838519 ) ) ;
#14642 = CARTESIAN_POINT ( 'NONE',  ( 0.000000000000000000, 69.42325613327489009, -34.44570377933524696 ) ) ;
#14643 = CARTESIAN_POINT ( 'NONE',  ( 92.69370383062498320, 90.00000000000002842, 87.10281250086714522 ) ) ;
#14644 = PLANE ( 'NONE',  #32794 ) ;
#14645 = DIRECTION ( 'NONE',  ( -1.000000000000000000, -0.000000000000000000, 0.000000000000000000 ) ) ;
#14646 = DIRECTION ( 'NONE',  ( -7.943659481576819828E-16, -1.065814103640131188E-14, -1.000000000000000000 ) ) ;
#14647 = DIRECTION ( 'NONE',  ( 0.000000000000000000, -0.8090169943749531134, 0.5877852522924653655 ) ) ;
#14648 = DIRECTION ( 'NONE',  ( 0.000000000000000000, 0.000000000000000000, -1.000000000000000000 ) ) ;
#14649 = CARTESIAN_POINT ( 'NONE',  ( 11.99999999999999822, 0.000000000000000000, 0.000000000000000000 ) ) ;
#14650 = CARTESIAN_POINT ( 'NONE',  ( 2.500000000000003109, -4.330127018922192761, -6.000000000000000000 ) ) ;
#14651 = EDGE_CURVE ( 'NONE', #9220, #33472, #16109, .T. ) ;
#14652 =( GEOMETRIC_REPRESENTATION_CONTEXT ( 3 ) GLOBAL_UNCERTAINTY_ASSIGNED_CONTEXT ( ( #48865 ) ) GLOBAL_UNIT_ASSIGNED_CONTEXT ( ( #23668, #47342, #18755 ) ) REPRESENTATION_CONTEXT ( 'NONE', 'WORKASPACE' ) );
#14653 = AXIS2_PLACEMENT_3D ( 'NONE', #61256, #33396, #3752 ) ;
#14654 = CARTESIAN_POINT ( 'NONE',  ( 2.500000000000032419, 80.00000000000000000, -279.9999999999999432 ) ) ;
#14655 = CARTESIAN_POINT ( 'NONE',  ( 92.69370383062498320, 90.00000000000002842, 89.80156250086714920 ) ) ;
#14656 = CARTESIAN_POINT ( 'NONE',  ( 95.39412261730194587, 87.35656277621939125, 75.00000000000001421 ) ) ;
#14657 = AXIS2_PLACEMENT_3D ( 'NONE', #18352, #51836, #1119 ) ;
#14658 = CARTESIAN_POINT ( 'NONE',  ( 7.400000000000003908, 1.056673655987569448E-14, 5.892267102770835596E-15 ) ) ;
#14659 = CARTESIAN_POINT ( 'NONE',  ( -96.32499999999996021, -212.2949673200287179, 87.56583333333333030 ) ) ;
#14660 = EDGE_CURVE ( 'NONE', #63551, #55642, #70505, .T. ) ;
#14661 = ADVANCED_FACE ( 'NONE', ( #61244 ), #21746, .F. ) ;
#14662 = VECTOR ( 'NONE', #69017, 1000.000000000000114 ) ;
#14663 = DIRECTION ( 'NONE',  ( -0.000000000000000000, -0.000000000000000000, 1.000000000000000000 ) ) ;
#14664 = AXIS2_PLACEMENT_3D ( 'NONE', #8903, #10008, #21271 ) ;
#14665 = ORIENTED_EDGE ( 'NONE', *, *, #30383, .F. ) ;
#14666 = CARTESIAN_POINT ( 'NONE',  ( 10.00000000000000000, 36.13751322684419165, 21.40280677340384230 ) ) ;
#14667 = CARTESIAN_POINT ( 'NONE',  ( 0.000000000000000000, 0.000000000000000000, 0.000000000000000000 ) ) ;
#14668 = CARTESIAN_POINT ( 'NONE',  ( 93.67500000000001137, -207.7050326799711968, 81.71854166840095957 ) ) ;
#14669 = ADVANCED_FACE ( 'NONE', ( #44700 ), #39049, .T. ) ;
#14670 = DIRECTION ( 'NONE',  ( 0.000000000000000000, -0.5000000000000011102, -0.8660254037844380415 ) ) ;
#14671 = VECTOR ( 'NONE', #36324, 1000.000000000000000 ) ;
#14672 = AXIS2_PLACEMENT_3D ( 'NONE', #16761, #11115, #613 ) ;
#14673 = EDGE_LOOP ( 'NONE', ( #36273, #60285, #20639, #34896 ) ) ;
#14674 = ORIENTED_EDGE ( 'NONE', *, *, #2678, .F. ) ;
#14675 = CARTESIAN_POINT ( 'NONE',  ( 7.893099573151324044, -11.68370571044642503, 0.000000000000000000 ) ) ;
#14676 = DIRECTION ( 'NONE',  ( -0.000000000000000000, -0.000000000000000000, -1.000000000000000000 ) ) ;
#14677 = VERTEX_POINT ( 'NONE', #49938 ) ;
#14678 = CARTESIAN_POINT ( 'NONE',  ( 92.69370383062501162, -209.9999999999999716, 80.11781250086713158 ) ) ;
#14679 = CARTESIAN_POINT ( 'NONE',  ( 93.84685191531251292, -211.9973110713294489, 84.82739583420048746 ) ) ;
#14680 = EDGE_CURVE ( 'NONE', #56976, #71434, #24855, .T. ) ;
#14681 = VERTEX_POINT ( 'NONE', #21355 ) ;
#14682 = CARTESIAN_POINT ( 'NONE',  ( 93.84685191531249870, -208.0026889286704943, 85.88572916753381037 ) ) ;
#14683 = ORIENTED_EDGE ( 'NONE', *, *, #32683, .F. ) ;
#14684 = PLANE ( 'NONE',  #41850 ) ;
#14685 = VERTEX_POINT ( 'NONE', #33384 ) ;
#14686 = CARTESIAN_POINT ( 'NONE',  ( -93.84685191531252713, 88.00268892867056536, 76.67822916753381435 ) ) ;
#14687 = ORIENTED_EDGE ( 'NONE', *, *, #73907, .F. ) ;
#14688 = VERTEX_POINT ( 'NONE', #27762 ) ;
#14689 = FACE_OUTER_BOUND ( 'NONE', #13318, .T. ) ;
#14690 = ORIENTED_EDGE ( 'NONE', *, *, #1742, .F. ) ;
#14691 = DIRECTION ( 'NONE',  ( -1.000000000000000000, -0.000000000000000000, -0.000000000000000000 ) ) ;
#14692 = DIRECTION ( 'NONE',  ( 0.000000000000000000, 0.4539904997395477482, -0.8910065241883674547 ) ) ;
#14693 = EDGE_CURVE ( 'NONE', #16267, #11059, #61608, .T. ) ;
#14694 = ORIENTED_EDGE ( 'NONE', *, *, #12230, .T. ) ;
#14695 = DIRECTION ( 'NONE',  ( 1.000000000000000000, 0.000000000000000000, 0.000000000000000000 ) ) ;
#14696 = EDGE_CURVE ( 'NONE', #20114, #61214, #44080, .T. ) ;
#14697 = VERTEX_POINT ( 'NONE', #22124 ) ;
#14698 = DIRECTION ( 'NONE',  ( -1.000000000000000000, 0.000000000000000000, 0.000000000000000000 ) ) ;
#14699 = EDGE_CURVE ( 'NONE', #15522, #27844, #10095, .T. ) ;
#14700 = ORIENTED_EDGE ( 'NONE', *, *, #21617, .F. ) ;
#14701 = ORIENTED_EDGE ( 'NONE', *, *, #12463, .T. ) ;
#14702 = VERTEX_POINT ( 'NONE', #55962 ) ;
#14703 = CARTESIAN_POINT ( 'NONE',  ( 95.00000000000000000, -207.3369185715606307, 78.68906250086713783 ) ) ;
#14704 = CYLINDRICAL_SURFACE ( 'NONE', #27337, 3.299999999999983391 ) ;
#14705 = CONTEXT_DEPENDENT_SHAPE_REPRESENTATION ( #24913, #13911 ) ;
#14706 = CARTESIAN_POINT ( 'NONE',  ( 0.000000000000000000, -35.95386929396248377, -10.96151621346525751 ) ) ;
#14707 = VERTEX_POINT ( 'NONE', #72130 ) ;
#14708 = VERTEX_POINT ( 'NONE', #14989 ) ;
#14709 = CARTESIAN_POINT ( 'NONE',  ( -92.35000000000003695, 90.00000000000004263, 80.79249999999998977 ) ) ;
#14710 = VERTEX_POINT ( 'NONE', #9346 ) ;
#14711 = CARTESIAN_POINT ( 'NONE',  ( -92.34999999999999432, -209.9999999999999716, 84.60249999999999204 ) ) ;
#14712 = FACE_OUTER_BOUND ( 'NONE', #7522, .T. ) ;
#14713 = CARTESIAN_POINT ( 'NONE',  ( -96.15314808468752972, 91.99731107132950569, 78.90072916753382515 ) ) ;
#14714 = AXIS2_PLACEMENT_3D ( 'NONE', #9563, #71215, #49035 ) ;
#14715 = EDGE_LOOP ( 'NONE', ( #27363, #35156, #31069, #34452 ) ) ;
#14716 = CARTESIAN_POINT ( 'NONE',  ( 92.69370383062498320, 88.66845928578037217, 78.26572916753380582 ) ) ;
#14717 = VECTOR ( 'NONE', #45787, 1000.000000000000114 ) ;
#14718 = VERTEX_POINT ( 'NONE', #32270 ) ;
#14719 = DIRECTION ( 'NONE',  ( 0.000000000000000000, 0.000000000000000000, 1.000000000000000000 ) ) ;
#14720 = CARTESIAN_POINT ( 'NONE',  ( 12.00000000000000000, -0.9646360437372099028, 23.52805723605590771 ) ) ;
#14721 = CARTESIAN_POINT ( 'NONE',  ( 96.90829729882861443, 88.16127723153182671, 74.99954709728268654 ) ) ;
#14722 = CYLINDRICAL_SURFACE ( 'NONE', #52332, 31.99999999999999289 ) ;
#14723 = DIRECTION ( 'NONE',  ( 0.000000000000000000, 0.5877852522924743583, -0.8090169943749466741 ) ) ;
#14724 = CARTESIAN_POINT ( 'NONE',  ( -97.30629616937497417, -211.3315407142195852, 82.71072916753378479 ) ) ;
#14725 = LINE ( 'NONE', #59871, #34972 ) ;
#14726 = FACE_OUTER_BOUND ( 'NONE', #44858, .T. ) ;
#14727 = AXIS2_PLACEMENT_3D ( 'NONE', #26104, #49037, #13350 ) ;
#14728 = CARTESIAN_POINT ( 'NONE',  ( 11.99999999999999822, -14.67089635893764665, 73.72996012237435082 ) ) ;
#14729 = VERTEX_POINT ( 'NONE', #63843 ) ;
#14730 = AXIS2_PLACEMENT_3D ( 'NONE', #16217, #27494, #55704 ) ;
#14731 = ORIENTED_EDGE ( 'NONE', *, *, #17146, .T. ) ;
#14732 = CARTESIAN_POINT ( 'NONE',  ( 0.000000000000000000, 65.59268652807210742, 36.72794159290264560 ) ) ;
#14733 = LINE ( 'NONE', #66618, #60371 ) ;
#14734 = CARTESIAN_POINT ( 'NONE',  ( 11.99999999999999822, 77.32052557432849937, -5.256550761632002633 ) ) ;
#14735 = CARTESIAN_POINT ( 'NONE',  ( -95.00000000000002842, 92.66308142843932671, 86.30906250086715659 ) ) ;
#14736 = DIRECTION ( 'NONE',  ( -0.000000000000000000, -0.000000000000000000, -1.000000000000000000 ) ) ;
#14737 = PLANE ( 'NONE',  #35014 ) ;
#14738 = VERTEX_POINT ( 'NONE', #6329 ) ;
#14739 = DIRECTION ( 'NONE',  ( 0.000000000000000000, 0.000000000000000000, -1.000000000000000000 ) ) ;
#14740 = EDGE_CURVE ( 'NONE', #19443, #34985, #66309, .T. ) ;
#14741 = CARTESIAN_POINT ( 'NONE',  ( -94.99999999999997158, -213.0599564267049857, 85.15812500173429100 ) ) ;
#14742 = DIRECTION ( 'NONE',  ( -1.000000000000000000, -0.000000000000000000, 0.000000000000000000 ) ) ;
#14743 = DIRECTION ( 'NONE',  ( 1.000000000000000000, 0.000000000000000000, 0.000000000000000000 ) ) ;
#14744 = DIRECTION ( 'NONE',  ( 0.000000000000000000, -0.5877852522924624790, -0.8090169943749550008 ) ) ;
#14745 = DIRECTION ( 'NONE',  ( 0.000000000000000000, 0.9135454576426003115, 0.4067366430758017071 ) ) ;
#14746 = CARTESIAN_POINT ( 'NONE',  ( 94.99999999999998579, 90.00000000000002842, 90.00000000000000000 ) ) ;
#14747 = CARTESIAN_POINT ( 'NONE',  ( -94.99999999999997158, -212.6630814284392557, 82.34031250086714238 ) ) ;
#14748 = FILL_AREA_STYLE ('',( #36950 ) ) ;
#14749 = EDGE_CURVE ( 'NONE', #69181, #39875, #11571, .T. ) ;
#14750 = EDGE_CURVE ( 'NONE', #52748, #47732, #23982, .T. ) ;
#14751 = CARTESIAN_POINT ( 'NONE',  ( 96.32499999999998863, 87.70503267997126784, 76.32104166840096582 ) ) ;
#14752 =( BOUNDED_CURVE ( )  B_SPLINE_CURVE ( 2, ( #20008, #42966, #14381, #63982, #22644, #12093, #11710 ),
 .UNSPECIFIED., .F., .F. ) 
 B_SPLINE_CURVE_WITH_KNOTS ( ( 3, 2, 2, 3 ),
 ( 0.4656806970056963091, 0.4727362912391187555, 0.4797920567800010860, 0.4868478063929145838 ),
 .UNSPECIFIED. ) 
 CURVE ( )  GEOMETRIC_REPRESENTATION_ITEM ( )  RATIONAL_B_SPLINE_CURVE ( ( 0.9999934945994379820, 0.8660286565636942102, 1.000000000000000000, 0.8660254037844387076, 1.000000000000000000, 0.8660254037844387076, 1.000000000000000000 ) ) 
 REPRESENTATION_ITEM ( '' )  );
#14753 = FACE_OUTER_BOUND ( 'NONE', #62720, .T. ) ;
#14754 = DIRECTION ( 'NONE',  ( 0.000000000000000000, 0.000000000000000000, 1.000000000000000000 ) ) ;
#14755 = CARTESIAN_POINT ( 'NONE',  ( -97.65000000000001990, 90.00000000000004263, 88.73000000000000398 ) ) ;
#14756 = ORIENTED_EDGE ( 'NONE', *, *, #35303, .F. ) ;
#14757 = EDGE_CURVE ( 'NONE', #13857, #21073, #58184, .T. ) ;
#14758 = AXIS2_PLACEMENT_3D ( 'NONE', #23867, #18949, #7321 ) ;
#14759 = CARTESIAN_POINT ( 'NONE',  ( 92.35000000030105127, 90.00002455906435728, 87.53856274002153270 ) ) ;
#14760 = DIRECTION ( 'NONE',  ( 1.000000000000000000, -0.000000000000000000, -0.000000000000000000 ) ) ;
#14761 = CARTESIAN_POINT ( 'NONE',  ( 92.35000000000003695, -208.4700217866474929, 79.78708333333331382 ) ) ;
#14762 = AXIS2_PLACEMENT_3D ( 'NONE', #31872, #20220, #43563 ) ;
#14763 = CARTESIAN_POINT ( 'NONE',  ( 0.000000000000000000, 0.000000000000000000, 0.000000000000000000 ) ) ;
#14764 = VERTEX_POINT ( 'NONE', #12681 ) ;
#14765 = CARTESIAN_POINT ( 'NONE',  ( -95.00000000000002842, 93.05995642670504253, 75.95062500173428077 ) ) ;
#14766 = CARTESIAN_POINT ( 'NONE',  ( 10.00000000000000000, -38.55633173627023069, 16.65560815589396526 ) ) ;
#14767 = EDGE_CURVE ( 'NONE', #67442, #27250, #46536, .T. ) ;
#14768 = ORIENTED_EDGE ( 'NONE', *, *, #71339, .F. ) ;
#14769 = AXIS2_PLACEMENT_3D ( 'NONE', #23567, #19029, #20134 ) ;
#14770 = DIRECTION ( 'NONE',  ( 0.000000000000000000, 0.000000000000000000, 1.000000000000000000 ) ) ;
#14771 = AXIS2_PLACEMENT_3D ( 'NONE', #63602, #42879, #36115 ) ;
#14772 = EDGE_CURVE ( 'NONE', #71840, #53791, #57826, .T. ) ;
#14773 = ORIENTED_EDGE ( 'NONE', *, *, #64593, .F. ) ;
#14774 = ORIENTED_EDGE ( 'NONE', *, *, #14147, .F. ) ;
#14775 = VECTOR ( 'NONE', #61631, 1000.000000000000000 ) ;
#14776 = CARTESIAN_POINT ( 'NONE',  ( 11.99999999999999822, -71.91182617369207719, 28.89263327155721228 ) ) ;
#14777 = CIRCLE ( 'NONE', #1630, 82.00000000000000000 ) ;
#14778 = ORIENTED_EDGE ( 'NONE', *, *, #45680, .F. ) ;
#14779 = ORIENTED_EDGE ( 'NONE', *, *, #32489, .T. ) ;
#14780 = ORIENTED_EDGE ( 'NONE', *, *, #56544, .F. ) ;
#14781 = EDGE_LOOP ( 'NONE', ( #13929, #38070, #64097, #67670 ) ) ;
#14782 = DIRECTION ( 'NONE',  ( -0.7533909544171996098, -0.6575728627325956310, 0.000000000000000000 ) ) ;
#14783 = EDGE_CURVE ( 'NONE', #51571, #42708, #17226, .T. ) ;
#14784 = VERTEX_POINT ( 'NONE', #52534 ) ;
#14785 = EDGE_CURVE ( 'NONE', #45184, #17672, #8357, .T. ) ;
#14786 = ORIENTED_EDGE ( 'NONE', *, *, #41200, .F. ) ;
#14787 = CARTESIAN_POINT ( 'NONE',  ( 92.69370383062498320, 88.66845928578037217, 76.51947916753381662 ) ) ;
#14788 = CARTESIAN_POINT ( 'NONE',  ( 11.99999999999999822, 0.000000000000000000, 0.000000000000000000 ) ) ;
#14789 = DIRECTION ( 'NONE',  ( -1.000000000000000000, -0.000000000000000000, 0.000000000000000000 ) ) ;
#14790 = ORIENTED_EDGE ( 'NONE', *, *, #9917, .T. ) ;
#14791 = EDGE_LOOP ( 'NONE', ( #35142, #1179, #53118, #45968 ) ) ;
#14792 = B_SPLINE_CURVE_WITH_KNOTS ( 'NONE', 3,
 ( #33467, #44777, #38010, #60943, #44403, #9434, #44029, #27458 ),
 .UNSPECIFIED., .F., .F.,
 ( 4, 2, 2, 4 ),
 ( 0.002921158011986722466, 0.003648658599403074854, 0.004376159186819426374, 0.005831160361652130281 ),
 .UNSPECIFIED. ) ;
#14793 = VERTEX_POINT ( 'NONE', #40161 ) ;
#14794 = CARTESIAN_POINT ( 'NONE',  ( 94.99999999999998579, 92.66308142843935514, 89.48406250086713953 ) ) ;
#14795 = EDGE_LOOP ( 'NONE', ( #54233, #68935 ) ) ;
#14796 = CARTESIAN_POINT ( 'NONE',  ( 92.69370383062501162, -208.6684592857803011, 89.58989583420047609 ) ) ;
#14797 = DIRECTION ( 'NONE',  ( 0.000000000000000000, 0.000000000000000000, -1.000000000000000000 ) ) ;
#14798 = CARTESIAN_POINT ( 'NONE',  ( 97.64999999999992042, 91.52997821335256390, 84.02041666666666231 ) ) ;
#14799 = CARTESIAN_POINT ( 'NONE',  ( -96.73564493164514033, 91.73956328105568048, 74.87701898318914573 ) ) ;
#14800 = CARTESIAN_POINT ( 'NONE',  ( 97.65000000000000568, 91.52997821335252127, 77.74979166840097378 ) ) ;
#14801 = CARTESIAN_POINT ( 'NONE',  ( 0.000000000000000000, 0.000000000000000000, -80.00000000000000000 ) ) ;
#14802 = CARTESIAN_POINT ( 'NONE',  ( -92.35000000000003695, 90.00000000000004263, 78.25249999999999773 ) ) ;
#14803 = DIRECTION ( 'NONE',  ( 0.000000000000000000, -0.8090169943749426773, 0.5877852522924796874 ) ) ;
#14804 = CARTESIAN_POINT ( 'NONE',  ( -97.64999999999994884, -211.5299782133524502, 76.16229166840095388 ) ) ;
#14805 = CARTESIAN_POINT ( 'NONE',  ( -95.00000000000002842, 92.66308142843932671, 89.64281250086715147 ) ) ;
#14806 = ORIENTED_EDGE ( 'NONE', *, *, #66333, .T. ) ;
#14807 =( REPRESENTATION_RELATIONSHIP ('NONE','NONE', #31117, #50888 ) REPRESENTATION_RELATIONSHIP_WITH_TRANSFORMATION ( #67702 )SHAPE_REPRESENTATION_RELATIONSHIP( ) );
#14808 = VECTOR ( 'NONE', #9289, 1000.000000000000000 ) ;
#14810 = CARTESIAN_POINT ( 'NONE',  ( -95.00000000000002842, 87.33691857156074434, 89.16656250086712987 ) ) ;
#14809 = CARTESIAN_POINT ( 'NONE',  ( 94.99999999999998579, 92.66308142843935514, 89.48406250086713953 ) ) ;
#14811 = ORIENTED_EDGE ( 'NONE', *, *, #10296, .T. ) ;
#14812 = CARTESIAN_POINT ( 'NONE',  ( 93.84685191531248449, 91.99731107132950569, 78.26572916753382003 ) ) ;
#14813 = CARTESIAN_POINT ( 'NONE',  ( 10.00000000000000000, -77.19088730480518734, -6.903761155838607166 ) ) ;
#14814 = LINE ( 'NONE', #60695, #3109 ) ;
#14815 = CARTESIAN_POINT ( 'NONE',  ( 96.32499999999997442, 92.29496732002878900, 82.24770833506762813 ) ) ;
#14816 = DIRECTION ( 'NONE',  ( -0.7273375899149812085, 0.6862798483830533369, 0.000000000000000000 ) ) ;
#14817 = LINE ( 'NONE', #26094, #52306 ) ;
#14818 = EDGE_LOOP ( 'NONE', ( #25946, #7494, #11013, #31869 ) ) ;
#14819 = LINE ( 'NONE', #42662, #196 ) ;
#14820 = DIRECTION ( 'NONE',  ( -1.000000000000000000, -0.000000000000000000, -0.000000000000000000 ) ) ;
#14821 = ORIENTED_EDGE ( 'NONE', *, *, #36645, .F. ) ;
#14822 = ORIENTED_EDGE ( 'NONE', *, *, #13400, .T. ) ;
#14823 = CARTESIAN_POINT ( 'NONE',  ( -92.35000000000005116, 91.52997821335253548, 81.48041666666665606 ) ) ;
#14824 = DIRECTION ( 'NONE',  ( 1.000000000000000000, 0.000000000000000000, 0.000000000000000000 ) ) ;
#14825 = CARTESIAN_POINT ( 'NONE',  ( -10.00000000000000000, 0.000000000000000000, 0.000000000000000000 ) ) ;
#14826 = CARTESIAN_POINT ( 'NONE',  ( 0.000000000000000000, 0.000000000000000000, -270.0000000000000000 ) ) ;
#14827 = CARTESIAN_POINT ( 'NONE',  ( 10.00000000000000000, 0.000000000000000000, 0.000000000000000000 ) ) ;
#14828 = CARTESIAN_POINT ( 'NONE',  ( 10.00000000000000000, 0.000000000000000000, 0.000000000000000000 ) ) ;
#14829 = DIRECTION ( 'NONE',  ( 1.000000000000000000, 0.000000000000000000, 0.000000000000000000 ) ) ;
#14830 = AXIS2_PLACEMENT_3D ( 'NONE', #51374, #60542, #17173 ) ;
#14831 = ORIENTED_EDGE ( 'NONE', *, *, #7468, .F. ) ;
#14832 = CARTESIAN_POINT ( 'NONE',  ( -96.15314808468751551, 88.00268892867056536, 82.12864583420046927 ) ) ;
#14833 = ADVANCED_FACE ( 'NONE', ( #68372 ), #11214, .F. ) ;
#14834 = FACE_OUTER_BOUND ( 'NONE', #71842, .T. ) ;
#14835 = AXIS2_PLACEMENT_3D ( 'NONE', #47213, #34823, #29527 ) ;
#14836 = CIRCLE ( 'NONE', #19601, 31.99999999999998579 ) ;
#14837 = AXIS2_PLACEMENT_3D ( 'NONE', #70484, #30281, #58486 ) ;
#14838 = LINE ( 'NONE', #37787, #60646 ) ;
#14839 = EDGE_CURVE ( 'NONE', #46085, #15234, #63958, .T. ) ;
#14840 = SURFACE_STYLE_USAGE ( .BOTH. , #71974 ) ;
#14841 = CARTESIAN_POINT ( 'NONE',  ( 0.000000000000000000, -71.87247863392386193, -39.47590169984923136 ) ) ;
#14842 = EDGE_CURVE ( 'NONE', #63432, #52407, #69108, .T. ) ;
#14843 = DIRECTION ( 'NONE',  ( -1.000000000000000000, 0.000000000000000000, 0.000000000000000000 ) ) ;
#14844 = CARTESIAN_POINT ( 'NONE',  ( -93.67499999999998295, -207.7050326799711968, 87.24833333333333485 ) ) ;
#14845 = CARTESIAN_POINT ( 'NONE',  ( -10.00000000000000000, 0.000000000000000000, 0.000000000000000000 ) ) ;
#14846 = EDGE_CURVE ( 'NONE', #62600, #20222, #23607, .T. ) ;
#14847 = FACE_OUTER_BOUND ( 'NONE', #19964, .T. ) ;
#14848 = DIRECTION ( 'NONE',  ( -1.000000000000000000, 0.000000000000000000, -0.000000000000000000 ) ) ;
#14849 = CARTESIAN_POINT ( 'NONE',  ( 97.30629616937498838, 88.66845928578035796, 79.27114583420048177 ) ) ;
#14850 = VECTOR ( 'NONE', #49935, 1000.000000000000000 ) ;
#14851 = CARTESIAN_POINT ( 'NONE',  ( -97.30629616937495996, -209.9999999999999716, 83.45156250086715488 ) ) ;
#14852 = CARTESIAN_POINT ( 'NONE',  ( 0.000000000000000000, 60.67117009219135326, 55.16347631943062169 ) ) ;
#14853 = ORIENTED_EDGE ( 'NONE', *, *, #68323, .T. ) ;
#14854 = ADVANCED_FACE ( 'NONE', ( #5595 ), #62747, .F. ) ;
#14855 = CARTESIAN_POINT ( 'NONE',  ( -25.50183398199384754, -112.6408924756582053, -5.500000000000000000 ) ) ;
#14856 = CARTESIAN_POINT ( 'NONE',  ( -93.67499999999998295, -212.2949673200287179, 76.87666666666666515 ) ) ;
#14857 = CARTESIAN_POINT ( 'NONE',  ( 0.000000000000000000, -41.76937507738831812, 62.50329211542423025 ) ) ;
#14858 = CARTESIAN_POINT ( 'NONE',  ( 92.69370383062501162, -209.9999999999999716, 82.65781250086713783 ) ) ;
#14859 = VERTEX_POINT ( 'NONE', #1090 ) ;
#14860 = VECTOR ( 'NONE', #68750, 1000.000000000000000 ) ;
#14861 = CARTESIAN_POINT ( 'NONE',  ( 96.76339072695074606, 88.50623689698961982, 74.79348190356851944 ) ) ;
#14862 = EDGE_CURVE ( 'NONE', #61671, #28369, #23115, .T. ) ;
#14863 = ORIENTED_EDGE ( 'NONE', *, *, #56899, .F. ) ;
#14864 = CARTESIAN_POINT ( 'NONE',  ( 6.377742925735834234, -145.7647898336708181, -5.500000000000000000 ) ) ;
#14865 = ADVANCED_FACE ( 'NONE', ( #46915 ), #34506, .T. ) ;
#14866 = ORIENTED_EDGE ( 'NONE', *, *, #25863, .F. ) ;
#14867 = DIRECTION ( 'NONE',  ( -0.000000000000000000, -0.000000000000000000, 1.000000000000000000 ) ) ;
#14868 = EDGE_CURVE ( 'NONE', #16620, #68748, #57452, .T. ) ;
#14869 = ADVANCED_FACE ( 'NONE', ( #51806 ), #24710, .F. ) ;
#14870 = AXIS2_PLACEMENT_3D ( 'NONE', #37640, #32710, #60932 ) ;
#14871 = ORIENTED_EDGE ( 'NONE', *, *, #8857, .F. ) ;
#14872 = CARTESIAN_POINT ( 'NONE',  ( 96.15314808468750130, -211.9973110713294489, 78.58322916753382970 ) ) ;
#14873 = CYLINDRICAL_SURFACE ( 'NONE', #68096, 82.00000000000000000 ) ;
#14874 = ADVANCED_FACE ( 'NONE', ( #14160 ), #20169, .T. ) ;
#14875 = FACE_OUTER_BOUND ( 'NONE', #9958, .T. ) ;
#14876 = VECTOR ( 'NONE', #17661, 1000.000000000000000 ) ;
#14877 = DIRECTION ( 'NONE',  ( -1.000000000000000000, 0.000000000000000000, -0.000000000000000000 ) ) ;
#14878 = CARTESIAN_POINT ( 'NONE',  ( 97.30629616937498838, 91.33154071421968467, 85.72697916753381264 ) ) ;
#14879 = CIRCLE ( 'NONE', #22079, 31.99999999999998934 ) ;
#14880 = CARTESIAN_POINT ( 'NONE',  ( 10.00000000000000000, -74.65374052328644439, -8.840884882375878107 ) ) ;
#14881 = CARTESIAN_POINT ( 'NONE',  ( 92.35000000000002274, -211.5299782133524502, 79.89291666666666458 ) ) ;
#14882 = VERTEX_POINT ( 'NONE', #1460 ) ;
#14883 = EDGE_CURVE ( 'NONE', #32014, #45965, #14595, .T. ) ;
#14884 = ORIENTED_EDGE ( 'NONE', *, *, #42050, .T. ) ;
#14885 = ORIENTED_EDGE ( 'NONE', *, *, #22577, .F. ) ;
#14886 = AXIS2_PLACEMENT_3D ( 'NONE', #46759, #47132, #29814 ) ;
#14887 = EDGE_LOOP ( 'NONE', ( #1059, #37295, #49547, #16345 ) ) ;
#14888 = DIRECTION ( 'NONE',  ( 0.000000000000000000, 0.000000000000000000, -1.000000000000000000 ) ) ;
#14889 = VECTOR ( 'NONE', #107, 1000.000000000000000 ) ;
#14890 = CARTESIAN_POINT ( 'NONE',  ( -96.15314808468751551, 88.00268892867056536, 85.46239583420047836 ) ) ;
#14891 = DIRECTION ( 'NONE',  ( -1.000000000000000000, 0.000000000000000000, 0.000000000000000000 ) ) ;
#14892 = DIRECTION ( 'NONE',  ( -1.000000000000000000, -0.000000000000000000, 0.000000000000000000 ) ) ;
#14893 = CARTESIAN_POINT ( 'NONE',  ( 10.00000000000000000, -10.96151621346514382, 35.95386929396252640 ) ) ;
#14894 = DIRECTION ( 'NONE',  ( 0.000000000000000000, 0.000000000000000000, -1.000000000000000000 ) ) ;
#14895 = ORIENTED_EDGE ( 'NONE', *, *, #10776, .F. ) ;
#14896 = CARTESIAN_POINT ( 'NONE',  ( -96.32499999999996021, -212.2949673200287179, 87.01020833506763097 ) ) ;
#14897 = EDGE_LOOP ( 'NONE', ( #31899, #46392, #30500, #48536 ) ) ;
#14898 = DIRECTION ( 'NONE',  ( -1.000000000000000000, -0.000000000000000000, -0.000000000000000000 ) ) ;
#14899 = ORIENTED_EDGE ( 'NONE', *, *, #3344, .T. ) ;
#14900 = CARTESIAN_POINT ( 'NONE',  ( -92.35000000000005116, 91.52997821335253548, 84.09979166840095388 ) ) ;
#14901 = ORIENTED_EDGE ( 'NONE', *, *, #10877, .T. ) ;
#14902 = CARTESIAN_POINT ( 'NONE',  ( 96.15314808468748708, 91.99731107132950569, 87.04989583420048405 ) ) ;
#14903 = LINE ( 'NONE', #54027, #59829 ) ;
#14904 = CARTESIAN_POINT ( 'NONE',  ( 2.184357737007946383E-12, -120.0000000000000000, -48.99999999999997158 ) ) ;
#14905 = AXIS2_PLACEMENT_3D ( 'NONE', #45626, #68548, #17033 ) ;
#14906 = LINE ( 'NONE', #25814, #2640 ) ;
#14907 = CARTESIAN_POINT ( 'NONE',  ( 25.44550000000002399, 3.673940397442060361E-16, -3.000000000000000444 ) ) ;
#14908 = CARTESIAN_POINT ( 'NONE',  ( -10.00000000000000000, 0.000000000000000000, 0.000000000000000000 ) ) ;
#14909 = EDGE_LOOP ( 'NONE', ( #35675, #56988, #15528, #61658 ) ) ;
#14910 = FACE_OUTER_BOUND ( 'NONE', #65668, .T. ) ;
#14911 = CARTESIAN_POINT ( 'NONE',  ( 0.000000000000000000, -37.01155633439053361, -6.555932627142825986 ) ) ;
#14912 = VERTEX_POINT ( 'NONE', #64567 ) ;
#14913 = ORIENTED_EDGE ( 'NONE', *, *, #57134, .T. ) ;
#14914 = DIRECTION ( 'NONE',  ( 1.000000000000000000, 0.000000000000000000, 0.000000000000000000 ) ) ;
#14915 = DIRECTION ( 'NONE',  ( 5.778480238264233142E-17, -1.000000000000000000, 0.000000000000000000 ) ) ;
#14916 = AXIS2_PLACEMENT_3D ( 'NONE', #42757, #65691, #60071 ) ;
#14917 = CYLINDRICAL_SURFACE ( 'NONE', #2932, 77.49899999999999523 ) ;
#14918 = CARTESIAN_POINT ( 'NONE',  ( -93.84685191531247028, -211.9973110713294489, 83.66322916753382799 ) ) ;
#14919 = VERTEX_POINT ( 'NONE', #19432 ) ;
#14920 = CYLINDRICAL_SURFACE ( 'NONE', #27315, 2.649999999999985700 ) ;
#14921 = ORIENTED_EDGE ( 'NONE', *, *, #215, .T. ) ;
#14922 = EDGE_CURVE ( 'NONE', #10184, #14708, #69940, .T. ) ;
#14923 = CARTESIAN_POINT ( 'NONE',  ( 11.99999999999999822, -75.16055320797043748, 18.89407956138231270 ) ) ;
#14924 = AXIS2_PLACEMENT_3D ( 'NONE', #34122, #57069, #50292 ) ;
#14925 = FACE_BOUND ( 'NONE', #55864, .T. ) ;
#14926 = EDGE_CURVE ( 'NONE', #64628, #46924, #66063, .T. ) ;
#14927 = CYLINDRICAL_SURFACE ( 'NONE', #60979, 32.00000000000000000 ) ;
#14928 = CARTESIAN_POINT ( 'NONE',  ( 96.15314808468748708, 88.00268892867053694, 78.42447916753381776 ) ) ;
#14929 = DIRECTION ( 'NONE',  ( -1.000000000000000000, 0.000000000000000000, 0.000000000000000000 ) ) ;
#14930 = CYLINDRICAL_SURFACE ( 'NONE', #37268, 16.00000000000000000 ) ;
#14931 = CARTESIAN_POINT ( 'NONE',  ( 0.000000000000000000, -14.67089635893658794, -73.72996012237454977 ) ) ;
#14932 = DIRECTION ( 'NONE',  ( 0.000000000000000000, 0.000000000000000000, 1.000000000000000000 ) ) ;
#14933 = ADVANCED_FACE ( 'NONE', ( #71295 ), #30707, .T. ) ;
#14935 = EDGE_CURVE ( 'NONE', #26601, #16458, #27874, .T. ) ;
#14934 = DIRECTION ( 'NONE',  ( 1.000000000000000000, 0.000000000000000000, -0.000000000000000000 ) ) ;
#14936 = DIRECTION ( 'NONE',  ( 0.000000000000000000, 0.9510565162951521989, 0.3090169943749515591 ) ) ;
#14937 = VECTOR ( 'NONE', #41611, 1000.000000000000000 ) ;
#14938 = VECTOR ( 'NONE', #14300, 1000.000000000000000 ) ;
#14939 = CARTESIAN_POINT ( 'NONE',  ( 0.000000000000000000, -80.28980883073747066, -16.65972982745017461 ) ) ;
#14940 = DIRECTION ( 'NONE',  ( -1.000000000000000000, 0.000000000000000000, -0.000000000000000000 ) ) ;
#14941 = ORIENTED_EDGE ( 'NONE', *, *, #389, .T. ) ;
#14942 = CIRCLE ( 'NONE', #28145, 82.00000000000000000 ) ;
#14943 = CARTESIAN_POINT ( 'NONE',  ( -95.00000000000002842, 92.66308142843932671, 82.49906250086715431 ) ) ;
#14944 = CIRCLE ( 'NONE', #40183, 82.00000000000000000 ) ;
#14945 = DIRECTION ( 'NONE',  ( 0.000000000000000000, 0.000000000000000000, 1.000000000000000000 ) ) ;
#14946 = EDGE_CURVE ( 'NONE', #50389, #72303, #69879, .T. ) ;
#14947 = AXIS2_PLACEMENT_3D ( 'NONE', #62100, #57202, #29347 ) ;
#14948 = ADVANCED_FACE ( 'NONE', ( #31454 ), #47283, .F. ) ;
#14949 = CARTESIAN_POINT ( 'NONE',  ( 11.99999999999999822, 30.41916302227216562, -71.27951684757994144 ) ) ;
#14950 = AXIS2_PLACEMENT_3D ( 'NONE', #37167, #31871, #43919 ) ;
#14951 = VERTEX_POINT ( 'NONE', #37110 ) ;
#14952 = FACE_OUTER_BOUND ( 'NONE', #12874, .T. ) ;
#14953 = DIRECTION ( 'NONE',  ( -0.000000000000000000, 0.1045284632676570929, -0.9945218953682730678 ) ) ;
#14954 = FACE_BOUND ( 'NONE', #27008, .T. ) ;
#14955 = AXIS2_PLACEMENT_3D ( 'NONE', #16106, #53459, #42192 ) ;
#14956 = CARTESIAN_POINT ( 'NONE',  ( 10.00000000000000000, 12.26510123303259725, 35.53030884539089840 ) ) ;
#14957 = EDGE_CURVE ( 'NONE', #1522, #65198, #25501, .T. ) ;
#14958 = EDGE_CURVE ( 'NONE', #58250, #73508, #25818, .T. ) ;
#14959 = CARTESIAN_POINT ( 'NONE',  ( 96.15314808468750130, -211.9973110713294489, 77.94822916753382458 ) ) ;
#14960 = ORIENTED_EDGE ( 'NONE', *, *, #24447, .F. ) ;
#14961 = EDGE_LOOP ( 'NONE', ( #17025, #62430, #44757, #58599 ) ) ;
#14962 = DIRECTION ( 'NONE',  ( 0.2306669878475637314, 0.9730327541852493711, 0.000000000000000000 ) ) ;
#14963 = CARTESIAN_POINT ( 'NONE',  ( 0.000000000000000000, 0.000000000000000000, 0.000000000000000000 ) ) ;
#14964 =( BOUNDED_CURVE ( )  B_SPLINE_CURVE ( 2, ( #59245, #1031, #1770, #46864, #58495, #24657, #6991 ),
 .UNSPECIFIED., .F., .F. ) 
 B_SPLINE_CURVE_WITH_KNOTS ( ( 3, 2, 2, 3 ),
 ( 0.5416666666666665186, 0.5486111111111110494, 0.5555555555555553582, 0.5624999999999997780 ),
 .UNSPECIFIED. ) 
 CURVE ( )  GEOMETRIC_REPRESENTATION_ITEM ( )  RATIONAL_B_SPLINE_CURVE ( ( 1.000000000000002220, 0.8660254037844365982, 1.000000000000000000, 0.8660254037844387076, 1.000000000000000000, 0.8660254037844430375, 0.9999999999999956701 ) ) 
 REPRESENTATION_ITEM ( '' )  );
#14965 = DIRECTION ( 'NONE',  ( 1.000000000000000000, 0.000000000000000000, 0.000000000000000000 ) ) ;
#14966 = PLANE ( 'NONE',  #5744 ) ;
#14967 = CARTESIAN_POINT ( 'NONE',  ( 97.30629616937498838, -209.9999999999999716, 74.87906250086714977 ) ) ;
#14968 = VERTEX_POINT ( 'NONE', #52920 ) ;
#14969 = CARTESIAN_POINT ( 'NONE',  ( -7.500000000000016875, -80.00000000000001421, -189.9999999999999147 ) ) ;
#14970 = VERTEX_POINT ( 'NONE', #58548 ) ;
#14971 = ORIENTED_EDGE ( 'NONE', *, *, #6722, .T. ) ;
#14972 = LINE ( 'NONE', #25150, #36982 ) ;
#14973 = CARTESIAN_POINT ( 'NONE',  ( -92.35000000000002274, 89.99997826787523536, 89.12687425009508502 ) ) ;
#14974 = ORIENTED_EDGE ( 'NONE', *, *, #3016, .T. ) ;
#14975 = LINE ( 'NONE', #37183, #28175 ) ;
#14976 = CARTESIAN_POINT ( 'NONE',  ( 97.64999999999999147, -209.9999999999999716, 78.96687500173429441 ) ) ;
#14977 = CARTESIAN_POINT ( 'NONE',  ( 92.34999999999999432, 88.47002178664753558, 86.87791666666664980 ) ) ;
#14978 = ORIENTED_EDGE ( 'NONE', *, *, #61916, .F. ) ;
#14979 = CYLINDRICAL_SURFACE ( 'NONE', #39492, 37.49900000000000233 ) ;
#14980 = CARTESIAN_POINT ( 'NONE',  ( 97.64999999999999147, 89.99999997928482287, 80.87187500099604165 ) ) ;
#14981 = ORIENTED_EDGE ( 'NONE', *, *, #73213, .F. ) ;
#14982 = LINE ( 'NONE', #33372, #45266 ) ;
#14983 = CARTESIAN_POINT ( 'NONE',  ( -95.00000000000002842, 87.33691857156074434, 84.24531250086717193 ) ) ;
#14984 = VECTOR ( 'NONE', #43995, 1000.000000000000000 ) ;
#14985 = CARTESIAN_POINT ( 'NONE',  ( 92.69370383062498320, 90.00000000000002842, 82.02281250086714692 ) ) ;
#14986 = VERTEX_POINT ( 'NONE', #31079 ) ;
#14987 = CYLINDRICAL_SURFACE ( 'NONE', #25246, 82.00000000000000000 ) ;
#14988 = ORIENTED_EDGE ( 'NONE', *, *, #66407, .F. ) ;
#14989 = CARTESIAN_POINT ( 'NONE',  ( 11.99999999999999822, -80.28980883073745645, -16.65972982745018172 ) ) ;
#14990 = EDGE_LOOP ( 'NONE', ( #13188, #56772, #32524, #47993 ) ) ;
#14991 = VERTEX_POINT ( 'NONE', #70930 ) ;
#14992 = VERTEX_POINT ( 'NONE', #36355 ) ;
#14993 = CARTESIAN_POINT ( 'NONE',  ( 6.000000000000000000, -21.60688246758530795, -79.10210256391388839 ) ) ;
#14994 = ORIENTED_EDGE ( 'NONE', *, *, #67580, .T. ) ;
#14995 = CYLINDRICAL_SURFACE ( 'NONE', #62363, 2.649999999999999467 ) ;
#14996 = DIRECTION ( 'NONE',  ( -1.000000000000000000, 0.000000000000000000, 0.000000000000000000 ) ) ;
#14997 = ORIENTED_EDGE ( 'NONE', *, *, #21278, .T. ) ;
#14998 = FACE_OUTER_BOUND ( 'NONE', #61959, .T. ) ;
#14999 = CARTESIAN_POINT ( 'NONE',  ( -92.69370383062498320, -209.9999999999999716, 79.80031250086713612 ) ) ;
#15000 = ORIENTED_EDGE ( 'NONE', *, *, #29671, .F. ) ;
#15001 = CARTESIAN_POINT ( 'NONE',  ( 10.00000000000000000, 54.21277698773752718, -55.38113227695725271 ) ) ;
#15002 = DIRECTION ( 'NONE',  ( -1.000000000000000000, 0.000000000000000000, 0.000000000000000000 ) ) ;
#15003 = DIRECTION ( 'NONE',  ( -1.000000000000000000, 0.000000000000000000, 0.000000000000000000 ) ) ;
#15004 = DIRECTION ( 'NONE',  ( -0.000000000000000000, -0.000000000000000000, 1.000000000000000000 ) ) ;
#15005 = CIRCLE ( 'NONE', #29478, 77.49900000000000944 ) ;
#15006 = EDGE_CURVE ( 'NONE', #32157, #33300, #7430, .T. ) ;
#15007 = ADVANCED_FACE ( 'NONE', ( #36724 ), #53285, .T. ) ;
#15008 = DIRECTION ( 'NONE',  ( 1.000000000000000000, 0.000000000000000000, -0.000000000000000000 ) ) ;
#15009 = EDGE_CURVE ( 'NONE', #45314, #21818, #8154, .T. ) ;
#15010 = FACE_OUTER_BOUND ( 'NONE', #5637, .T. ) ;
#15011 = CARTESIAN_POINT ( 'NONE',  ( 94.99999999999998579, 92.66308142843932671, 89.48406250086713953 ) ) ;
#15012 = CARTESIAN_POINT ( 'NONE',  ( -10.00000000000000000, 0.000000000000000000, 0.000000000000000000 ) ) ;
#15013 = CARTESIAN_POINT ( 'NONE',  ( 97.64999999999999147, 90.00000000000002842, 88.41249999999999432 ) ) ;
#15014 = CARTESIAN_POINT ( 'NONE',  ( -95.00000000000002842, 93.05995642670504253, 88.65062500173428361 ) ) ;
#15016 = ADVANCED_FACE ( 'NONE', ( #14910 ), #44613, .T. ) ;
#15015 = DIRECTION ( 'NONE',  ( 0.000000000000000000, 0.000000000000000000, 1.000000000000000000 ) ) ;
#15017 = CARTESIAN_POINT ( 'NONE',  ( 10.00000000000000000, -75.11725578898470701, 2.956366410620372864 ) ) ;
#15018 = CYLINDRICAL_SURFACE ( 'NONE', #21856, 31.99999999999998579 ) ;
#15019 = CARTESIAN_POINT ( 'NONE',  ( 10.00000000000000000, 27.13269053701096922, 25.88420570971410228 ) ) ;
#15020 = ADVANCED_FACE ( 'NONE', ( #72045 ), #26181, .T. ) ;
#15021 = CARTESIAN_POINT ( 'NONE',  ( 10.00000000000000000, -35.92658777277502935, -10.74501242461320594 ) ) ;
#15022 = FACE_OUTER_BOUND ( 'NONE', #66511, .T. ) ;
#15023 = AXIS2_PLACEMENT_3D ( 'NONE', #59281, #59653, #8136 ) ;
#15024 = LINE ( 'NONE', #45104, #4709 ) ;
#15025 = DIRECTION ( 'NONE',  ( -1.000000000000000000, -0.000000000000000000, -0.000000000000000000 ) ) ;
#15026 = CARTESIAN_POINT ( 'NONE',  ( -92.34999999999999432, -211.5299782133524502, 87.08958333333333712 ) ) ;
#15027 = EDGE_CURVE ( 'NONE', #14919, #35421, #41141, .T. ) ;
#15028 = CARTESIAN_POINT ( 'NONE',  ( -93.09170270117147084, 88.16127723153179829, 74.99954709728268654 ) ) ;
#15029 = EDGE_CURVE ( 'NONE', #49297, #63158, #60785, .T. ) ;
#15030 = ORIENTED_EDGE ( 'NONE', *, *, #43066, .F. ) ;
#15031 = VECTOR ( 'NONE', #18615, 1000.000000000000000 ) ;
#15032 = PLANE ( 'NONE',  #63545 ) ;
#15033 = CIRCLE ( 'NONE', #10212, 82.00000000000000000 ) ;
#15034 = CARTESIAN_POINT ( 'NONE',  ( 4.999999999999999112, 41.81611651403868990, -3.925862922255709542 ) ) ;
#15035 = CARTESIAN_POINT ( 'NONE',  ( -12.75000000000506617, -119.9999999999999005, 127.5000000000003411 ) ) ;
#15036 = CARTESIAN_POINT ( 'NONE',  ( 0.000000000000000000, 0.000000000000000000, -44.99999999999998579 ) ) ;
#15037 = AXIS2_PLACEMENT_3D ( 'NONE', #39752, #11527, #23197 ) ;
#15038 = EDGE_CURVE ( 'NONE', #40774, #4927, #42325, .T. ) ;
#15039 = EDGE_CURVE ( 'NONE', #24219, #60230, #24849, .T. ) ;
#15040 = ORIENTED_EDGE ( 'NONE', *, *, #55273, .F. ) ;
#15041 = VECTOR ( 'NONE', #62674, 1000.000000000000000 ) ;
#15042 = ORIENTED_EDGE ( 'NONE', *, *, #45187, .T. ) ;
#15043 = LINE ( 'NONE', #21411, #15485 ) ;
#15044 = LINE ( 'NONE', #21050, #28368 ) ;
#15045 = VERTEX_POINT ( 'NONE', #44979 ) ;
#15046 = CARTESIAN_POINT ( 'NONE',  ( 95.00000000000000000, -212.6630814284392557, 81.54656250086713953 ) ) ;
#15047 = CARTESIAN_POINT ( 'NONE',  ( 92.69370383062501162, -211.3315407142195852, 86.67947916753382742 ) ) ;
#15048 = ORIENTED_EDGE ( 'NONE', *, *, #52602, .F. ) ;
#15049 = CIRCLE ( 'NONE', #9043, 42.00000000000000000 ) ;
#15050 = CARTESIAN_POINT ( 'NONE',  ( 92.69370383062501162, -211.3315407142195852, 86.67947916753382742 ) ) ;
#15051 = VERTEX_POINT ( 'NONE', #16019 ) ;
#15052 = DIRECTION ( 'NONE',  ( 0.000000000000000000, 0.000000000000000000, 1.000000000000000000 ) ) ;
#15053 = ORIENTED_EDGE ( 'NONE', *, *, #55491, .T. ) ;
#15054 = CARTESIAN_POINT ( 'NONE',  ( -93.84685191531254134, 91.99731107132950569, 78.79489583420048859 ) ) ;
#15055 = ORIENTED_EDGE ( 'NONE', *, *, #63915, .F. ) ;
#15056 = AXIS2_PLACEMENT_3D ( 'NONE', #69238, #56492, #50460 ) ;
#15057 = ORIENTED_EDGE ( 'NONE', *, *, #40338, .F. ) ;
#15058 = CARTESIAN_POINT ( 'NONE',  ( 10.00000000000000000, 0.000000000000000000, 0.000000000000000000 ) ) ;
#15059 = ORIENTED_EDGE ( 'NONE', *, *, #14413, .T. ) ;
#15060 = CYLINDRICAL_SURFACE ( 'NONE', #31709, 82.00000000000000000 ) ;
#15061 = CARTESIAN_POINT ( 'NONE',  ( 11.99999999999999822, 58.39081064771822582, -50.95692526931267707 ) ) ;
#15062 = ORIENTED_EDGE ( 'NONE', *, *, #72806, .F. ) ;
#15063 = LINE ( 'NONE', #38001, #8187 ) ;
#15064 = ORIENTED_EDGE ( 'NONE', *, *, #72245, .F. ) ;
#15065 = DIRECTION ( 'NONE',  ( -1.000000000000000000, -0.000000000000000000, -0.000000000000000000 ) ) ;
#15066 = ORIENTED_EDGE ( 'NONE', *, *, #30282, .F. ) ;
#15067 = EDGE_CURVE ( 'NONE', #44704, #36890, #35832, .T. ) ;
#15068 = ORIENTED_EDGE ( 'NONE', *, *, #70796, .F. ) ;
#15069 = ORIENTED_EDGE ( 'NONE', *, *, #50238, .F. ) ;
#15070 = DIRECTION ( 'NONE',  ( 0.000000000000000000, 0.6494480483301793283, 0.7604059656000345946 ) ) ;
#15071 = ITEM_DEFINED_TRANSFORMATION ( 'NONE', 'NONE', #1605,  #43395 ) ;
#15072 = DIRECTION ( 'NONE',  ( -1.000000000000000000, 0.000000000000000000, 0.000000000000000000 ) ) ;
#15073 = VERTEX_POINT ( 'NONE', #44232 ) ;
#15074 = ORIENTED_EDGE ( 'NONE', *, *, #46776, .F. ) ;
#15076 = EDGE_CURVE ( 'NONE', #42748, #3975, #50726, .T. ) ;
#15075 = ORIENTED_EDGE ( 'NONE', *, *, #31320, .T. ) ;
#15077 = FACE_OUTER_BOUND ( 'NONE', #9431, .T. ) ;
#15078 = CARTESIAN_POINT ( 'NONE',  ( -0.7195005275814509993, -118.6838241033926948, 2.500000000000000000 ) ) ;
#15079 = ADVANCED_FACE ( 'NONE', ( #61158 ), #61899, .F. ) ;
#15080 = CARTESIAN_POINT ( 'NONE',  ( -93.84685191531254134, 91.99731107132950569, 79.42989583420049371 ) ) ;
#15081 = EDGE_LOOP ( 'NONE', ( #20545, #1712, #22785 ) ) ;
#15082 = CARTESIAN_POINT ( 'NONE',  ( 97.30629616937498838, 91.33154071421968467, 79.21822916753380639 ) ) ;
#15083 = ORIENTED_EDGE ( 'NONE', *, *, #59437, .F. ) ;
#15084 = CARTESIAN_POINT ( 'NONE',  ( -14.87942725330654348, -141.9795960975983178, 5.500000000000000000 ) ) ;
#15085 = CARTESIAN_POINT ( 'NONE',  ( -92.69370383062498320, -211.3315407142195852, 88.63739583420047552 ) ) ;
#15086 = CARTESIAN_POINT ( 'NONE',  ( 4.652319770550017886, -3.087484620012992398, -1.687189089856322655 ) ) ;
#15087 = VECTOR ( 'NONE', #67899, 1000.000000000000000 ) ;
#15088 = DIRECTION ( 'NONE',  ( -1.000000000000000000, -0.000000000000000000, 0.000000000000000000 ) ) ;
#15089 = CARTESIAN_POINT ( 'NONE',  ( 94.99999999999998579, 90.00000000000002842, 90.00000000000000000 ) ) ;
#15090 = CARTESIAN_POINT ( 'NONE',  ( -92.69370383062498320, -209.9999999999999716, 80.43531250086714124 ) ) ;
#15091 = EDGE_CURVE ( 'NONE', #36680, #65205, #60361, .T. ) ;
#15092 = CARTESIAN_POINT ( 'NONE',  ( 11.99999999999999822, 5.256550761633951296, -77.32052557432835727 ) ) ;
#15093 = DIRECTION ( 'NONE',  ( 0.000000000000000000, 0.000000000000000000, 1.000000000000000000 ) ) ;
#15094 = VECTOR ( 'NONE', #17849, 1000.000000000000000 ) ;
#15095 = FACE_OUTER_BOUND ( 'NONE', #38859, .T. ) ;
#15096 = VERTEX_POINT ( 'NONE', #10380 ) ;
#15097 = CIRCLE ( 'NONE', #58355, 31.99999999999998579 ) ;
#15098 = ORIENTED_EDGE ( 'NONE', *, *, #11069, .T. ) ;
#15099 = CARTESIAN_POINT ( 'NONE',  ( 0.000000000000000000, -51.03279382321125723, 55.19960302592048862 ) ) ;
#15100 = CIRCLE ( 'NONE', #12686, 82.00000000000000000 ) ;
#15101 = DIRECTION ( 'NONE',  ( -1.000000000000000000, 0.000000000000000000, 0.000000000000000000 ) ) ;
#15102 = LINE ( 'NONE', #26015, #60792 ) ;
#15103 = CARTESIAN_POINT ( 'NONE',  ( -97.30629616937501680, 88.66845928578038638, 85.25072916753379104 ) ) ;
#15104 = DIRECTION ( 'NONE',  ( 0.000000000000000000, 0.000000000000000000, 1.000000000000000000 ) ) ;
#15105 = PLANE ( 'NONE',  #1410 ) ;
#15106 = AXIS2_PLACEMENT_3D ( 'NONE', #68572, #50518, #10669 ) ;
#15107 = VECTOR ( 'NONE', #8359, 1000.000000000000000 ) ;
#15108 = ADVANCED_FACE ( 'NONE', ( #9268 ), #26923, .T. ) ;
#15109 = ORIENTED_EDGE ( 'NONE', *, *, #46280, .F. ) ;
#15110 = DIRECTION ( 'NONE',  ( -1.000000000000000000, 0.000000000000000000, 0.000000000000000000 ) ) ;
#15111 = CARTESIAN_POINT ( 'NONE',  ( 11.99999999999999822, 0.000000000000000000, 0.000000000000000000 ) ) ;
#15112 = CARTESIAN_POINT ( 'NONE',  ( 10.00000000000000000, -17.67226234102801286, -33.17418723428327354 ) ) ;
#15113 = CARTESIAN_POINT ( 'NONE',  ( 92.35000000049295465, 89.99996796756887818, 85.63541623677173220 ) ) ;
#15114 = LINE ( 'NONE', #2412, #9353 ) ;
#15115 = CIRCLE ( 'NONE', #37979, 42.00000000000000000 ) ;
#15116 = DIRECTION ( 'NONE',  ( 0.7273375899149793211, -0.6862798483830554463, 0.000000000000000000 ) ) ;
#15117 = CARTESIAN_POINT ( 'NONE',  ( -93.84685191531248449, -208.0026889286704943, 83.87489583420048689 ) ) ;
#15118 = EDGE_CURVE ( 'NONE', #56648, #21247, #67158, .T. ) ;
#15119 = DIRECTION ( 'NONE',  ( 0.000000000000000000, -0.9876883405951393247, 0.1564344650402205161 ) ) ;
#15120 = ADVANCED_FACE ( 'NONE', ( #33297 ), #32927, .F. ) ;
#15121 = EDGE_CURVE ( 'NONE', #55663, #69466, #13482, .T. ) ;
#15122 = LINE ( 'NONE', #72620, #44268 ) ;
#15123 = LINE ( 'NONE', #15497, #40599 ) ;
#15124 = PLANE ( 'NONE',  #35771 ) ;
#15125 = EDGE_LOOP ( 'NONE', ( #51783, #29233, #40967, #2461 ) ) ;
#15126 = CARTESIAN_POINT ( 'NONE',  ( 93.67499999999998295, 92.29496732002878900, 77.27354166840096639 ) ) ;
#15127 = DIRECTION ( 'NONE',  ( 0.000000000000000000, 1.000000000000000000, 3.491481338843133355E-15 ) ) ;
#15128 = CARTESIAN_POINT ( 'NONE',  ( 0.000000000000000000, -6.903761155837252694, -77.19088730480530103 ) ) ;
#15129 = DIRECTION ( 'NONE',  ( -0.000000000000000000, -0.5877852522924789103, 0.8090169943749432324 ) ) ;
#15130 = ORIENTED_EDGE ( 'NONE', *, *, #16841, .F. ) ;
#15131 = CARTESIAN_POINT ( 'NONE',  ( 97.64999999999999147, 90.00000000000002842, 78.25249999999999773 ) ) ;
#15132 = CYLINDRICAL_SURFACE ( 'NONE', #27069, 16.00000000000000000 ) ;
#15133 = ORIENTED_EDGE ( 'NONE', *, *, #64593, .T. ) ;
#15134 = LINE ( 'NONE', #73008, #29186 ) ;
#15135 = CARTESIAN_POINT ( 'NONE',  ( -93.67500000000003979, 92.29496732002878900, 77.72333333333332916 ) ) ;
#15136 = VECTOR ( 'NONE', #50118, 1000.000000000000000 ) ;
#15137 = ORIENTED_EDGE ( 'NONE', *, *, #13347, .F. ) ;
#15138 = CARTESIAN_POINT ( 'NONE',  ( -235.0000123116479926, -117.0000000000000142, -2.500000000000000000 ) ) ;
#15139 = ORIENTED_EDGE ( 'NONE', *, *, #11631, .F. ) ;
#15140 = DIRECTION ( 'NONE',  ( -1.000000000000000000, 0.000000000000000000, 0.000000000000000000 ) ) ;
#15141 = ORIENTED_EDGE ( 'NONE', *, *, #60280, .T. ) ;
#15142 = AXIS2_PLACEMENT_3D ( 'NONE', #33196, #21930, #27935 ) ;
#15143 = ORIENTED_EDGE ( 'NONE', *, *, #59160, .F. ) ;
#15144 = AXIS2_PLACEMENT_3D ( 'NONE', #63312, #52762, #46019 ) ;
#15145 = ORIENTED_EDGE ( 'NONE', *, *, #10303, .F. ) ;
#15146 = ORIENTED_EDGE ( 'NONE', *, *, #9834, .T. ) ;
#15147 = CYLINDRICAL_SURFACE ( 'NONE', #33538, 82.00000000000000000 ) ;
#15148 = EDGE_CURVE ( 'NONE', #8551, #57100, #65136, .T. ) ;
#15149 = VERTEX_POINT ( 'NONE', #34418 ) ;
#15150 = PRODUCT_DEFINITION_SHAPE ( 'NONE', 'NONE',  #56863 ) ;
#15151 = VECTOR ( 'NONE', #4966, 1000.000000000000000 ) ;
#15152 = CIRCLE ( 'NONE', #27162, 31.99999999999998579 ) ;
#15153 = EDGE_LOOP ( 'NONE', ( #11304, #67609, #5409, #53259 ) ) ;
#15154 = CARTESIAN_POINT ( 'NONE',  ( 97.30629616937498838, 91.33154071421968467, 76.83697916753382628 ) ) ;
#15155 = CARTESIAN_POINT ( 'NONE',  ( 95.00000000000000000, -209.9999999999999716, 90.00000000000000000 ) ) ;
#15156 = DIRECTION ( 'NONE',  ( -1.000000000000000000, 0.000000000000000000, 0.000000000000000000 ) ) ;
#15157 = VERTEX_POINT ( 'NONE', #17873 ) ;
#15158 = ORIENTED_EDGE ( 'NONE', *, *, #68261, .F. ) ;
#15159 = ORIENTED_EDGE ( 'NONE', *, *, #656, .F. ) ;
#15160 = DIRECTION ( 'NONE',  ( -1.000000000000000000, -0.000000000000000000, -0.000000000000000000 ) ) ;
#15161 = VERTEX_POINT ( 'NONE', #68279 ) ;
#15162 = CARTESIAN_POINT ( 'NONE',  ( 93.84685191531249870, -208.0026889286704943, 87.63197916753379957 ) ) ;
#15163 = DIRECTION ( 'NONE',  ( 0.000000000000000000, 0.000000000000000000, 1.000000000000000000 ) ) ;
#15164 = CARTESIAN_POINT ( 'NONE',  ( 0.000000000000000000, 0.000000000000000000, 0.000000000000000000 ) ) ;
#15165 = AXIS2_PLACEMENT_3D ( 'NONE', #37901, #37166, #25498 ) ;
#15166 = CARTESIAN_POINT ( 'NONE',  ( -92.34999999999996589, -208.4700217866474645, 80.21041666666666003 ) ) ;
#15167 = DIRECTION ( 'NONE',  ( 1.000000000000000000, -0.000000000000000000, -0.000000000000000000 ) ) ;
#15168 = LINE ( 'NONE', #56526, #691 ) ;
#15169 = EDGE_CURVE ( 'NONE', #4854, #13140, #19484, .T. ) ;
#15170 = CARTESIAN_POINT ( 'NONE',  ( 6.377742925735834234, -145.7647898336708181, 2.500000000000000000 ) ) ;
#15171 = DIRECTION ( 'NONE',  ( -1.000000000000000000, -0.000000000000000000, 0.000000000000000000 ) ) ;
#15172 = CARTESIAN_POINT ( 'NONE',  ( -94.99999999999997158, -213.0599564267049857, 74.99812500173430863 ) ) ;
#15173 = ADVANCED_FACE ( 'NONE', ( #11129 ), #40435, .F. ) ;
#15174 = CARTESIAN_POINT ( 'NONE',  ( 11.99999999999999822, 0.000000000000000000, 0.000000000000000000 ) ) ;
#15175 = ORIENTED_EDGE ( 'NONE', *, *, #33929, .F. ) ;
#15176 = UNCERTAINTY_MEASURE_WITH_UNIT (LENGTH_MEASURE( 1.000000000000000082E-05 ), #38524, 'distance_accuracy_value', 'NONE');
#15178 = CARTESIAN_POINT ( 'NONE',  ( -95.00000000000002842, 87.33691857156074434, 86.62656250086715204 ) ) ;
#15177 = CARTESIAN_POINT ( 'NONE',  ( 97.30629616937498838, 90.00000000000002842, 86.15031250086714465 ) ) ;
#15179 = ORIENTED_EDGE ( 'NONE', *, *, #28411, .F. ) ;
#15180 = DIRECTION ( 'NONE',  ( 0.000000000000000000, 1.000000000000000000, 0.000000000000000000 ) ) ;
#15181 = CARTESIAN_POINT ( 'NONE',  ( -97.64999999990722301, -209.9999861897314304, 80.55392363651652943 ) ) ;
#15182 = DIRECTION ( 'NONE',  ( 0.8225049752423786442, 0.5687579148473752566, -0.000000000000000000 ) ) ;
#15183 = DIRECTION ( 'NONE',  ( 1.000000000000000000, 0.000000000000000000, -0.000000000000000000 ) ) ;
#15184 = CARTESIAN_POINT ( 'NONE',  ( -92.69370383062498320, -208.6684592857803295, 88.74322916753382628 ) ) ;
#15185 = DIRECTION ( 'NONE',  ( -1.000000000000000000, 0.000000000000000000, 0.000000000000000000 ) ) ;
#15186 = EDGE_CURVE ( 'NONE', #19812, #67617, #11141, .T. ) ;
#15187 = EDGE_CURVE ( 'NONE', #9891, #30579, #50778, .T. ) ;
#15188 = LINE ( 'NONE', #27950, #242 ) ;
#15189 = DIRECTION ( 'NONE',  ( 1.000000000000000000, 0.000000000000000000, 0.000000000000000000 ) ) ;
#15190 = ORIENTED_EDGE ( 'NONE', *, *, #23134, .F. ) ;
#15191 = EDGE_LOOP ( 'NONE', ( #677, #14438, #15664, #45445 ) ) ;
#15192 = CARTESIAN_POINT ( 'NONE',  ( -97.65000000000001990, 90.00000000000004263, 79.83999999999998920 ) ) ;
#15193 = DIRECTION ( 'NONE',  ( 0.000000000000000000, 0.000000000000000000, 1.000000000000000000 ) ) ;
#15194 = DIRECTION ( 'NONE',  ( -0.000000000000000000, -0.000000000000000000, 1.000000000000000000 ) ) ;
#15195 = DIRECTION ( 'NONE',  ( -1.000000000000000000, -0.000000000000000000, -0.000000000000000000 ) ) ;
#15196 = CARTESIAN_POINT ( 'NONE',  ( 97.64997150697683992, 91.52999466380714466, 87.27479280632991276 ) ) ;
#15197 = CARTESIAN_POINT ( 'NONE',  ( 0.000000000000000000, 59.75363087400076267, 56.15606465354979093 ) ) ;
#15198 = CARTESIAN_POINT ( 'NONE',  ( 2.184357737007946383E-12, -120.0000000000000000, -48.99999999999997158 ) ) ;
#15199 =( BOUNDED_CURVE ( )  B_SPLINE_CURVE ( 2, ( #61175, #72431, #21291, #26940, #66443, #73176, #15677, #55149, #31474, #20934, #49868 ),
 .UNSPECIFIED., .F., .F. ) 
 B_SPLINE_CURVE_WITH_KNOTS ( ( 3, 2, 2, 2, 2, 3 ),
 ( 0.4233457466685775494, 0.4233459324529422196, 0.4304016979938244392, 0.4374574635347067142, 0.4445132290755889337, 0.4445132602971393343 ),
 .UNSPECIFIED. ) 
 CURVE ( )  GEOMETRIC_REPRESENTATION_ITEM ( )  RATIONAL_B_SPLINE_CURVE ( ( 0.9999929448534778942, 0.9999964723338524708, 1.000000000000000000, 0.8660254037844387076, 1.000000000000000000, 0.8660254037844387076, 1.000000000000000000, 0.8660254037844387076, 1.000000000000000000, 0.9999994071664397577, 0.9999988143381259853 ) ) 
 REPRESENTATION_ITEM ( '' )  );
#15200 = EDGE_CURVE ( 'NONE', #44494, #74057, #46086, .T. ) ;
#15201 = CIRCLE ( 'NONE', #57228, 31.99999999999999289 ) ;
#15202 = ORIENTED_EDGE ( 'NONE', *, *, #31482, .F. ) ;
#15203 = CARTESIAN_POINT ( 'NONE',  ( -97.30629616937501680, 90.00000000000004263, 82.65781250086713783 ) ) ;
#15204 = AXIS2_PLACEMENT_3D ( 'NONE', #2353, #71084, #60214 ) ;
#15205 = DIRECTION ( 'NONE',  ( -1.000000000000000000, 0.000000000000000000, -0.000000000000000000 ) ) ;
#15206 = DIRECTION ( 'NONE',  ( -1.000000000000000000, 0.000000000000000000, -0.000000000000000000 ) ) ;
#15207 = DIRECTION ( 'NONE',  ( -1.000000000000000000, 0.000000000000000000, 0.000000000000000000 ) ) ;
#15208 = VECTOR ( 'NONE', #58980, 1000.000000000000227 ) ;
#15209 = DIRECTION ( 'NONE',  ( -0.000000000000000000, -0.000000000000000000, -1.000000000000000000 ) ) ;
#15210 = DIRECTION ( 'NONE',  ( 0.000000000000000000, 0.8660254037844432595, -0.4999999999999919509 ) ) ;
#15211 = LINE ( 'NONE', #3960, #28629 ) ;
#15212 = CIRCLE ( 'NONE', #25993, 42.00000000000000000 ) ;
#15213 = DIRECTION ( 'NONE',  ( 0.000000000000000000, -0.5877852522924789103, 0.8090169943749432324 ) ) ;
#15214 = DIRECTION ( 'NONE',  ( 0.000000000000000000, 0.000000000000000000, 1.000000000000000000 ) ) ;
#15215 = EDGE_CURVE ( 'NONE', #19149, #61856, #43562, .T. ) ;
#15216 = EDGE_CURVE ( 'NONE', #9077, #20714, #28785, .T. ) ;
#15217 = EDGE_CURVE ( 'NONE', #60376, #62960, #64002, .T. ) ;
#15218 = AXIS2_PLACEMENT_3D ( 'NONE', #48129, #20282, #42131 ) ;
#15219 = CARTESIAN_POINT ( 'NONE',  ( 93.84685191531248449, 88.00268892867053694, 80.38239583420048007 ) ) ;
#15220 = CARTESIAN_POINT ( 'NONE',  ( -96.15314808468747287, -208.0026889286704943, 82.07572916753382231 ) ) ;
#15221 = LINE ( 'NONE', #9587, #54193 ) ;
#15222 = VERTEX_POINT ( 'NONE', #33682 ) ;
#15223 = CYLINDRICAL_SURFACE ( 'NONE', #17299, 16.00000000000000000 ) ;
#15224 = CARTESIAN_POINT ( 'NONE',  ( -96.32499999999996021, -212.2949673200287179, 78.04083333333333883 ) ) ;
#15225 = FACE_OUTER_BOUND ( 'NONE', #22176, .T. ) ;
#15226 = AXIS2_PLACEMENT_3D ( 'NONE', #8953, #60109, #14962 ) ;
#15227 = CARTESIAN_POINT ( 'NONE',  ( -92.69370383062504004, 90.00000000000004263, 78.68906250086715204 ) ) ;
#15228 = CARTESIAN_POINT ( 'NONE',  ( 92.69370383062501162, -208.6684592857803011, 83.23989583420046756 ) ) ;
#15229 = VERTEX_POINT ( 'NONE', #45734 ) ;
#15230 = AXIS2_PLACEMENT_3D ( 'NONE', #53538, #25703, #49369 ) ;
#15231 = DIRECTION ( 'NONE',  ( 0.000000000000000000, 0.9876883405951371042, 0.1564344650402346437 ) ) ;
#15232 = ORIENTED_EDGE ( 'NONE', *, *, #22071, .T. ) ;
#15233 = CARTESIAN_POINT ( 'NONE',  ( -3.000000000000000000, 16.61724383029390140, -20.69703378468903665 ) ) ;
#15234 = VERTEX_POINT ( 'NONE', #34802 ) ;
#15235 = CARTESIAN_POINT ( 'NONE',  ( -97.64999999992180335, 90.00001303125199570, 79.28395951162846700 ) ) ;
#15236 = ORIENTED_EDGE ( 'NONE', *, *, #41200, .T. ) ;
#15237 = ORIENTED_EDGE ( 'NONE', *, *, #36241, .F. ) ;
#15238 = CARTESIAN_POINT ( 'NONE',  ( 96.15314808468750130, -211.9973110713294489, 79.21822916753382060 ) ) ;
#15239 = DIRECTION ( 'NONE',  ( -1.000000000000000000, 0.000000000000000000, 0.000000000000000000 ) ) ;
#15240 = APPLICATION_CONTEXT ( 'automotive_design' ) ;
#15241 = CARTESIAN_POINT ( 'NONE',  ( -93.67500000000003979, 92.29496732002878900, 76.53270833506762472 ) ) ;
#15242 = EDGE_CURVE ( 'NONE', #68973, #39661, #27973, .T. ) ;
#15243 = CARTESIAN_POINT ( 'NONE',  ( -96.25799313133936153, 87.71227518788532507, 74.97309184317512631 ) ) ;
#15244 = CARTESIAN_POINT ( 'NONE',  ( 92.69370383062498320, 90.00000000000002842, 85.35656250086715602 ) ) ;
#15245 = VECTOR ( 'NONE', #73626, 1000.000000000000000 ) ;
#15246 = CARTESIAN_POINT ( 'NONE',  ( 95.04693102382854875, 87.35041560265749183, 75.00000002508419072 ) ) ;
#15247 = CARTESIAN_POINT ( 'NONE',  ( 92.35000000000000853, -209.9999999999999716, 83.01499999999998636 ) ) ;
#15248 = EDGE_CURVE ( 'NONE', #11372, #73020, #17139, .T. ) ;
#15249 = AXIS2_PLACEMENT_3D ( 'NONE', #27004, #43950, #4861 ) ;
#15250 = ORIENTED_EDGE ( 'NONE', *, *, #9187, .F. ) ;
#15251 = VERTEX_POINT ( 'NONE', #22409 ) ;
#15252 = ORIENTED_EDGE ( 'NONE', *, *, #31215, .T. ) ;
#15253 = ORIENTED_EDGE ( 'NONE', *, *, #5529, .T. ) ;
#15254 = CARTESIAN_POINT ( 'NONE',  ( 92.34999999999998010, -208.4700217866475214, 89.31208333333333371 ) ) ;
#15255 = EDGE_CURVE ( 'NONE', #71243, #23688, #45955, .T. ) ;
#15256 = CARTESIAN_POINT ( 'NONE',  ( -97.64999999999990621, -208.4700217866474077, 85.50208333333331723 ) ) ;
#15257 = VECTOR ( 'NONE', #30806, 1000.000000000000000 ) ;
#15258 = CARTESIAN_POINT ( 'NONE',  ( -93.67500000000003979, 87.70503267997129626, 82.03604166840096923 ) ) ;
#15259 = VECTOR ( 'NONE', #5491, 1000.000000000000000 ) ;
#15260 = CARTESIAN_POINT ( 'NONE',  ( 0.000000000000000000, -120.0000000000000000, 2.500000000000000000 ) ) ;
#15261 = EDGE_CURVE ( 'NONE', #5579, #49448, #25309, .T. ) ;
#15262 = DIRECTION ( 'NONE',  ( 1.000000000000000000, -7.677074106448950501E-15, -2.598394312951952234E-14 ) ) ;
#15263 = CARTESIAN_POINT ( 'NONE',  ( 0.000000000000000000, -33.71516098798793593, 74.74816331893418919 ) ) ;
#15264 = VERTEX_POINT ( 'NONE', #67011 ) ;
#15265 = CARTESIAN_POINT ( 'NONE',  ( -96.32499999999996021, -207.7050326799711968, 86.79854166840097207 ) ) ;
#15266 = ORIENTED_EDGE ( 'NONE', *, *, #54012, .F. ) ;
#15267 = LINE ( 'NONE', #60047, #13384 ) ;
#15268 = ORIENTED_EDGE ( 'NONE', *, *, #58979, .F. ) ;
#15269 = CARTESIAN_POINT ( 'NONE',  ( -97.65000000000001990, 90.00000000000004263, 81.82437500173429612 ) ) ;
#15270 = ORIENTED_EDGE ( 'NONE', *, *, #13878, .F. ) ;
#15271 = CARTESIAN_POINT ( 'NONE',  ( 96.15314808468748708, 91.99731107132950569, 83.87489583420048689 ) ) ;
#15272 = DIRECTION ( 'NONE',  ( -0.9966891607226786576, -0.08130631524009861166, 0.000000000000000000 ) ) ;
#15273 = CARTESIAN_POINT ( 'NONE',  ( -92.75110981005069277, 89.40965860031441537, 74.79348190356854786 ) ) ;
#15274 = DIRECTION ( 'NONE',  ( 0.000000000000000000, 0.000000000000000000, -1.000000000000000000 ) ) ;
#15275 = EDGE_CURVE ( 'NONE', #72197, #54634, #7542, .T. ) ;
#15276 = FACE_OUTER_BOUND ( 'NONE', #70560, .T. ) ;
#15277 = VERTEX_POINT ( 'NONE', #32789 ) ;
#15278 = DIRECTION ( 'NONE',  ( -0.9038112904824853189, 0.4279312458752977943, 0.000000000000000000 ) ) ;
#15279 = CARTESIAN_POINT ( 'NONE',  ( -95.00000000000002842, 90.00000000000004263, 90.00000000000000000 ) ) ;
#15280 = VERTEX_POINT ( 'NONE', #10238 ) ;
#15281 = VERTEX_POINT ( 'NONE', #55738 ) ;
#15282 = VECTOR ( 'NONE', #8227, 1000.000000000000000 ) ;
#15283 = DIRECTION ( 'NONE',  ( 0.000000000000000000, 0.7431448254773878048, -0.6691306063588654540 ) ) ;
#15284 = EDGE_CURVE ( 'NONE', #57864, #73677, #31566, .T. ) ;
#15285 = DIRECTION ( 'NONE',  ( 0.000000000000000000, 0.000000000000000000, 1.000000000000000000 ) ) ;
#15286 = CARTESIAN_POINT ( 'NONE',  ( -97.30629616937497417, -211.3315407142195852, 83.50447916753383026 ) ) ;
#15287 = EDGE_LOOP ( 'NONE', ( #24801, #19130, #46818, #46117 ) ) ;
#15288 = CARTESIAN_POINT ( 'NONE',  ( 11.99999999999999822, 55.38113227695858143, -54.21277698773617715 ) ) ;
#15289 = EDGE_CURVE ( 'NONE', #42474, #69810, #70502, .T. ) ;
#15290 = VERTEX_POINT ( 'NONE', #73387 ) ;
#15291 = DIRECTION ( 'NONE',  ( 1.000000000000000000, 0.000000000000000000, 0.000000000000000000 ) ) ;
#15292 = EDGE_CURVE ( 'NONE', #12564, #17471, #3520, .T. ) ;
#15293 = DIRECTION ( 'NONE',  ( -1.000000000000000000, -0.000000000000000000, -0.000000000000000000 ) ) ;
#15294 = CARTESIAN_POINT ( 'NONE',  ( -13.36666666666666536, 0.000000000000000000, -1.466666666666671670 ) ) ;
#15295 = CARTESIAN_POINT ( 'NONE',  ( 97.30629616937498838, 90.00000000000002842, 79.80031250086713612 ) ) ;
#15296 = CARTESIAN_POINT ( 'NONE',  ( 0.000000000000000000, 0.000000000000000000, -44.99999999999998579 ) ) ;
#15297 = CARTESIAN_POINT ( 'NONE',  ( 0.000000000000000000, 0.000000000000000000, 0.000000000000000000 ) ) ;
#15298 = DIRECTION ( 'NONE',  ( -1.000000000000000000, 0.000000000000000000, 0.000000000000000000 ) ) ;
#15299 = CARTESIAN_POINT ( 'NONE',  ( 10.00000000000000000, -60.67117009219176538, 55.16347631943019536 ) ) ;
#15300 = DIRECTION ( 'NONE',  ( 0.000000000000000000, 0.000000000000000000, -1.000000000000000000 ) ) ;
#15301 = CARTESIAN_POINT ( 'NONE',  ( -96.32499999999996021, -212.2949673200287179, 86.93083333333332519 ) ) ;
#15302 = EDGE_CURVE ( 'NONE', #5092, #52184, #58023, .T. ) ;
#15303 = AXIS2_PLACEMENT_3D ( 'NONE', #55523, #67170, #4039 ) ;
#15304 = LINE ( 'NONE', #42777, #21601 ) ;
#15305 = ADVANCED_FACE ( 'NONE', ( #38075 ), #38451, .T. ) ;
#15306 = CARTESIAN_POINT ( 'NONE',  ( 92.34999999999999432, 88.47002178664752137, 76.79729166840095900 ) ) ;
#15307 = ORIENTED_EDGE ( 'NONE', *, *, #48566, .F. ) ;
#15308 = CARTESIAN_POINT ( 'NONE',  ( -93.84685191531252713, 88.00268892867056536, 83.50447916753381605 ) ) ;
#15309 = DIRECTION ( 'NONE',  ( 0.000000000000000000, 0.000000000000000000, 1.000000000000000000 ) ) ;
#15310 = VECTOR ( 'NONE', #21373, 1000.000000000000000 ) ;
#15311 = SHAPE_REPRESENTATION ( 'coupling', ( #43395 ), #59156 ) ;
#15312 = CARTESIAN_POINT ( 'NONE',  ( 21.07894319797337701, -103.8699611390234878, 5.500000000000000000 ) ) ;
#15313 = ORIENTED_EDGE ( 'NONE', *, *, #60273, .F. ) ;
#15314 = DIRECTION ( 'NONE',  ( -0.000000000000000000, -0.000000000000000000, 1.000000000000000000 ) ) ;
#15315 = CYLINDRICAL_SURFACE ( 'NONE', #19195, 31.99999999999999289 ) ;
#15316 = DIRECTION ( 'NONE',  ( 0.000000000000000000, 0.000000000000000000, 1.000000000000000000 ) ) ;
#15317 = DIRECTION ( 'NONE',  ( -1.000000000000000000, -0.000000000000000000, -0.000000000000000000 ) ) ;
#15318 = CARTESIAN_POINT ( 'NONE',  ( 92.69370383062501162, -209.9999999999999716, 78.37156250086715659 ) ) ;
#15319 = EDGE_LOOP ( 'NONE', ( #801, #73195 ) ) ;
#15320 = VERTEX_POINT ( 'NONE', #27530 ) ;
#15321 = VECTOR ( 'NONE', #26758, 1000.000000000000000 ) ;
#15322 = DIRECTION ( 'NONE',  ( 0.000000000000000000, 0.000000000000000000, 1.000000000000000000 ) ) ;
#15323 = CARTESIAN_POINT ( 'NONE',  ( 10.00000000000000000, 0.000000000000000000, 0.000000000000000000 ) ) ;
#15324 = CARTESIAN_POINT ( 'NONE',  ( 2.746707903440850533E-12, -120.0000000000000000, -70.59999999999999432 ) ) ;
#15325 = CARTESIAN_POINT ( 'NONE',  ( 0.000000000000000000, -41.76106447765533147, 62.50884508063410294 ) ) ;
#15326 = LINE ( 'NONE', #48803, #64547 ) ;
#15327 = CARTESIAN_POINT ( 'NONE',  ( 92.69370383062501162, -211.3315407142195852, 75.24947916753383481 ) ) ;
#15328 = ORIENTED_EDGE ( 'NONE', *, *, #51158, .F. ) ;
#15329 = ADVANCED_FACE ( 'NONE', ( #21141 ), #32425, .T. ) ;
#15330 = DIRECTION ( 'NONE',  ( 0.000000000000000000, -0.8910065241883722287, 0.4539904997395382558 ) ) ;
#15331 = ORIENTED_EDGE ( 'NONE', *, *, #31230, .F. ) ;
#15332 = VERTEX_POINT ( 'NONE', #15887 ) ;
#15333 = CARTESIAN_POINT ( 'NONE',  ( -23.97194136764370498, -131.3950000906648938, 5.500000000000000000 ) ) ;
#15334 = EDGE_CURVE ( 'NONE', #71738, #72957, #36348, .T. ) ;
#15335 = DIRECTION ( 'NONE',  ( 1.000000000000000000, 0.000000000000000000, 0.000000000000000000 ) ) ;
#15336 = ORIENTED_EDGE ( 'NONE', *, *, #70410, .T. ) ;
#15337 = LINE ( 'NONE', #72479, #26938 ) ;
#15338 = CARTESIAN_POINT ( 'NONE',  ( 97.64999999999997726, -208.4700217866474645, 81.55979166840097605 ) ) ;
#15339 = EDGE_CURVE ( 'NONE', #64804, #34327, #6368, .T. ) ;
#15340 = CARTESIAN_POINT ( 'NONE',  ( 97.64999999999997726, 88.47002178664753558, 82.64458333333331552 ) ) ;
#15341 = VERTEX_POINT ( 'NONE', #39192 ) ;
#15342 = FACE_OUTER_BOUND ( 'NONE', #33290, .T. ) ;
#15343 = ORIENTED_EDGE ( 'NONE', *, *, #10033, .F. ) ;
#15344 = CARTESIAN_POINT ( 'NONE',  ( 11.99999999999999822, 29.01471420065673712, -76.69515212745983490 ) ) ;
#15345 = ORIENTED_EDGE ( 'NONE', *, *, #37718, .T. ) ;
#15346 = CARTESIAN_POINT ( 'NONE',  ( 8.700667342345820288, -98.11853780484867116, 5.500000000000000000 ) ) ;
#15347 = CARTESIAN_POINT ( 'NONE',  ( -97.30629616937501680, 88.66845928578038638, 86.04447916753382231 ) ) ;
#15348 = AXIS2_PLACEMENT_3D ( 'NONE', #30766, #8599, #31883 ) ;
#15349 = CARTESIAN_POINT ( 'NONE',  ( 96.15314808468748708, 91.99731107132950569, 81.17614583420048291 ) ) ;
#15350 = VERTEX_POINT ( 'NONE', #62128 ) ;
#15351 = CIRCLE ( 'NONE', #36939, 31.99999999999998579 ) ;
#15352 = FACE_OUTER_BOUND ( 'NONE', #12603, .T. ) ;
#15353 = CARTESIAN_POINT ( 'NONE',  ( -10.00000000000000000, 0.000000000000000000, 0.000000000000000000 ) ) ;
#15354 = ORIENTED_EDGE ( 'NONE', *, *, #3244, .T. ) ;
#15355 = CARTESIAN_POINT ( 'NONE',  ( 23.49955575014745435, 0.001194404164629722436, -80.00000000000000000 ) ) ;
#15356 = ORIENTED_EDGE ( 'NONE', *, *, #62833, .T. ) ;
#15357 = AXIS2_PLACEMENT_3D ( 'NONE', #44527, #33596, #73814 ) ;
#15358 = VERTEX_POINT ( 'NONE', #50830 ) ;
#15359 = CIRCLE ( 'NONE', #72923, 82.00000000000000000 ) ;
#15360 = CARTESIAN_POINT ( 'NONE',  ( 0.000000000000000000, -30.80686688397025108, 21.53537804866070715 ) ) ;
#15361 = ADVANCED_FACE ( 'NONE', ( #73759 ), #66655, .T. ) ;
#15362 = ORIENTED_EDGE ( 'NONE', *, *, #21277, .F. ) ;
#15363 = CARTESIAN_POINT ( 'NONE',  ( -35.50000000000000711, -120.0000000000000000, 2.500000000000000000 ) ) ;
#15364 = CARTESIAN_POINT ( 'NONE',  ( 97.64999999999999147, 90.00000000000002842, 87.85687500173429498 ) ) ;
#15365 = ORIENTED_EDGE ( 'NONE', *, *, #41767, .F. ) ;
#15366 = DIRECTION ( 'NONE',  ( -1.000000000000000000, -2.889240119132116694E-16, 0.000000000000000000 ) ) ;
#15367 = CARTESIAN_POINT ( 'NONE',  ( -97.30629616937495996, -209.9999999999999716, 80.75281250086715090 ) ) ;
#15368 = ORIENTED_EDGE ( 'NONE', *, *, #62559, .F. ) ;
#15369 = DIRECTION ( 'NONE',  ( 0.000000000000000000, 0.000000000000000000, -1.000000000000000000 ) ) ;
#15370 = DIRECTION ( 'NONE',  ( 0.000000000000000000, 0.000000000000000000, 1.000000000000000000 ) ) ;
#15371 = LINE ( 'NONE', #54496, #11701 ) ;
#15372 = CARTESIAN_POINT ( 'NONE',  ( 11.99999999999999822, 62.50884508063427347, 41.76106447765511831 ) ) ;
#15373 = CARTESIAN_POINT ( 'NONE',  ( 10.00000000000000000, -40.68715046381937128, 10.41901085202062660 ) ) ;
#15374 = EDGE_CURVE ( 'NONE', #24130, #11963, #26781, .T. ) ;
#15375 = EDGE_CURVE ( 'NONE', #44000, #68072, #57054, .T. ) ;
#15376 = B_SPLINE_CURVE_WITH_KNOTS ( 'NONE', 3,
 ( #70445, #65210, #59566, #53548, #41899, #25352, #30240, #60679, #53180, #64840, #71936, #8051, #24603, #36996, #65955, #14799, #70826, #60319, #13321, #25713, #47906, #43404, #30972, #20450 ),
 .UNSPECIFIED., .F., .F.,
 ( 4, 2, 2, 2, 2, 2, 2, 2, 2, 2, 2, 4 ),
 ( -0.009991285186810493213, -0.009254074022779614286, -0.008516862858748735360, -0.007779651694717856433, -0.007411046112702417837, -0.007042440530686980109, -0.006673834948671541513, -0.006305229366656103784, -0.005568018202625168479, -0.004830807038594233174, -0.004462201456578745139, -0.004093595874563257103 ),
 .UNSPECIFIED. ) ;
#15377 = AXIS2_PLACEMENT_3D ( 'NONE', #14880, #47990, #3259 ) ;
#15378 = CARTESIAN_POINT ( 'NONE',  ( -95.00000000002617639, -209.9999999999999432, -74.99999999999349143 ) ) ;
#15380 = AXIS2_PLACEMENT_3D ( 'NONE', #1817, #47276, #64203 ) ;
#15379 = CARTESIAN_POINT ( 'NONE',  ( 97.30629616937498838, 90.00000000000002842, 88.05531250086713158 ) ) ;
#15381 = DIRECTION ( 'NONE',  ( -1.000000000000000000, 0.000000000000000000, -0.000000000000000000 ) ) ;
#15382 = CARTESIAN_POINT ( 'NONE',  ( -10.00000000000000000, 0.000000000000000000, 0.000000000000000000 ) ) ;
#15383 = AXIS2_PLACEMENT_3D ( 'NONE', #55374, #49718, #15891 ) ;
#15384 = DIRECTION ( 'NONE',  ( -4.476705744456276711E-17, 1.000000000000000000, -0.000000000000000000 ) ) ;
#15385 = AXIS2_PLACEMENT_3D ( 'NONE', #47861, #19288, #31303 ) ;
#15386 = DIRECTION ( 'NONE',  ( -1.000000000000000000, 0.000000000000000000, 0.000000000000000000 ) ) ;
#15387 = CARTESIAN_POINT ( 'NONE',  ( -92.35000000000003695, 89.99999990163421160, 80.23687499810812085 ) ) ;
#15388 = CARTESIAN_POINT ( 'NONE',  ( -97.65000000000001990, 90.00000000000004263, 87.53937500173429953 ) ) ;
#15389 = ADVANCED_FACE ( 'NONE', ( #27727 ), #33350, .T. ) ;
#15390 = CIRCLE ( 'NONE', #52637, 20.20000000000036522 ) ;
#15391 = CARTESIAN_POINT ( 'NONE',  ( 1.560000000000000053, -1.299038105676658450, -0.7500000000000007772 ) ) ;
#15392 = CARTESIAN_POINT ( 'NONE',  ( 6.000000000000000000, -34.94270380257692921, 74.18225833017875459 ) ) ;
#15393 = PLANE ( 'NONE',  #48532 ) ;
#15394 = CARTESIAN_POINT ( 'NONE',  ( 0.000000000000000000, 14.60985201121704513, 18.46759930825707841 ) ) ;
#15395 = CARTESIAN_POINT ( 'NONE',  ( -96.32499999999996021, -207.7050326799711968, 85.44916666666665606 ) ) ;
#15396 = FACE_OUTER_BOUND ( 'NONE', #60504, .T. ) ;
#15397 =( BOUNDED_CURVE ( )  B_SPLINE_CURVE ( 2, ( #69528, #42808, #2253, #65738, #19128, #59359, #60117 ),
 .UNSPECIFIED., .F., .F. ) 
 B_SPLINE_CURVE_WITH_KNOTS ( ( 3, 2, 2, 3 ),
 ( 0.6875000000000000000, 0.6944444444444443088, 0.7013888888888887285, 0.7083333333333331483 ),
 .UNSPECIFIED. ) 
 CURVE ( )  GEOMETRIC_REPRESENTATION_ITEM ( )  RATIONAL_B_SPLINE_CURVE ( ( 1.000000000000000000, 0.8660254037844387076, 1.000000000000000000, 0.8660254037844387076, 1.000000000000000000, 0.8660254037844430375, 0.9999999999999956701 ) ) 
 REPRESENTATION_ITEM ( '' )  );
#15398 = CIRCLE ( 'NONE', #22616, 32.00000000000000000 ) ;
#15399 = DIRECTION ( 'NONE',  ( -1.000000000000000000, -0.000000000000000000, 0.000000000000000000 ) ) ;
#15400 = DIRECTION ( 'NONE',  ( -1.000000000000000000, -0.000000000000000000, 0.000000000000000000 ) ) ;
#15401 = CARTESIAN_POINT ( 'NONE',  ( 7.400000000000014566, 1.517926714436184493E-13, 13.10000000000024123 ) ) ;
#15402 = VECTOR ( 'NONE', #25753, 1000.000000000000000 ) ;
#15403 = CIRCLE ( 'NONE', #57447, 15.99999999999999822 ) ;
#15404 = CYLINDRICAL_SURFACE ( 'NONE', #23426, 77.49899999999999523 ) ;
#15405 = VECTOR ( 'NONE', #59414, 1000.000000000000000 ) ;
#15406 = AXIS2_PLACEMENT_3D ( 'NONE', #10791, #17903, #27705 ) ;
#15407 = ORIENTED_EDGE ( 'NONE', *, *, #1176, .T. ) ;
#15408 = ORIENTED_EDGE ( 'NONE', *, *, #1560, .T. ) ;
#15409 = CARTESIAN_POINT ( 'NONE',  ( 0.000000000000000000, -30.41916302227060598, -71.27951684758059514 ) ) ;
#15410 = DIRECTION ( 'NONE',  ( 0.000000000000000000, 0.000000000000000000, 1.000000000000000000 ) ) ;
#15411 = ORIENTED_EDGE ( 'NONE', *, *, #44740, .T. ) ;
#15412 = CARTESIAN_POINT ( 'NONE',  ( 96.15314808468748708, -208.0026889286704943, 81.81114583420047381 ) ) ;
#15413 = CARTESIAN_POINT ( 'NONE',  ( 92.69370383062501162, -209.9999999999999716, 86.62656250086715204 ) ) ;
#15414 = ORIENTED_EDGE ( 'NONE', *, *, #56224, .T. ) ;
#15415 = CARTESIAN_POINT ( 'NONE',  ( 92.69370383062501162, -209.9999999999999716, 86.62656250086715204 ) ) ;
#15416 = CIRCLE ( 'NONE', #71814, 77.49900000000000944 ) ;
#15417 = VERTEX_POINT ( 'NONE', #10813 ) ;
#15418 = EDGE_CURVE ( 'NONE', #13981, #1170, #5190, .T. ) ;
#15419 = CARTESIAN_POINT ( 'NONE',  ( 10.00000000000000000, -75.11764819372145041, -2.946379043147127064 ) ) ;
#15420 = ORIENTED_EDGE ( 'NONE', *, *, #53796, .F. ) ;
#15421 = CARTESIAN_POINT ( 'NONE',  ( -92.69370383062502583, 91.33154071421968467, 78.10697916753383652 ) ) ;
#15422 = AXIS2_PLACEMENT_3D ( 'NONE', #9803, #71828, #32713 ) ;
#15423 = VERTEX_POINT ( 'NONE', #28838 ) ;
#15424 = EDGE_CURVE ( 'NONE', #66997, #57978, #5149, .T. ) ;
#15425 = ORIENTED_EDGE ( 'NONE', *, *, #42513, .T. ) ;
#15426 = DIRECTION ( 'NONE',  ( 1.000000000000000000, -0.000000000000000000, 0.000000000000000000 ) ) ;
#15427 = CIRCLE ( 'NONE', #58693, 82.00000000000000000 ) ;
#15428 = ORIENTED_EDGE ( 'NONE', *, *, #54846, .F. ) ;
#15429 = LINE ( 'NONE', #4179, #50932 ) ;
#15430 = DIRECTION ( 'NONE',  ( -0.9435911131814395114, 0.3311129884571304971, 0.000000000000000000 ) ) ;
#15431 = CIRCLE ( 'NONE', #61117, 16.00000000000000000 ) ;
#15432 = EDGE_CURVE ( 'NONE', #40405, #48739, #17193, .T. ) ;
#15433 = VERTEX_POINT ( 'NONE', #61576 ) ;
#15434 = CARTESIAN_POINT ( 'NONE',  ( 5.999999999999999112, -33.71516098798793593, 74.74816331893417498 ) ) ;
#15435 = ORIENTED_EDGE ( 'NONE', *, *, #65859, .F. ) ;
#15436 = CIRCLE ( 'NONE', #35831, 82.00000000000000000 ) ;
#15437 = CARTESIAN_POINT ( 'NONE',  ( 15.00000000000000000, -0.9646360437372099028, 23.52805723605590771 ) ) ;
#15438 = EDGE_CURVE ( 'NONE', #27488, #61944, #3963, .T. ) ;
#15439 = ORIENTED_EDGE ( 'NONE', *, *, #47267, .F. ) ;
#15440 = ORIENTED_EDGE ( 'NONE', *, *, #26738, .T. ) ;
#15441 = VERTEX_POINT ( 'NONE', #68332 ) ;
#15442 = CARTESIAN_POINT ( 'NONE',  ( 97.30629616937498838, -208.6684592857803011, 74.77322916753379900 ) ) ;
#15443 = DIRECTION ( 'NONE',  ( -0.000000000000000000, -0.000000000000000000, 1.000000000000000000 ) ) ;
#15444 = ORIENTED_EDGE ( 'NONE', *, *, #34309, .F. ) ;
#15445 = ORIENTED_EDGE ( 'NONE', *, *, #15719, .F. ) ;
#15446 = ORIENTED_EDGE ( 'NONE', *, *, #31555, .F. ) ;
#15447 = DIRECTION ( 'NONE',  ( 1.000000000000000000, -0.000000000000000000, 0.000000000000000000 ) ) ;
#15448 = DIRECTION ( 'NONE',  ( -0.000000000000000000, -0.000000000000000000, 1.000000000000000000 ) ) ;
#15449 = EDGE_CURVE ( 'NONE', #278, #33646, #66368, .T. ) ;
#15451 = CARTESIAN_POINT ( 'NONE',  ( -92.35000000000005116, 91.52997821335253548, 89.73541666666666572 ) ) ;
#15450 = AXIS2_PLACEMENT_3D ( 'NONE', #44120, #72669, #53931 ) ;
#15452 = EDGE_CURVE ( 'NONE', #26707, #34118, #391, .T. ) ;
#15453 = ORIENTED_EDGE ( 'NONE', *, *, #41198, .F. ) ;
#15454 = CARTESIAN_POINT ( 'NONE',  ( 97.30629616937498838, 90.00000000000002842, 77.89531250086714920 ) ) ;
#15455 = VERTEX_POINT ( 'NONE', #16449 ) ;
#15456 = FACE_OUTER_BOUND ( 'NONE', #9509, .T. ) ;
#15457 = CARTESIAN_POINT ( 'NONE',  ( -92.69370383062498320, -209.9999999999999716, 88.69031250086715090 ) ) ;
#15458 = CIRCLE ( 'NONE', #3467, 2.649999999999985700 ) ;
#15459 = CARTESIAN_POINT ( 'NONE',  ( 96.90829729882862864, -211.8387227684681591, 74.99954709728268654 ) ) ;
#15460 = DIRECTION ( 'NONE',  ( -1.000000000000000000, 0.000000000000000000, 0.000000000000000000 ) ) ;
#15461 = DIRECTION ( 'NONE',  ( 0.000000000000000000, 0.000000000000000000, 1.000000000000000000 ) ) ;
#15462 = CARTESIAN_POINT ( 'NONE',  ( -97.30629616937497417, -211.3315407142195852, 78.90072916753381094 ) ) ;
#15463 = AXIS2_PLACEMENT_3D ( 'NONE', #23743, #57964, #51576 ) ;
#15464 = VECTOR ( 'NONE', #56385, 1000.000000000000000 ) ;
#15465 = CARTESIAN_POINT ( 'NONE',  ( 92.34999999999999432, 90.00000000000002842, 86.82500000000000284 ) ) ;
#15466 = DIRECTION ( 'NONE',  ( 0.6862798483830534479, 0.7273375899149810975, 0.000000000000000000 ) ) ;
#15467 = CYLINDRICAL_SURFACE ( 'NONE', #47896, 12.49999999999999645 ) ;
#15468 = ORIENTED_EDGE ( 'NONE', *, *, #71520, .T. ) ;
#15469 = ADVANCED_FACE ( 'NONE', ( #11177 ), #15709, .F. ) ;
#15470 = ADVANCED_FACE ( 'NONE', ( #4825 ), #34474, .T. ) ;
#15471 = AXIS2_PLACEMENT_3D ( 'NONE', #44344, #38705, #10123 ) ;
#15472 = VERTEX_POINT ( 'NONE', #57417 ) ;
#15473 = LINE ( 'NONE', #38415, #57684 ) ;
#15474 = CIRCLE ( 'NONE', #16662, 15.80000000000028315 ) ;
#15475 = CARTESIAN_POINT ( 'NONE',  ( 97.64999999999999147, 90.00000000000002842, 84.60249999999999204 ) ) ;
#15476 = CARTESIAN_POINT ( 'NONE',  ( 95.05423112903736182, -207.6112450486803880, 74.83591575723767164 ) ) ;
#15477 = CARTESIAN_POINT ( 'NONE',  ( -96.15314808468752972, 91.99731107132950569, 80.64697916753381435 ) ) ;
#15478 = CARTESIAN_POINT ( 'NONE',  ( 10.00000000000000000, 59.03342792756263435, 46.54456581323825048 ) ) ;
#15479 = DIRECTION ( 'NONE',  ( -1.000000000000000000, -0.000000000000000000, -0.000000000000000000 ) ) ;
#15480 = ORIENTED_EDGE ( 'NONE', *, *, #40609, .F. ) ;
#15481 = DIRECTION ( 'NONE',  ( -8.783410004945701396E-16, -1.065814103640131188E-14, -1.000000000000000000 ) ) ;
#15482 = VECTOR ( 'NONE', #15293, 1000.000000000000000 ) ;
#15483 = AXIS2_PLACEMENT_3D ( 'NONE', #19159, #19893, #36449 ) ;
#15484 = LINE ( 'NONE', #3489, #73648 ) ;
#15486 = CARTESIAN_POINT ( 'NONE',  ( 11.99999999999999822, 0.000000000000000000, 0.000000000000000000 ) ) ;
#15485 = VECTOR ( 'NONE', #20688, 999.9999999999998863 ) ;
#15487 = AXIS2_PLACEMENT_3D ( 'NONE', #34963, #23316, #16552 ) ;
#15488 = CARTESIAN_POINT ( 'NONE',  ( -95.00000000000002842, 93.05995642670504253, 89.84125000000000227 ) ) ;
#15489 = CARTESIAN_POINT ( 'NONE',  ( 10.00000000000000000, 0.000000000000000000, 0.000000000000000000 ) ) ;
#15490 = CARTESIAN_POINT ( 'NONE',  ( -94.99999999999997158, -207.3369185715606307, 78.84781250086714977 ) ) ;
#15491 = AXIS2_PLACEMENT_3D ( 'NONE', #10438, #60839, #43567 ) ;
#15492 = AXIS2_PLACEMENT_3D ( 'NONE', #45578, #39553, #40287 ) ;
#15493 = FACE_OUTER_BOUND ( 'NONE', #40693, .T. ) ;
#15494 = AXIS2_PLACEMENT_3D ( 'NONE', #5089, #68970, #5460 ) ;
#15495 = ORIENTED_EDGE ( 'NONE', *, *, #9675, .F. ) ;
#15496 = CARTESIAN_POINT ( 'NONE',  ( 10.00000000000000000, -73.95703589263990807, 23.16143007188399139 ) ) ;
#15497 = CARTESIAN_POINT ( 'NONE',  ( 12.00000000000000000, -22.67460108101774452, 6.353146135318220367 ) ) ;
#15498 = CARTESIAN_POINT ( 'NONE',  ( 10.00000000000000000, 0.000000000000000000, 0.000000000000000000 ) ) ;
#15499 = VERTEX_POINT ( 'NONE', #5929 ) ;
#15500 = FACE_BOUND ( 'NONE', #14795, .T. ) ;
#15501 = CYLINDRICAL_SURFACE ( 'NONE', #11403, 16.00000000000000000 ) ;
#15502 = EDGE_CURVE ( 'NONE', #19022, #20908, #33740, .T. ) ;
#15503 = LINE ( 'NONE', #32782, #47992 ) ;
#15504 = EDGE_LOOP ( 'NONE', ( #47525, #5393, #783, #48735, #62229, #40985 ) ) ;
#15505 = EDGE_CURVE ( 'NONE', #7487, #38564, #10432, .T. ) ;
#15506 = CIRCLE ( 'NONE', #57548, 31.99999999999998934 ) ;
#15507 = CARTESIAN_POINT ( 'NONE',  ( 10.00000000000000000, -6.736453364083292428, -36.88895765772640800 ) ) ;
#15508 = CARTESIAN_POINT ( 'NONE',  ( 10.00000000000000000, 75.11764819372149304, 29.05362095685338986 ) ) ;
#15509 = ORIENTED_EDGE ( 'NONE', *, *, #13310, .F. ) ;
#15510 = EDGE_CURVE ( 'NONE', #61033, #20162, #48372, .T. ) ;
#15511 = DIRECTION ( 'NONE',  ( -1.000000000000000000, 0.000000000000000000, 0.000000000000000000 ) ) ;
#15512 = CARTESIAN_POINT ( 'NONE',  ( -97.64996763243318867, -208.4700030992240727, 87.48645704240065868 ) ) ;
#15513 = ORIENTED_EDGE ( 'NONE', *, *, #64442, .T. ) ;
#15514 = CIRCLE ( 'NONE', #9505, 5.000000000000000888 ) ;
#15515 = EDGE_CURVE ( 'NONE', #2062, #49474, #15957, .T. ) ;
#15516 = LINE ( 'NONE', #7753, #48636 ) ;
#15517 = AXIS2_PLACEMENT_3D ( 'NONE', #6868, #7977, #29779 ) ;
#15518 = ORIENTED_EDGE ( 'NONE', *, *, #66, .F. ) ;
#15519 = CARTESIAN_POINT ( 'NONE',  ( -96.32499999999996021, -207.7050326799711968, 84.89354166840095672 ) ) ;
#15520 = FACE_OUTER_BOUND ( 'NONE', #65111, .T. ) ;
#15521 = CIRCLE ( 'NONE', #9511, 31.99999999999998224 ) ;
#15522 = VERTEX_POINT ( 'NONE', #5189 ) ;
#15523 = EDGE_CURVE ( 'NONE', #64668, #17422, #1574, .T. ) ;
#15524 = ORIENTED_EDGE ( 'NONE', *, *, #40184, .T. ) ;
#15525 = AXIS2_PLACEMENT_3D ( 'NONE', #28537, #68035, #45111 ) ;
#15526 = EDGE_LOOP ( 'NONE', ( #65933, #46709, #45689, #38836 ) ) ;
#15527 = CARTESIAN_POINT ( 'NONE',  ( -7.400000000000003908, -1.056673655988042765E-14, -5.892267102755452808E-15 ) ) ;
#15528 = ORIENTED_EDGE ( 'NONE', *, *, #22089, .T. ) ;
#15529 = ORIENTED_EDGE ( 'NONE', *, *, #19028, .F. ) ;
#15530 = CARTESIAN_POINT ( 'NONE',  ( 93.84685191531248449, 88.00268892867053694, 77.20739583420048291 ) ) ;
#15531 = DIRECTION ( 'NONE',  ( -0.000000000000000000, -0.000000000000000000, 1.000000000000000000 ) ) ;
#15532 = ADVANCED_FACE ( 'NONE', ( #22466 ), #22845, .T. ) ;
#15533 = CARTESIAN_POINT ( 'NONE',  ( 2.874421927457452952, -143.3717286177755739, -5.500000000000000000 ) ) ;
#15534 = ORIENTED_EDGE ( 'NONE', *, *, #41524, .F. ) ;
#15536 = EDGE_LOOP ( 'NONE', ( #68156, #65151, #62973, #23765 ) ) ;
#15535 = AXIS2_PLACEMENT_3D ( 'NONE', #58280, #53017, #24435 ) ;
#15537 = EDGE_LOOP ( 'NONE', ( #40879, #5569, #18061, #57615 ) ) ;
#15538 = CARTESIAN_POINT ( 'NONE',  ( 94.99999999999998579, 92.66308142843935514, 87.57906250086713840 ) ) ;
#15539 = ORIENTED_EDGE ( 'NONE', *, *, #12878, .T. ) ;
#15540 = CARTESIAN_POINT ( 'NONE',  ( 97.30629616937498838, -208.6684592857803011, 84.29822916753380468 ) ) ;
#15541 = AXIS2_PLACEMENT_3D ( 'NONE', #38192, #44212, #61135 ) ;
#15542 = AXIS2_PLACEMENT_3D ( 'NONE', #9714, #55578, #33002 ) ;
#15543 = APPLICATION_PROTOCOL_DEFINITION ( 'draft international standard', 'automotive_design', 1998, #44574 ) ;
#15544 = DIRECTION ( 'NONE',  ( -1.000000000000000000, -0.000000000000000000, -0.000000000000000000 ) ) ;
#15545 = CARTESIAN_POINT ( 'NONE',  ( -10.00000000000000000, 0.000000000000000000, 0.000000000000000000 ) ) ;
#15546 = DIRECTION ( 'NONE',  ( -1.000000000000000000, 0.000000000000000000, 0.000000000000000000 ) ) ;
#15547 = CARTESIAN_POINT ( 'NONE',  ( 0.000000000000000000, 0.000000000000000000, -1.199999999999999956 ) ) ;
#15548 = LINE ( 'NONE', #4661, #58863 ) ;
#15549 = VECTOR ( 'NONE', #39772, 1000.000000000000000 ) ;
#15550 = CARTESIAN_POINT ( 'NONE',  ( 92.35000000002543175, -209.9999999999998863, -74.99999999999342037 ) ) ;
#15551 = AXIS2_PLACEMENT_3D ( 'NONE', #60188, #43270, #9027 ) ;
#15552 = CARTESIAN_POINT ( 'NONE',  ( -97.30629616937497417, -211.3315407142195852, 87.15572916753380639 ) ) ;
#15553 = EDGE_CURVE ( 'NONE', #9784, #34086, #30673, .T. ) ;
#15554 = CARTESIAN_POINT ( 'NONE',  ( -97.30629616937501680, 90.00000000000004263, 87.26156250086715715 ) ) ;
#15555 = ADVANCED_FACE ( 'NONE', ( #12279 ), #1053, .F. ) ;
#15556 = ORIENTED_EDGE ( 'NONE', *, *, #59683, .T. ) ;
#15558 = CARTESIAN_POINT ( 'NONE',  ( -97.30629616937501680, 91.33154071421968467, 87.04989583420048405 ) ) ;
#15557 = CARTESIAN_POINT ( 'NONE',  ( 97.30629616937498838, 90.00000000000002842, 87.42031250086714067 ) ) ;
#15559 = EDGE_LOOP ( 'NONE', ( #5756, #34890, #29455, #15133 ) ) ;
#15560 = DIRECTION ( 'NONE',  ( 1.000000000000000000, 0.000000000000000000, -0.000000000000000000 ) ) ;
#15561 = CARTESIAN_POINT ( 'NONE',  ( 11.99999999999999822, -41.76106447765533147, 62.50884508063410294 ) ) ;
#15562 = CYLINDRICAL_SURFACE ( 'NONE', #11541, 2.649999999999985700 ) ;
#15563 = DIRECTION ( 'NONE',  ( 0.000000000000000000, 0.000000000000000000, 1.000000000000000000 ) ) ;
#15564 = CARTESIAN_POINT ( 'NONE',  ( 10.00000000000000000, -75.11764819372145041, -2.946379043147127064 ) ) ;
#15565 = DIRECTION ( 'NONE',  ( 0.000000000000000000, 0.000000000000000000, -1.000000000000000000 ) ) ;
#15566 = CARTESIAN_POINT ( 'NONE',  ( 0.000000000000000000, -37.01155633439063308, 6.555932627142289526 ) ) ;
#15567 = CARTESIAN_POINT ( 'NONE',  ( 0.000000000000000000, 73.95703589263973754, 23.16143007188452430 ) ) ;
#15568 = ORIENTED_EDGE ( 'NONE', *, *, #64171, .T. ) ;
#15569 = ORIENTED_EDGE ( 'NONE', *, *, #62245, .T. ) ;
#15570 = CARTESIAN_POINT ( 'NONE',  ( -95.00000000000002842, 86.94004357329504273, 81.26874999999999716 ) ) ;
#15571 = DIRECTION ( 'NONE',  ( 0.000000000000000000, 0.000000000000000000, 1.000000000000000000 ) ) ;
#15572 = CARTESIAN_POINT ( 'NONE',  ( -97.64999999999994884, 88.47002178664749295, 78.62291666666668277 ) ) ;
#15573 = DIRECTION ( 'NONE',  ( 1.000000000000000000, 0.000000000000000000, 0.000000000000000000 ) ) ;
#15574 = CARTESIAN_POINT ( 'NONE',  ( 11.99999999999999822, 31.47745569255140552, 68.26794271651274926 ) ) ;
#15575 = CARTESIAN_POINT ( 'NONE',  ( 10.00000000000000000, -77.49459641780886443, -0.8261519478439277586 ) ) ;
#15576 = CARTESIAN_POINT ( 'NONE',  ( -97.65000000000001990, 90.00000000000004263, 90.00000000000000000 ) ) ;
#15577 = CARTESIAN_POINT ( 'NONE',  ( 0.000000000000000000, 0.000000000000000000, 0.000000000000000000 ) ) ;
#15578 = CIRCLE ( 'NONE', #68403, 82.00000000000000000 ) ;
#15579 = ORIENTED_EDGE ( 'NONE', *, *, #34806, .F. ) ;
#15580 = CARTESIAN_POINT ( 'NONE',  ( -92.69370383062502583, 88.66845928578038638, 80.38239583420049428 ) ) ;
#15581 = AXIS2_PLACEMENT_3D ( 'NONE', #39242, #4304, #10657 ) ;
#15583 = CARTESIAN_POINT ( 'NONE',  ( 2.746707903440850533E-12, -120.0000000000000000, -70.59999999999999432 ) ) ;
#15582 = CIRCLE ( 'NONE', #57564, 31.99999999999999289 ) ;
#15584 = CARTESIAN_POINT ( 'NONE',  ( 0.000000000000000000, -35.38097989696520074, 12.42422080174625520 ) ) ;
#15585 = CARTESIAN_POINT ( 'NONE',  ( 0.000000000000000000, 14.60985201121729737, -18.46759930825687945 ) ) ;
#15586 = CARTESIAN_POINT ( 'NONE',  ( 0.000000000000000000, 0.000000000000000000, 0.000000000000000000 ) ) ;
#15587 = AXIS2_PLACEMENT_3D ( 'NONE', #52282, #10671, #22330 ) ;
#15588 = CARTESIAN_POINT ( 'NONE',  ( -4.250000000000000000, -13.95926121303099343, -1.199999999999999956 ) ) ;
#15589 = CARTESIAN_POINT ( 'NONE',  ( -10.00000000000000000, 0.000000000000000000, 0.000000000000000000 ) ) ;
#15590 =( NAMED_UNIT ( * ) SI_UNIT ( $, .STERADIAN. ) SOLID_ANGLE_UNIT ( ) );
#15591 = CYLINDRICAL_SURFACE ( 'NONE', #49680, 31.99999999999998579 ) ;
#15592 = EDGE_CURVE ( 'NONE', #69529, #20602, #41230, .T. ) ;
#15593 = CARTESIAN_POINT ( 'NONE',  ( 93.84685191531248449, 88.00268892867053694, 79.74739583420048916 ) ) ;
#15594 = CARTESIAN_POINT ( 'NONE',  ( -97.30629616937497417, -208.6684592857803295, 82.12864583420048348 ) ) ;
#15595 = LINE ( 'NONE', #55819, #12164 ) ;
#15596 = AXIS2_PLACEMENT_3D ( 'NONE', #67912, #63037, #56643 ) ;
#15597 = ORIENTED_EDGE ( 'NONE', *, *, #71050, .F. ) ;
#15598 = DIRECTION ( 'NONE',  ( -1.000000000000000000, -0.000000000000000000, 0.000000000000000000 ) ) ;
#15599 = CARTESIAN_POINT ( 'NONE',  ( -93.67499999999998295, -212.2949673200287179, 79.41666666666665719 ) ) ;
#15600 = CARTESIAN_POINT ( 'NONE',  ( 0.000000000000000000, 2.956366410621684260, -75.11725578898465017 ) ) ;
#15601 = VECTOR ( 'NONE', #54060, 1000.000000000000000 ) ;
#15602 = VECTOR ( 'NONE', #65127, 1000.000000000000227 ) ;
#15603 = VECTOR ( 'NONE', #1378, 1000.000000000000000 ) ;
#15604 = EDGE_CURVE ( 'NONE', #70908, #11546, #30334, .T. ) ;
#15605 = CIRCLE ( 'NONE', #58871, 82.00000000000000000 ) ;
#15606 = AXIS2_PLACEMENT_3D ( 'NONE', #38253, #55173, #8946 ) ;
#15607 = CARTESIAN_POINT ( 'NONE',  ( -96.15314808468751551, 88.00268892867056536, 77.20739583420048291 ) ) ;
#15608 = CARTESIAN_POINT ( 'NONE',  ( 93.84685191531249870, -208.0026889286704943, 81.91697916753381037 ) ) ;
#15609 = ORIENTED_EDGE ( 'NONE', *, *, #35293, .T. ) ;
#15610 = ADVANCED_FACE ( 'NONE', ( #64175 ), #2159, .T. ) ;
#15611 = DIRECTION ( 'NONE',  ( -1.000000000000000000, -0.000000000000000000, 0.000000000000000000 ) ) ;
#15612 = ORIENTED_EDGE ( 'NONE', *, *, #48583, .F. ) ;
#15613 = DIRECTION ( 'NONE',  ( -1.000000000000000000, 0.000000000000000000, 0.000000000000000000 ) ) ;
#15614 = VERTEX_POINT ( 'NONE', #52137 ) ;
#15615 = EDGE_CURVE ( 'NONE', #70065, #16929, #7761, .T. ) ;
#15616 = ADVANCED_FACE ( 'NONE', ( #29934 ), #58901, .F. ) ;
#15617 = LINE ( 'NONE', #51298, #1167 ) ;
#15618 = ORIENTED_EDGE ( 'NONE', *, *, #20561, .T. ) ;
#15619 = ORIENTED_EDGE ( 'NONE', *, *, #33025, .F. ) ;
#15620 = CARTESIAN_POINT ( 'NONE',  ( 92.69370383062501162, -211.3315407142195852, 75.24947916753383481 ) ) ;
#15621 = CARTESIAN_POINT ( 'NONE',  ( 19.29194287201271862, -133.5026271600380880, 2.500000000000000000 ) ) ;
#15622 = DIRECTION ( 'NONE',  ( 0.000000000000000000, 0.07845909572784530439, -0.9969173337331279638 ) ) ;
#15623 =( BOUNDED_CURVE ( )  B_SPLINE_CURVE ( 2, ( #29690, #24087, #68085, #11305, #57921, #39520, #62463 ),
 .UNSPECIFIED., .F., .F. ) 
 B_SPLINE_CURVE_WITH_KNOTS ( ( 3, 2, 2, 3 ),
 ( 0.9583333333333337034, 0.9652777777777781232, 0.9722222222222225430, 0.9791666666666669627 ),
 .UNSPECIFIED. ) 
 CURVE ( )  GEOMETRIC_REPRESENTATION_ITEM ( )  RATIONAL_B_SPLINE_CURVE ( ( 0.9999999999999935607, 0.8660254037844451469, 1.000000000000000000, 0.8660254037844387076, 1.000000000000000000, 0.8660254037844322683, 1.000000000000006439 ) ) 
 REPRESENTATION_ITEM ( '' )  );
#15624 = CARTESIAN_POINT ( 'NONE',  ( -96.91066463018650268, 88.26122129797420257, 74.95660481729453295 ) ) ;
#15625 = CARTESIAN_POINT ( 'NONE',  ( 96.15314808468748708, 88.00268892867053694, 86.83822916753382515 ) ) ;
#15626 = AXIS2_PLACEMENT_3D ( 'NONE', #37388, #49010, #8799 ) ;
#15627 = EDGE_CURVE ( 'NONE', #423, #30489, #67676, .T. ) ;
#15628 = DIRECTION ( 'NONE',  ( -1.000000000000000000, 0.000000000000000000, 0.000000000000000000 ) ) ;
#15629 = CARTESIAN_POINT ( 'NONE',  ( 96.32499999999998863, -207.7050326799711968, 77.08833333333332405 ) ) ;
#15630 = ORIENTED_EDGE ( 'NONE', *, *, #44237, .T. ) ;
#15631 = ORIENTED_EDGE ( 'NONE', *, *, #70276, .F. ) ;
#15632 = EDGE_LOOP ( 'NONE', ( #11449, #26314, #48379, #3421 ) ) ;
#15633 = VERTEX_POINT ( 'NONE', #17556 ) ;
#15634 =( LENGTH_UNIT ( ) NAMED_UNIT ( * ) SI_UNIT ( .MILLI., .METRE. ) );
#15635 = AXIS2_PLACEMENT_3D ( 'NONE', #4797, #16420, #39356 ) ;
#15636 = PRESENTATION_STYLE_ASSIGNMENT (( #50193 ) ) ;
#15637 = DIRECTION ( 'NONE',  ( 0.000000000000000000, -0.9510565162951566398, 0.3090169943749381809 ) ) ;
#15638 = CARTESIAN_POINT ( 'NONE',  ( -97.65000000000001990, 88.47002178664754979, 81.87729166840097150 ) ) ;
#15639 = PLANE ( 'NONE',  #43820 ) ;
#15640 = DIRECTION ( 'NONE',  ( -0.000000000000000000, -0.000000000000000000, 1.000000000000000000 ) ) ;
#15641 = DIRECTION ( 'NONE',  ( -0.000000000000000000, 1.000000000000000000, -0.000000000000000000 ) ) ;
#15642 = VERTEX_POINT ( 'NONE', #30309 ) ;
#15643 = CARTESIAN_POINT ( 'NONE',  ( -97.64999999999994884, -211.5299782133524502, 85.05229166840096866 ) ) ;
#15645 = VERTEX_POINT ( 'NONE', #41979 ) ;
#15644 = EDGE_CURVE ( 'NONE', #49408, #70179, #43618, .T. ) ;
#15646 = CARTESIAN_POINT ( 'NONE',  ( -10.00000000000000000, 0.000000000000000000, 0.000000000000000000 ) ) ;
#15647 = VERTEX_POINT ( 'NONE', #58152 ) ;
#15648 = CARTESIAN_POINT ( 'NONE',  ( -95.00000000000002842, 93.05995642670501411, 84.20562500173429044 ) ) ;
#15649 =( BOUNDED_CURVE ( )  B_SPLINE_CURVE ( 2, ( #39897, #41371, #24090 ),
 .UNSPECIFIED., .F., .F. ) 
 B_SPLINE_CURVE_WITH_KNOTS ( ( 3, 3 ),
 ( 0.000000000000000000, 2.334341054548227728E-05 ),
 .UNSPECIFIED. ) 
 CURVE ( )  GEOMETRIC_REPRESENTATION_ITEM ( )  RATIONAL_B_SPLINE_CURVE ( ( 0.9459494467533928752, 0.9464399322878992438, 0.9469490141588211563 ) ) 
 REPRESENTATION_ITEM ( '' )  );
#15651 = EDGE_CURVE ( 'NONE', #4576, #64387, #35581, .T. ) ;
#15650 = ORIENTED_EDGE ( 'NONE', *, *, #40264, .F. ) ;
#15652 = CARTESIAN_POINT ( 'NONE',  ( 97.30629616937498838, 90.00000000000002842, 81.86406250086714920 ) ) ;
#15653 = CARTESIAN_POINT ( 'NONE',  ( -94.99999999999997158, -209.9999999999999716, 90.00000000000000000 ) ) ;
#15654 = CARTESIAN_POINT ( 'NONE',  ( -92.35000000002592913, -210.0000117261698165, 82.77687459617060028 ) ) ;
#15655 = CARTESIAN_POINT ( 'NONE',  ( -3.000000000000000000, -26.23277895567251505, 4.042438405569750870 ) ) ;
#15656 = AXIS2_PLACEMENT_3D ( 'NONE', #42952, #42576, #65887 ) ;
#15657 = DIRECTION ( 'NONE',  ( 0.000000000000000000, 0.000000000000000000, 1.000000000000000000 ) ) ;
#15658 = CARTESIAN_POINT ( 'NONE',  ( 0.000000000000000000, -74.65374052328654386, 8.840884882374837161 ) ) ;
#15659 = ORIENTED_EDGE ( 'NONE', *, *, #38084, .F. ) ;
#15660 = DIRECTION ( 'NONE',  ( -1.000000000000000000, 0.000000000000000000, 0.000000000000000000 ) ) ;
#15661 = AXIS2_PLACEMENT_3D ( 'NONE', #5259, #33418, #46208 ) ;
#15662 = AXIS2_PLACEMENT_3D ( 'NONE', #19520, #29682, #13141 ) ;
#15663 = LINE ( 'NONE', #2927, #31098 ) ;
#15664 = ORIENTED_EDGE ( 'NONE', *, *, #49219, .T. ) ;
#15665 = ORIENTED_EDGE ( 'NONE', *, *, #20611, .T. ) ;
#15666 = AXIS2_PLACEMENT_3D ( 'NONE', #17816, #46398, #64072 ) ;
#15667 = AXIS2_PLACEMENT_3D ( 'NONE', #33910, #57601, #68127 ) ;
#15668 = CARTESIAN_POINT ( 'NONE',  ( -7.572224309238338336, -145.4393675041377492, 5.500000000000000000 ) ) ;
#15669 = DIRECTION ( 'NONE',  ( -1.000000000000000000, -0.000000000000000000, -0.000000000000000000 ) ) ;
#15670 = DIRECTION ( 'NONE',  ( 0.000000000000000000, -0.9238795325112821866, -0.3826834323651008285 ) ) ;
#15671 = CARTESIAN_POINT ( 'NONE',  ( -93.84685191531247028, -211.9973110713294489, 79.85322916753381151 ) ) ;
#15672 = ORIENTED_EDGE ( 'NONE', *, *, #41363, .T. ) ;
#15673 = CARTESIAN_POINT ( 'NONE',  ( 10.00000000000000000, -68.27212725128254078, -31.46837873495049465 ) ) ;
#15674 = ORIENTED_EDGE ( 'NONE', *, *, #52301, .T. ) ;
#15675 = CARTESIAN_POINT ( 'NONE',  ( -12.50000000000000000, -120.0000000000000000, 40.00000000000000711 ) ) ;
#15676 = CARTESIAN_POINT ( 'NONE',  ( 0.000000000000000000, 8.840884882375075193, 74.65374052328651544 ) ) ;
#15677 = CARTESIAN_POINT ( 'NONE',  ( 96.32499999999998863, -207.7050326799711968, 82.88270833506763324 ) ) ;
#15678 = CARTESIAN_POINT ( 'NONE',  ( 94.99999999999998579, 87.33691857156068750, 77.73656250086713726 ) ) ;
#15679 = CARTESIAN_POINT ( 'NONE',  ( 0.000000000000000000, 76.66974797899835892, 11.30684508768366570 ) ) ;
#15680 = DIRECTION ( 'NONE',  ( -0.000000000000000000, 0.000000000000000000, 1.000000000000000000 ) ) ;
#15681 = LINE ( 'NONE', #8560, #66095 ) ;
#15682 = CARTESIAN_POINT ( 'NONE',  ( 92.50303120605391882, 90.24436280099763508, 74.91343443312143791 ) ) ;
#15683 = DIRECTION ( 'NONE',  ( 0.000000000000000000, 0.000000000000000000, 1.000000000000000000 ) ) ;
#15684 = DIRECTION ( 'NONE',  ( 2.603472992746261562E-14, 2.546204323184492723E-14, -1.000000000000000000 ) ) ;
#15685 = CYLINDRICAL_SURFACE ( 'NONE', #59811, 3.000000000000000888 ) ;
#15686 = CARTESIAN_POINT ( 'NONE',  ( -97.64999999996642543, 89.99999234487438571, 78.01464417100932280 ) ) ;
#15688 = EDGE_CURVE ( 'NONE', #40498, #64184, #40873, .T. ) ;
#15687 = ORIENTED_EDGE ( 'NONE', *, *, #59417, .F. ) ;
#15689 = CIRCLE ( 'NONE', #45703, 3.299999999999983391 ) ;
#15690 = CARTESIAN_POINT ( 'NONE',  ( -92.69370383062505425, 91.33154071421968467, 83.66322916753381378 ) ) ;
#15691 = DIRECTION ( 'NONE',  ( -1.000000000000000000, -0.000000000000000000, -0.000000000000000000 ) ) ;
#15692 = EDGE_CURVE ( 'NONE', #46710, #31992, #7010, .T. ) ;
#15693 = CARTESIAN_POINT ( 'NONE',  ( 7.103376864691351012E-17, -120.0000000000000000, -85.59999999999999432 ) ) ;
#15694 = EDGE_CURVE ( 'NONE', #39027, #24045, #24675, .T. ) ;
#15695 = ORIENTED_EDGE ( 'NONE', *, *, #2194, .F. ) ;
#15696 = DIRECTION ( 'NONE',  ( -1.000000000000000000, -0.000000000000000000, 0.000000000000000000 ) ) ;
#15697 = DIRECTION ( 'NONE',  ( 1.000000000000000000, 0.000000000000000000, 0.000000000000000000 ) ) ;
#15698 = DIRECTION ( 'NONE',  ( 0.000000000000000000, 0.000000000000000000, 1.000000000000000000 ) ) ;
#15699 = PRESENTATION_LAYER_ASSIGNMENT (  '', '', ( #55299 ) ) ;
#15700 = EDGE_CURVE ( 'NONE', #38545, #39945, #11908, .T. ) ;
#15701 = CIRCLE ( 'NONE', #31312, 82.00000000000000000 ) ;
#15702 = DIRECTION ( 'NONE',  ( 0.000000000000000000, 0.000000000000000000, 1.000000000000000000 ) ) ;
#15703 = CARTESIAN_POINT ( 'NONE',  ( 95.00000000000000000, -212.6630814284392557, 78.53031250086715431 ) ) ;
#15704 = CIRCLE ( 'NONE', #25319, 82.00000000000000000 ) ;
#15705 = ORIENTED_EDGE ( 'NONE', *, *, #3664, .F. ) ;
#15706 = ORIENTED_EDGE ( 'NONE', *, *, #44819, .T. ) ;
#15707 = DIRECTION ( 'NONE',  ( 1.000000000000000000, 0.000000000000000000, 0.000000000000000000 ) ) ;
#15708 = ADVANCED_FACE ( 'NONE', ( #6294 ), #35215, .F. ) ;
#15709 = PLANE ( 'NONE',  #42372 ) ;
#15710 = CARTESIAN_POINT ( 'NONE',  ( -1.192633404626841198, -119.0902607174754451, -2.500000000000000000 ) ) ;
#15711 = DIRECTION ( 'NONE',  ( -1.000000000000000000, 0.000000000000000000, -0.000000000000000000 ) ) ;
#15712 = EDGE_CURVE ( 'NONE', #23400, #23659, #32150, .T. ) ;
#15713 = LINE ( 'NONE', #28463, #30879 ) ;
#15714 = EDGE_CURVE ( 'NONE', #25323, #9618, #37071, .T. ) ;
#15715 = CARTESIAN_POINT ( 'NONE',  ( 95.00000000000000000, -212.6630814284392557, 75.99031250086716227 ) ) ;
#15716 = VERTEX_POINT ( 'NONE', #59635 ) ;
#15717 = CARTESIAN_POINT ( 'NONE',  ( 15.00000000000000000, -23.29833615347109088, -3.418703333116486665 ) ) ;
#15718 = VERTEX_POINT ( 'NONE', #71259 ) ;
#15719 = EDGE_CURVE ( 'NONE', #39507, #67503, #26826, .T. ) ;
#15720 = EDGE_LOOP ( 'NONE', ( #63534, #68746, #64368, #17008 ) ) ;
#15721 = DIRECTION ( 'NONE',  ( 0.000000000000000000, 0.000000000000000000, -1.000000000000000000 ) ) ;
#15722 = DIRECTION ( 'NONE',  ( 0.000000000000000000, -0.9781476007338070211, 0.2079116908177525425 ) ) ;
#15723 = ORIENTED_EDGE ( 'NONE', *, *, #56825, .F. ) ;
#15724 = CARTESIAN_POINT ( 'NONE',  ( 0.000000000000000000, -49.70050353004846500, -59.46389618802017907 ) ) ;
#15725 = CARTESIAN_POINT ( 'NONE',  ( 92.35000000000000853, -209.9999999999999716, 79.91937500173429498 ) ) ;
#15726 = CARTESIAN_POINT ( 'NONE',  ( 94.99999999999998579, 86.94004357329500010, 83.17374999999999829 ) ) ;
#15727 = ORIENTED_EDGE ( 'NONE', *, *, #5887, .F. ) ;
#15728 = DIRECTION ( 'NONE',  ( -1.000000000000000000, 0.000000000000000000, -0.000000000000000000 ) ) ;
#15729 = ORIENTED_EDGE ( 'NONE', *, *, #10174, .F. ) ;
#15730 = EDGE_CURVE ( 'NONE', #45237, #6205, #42348, .T. ) ;
#15731 = DIRECTION ( 'NONE',  ( -1.000000000000000000, 0.000000000000000000, 0.000000000000000000 ) ) ;
#15732 = VERTEX_POINT ( 'NONE', #32528 ) ;
#15733 = DIRECTION ( 'NONE',  ( -1.000000000000000000, 0.000000000000000000, -0.000000000000000000 ) ) ;
#15734 = CARTESIAN_POINT ( 'NONE',  ( -92.69370383062504004, 90.00000000000004263, 83.76906250086716454 ) ) ;
#15735 = CARTESIAN_POINT ( 'NONE',  ( 96.15314808468748708, 91.99731107132950569, 78.00114583420048575 ) ) ;
#15736 = ORIENTED_EDGE ( 'NONE', *, *, #69416, .F. ) ;
#15737 = DIRECTION ( 'NONE',  ( 0.000000000000000000, 0.000000000000000000, 1.000000000000000000 ) ) ;
#15738 = CIRCLE ( 'NONE', #44520, 31.99999999999999645 ) ;
#15739 = CARTESIAN_POINT ( 'NONE',  ( 10.00000000000000000, -4.992566952384716927, -37.16516213103282951 ) ) ;
#15740 = ORIENTED_EDGE ( 'NONE', *, *, #2446, .F. ) ;
#15741 = CARTESIAN_POINT ( 'NONE',  ( 5.999999999999999112, 71.21200624218795383, 40.65526001592638039 ) ) ;
#15742 = CIRCLE ( 'NONE', #3739, 26.50000000000000355 ) ;
#15743 = CARTESIAN_POINT ( 'NONE',  ( -97.30629616937497417, -208.6684592857803011, 82.60489583420047666 ) ) ;
#15744 = ORIENTED_EDGE ( 'NONE', *, *, #37519, .F. ) ;
#15745 = EDGE_LOOP ( 'NONE', ( #24780, #18493, #63713, #2280 ) ) ;
#15746 = CARTESIAN_POINT ( 'NONE',  ( 10.00000000000000000, -55.38113227695820484, 54.21277698773656084 ) ) ;
#15747 = ORIENTED_EDGE ( 'NONE', *, *, #23583, .F. ) ;
#15748 = CARTESIAN_POINT ( 'NONE',  ( 10.00000000000000000, 0.000000000000000000, 0.000000000000000000 ) ) ;
#15749 = CARTESIAN_POINT ( 'NONE',  ( -97.51367041768831712, -210.0000000000000284, 74.91808492278045151 ) ) ;
#15750 = VERTEX_POINT ( 'NONE', #66025 ) ;
#15751 = CARTESIAN_POINT ( 'NONE',  ( -92.69370383062498320, -209.9999999999999716, 81.07031250086714635 ) ) ;
#15752 = ORIENTED_EDGE ( 'NONE', *, *, #44063, .F. ) ;
#15753 = DIRECTION ( 'NONE',  ( -1.000000000000000000, 0.000000000000000000, 0.000000000000000000 ) ) ;
#15754 = LINE ( 'NONE', #46190, #70457 ) ;
#15755 = FACE_OUTER_BOUND ( 'NONE', #43958, .T. ) ;
#15756 = DIRECTION ( 'NONE',  ( -1.000000000000000000, -0.000000000000000000, -0.000000000000000000 ) ) ;
#15757 = MECHANICAL_DESIGN_GEOMETRIC_PRESENTATION_REPRESENTATION (  '', ( #61378 ), #38562 ) ;
#15758 = DIRECTION ( 'NONE',  ( 0.1276937514489679404, 0.9918136447140103451, 0.000000000000000000 ) ) ;
#15759 = AXIS2_PLACEMENT_3D ( 'NONE', #24177, #62943, #57654 ) ;
#15760 = VECTOR ( 'NONE', #74186, 1000.000000000000000 ) ;
#15761 = DIRECTION ( 'NONE',  ( 0.000000000000000000, 0.000000000000000000, 1.000000000000000000 ) ) ;
#15762 = CARTESIAN_POINT ( 'NONE',  ( 92.69370383062498320, 88.66845928578035796, 87.15572916753380639 ) ) ;
#15763 = CARTESIAN_POINT ( 'NONE',  ( -7.572224309238338336, -145.4393675041377492, 5.500000000000000000 ) ) ;
#15764 = AXIS2_PLACEMENT_3D ( 'NONE', #37432, #49061, #26865 ) ;
#15765 = DIRECTION ( 'NONE',  ( -0.4279312458752990711, -0.9038112904824846527, 0.000000000000000000 ) ) ;
#15766 = CARTESIAN_POINT ( 'NONE',  ( -2.499999999999970690, 73.00000000000001421, -201.6999999999999886 ) ) ;
#15767 = DIRECTION ( 'NONE',  ( -0.000000000000000000, 0.9781476007338067991, 0.2079116908177533474 ) ) ;
#15768 = CARTESIAN_POINT ( 'NONE',  ( 10.00000000000000000, 37.48860685352291000, -0.8828120875901940279 ) ) ;
#15769 = CARTESIAN_POINT ( 'NONE',  ( 0.000000000000000000, 55.20638768913831029, -51.02545421589267960 ) ) ;
#15770 = DIRECTION ( 'NONE',  ( 0.000000000000000000, 0.000000000000000000, 1.000000000000000000 ) ) ;
#15771 = DIRECTION ( 'NONE',  ( 1.000000000000000000, 0.000000000000000000, 0.000000000000000000 ) ) ;
#15772 = CARTESIAN_POINT ( 'NONE',  ( 5.000000000000000000, 2.886751345948137981, -5.553418012614792509 ) ) ;
#15773 = EDGE_CURVE ( 'NONE', #21881, #3726, #43477, .T. ) ;
#15774 = CARTESIAN_POINT ( 'NONE',  ( 0.9774260708577211521, -121.1378217241763622, -2.500000000000000000 ) ) ;
#15775 = DIRECTION ( 'NONE',  ( 1.000000000000000000, 0.000000000000000000, 0.000000000000000000 ) ) ;
#15776 = EDGE_CURVE ( 'NONE', #2169, #2136, #60750, .T. ) ;
#15777 = CARTESIAN_POINT ( 'NONE',  ( -96.32499999999996021, -212.2949673200287179, 85.02583333333332405 ) ) ;
#15778 = EDGE_CURVE ( 'NONE', #56906, #9702, #60459, .T. ) ;
#15779 = EDGE_CURVE ( 'NONE', #71157, #1966, #14498, .T. ) ;
#15780 = DIRECTION ( 'NONE',  ( 0.000000000000000000, 0.000000000000000000, 1.000000000000000000 ) ) ;
#15781 = PRODUCT_DEFINITION_SHAPE ( 'NONE', 'NONE',  #11351 ) ;
#15782 = ADVANCED_FACE ( 'NONE', ( #14875 ), #37820, .T. ) ;
#15783 = ORIENTED_EDGE ( 'NONE', *, *, #44646, .F. ) ;
#15784 = CARTESIAN_POINT ( 'NONE',  ( 15.00000000000000000, -13.04903810567646971, 19.60159698893442481 ) ) ;
#15785 = CARTESIAN_POINT ( 'NONE',  ( 0.000000000000000000, -65.58780272294048075, -36.73666225445966660 ) ) ;
#15786 = PLANE ( 'NONE',  #50209 ) ;
#15787 = DIRECTION ( 'NONE',  ( -1.000000000000000000, -0.000000000000000000, 0.000000000000000000 ) ) ;
#15788 = EDGE_CURVE ( 'NONE', #55514, #3975, #8119, .T. ) ;
#15789 = AXIS2_PLACEMENT_3D ( 'NONE', #1644, #11750, #34696 ) ;
#15790 = AXIS2_PLACEMENT_3D ( 'NONE', #1114, #36373, #7072 ) ;
#15791 = CARTESIAN_POINT ( 'NONE',  ( 95.00000000000000000, -207.3369185715606307, 87.73781250086715033 ) ) ;
#15792 = VECTOR ( 'NONE', #57662, 1000.000000000000000 ) ;
#15793 = VERTEX_POINT ( 'NONE', #31423 ) ;
#15794 = ORIENTED_EDGE ( 'NONE', *, *, #6291, .F. ) ;
#15795 = DIRECTION ( 'NONE',  ( -1.000000000000000000, 0.000000000000000000, 0.000000000000000000 ) ) ;
#15796 = PLANE ( 'NONE',  #53547 ) ;
#15797 = EDGE_LOOP ( 'NONE', ( #31605, #58435 ) ) ;
#15798 =( REPRESENTATION_RELATIONSHIP ('NONE','NONE', #31117, #33525 ) REPRESENTATION_RELATIONSHIP_WITH_TRANSFORMATION ( #72 )SHAPE_REPRESENTATION_RELATIONSHIP( ) );
#15799 = CARTESIAN_POINT ( 'NONE',  ( 96.15314808468750130, -211.9973110713294489, 78.42447916753381776 ) ) ;
#15800 = CARTESIAN_POINT ( 'NONE',  ( 96.15314808468750130, -211.9973110713294489, 85.56822916753381492 ) ) ;
#15802 = VERTEX_POINT ( 'NONE', #54364 ) ;
#15801 = ADVANCED_FACE ( 'NONE', ( #65284 ), #8868, .F. ) ;
#15803 = CARTESIAN_POINT ( 'NONE',  ( 93.84685191531249870, -208.0026889286704943, 86.52072916753382970 ) ) ;
#15804 = ORIENTED_EDGE ( 'NONE', *, *, #9917, .F. ) ;
#15805 = DIRECTION ( 'NONE',  ( 0.000000000000000000, 0.000000000000000000, 1.000000000000000000 ) ) ;
#15806 = ORIENTED_EDGE ( 'NONE', *, *, #70363, .F. ) ;
#15807 = CIRCLE ( 'NONE', #9848, 12.49999999999999645 ) ;
#15808 = ADVANCED_FACE ( 'NONE', ( #8504 ), #48715, .T. ) ;
#15809 = EDGE_CURVE ( 'NONE', #19207, #67486, #49084, .T. ) ;
#15810 = CARTESIAN_POINT ( 'NONE',  ( 18.80329974962065265, -105.8248132807389084, 5.500000000000000000 ) ) ;
#15811 = AXIS2_PLACEMENT_3D ( 'NONE', #72031, #26544, #65669 ) ;
#15812 = EDGE_LOOP ( 'NONE', ( #47813, #3748, #16167, #34285 ) ) ;
#15813 = DIRECTION ( 'NONE',  ( 1.000000000000000000, 0.000000000000000000, 0.000000000000000000 ) ) ;
#15814 = AXIS2_PLACEMENT_3D ( 'NONE', #4711, #22733, #23462 ) ;
#15815 = ORIENTED_EDGE ( 'NONE', *, *, #14958, .T. ) ;
#15816 = CARTESIAN_POINT ( 'NONE',  ( -3.000000000000000000, -22.32062822937469804, -14.36278369418829826 ) ) ;
#15817 = DIRECTION ( 'NONE',  ( 0.000000000000000000, 0.000000000000000000, -1.000000000000000000 ) ) ;
#15818 = ORIENTED_EDGE ( 'NONE', *, *, #5734, .F. ) ;
#15819 = DIRECTION ( 'NONE',  ( -1.000000000000000000, 0.000000000000000000, 0.000000000000000000 ) ) ;
#15820 = ADVANCED_FACE ( 'NONE', ( #49455 ), #42714, .T. ) ;
#15821 = ORIENTED_EDGE ( 'NONE', *, *, #13392, .F. ) ;
#15822 = CARTESIAN_POINT ( 'NONE',  ( 10.00000000000000000, -30.00120703465222149, 22.64427369931158296 ) ) ;
#15823 = ORIENTED_EDGE ( 'NONE', *, *, #59180, .T. ) ;
#15824 = B_SPLINE_CURVE_WITH_KNOTS ( 'NONE', 3,
 ( #57636, #29042, #64014, #12489, #520, #23414 ),
 .UNSPECIFIED., .F., .F.,
 ( 4, 2, 4 ),
 ( 0.7528176110417461597, 0.8153862273023197993, 0.8779548435628933278 ),
 .UNSPECIFIED. ) ;
#15825 = ORIENTED_EDGE ( 'NONE', *, *, #60469, .T. ) ;
#15826 = ORIENTED_EDGE ( 'NONE', *, *, #68832, .F. ) ;
#15827 = DIRECTION ( 'NONE',  ( 0.000000000000000000, 0.9510565162951544194, -0.3090169943749446757 ) ) ;
#15828 = CONTEXT_DEPENDENT_SHAPE_REPRESENTATION ( #21052, #877 ) ;
#15829 = FACE_BOUND ( 'NONE', #17372, .T. ) ;
#15830 = ORIENTED_EDGE ( 'NONE', *, *, #23785, .F. ) ;
#15831 = EDGE_LOOP ( 'NONE', ( #57361, #24133, #27987, #64346 ) ) ;
#15832 = EDGE_LOOP ( 'NONE', ( #16776, #33086, #3674, #69516 ) ) ;
#15833 = DIRECTION ( 'NONE',  ( -0.000000000000000000, -0.000000000000000000, 1.000000000000000000 ) ) ;
#15834 = CARTESIAN_POINT ( 'NONE',  ( 5.999999999999999112, 56.15606465355041621, -59.75363087400017292 ) ) ;
#15835 = CARTESIAN_POINT ( 'NONE',  ( -95.73425683495055694, 85.91408486779589282, 74.64692065633565221 ) ) ;
#15836 = ORIENTED_EDGE ( 'NONE', *, *, #24508, .F. ) ;
#15837 = CARTESIAN_POINT ( 'NONE',  ( 94.99999999999998579, 87.33691857156068750, 77.10156250086711793 ) ) ;
#15838 = VERTEX_POINT ( 'NONE', #66754 ) ;
#15839 = DIRECTION ( 'NONE',  ( 0.000000000000000000, 0.9135454576426063067, -0.4067366430757881068 ) ) ;
#15840 = DIRECTION ( 'NONE',  ( 0.000000000000000000, -0.1045284632676449221, 0.9945218953682741780 ) ) ;
#15841 = ORIENTED_EDGE ( 'NONE', *, *, #6378, .F. ) ;
#15842 = CARTESIAN_POINT ( 'NONE',  ( 96.66135172262730180, -211.6008015735635865, 74.79754476654878204 ) ) ;
#15843 = DIRECTION ( 'NONE',  ( -1.000000000000000000, -0.000000000000000000, 0.000000000000000000 ) ) ;
#15844 = CARTESIAN_POINT ( 'NONE',  ( 11.99999999999999822, 0.000000000000000000, 0.000000000000000000 ) ) ;
#15845 = CARTESIAN_POINT ( 'NONE',  ( -93.84685191531248449, -208.0026889286704943, 79.27114583420046756 ) ) ;
#15846 = VECTOR ( 'NONE', #72510, 1000.000000000000114 ) ;
#15847 = DIRECTION ( 'NONE',  ( -1.000000000000000000, 0.000000000000000000, 0.000000000000000000 ) ) ;
#15848 = DIRECTION ( 'NONE',  ( 0.8774505977381971134, 0.4796670183876317051, -0.000000000000000000 ) ) ;
#15849 = DIRECTION ( 'NONE',  ( 0.000000000000000000, -0.8910065241883626808, -0.4539904997395568520 ) ) ;
#15850 = ORIENTED_EDGE ( 'NONE', *, *, #73943, .F. ) ;
#15851 = TOROIDAL_SURFACE ( 'NONE', #67475, 20.69999999999999929, 0.2999999999999981570 ) ;
#15852 = VERTEX_POINT ( 'NONE', #14120 ) ;
#15853 = CARTESIAN_POINT ( 'NONE',  ( 5.999999999999999112, 74.74816331893477184, -33.71516098798660011 ) ) ;
#15854 = DIRECTION ( 'NONE',  ( 1.000000000000000000, 0.000000000000000000, -0.000000000000000000 ) ) ;
#15855 = CARTESIAN_POINT ( 'NONE',  ( 92.49008991410272529, -209.8784921249854563, 74.91582548749271098 ) ) ;
#15856 = VECTOR ( 'NONE', #43241, 1000.000000000000000 ) ;
#15857 = CARTESIAN_POINT ( 'NONE',  ( -95.00000000000002842, 87.33691857156074434, 81.54656250086715374 ) ) ;
#15858 = CARTESIAN_POINT ( 'NONE',  ( -12.50000000000000000, -120.0000000000000000, -40.00000000000000711 ) ) ;
#15859 = DIRECTION ( 'NONE',  ( -1.000000000000000000, 0.000000000000000000, 0.000000000000000000 ) ) ;
#15860 = VECTOR ( 'NONE', #34399, 1000.000000000000000 ) ;
#15861 =( BOUNDED_CURVE ( )  B_SPLINE_CURVE ( 2, ( #19377, #64514, #12992, #47960, #69773, #52478, #53232 ),
 .UNSPECIFIED., .F., .F. ) 
 B_SPLINE_CURVE_WITH_KNOTS ( ( 3, 2, 2, 3 ),
 ( 0.6773535682752295228, 0.6844092574655884498, 0.6914650230064715020, 0.6985206468843488947 ),
 .UNSPECIFIED. ) 
 CURVE ( )  GEOMETRIC_REPRESENTATION_ITEM ( )  RATIONAL_B_SPLINE_CURVE ( ( 0.9999971005499255217, 0.8660268535251636202, 1.000000000000000000, 0.8660254037844387076, 1.000000000000000000, 0.8660280936759700010, 0.9999946203249505672 ) ) 
 REPRESENTATION_ITEM ( '' )  );
#15862 = ORIENTED_EDGE ( 'NONE', *, *, #62118, .T. ) ;
#15863 = CARTESIAN_POINT ( 'NONE',  ( -3.000000000000000000, 16.83928648764945279, -16.46020748918028076 ) ) ;
#15864 = FACE_OUTER_BOUND ( 'NONE', #14961, .T. ) ;
#15865 = CARTESIAN_POINT ( 'NONE',  ( 6.000000000000000000, 71.87247863392413194, 39.47590169984871267 ) ) ;
#15866 = AXIS2_PLACEMENT_3D ( 'NONE', #62639, #4376, #34039 ) ;
#15867 = EDGE_CURVE ( 'NONE', #12556, #65739, #70042, .T. ) ;
#15868 = DIRECTION ( 'NONE',  ( 0.000000000000000000, 0.000000000000000000, 1.000000000000000000 ) ) ;
#15869 = CARTESIAN_POINT ( 'NONE',  ( 10.00000000000000000, -27.75498641678764855, 31.52238457039589647 ) ) ;
#15870 = CARTESIAN_POINT ( 'NONE',  ( -96.15314808468747287, -208.0026889286704943, 79.53572916753381605 ) ) ;
#15871 = EDGE_CURVE ( 'NONE', #9438, #47803, #24384, .T. ) ;
#15872 = ADVANCED_FACE ( 'NONE', ( #5104 ), #39677, .T. ) ;
#15873 = DIRECTION ( 'NONE',  ( 0.000000000000000000, 0.000000000000000000, 1.000000000000000000 ) ) ;
#15874 = VERTEX_POINT ( 'NONE', #73117 ) ;
#15875 = DIRECTION ( 'NONE',  ( 0.000000000000000000, 0.000000000000000000, 1.000000000000000000 ) ) ;
#15876 = DIRECTION ( 'NONE',  ( 1.000000000000000000, 0.000000000000000000, -0.000000000000000000 ) ) ;
#15877 = CARTESIAN_POINT ( 'NONE',  ( -97.64999999999996305, -209.9999999999999716, 90.00000000000000000 ) ) ;
#15878 = ORIENTED_EDGE ( 'NONE', *, *, #26134, .F. ) ;
#15879 = DIRECTION ( 'NONE',  ( -1.000000000000000000, 0.000000000000000000, -0.000000000000000000 ) ) ;
#15880 = DIRECTION ( 'NONE',  ( 0.000000000000000000, -0.9876883405951394357, 0.1564344650402203496 ) ) ;
#15881 = DIRECTION ( 'NONE',  ( 0.000000000000000000, 0.000000000000000000, -1.000000000000000000 ) ) ;
#15882 = ADVANCED_FACE ( 'NONE', ( #50183 ), #10346, .F. ) ;
#15883 = VERTEX_POINT ( 'NONE', #38925 ) ;
#15884 = DIRECTION ( 'NONE',  ( 0.7585478161175723821, 0.6516173805718057377, -0.000000000000000000 ) ) ;
#15885 = ORIENTED_EDGE ( 'NONE', *, *, #51192, .F. ) ;
#15886 = CARTESIAN_POINT ( 'NONE',  ( 93.84685191531249870, -208.0026889286704943, 87.63197916753379957 ) ) ;
#15887 = CARTESIAN_POINT ( 'NONE',  ( -7.893099573151324044, -11.68370571044642503, -1.199999999999999956 ) ) ;
#15888 = VERTEX_POINT ( 'NONE', #16740 ) ;
#15889 = DIRECTION ( 'NONE',  ( 0.000000000000000000, -0.3090169943749548342, 0.9510565162951511997 ) ) ;
#15890 = VERTEX_POINT ( 'NONE', #45696 ) ;
#15891 = DIRECTION ( 'NONE',  ( 0.000000000000000000, 0.000000000000000000, 1.000000000000000000 ) ) ;
#15892 = ADVANCED_FACE ( 'NONE', ( #11094 ), #56600, .T. ) ;
#15893 = EDGE_CURVE ( 'NONE', #67479, #10604, #28000, .T. ) ;
#15894 = CARTESIAN_POINT ( 'NONE',  ( 0.000000000000000000, 0.000000000000000000, 0.000000000000000000 ) ) ;
#15895 = ORIENTED_EDGE ( 'NONE', *, *, #4510, .F. ) ;
#15896 = VERTEX_POINT ( 'NONE', #49817 ) ;
#15897 = EDGE_LOOP ( 'NONE', ( #31282, #39954, #35407, #48917 ) ) ;
#15898 = CARTESIAN_POINT ( 'NONE',  ( 0.000000000000000000, 0.000000000000000000, 0.000000000000000000 ) ) ;
#15899 = AXIS2_PLACEMENT_3D ( 'NONE', #62003, #3385, #72513 ) ;
#15900 = EDGE_LOOP ( 'NONE', ( #74324, #62979, #38683, #6195 ) ) ;
#15901 = AXIS2_PLACEMENT_3D ( 'NONE', #1823, #65681, #30342 ) ;
#15902 = ORIENTED_EDGE ( 'NONE', *, *, #45678, .T. ) ;
#15903 = CARTESIAN_POINT ( 'NONE',  ( 97.30629616937498838, 88.66845928578037217, 76.09614583420048461 ) ) ;
#15904 = DIRECTION ( 'NONE',  ( -1.000000000000000000, -0.000000000000000000, -0.000000000000000000 ) ) ;
#15905 = PLANE ( 'NONE',  #50091 ) ;
#15906 = EDGE_LOOP ( 'NONE', ( #37945, #70321, #33393, #47519 ) ) ;
#15907 = EDGE_LOOP ( 'NONE', ( #1046, #5292, #66135, #31627 ) ) ;
#15908 = VERTEX_POINT ( 'NONE', #61861 ) ;
#15909 = CARTESIAN_POINT ( 'NONE',  ( -10.00000000000000000, 0.000000000000000000, 0.000000000000000000 ) ) ;
#15910 = AXIS2_PLACEMENT_3D ( 'NONE', #17558, #17196, #63811 ) ;
#15911 = ORIENTED_EDGE ( 'NONE', *, *, #23338, .T. ) ;
#15912 = CARTESIAN_POINT ( 'NONE',  ( 92.69370383062501162, -208.6684592857803011, 84.50989583420046358 ) ) ;
#15913 = VECTOR ( 'NONE', #27868, 1000.000000000000114 ) ;
#15914 = APPLICATION_PROTOCOL_DEFINITION ( 'draft international standard', 'automotive_design', 1998, #26763 ) ;
#15915 = CARTESIAN_POINT ( 'NONE',  ( -1.459549131277904976, -119.6539995182286304, 2.500000000000000000 ) ) ;
#15916 = CARTESIAN_POINT ( 'NONE',  ( 10.00000000000000000, 73.72996012237440766, 14.67089635893739619 ) ) ;
#15917 = PLANE ( 'NONE',  #62970 ) ;
#15918 = DIRECTION ( 'NONE',  ( 0.000000000000000000, 0.9723699203976756689, 0.2334453638559094157 ) ) ;
#15919 = DIRECTION ( 'NONE',  ( -1.000000000000000000, -0.000000000000000000, -0.000000000000000000 ) ) ;
#15920 = CARTESIAN_POINT ( 'NONE',  ( 15.00000000000000000, 16.61724383029361718, -20.69703378468926402 ) ) ;
#15921 = CARTESIAN_POINT ( 'NONE',  ( -92.69370383062498320, -209.9999999999999716, 88.69031250086715090 ) ) ;
#15922 = CARTESIAN_POINT ( 'NONE',  ( -92.69370383062502583, 88.66845928578038638, 86.89114583420050053 ) ) ;
#15923 = ORIENTED_EDGE ( 'NONE', *, *, #34224, .F. ) ;
#15925 = CARTESIAN_POINT ( 'NONE',  ( -97.30629616937501680, 91.33154071421968467, 86.41489583420047893 ) ) ;
#15924 = CARTESIAN_POINT ( 'NONE',  ( 97.30629616937498838, 88.66845928578037217, 89.27239583420048064 ) ) ;
#15926 = ORIENTED_EDGE ( 'NONE', *, *, #5370, .F. ) ;
#15927 = CARTESIAN_POINT ( 'NONE',  ( 10.00000000000000000, -71.91182617369207719, 28.89263327155721228 ) ) ;
#15928 = CYLINDRICAL_SURFACE ( 'NONE', #9724, 31.99999999999998579 ) ;
#15929 = FACE_OUTER_BOUND ( 'NONE', #6235, .T. ) ;
#15930 = CARTESIAN_POINT ( 'NONE',  ( -97.30629616937497417, -211.3315407142195852, 89.06072916753382174 ) ) ;
#15931 = CARTESIAN_POINT ( 'NONE',  ( -3.000000000000000000, -18.13022148937263012, 15.02647892043544608 ) ) ;
#15932 = DIRECTION ( 'NONE',  ( -1.000000000000000000, 0.000000000000000000, 0.000000000000000000 ) ) ;
#15933 = DIRECTION ( 'NONE',  ( 0.000000000000000000, 0.000000000000000000, -1.000000000000000000 ) ) ;
#15934 = ORIENTED_EDGE ( 'NONE', *, *, #15893, .F. ) ;
#15935 = ORIENTED_EDGE ( 'NONE', *, *, #13651, .T. ) ;
#15936 = CARTESIAN_POINT ( 'NONE',  ( -96.32500000000001705, 87.70503267997129626, 82.48583333333333201 ) ) ;
#15937 = DIRECTION ( 'NONE',  ( -1.000000000000000000, 0.000000000000000000, 0.000000000000000000 ) ) ;
#15938 = LINE ( 'NONE', #38878, #6994 ) ;
#15939 = FACE_OUTER_BOUND ( 'NONE', #66034, .T. ) ;
#15940 = DIRECTION ( 'NONE',  ( 0.000000000000000000, 0.6494480483301849905, -0.7604059656000298206 ) ) ;
#15941 = CARTESIAN_POINT ( 'NONE',  ( 10.00000000000000000, -74.65491531819111515, 23.16904090965678975 ) ) ;
#15942 = DIRECTION ( 'NONE',  ( 1.000000000000000000, 0.000000000000000000, 0.000000000000000000 ) ) ;
#15943 = CYLINDRICAL_SURFACE ( 'NONE', #11982, 16.00000000000000000 ) ;
#15944 = ORIENTED_EDGE ( 'NONE', *, *, #19674, .T. ) ;
#15945 = PRODUCT_RELATED_PRODUCT_CATEGORY ( 'part', '', ( #62027 ) ) ;
#15946 = CARTESIAN_POINT ( 'NONE',  ( -92.69370383062504004, 90.00000000000004263, 81.07031250086714635 ) ) ;
#15947 = EDGE_CURVE ( 'NONE', #70917, #16273, #51304, .T. ) ;
#15948 = COLOUR_RGB ( '', 0.40784314, 0.44705882, 0.49803922) ;
#15949 = CARTESIAN_POINT ( 'NONE',  ( 92.35000000039362078, 90.00002930319625705, 82.45844277051448046 ) ) ;
#15950 = DIRECTION ( 'NONE',  ( -1.000000000000000000, 0.000000000000000000, -0.000000000000000000 ) ) ;
#15951 = CARTESIAN_POINT ( 'NONE',  ( 11.99999999999999822, 14.67089635893819377, -73.72996012237423713 ) ) ;
#15952 = EDGE_CURVE ( 'NONE', #52714, #12392, #73639, .T. ) ;
#15953 = DIRECTION ( 'NONE',  ( 1.000000000000000000, 0.000000000000000000, 0.000000000000000000 ) ) ;
#15954 = CARTESIAN_POINT ( 'NONE',  ( 10.00000000000000000, -21.53537804866103045, 30.80686688397002371 ) ) ;
#15955 = CARTESIAN_POINT ( 'NONE',  ( -96.15314808468747287, -208.0026889286704943, 89.69572916753382685 ) ) ;
#15956 = EDGE_CURVE ( 'NONE', #39383, #34204, #46026, .T. ) ;
#15957 = CIRCLE ( 'NONE', #33932, 31.99999999999999289 ) ;
#15958 = EDGE_CURVE ( 'NONE', #53342, #4680, #17194, .T. ) ;
#15959 = CARTESIAN_POINT ( 'NONE',  ( 94.99999999999998579, 92.66308142843932671, 81.38781250086715602 ) ) ;
#15960 = CARTESIAN_POINT ( 'NONE',  ( -92.69370383062498320, -211.3315407142195852, 83.71614583420048916 ) ) ;
#15961 = CYLINDRICAL_SURFACE ( 'NONE', #38572, 32.00000000000000000 ) ;
#15962 = VERTEX_POINT ( 'NONE', #21238 ) ;
#15963 = DIRECTION ( 'NONE',  ( 0.000000000000000000, 0.000000000000000000, 1.000000000000000000 ) ) ;
#15964 = CARTESIAN_POINT ( 'NONE',  ( -96.32499999999996021, -207.7050326799711968, 76.55916666666666970 ) ) ;
#15965 = DIRECTION ( 'NONE',  ( -1.000000000000000000, 0.000000000000000000, 0.000000000000000000 ) ) ;
#15966 = CIRCLE ( 'NONE', #66378, 12.50000000000022560 ) ;
#15967 = CARTESIAN_POINT ( 'NONE',  ( -92.69370383062505425, 88.66845928578038638, 78.63614583420046245 ) ) ;
#15969 = EDGE_CURVE ( 'NONE', #11647, #52639, #56966, .T. ) ;
#15968 = CARTESIAN_POINT ( 'NONE',  ( 92.69370383062501162, -211.3315407142195852, 80.17072916753379275 ) ) ;
#15970 = ORIENTED_EDGE ( 'NONE', *, *, #51700, .T. ) ;
#15971 = EDGE_CURVE ( 'NONE', #7975, #61324, #44193, .T. ) ;
#15972 = CARTESIAN_POINT ( 'NONE',  ( 0.000000000000000000, 0.000000000000000000, 0.000000000000000000 ) ) ;
#15973 = ORIENTED_EDGE ( 'NONE', *, *, #8845, .F. ) ;
#15974 = CARTESIAN_POINT ( 'NONE',  ( -92.35000000000177067, -209.9999969335172807, 75.79187510780353421 ) ) ;
#15975 = ORIENTED_EDGE ( 'NONE', *, *, #1047, .F. ) ;
#15976 = DIRECTION ( 'NONE',  ( 1.000000000000000000, 0.000000000000000000, 0.000000000000000000 ) ) ;
#15977 = ADVANCED_FACE ( 'NONE', ( #68623 ), #18124, .T. ) ;
#15978 = ORIENTED_EDGE ( 'NONE', *, *, #68668, .T. ) ;
#15979 = EDGE_LOOP ( 'NONE', ( #31586, #54749, #53526, #43146 ) ) ;
#15980 = VERTEX_POINT ( 'NONE', #16359 ) ;
#15981 = CARTESIAN_POINT ( 'NONE',  ( 97.30629616937498838, -208.6684592857803295, 74.93197916753381094 ) ) ;
#15982 = ORIENTED_EDGE ( 'NONE', *, *, #41841, .T. ) ;
#15983 = DIRECTION ( 'NONE',  ( -1.000000000000000000, -0.000000000000000000, 0.000000000000000000 ) ) ;
#15984 = AXIS2_PLACEMENT_3D ( 'NONE', #12256, #62683, #5164 ) ;
#15985 = CARTESIAN_POINT ( 'NONE',  ( 10.00000000000000000, 0.000000000000000000, 0.000000000000000000 ) ) ;
#15986 = CARTESIAN_POINT ( 'NONE',  ( 93.84685191531248449, 88.00268892867053694, 88.00239583420048461 ) ) ;
#15987 = CARTESIAN_POINT ( 'NONE',  ( 0.000000000000000000, -120.0000000000000000, -2.500000000000000000 ) ) ;
#15988 = CARTESIAN_POINT ( 'NONE',  ( 95.00000000000000000, -206.9400435732949575, 79.04625000000000057 ) ) ;
#15989 = ORIENTED_EDGE ( 'NONE', *, *, #5463, .F. ) ;
#15990 = PRODUCT_DEFINITION_FORMATION_WITH_SPECIFIED_SOURCE ( 'ANY', '', #55381, .NOT_KNOWN. ) ;
#15991 = ORIENTED_EDGE ( 'NONE', *, *, #20632, .F. ) ;
#15992 = VERTEX_POINT ( 'NONE', #12472 ) ;
#15993 = ORIENTED_EDGE ( 'NONE', *, *, #56987, .F. ) ;
#15994 = DIRECTION ( 'NONE',  ( 0.000000000000000000, 1.000000000000000000, 0.000000000000000000 ) ) ;
#15995 = AXIS2_PLACEMENT_3D ( 'NONE', #71536, #20037, #26780 ) ;
#15996 = CARTESIAN_POINT ( 'NONE',  ( 97.64999999999999147, -210.0000001051138270, 86.58687499784845443 ) ) ;
#15997 = CARTESIAN_POINT ( 'NONE',  ( 10.00000000000000000, 0.000000000000000000, 37.49900000000000233 ) ) ;
#15998 = DIRECTION ( 'NONE',  ( -0.000000000000000000, -0.000000000000000000, -1.000000000000000000 ) ) ;
#15999 = FACE_BOUND ( 'NONE', #55585, .T. ) ;
#16000 = LINE ( 'NONE', #61881, #17631 ) ;
#16001 = ORIENTED_EDGE ( 'NONE', *, *, #30803, .T. ) ;
#16002 = CARTESIAN_POINT ( 'NONE',  ( -92.34999999999999432, -209.9999999999999716, 82.14187500173429157 ) ) ;
#16003 = ORIENTED_EDGE ( 'NONE', *, *, #793, .F. ) ;
#16004 = DIRECTION ( 'NONE',  ( 0.000000000000000000, 0.000000000000000000, -1.000000000000000000 ) ) ;
#16005 = VERTEX_POINT ( 'NONE', #35411 ) ;
#16007 = CARTESIAN_POINT ( 'NONE',  ( -92.35000000000005116, 88.47002178664754979, 82.72395833506762131 ) ) ;
#16006 = CARTESIAN_POINT ( 'NONE',  ( 93.67499999999998295, 92.29496732002878900, 83.62354166840097491 ) ) ;
#16008 = AXIS2_PLACEMENT_3D ( 'NONE', #72379, #43837, #65647 ) ;
#16009 = VERTEX_POINT ( 'NONE', #39302 ) ;
#16010 = CARTESIAN_POINT ( 'NONE',  ( 97.30629616937498838, 90.00000000000002842, 83.13406250086715943 ) ) ;
#16011 = CIRCLE ( 'NONE', #4063, 3.000000000000000888 ) ;
#16012 = CARTESIAN_POINT ( 'NONE',  ( -97.30629616937501680, 90.00000000000004263, 89.80156250086714920 ) ) ;
#16014 = EDGE_CURVE ( 'NONE', #4375, #72136, #7587, .T. ) ;
#16013 = DIRECTION ( 'NONE',  ( -1.000000000000000000, 0.000000000000000000, 0.000000000000000000 ) ) ;
#16015 = CARTESIAN_POINT ( 'NONE',  ( 2.500000000000034639, 90.00000000000000000, -310.0000000000000000 ) ) ;
#16016 = CYLINDRICAL_SURFACE ( 'NONE', #58264, 32.00000000000000000 ) ;
#16017 = DIRECTION ( 'NONE',  ( 0.000000000000000000, 0.000000000000000000, 1.000000000000000000 ) ) ;
#16018 = VERTEX_POINT ( 'NONE', #38556 ) ;
#16019 = CARTESIAN_POINT ( 'NONE',  ( 15.69955575014939875, 0.001194404164567414856, -74.99999999999958789 ) ) ;
#16021 = DIRECTION ( 'NONE',  ( 0.4279312458753000703, 0.9038112904824842087, -0.000000000000000000 ) ) ;
#16020 = VECTOR ( 'NONE', #10117, 1000.000000000000000 ) ;
#16022 = AXIS2_PLACEMENT_3D ( 'NONE', #13901, #30826, #53037 ) ;
#16023 = CIRCLE ( 'NONE', #49648, 77.49899999999999523 ) ;
#16024 = DIRECTION ( 'NONE',  ( 0.000000000000000000, -0.8910065241883627918, -0.4539904997395570185 ) ) ;
#16025 = ORIENTED_EDGE ( 'NONE', *, *, #33334, .F. ) ;
#16026 = ORIENTED_EDGE ( 'NONE', *, *, #13151, .T. ) ;
#16027 = EDGE_CURVE ( 'NONE', #24755, #12738, #47244, .T. ) ;
#16028 = EDGE_CURVE ( 'NONE', #26970, #5289, #29193, .T. ) ;
#16029 = CARTESIAN_POINT ( 'NONE',  ( 0.000000000000000000, -37.01155633439053361, -6.555932627142825986 ) ) ;
#16030 = LINE ( 'NONE', #10392, #5414 ) ;
#16031 = DIRECTION ( 'NONE',  ( 0.000000000000000000, 0.8910065241883656784, 0.4539904997395510788 ) ) ;
#16032 = CARTESIAN_POINT ( 'NONE',  ( -93.84685191531248449, -208.0026889286704943, 79.42989583420049371 ) ) ;
#16033 = ORIENTED_EDGE ( 'NONE', *, *, #48740, .T. ) ;
#16034 = DIRECTION ( 'NONE',  ( -1.000000000000000000, -0.000000000000000000, 0.000000000000000000 ) ) ;
#16035 = ORIENTED_EDGE ( 'NONE', *, *, #47771, .F. ) ;
#16036 = VECTOR ( 'NONE', #52164, 1000.000000000000000 ) ;
#16037 = ADVANCED_FACE ( 'NONE', ( #69976 ), #24146, .F. ) ;
#16038 = DIRECTION ( 'NONE',  ( 1.000000000000000000, 0.000000000000000000, 0.000000000000000000 ) ) ;
#16039 = FACE_BOUND ( 'NONE', #32018, .T. ) ;
#16040 = CYLINDRICAL_SURFACE ( 'NONE', #70561, 31.99999999999998579 ) ;
#16041 = CARTESIAN_POINT ( 'NONE',  ( 97.30629616937498838, 90.00000000000002842, 75.35531250086714294 ) ) ;
#16042 = CARTESIAN_POINT ( 'NONE',  ( 11.99999999999999822, 0.000000000000000000, 0.000000000000000000 ) ) ;
#16043 = LINE ( 'NONE', #33315, #39689 ) ;
#16044 = DIRECTION ( 'NONE',  ( -1.000000000000000000, -0.000000000000000000, -0.000000000000000000 ) ) ;
#16045 = DIRECTION ( 'NONE',  ( 1.000000000000000000, 0.000000000000000000, 0.000000000000000000 ) ) ;
#16046 = CARTESIAN_POINT ( 'NONE',  ( 0.000000000000000000, 33.00180498840072829, -17.80606268964504935 ) ) ;
#16047 = PLANE ( 'NONE',  #25134 ) ;
#16048 = VECTOR ( 'NONE', #32502, 1000.000000000000000 ) ;
#16049 = EDGE_CURVE ( 'NONE', #12729, #66558, #18844, .T. ) ;
#16050 = CARTESIAN_POINT ( 'NONE',  ( 11.99999999999999822, 73.72996012237440766, 14.67089635893739619 ) ) ;
#16051 = LINE ( 'NONE', #65803, #70643 ) ;
#16052 = VECTOR ( 'NONE', #43356, 1000.000000000000000 ) ;
#16053 = EDGE_LOOP ( 'NONE', ( #22098, #7950, #73687, #38315 ) ) ;
#16054 = CARTESIAN_POINT ( 'NONE',  ( 10.00000000000000000, 0.000000000000000000, 0.000000000000000000 ) ) ;
#16055 = DIRECTION ( 'NONE',  ( 0.000000000000000000, 0.4539904997395479702, -0.8910065241883673437 ) ) ;
#16056 = VERTEX_POINT ( 'NONE', #52701 ) ;
#16057 = B_SPLINE_CURVE_WITH_KNOTS ( 'NONE', 1,
 ( #8521, #9624 ),
 .UNSPECIFIED., .F., .F.,
 ( 2, 2 ),
 ( 0.000000000000000000, 1.000000000000000000 ),
 .UNSPECIFIED. ) ;
#16058 = CARTESIAN_POINT ( 'NONE',  ( -92.69370383062504004, 90.00000000000004263, 82.34031250086714238 ) ) ;
#16059 = CIRCLE ( 'NONE', #25662, 77.49899999999999523 ) ;
#16061 = EDGE_CURVE ( 'NONE', #60419, #27599, #47794, .T. ) ;
#16060 = DIRECTION ( 'NONE',  ( -1.000000000000000000, 0.000000000000000000, 0.000000000000000000 ) ) ;
#16062 = EDGE_CURVE ( 'NONE', #62527, #30795, #25607, .T. ) ;
#16063 = ORIENTED_EDGE ( 'NONE', *, *, #30769, .T. ) ;
#16064 =( BOUNDED_CURVE ( )  B_SPLINE_CURVE ( 2, ( #48187, #7232, #42923, #71097, #14341, #42550, #37290 ),
 .UNSPECIFIED., .F., .F. ) 
 B_SPLINE_CURVE_WITH_KNOTS ( ( 3, 2, 2, 3 ),
 ( 0.5208333333333332593, 0.5277777777777776791, 0.5347222222222220989, 0.5416666666666665186 ),
 .UNSPECIFIED. ) 
 CURVE ( )  GEOMETRIC_REPRESENTATION_ITEM ( )  RATIONAL_B_SPLINE_CURVE ( ( 1.000000000000002220, 0.8660254037844365982, 1.000000000000000000, 0.8660254037844387076, 1.000000000000000000, 0.8660254037844408170, 0.9999999999999978906 ) ) 
 REPRESENTATION_ITEM ( '' )  );
#16065 = DIRECTION ( 'NONE',  ( 1.000000000000000000, 0.000000000000000000, 0.000000000000000000 ) ) ;
#16066 = EDGE_CURVE ( 'NONE', #7862, #1439, #41421, .T. ) ;
#16068 = DIRECTION ( 'NONE',  ( -1.000000000000000000, 0.000000000000000000, 0.000000000000000000 ) ) ;
#16067 = AXIS2_PLACEMENT_3D ( 'NONE', #49063, #9590, #66008 ) ;
#16069 = CARTESIAN_POINT ( 'NONE',  ( 11.99999999999999822, -2.946379043146863719, 75.11764819372146462 ) ) ;
#16070 = VECTOR ( 'NONE', #45000, 1000.000000000000000 ) ;
#16071 = DIRECTION ( 'NONE',  ( -0.000000000000000000, 0.5000000000000039968, -0.8660254037844363761 ) ) ;
#16072 = CIRCLE ( 'NONE', #40119, 16.00000000000000000 ) ;
#16073 = CARTESIAN_POINT ( 'NONE',  ( 97.30629616937498838, -211.3315407142195852, 78.63614583420049087 ) ) ;
#16074 = ORIENTED_EDGE ( 'NONE', *, *, #42713, .T. ) ;
#16075 = ORIENTED_EDGE ( 'NONE', *, *, #5722, .T. ) ;
#16076 = DIRECTION ( 'NONE',  ( -0.000000000000000000, -0.000000000000000000, 1.000000000000000000 ) ) ;
#16077 = DIRECTION ( 'NONE',  ( 0.000000000000000000, -0.9510565162951503115, -0.3090169943749573878 ) ) ;
#16078 = LINE ( 'NONE', #4078, #56851 ) ;
#16079 =( BOUNDED_CURVE ( )  B_SPLINE_CURVE ( 2, ( #36917, #30525, #54223, #65874, #2754, #54947, #31639 ),
 .UNSPECIFIED., .F., .F. ) 
 B_SPLINE_CURVE_WITH_KNOTS ( ( 3, 2, 2, 3 ),
 ( 0.8541666666666666297, 0.8611111111111110494, 0.8680555555555554692, 0.8749999999999997780 ),
 .UNSPECIFIED. ) 
 CURVE ( )  GEOMETRIC_REPRESENTATION_ITEM ( )  RATIONAL_B_SPLINE_CURVE ( ( 1.000000000000000000, 0.8660254037844387076, 1.000000000000000000, 0.8660254037844387076, 1.000000000000000000, 0.8660254037844430375, 0.9999999999999956701 ) ) 
 REPRESENTATION_ITEM ( '' )  );
#16080 = DIRECTION ( 'NONE',  ( -1.000000000000000000, 0.000000000000000000, 0.000000000000000000 ) ) ;
#16081 = DIRECTION ( 'NONE',  ( -1.000000000000000000, 0.000000000000000000, 0.000000000000000000 ) ) ;
#16082 = CARTESIAN_POINT ( 'NONE',  ( 93.67500000000001137, -212.2949673200287179, 88.20083333333332121 ) ) ;
#16083 = ORIENTED_EDGE ( 'NONE', *, *, #48819, .F. ) ;
#16084 = CARTESIAN_POINT ( 'NONE',  ( 0.000000000000000000, 0.000000000000000000, 0.000000000000000000 ) ) ;
#16085 = ORIENTED_EDGE ( 'NONE', *, *, #17382, .F. ) ;
#16086 = EDGE_LOOP ( 'NONE', ( #24951, #22707, #12113, #43496 ) ) ;
#16087 = CARTESIAN_POINT ( 'NONE',  ( 10.00000000000000000, 68.55367621811141987, 44.99326035066078333 ) ) ;
#16088 = SHAPE_REPRESENTATION_RELATIONSHIP ( 'NONE' , 'NONE' ,  #27826, #47128 ) ;
#16089 = DIRECTION ( 'NONE',  ( -1.000000000000000000, 0.000000000000000000, -0.000000000000000000 ) ) ;
#16090 = EDGE_LOOP ( 'NONE', ( #39134, #689, #64984, #22017 ) ) ;
#16091 = CARTESIAN_POINT ( 'NONE',  ( -2.500000000000015543, -73.00000000000001421, -258.2999999999999545 ) ) ;
#16092 = CARTESIAN_POINT ( 'NONE',  ( 97.64999999999997726, -211.5299782133524502, 81.45395833506763950 ) ) ;
#16093 = CARTESIAN_POINT ( 'NONE',  ( 94.99999999999998579, 93.05995642670504253, 81.58624999999999261 ) ) ;
#16094 = VERTEX_POINT ( 'NONE', #6834 ) ;
#16095 = EDGE_LOOP ( 'NONE', ( #10099, #67814, #62626, #10909 ) ) ;
#16096 = CARTESIAN_POINT ( 'NONE',  ( -10.43921258969510824, -98.89258801967538659, 5.500000000000000000 ) ) ;
#16097 = VECTOR ( 'NONE', #8912, 1000.000000000000000 ) ;
#16098 = VERTEX_POINT ( 'NONE', #65476 ) ;
#16099 = CARTESIAN_POINT ( 'NONE',  ( 92.35000000019411459, 89.99998015682159291, 84.36502760998348549 ) ) ;
#16100 = CARTESIAN_POINT ( 'NONE',  ( -97.30629616937501680, 91.33154071421968467, 84.66864583420047552 ) ) ;
#16101 = CARTESIAN_POINT ( 'NONE',  ( 97.30629616937498838, 88.66845928578037217, 79.11239583420046984 ) ) ;
#16102 = ORIENTED_EDGE ( 'NONE', *, *, #7892, .T. ) ;
#16103 = CYLINDRICAL_SURFACE ( 'NONE', #62197, 77.49899999999999523 ) ;
#16104 = FACE_OUTER_BOUND ( 'NONE', #2726, .T. ) ;
#16105 = EDGE_CURVE ( 'NONE', #44712, #50088, #41785, .T. ) ;
#16106 = CARTESIAN_POINT ( 'NONE',  ( 11.99999999999999822, -73.72996012237429397, -14.67089635893794508 ) ) ;
#16107 = CARTESIAN_POINT ( 'NONE',  ( -95.00000000000002842, 90.00000000000004263, 90.00000000000000000 ) ) ;
#16108 = VERTEX_POINT ( 'NONE', #29746 ) ;
#16109 = LINE ( 'NONE', #27375, #51309 ) ;
#16110 = CARTESIAN_POINT ( 'NONE',  ( -93.84685191531247028, -211.9973110713294489, 81.59947916753381492 ) ) ;
#16111 = CIRCLE ( 'NONE', #43709, 31.99999999999999645 ) ;
#16112 = ORIENTED_EDGE ( 'NONE', *, *, #9953, .T. ) ;
#16113 = EDGE_LOOP ( 'NONE', ( #28206, #45602, #63088, #22779 ) ) ;
#16114 = EDGE_CURVE ( 'NONE', #68978, #5092, #14310, .T. ) ;
#16115 = CARTESIAN_POINT ( 'NONE',  ( 97.64999999999999147, 90.00000000000002842, 80.15749999999999886 ) ) ;
#16116 = EDGE_CURVE ( 'NONE', #11355, #42185, #31242, .T. ) ;
#16117 = ORIENTED_EDGE ( 'NONE', *, *, #57485, .T. ) ;
#16118 = DIRECTION ( 'NONE',  ( 0.000000000000000000, -0.3090169943749548342, 0.9510565162951511997 ) ) ;
#16119 = VECTOR ( 'NONE', #54455, 1000.000000000000000 ) ;
#16120 = CARTESIAN_POINT ( 'NONE',  ( 15.00000000000000000, 20.85821328998741109, -10.92862929874522671 ) ) ;
#16121 = EDGE_LOOP ( 'NONE', ( #71449, #47461, #65630, #25143 ) ) ;
#16122 = CARTESIAN_POINT ( 'NONE',  ( -93.84685191531247028, -211.9973110713294489, 75.24947916753380639 ) ) ;
#16123 = EDGE_LOOP ( 'NONE', ( #34387, #22957, #23440, #30060, #3296, #43008, #53448, #2490, #37420, #10720, #46193, #8782, #72461, #69266, #19853, #1586, #41678, #2073, #6127, #41369, #10520, #73110, #40730, #29467, #62422, #54174, #8529, #16456, #65575, #27446, #44397, #36365, #61092, #3716, #59925, #10170, #25917, #61343, #28790, #73016, #49625, #36136, #13798, #87, #24040, #70116, #700, #26355, #3164, #56324, #18943, #64218 ) ) ;
#16124 = CIRCLE ( 'NONE', #10150, 16.00000000000000000 ) ;
#16125 = LINE ( 'NONE', #60878, #47084 ) ;
#16126 = CARTESIAN_POINT ( 'NONE',  ( 10.00000000000000000, 8.830959090342393125, 74.65491531819122883 ) ) ;
#16127 = DIRECTION ( 'NONE',  ( 0.000000000000000000, 0.000000000000000000, 1.000000000000000000 ) ) ;
#16128 = ADVANCED_FACE ( 'NONE', ( #12835 ), #35762, .T. ) ;
#16129 = CARTESIAN_POINT ( 'NONE',  ( 11.59999999999999787, 1.420590287010929336E-15, -44.99999999999998579 ) ) ;
#16130 = AXIS2_PLACEMENT_3D ( 'NONE', #63401, #13723, #71230 ) ;
#16131 = AXIS2_PLACEMENT_3D ( 'NONE', #54710, #3609, #26129 ) ;
#16132 = UNCERTAINTY_MEASURE_WITH_UNIT (LENGTH_MEASURE( 1.000000000000000082E-05 ), #58527, 'distance_accuracy_value', 'NONE');
#16133 = FACE_OUTER_BOUND ( 'NONE', #56887, .T. ) ;
#16134 = CARTESIAN_POINT ( 'NONE',  ( 94.99999999999998579, 92.66308142843932671, 88.21406250086712930 ) ) ;
#16135 = CARTESIAN_POINT ( 'NONE',  ( 5.250000000000000000, -13.95926121303099343, 0.000000000000000000 ) ) ;
#16136 = CARTESIAN_POINT ( 'NONE',  ( 0.000000000000000000, -17.80606268964563554, 33.00180498840040855 ) ) ;
#16137 = DIRECTION ( 'NONE',  ( -1.000000000000000000, 0.000000000000000000, 0.000000000000000000 ) ) ;
#16138 = CARTESIAN_POINT ( 'NONE',  ( -4.999999999999999112, 0.5616961504262225624, -0.5576671450146215570 ) ) ;
#16139 = CARTESIAN_POINT ( 'NONE',  ( 10.00000000000000000, 0.000000000000000000, 0.000000000000000000 ) ) ;
#16140 = LINE ( 'NONE', #50341, #20299 ) ;
#16141 = DIRECTION ( 'NONE',  ( -1.000000000000000000, -0.000000000000000000, 0.000000000000000000 ) ) ;
#16142 = VECTOR ( 'NONE', #65001, 1000.000000000000000 ) ;
#16143 = LINE ( 'NONE', #51094, #58411 ) ;
#16144 = EDGE_CURVE ( 'NONE', #66576, #15455, #41298, .T. ) ;
#16145 = DIRECTION ( 'NONE',  ( 0.000000000000000000, 0.000000000000000000, -1.000000000000000000 ) ) ;
#16146 = AXIS2_PLACEMENT_3D ( 'NONE', #6498, #29398, #52342 ) ;
#16147 = DIRECTION ( 'NONE',  ( 0.9781476007338069101, 2.546183866652752180E-17, 0.2079116908177528755 ) ) ;
#16148 = DIRECTION ( 'NONE',  ( -1.000000000000000000, 0.000000000000000000, 0.000000000000000000 ) ) ;
#16149 = CARTESIAN_POINT ( 'NONE',  ( 0.000000000000000000, 0.000000000000000000, 0.000000000000000000 ) ) ;
#16150 = CARTESIAN_POINT ( 'NONE',  ( -96.32499999999996021, -212.2949673200287179, 84.39083333333333314 ) ) ;
#16151 = CARTESIAN_POINT ( 'NONE',  ( 12.49999999999999645, 1.530808498934191127E-15, -54.99999999999998579 ) ) ;
#16152 = EDGE_CURVE ( 'NONE', #41791, #67978, #53077, .T. ) ;
#16153 = ADVANCED_FACE ( 'NONE', ( #13211 ), #1613, .F. ) ;
#16154 = CIRCLE ( 'NONE', #48568, 16.00000000000000000 ) ;
#16155 = EDGE_LOOP ( 'NONE', ( #22495, #39499, #39199, #4668 ) ) ;
#16156 = CARTESIAN_POINT ( 'NONE',  ( -14.25258209288423750, -138.6845900058201551, 2.500000000000000000 ) ) ;
#16157 = CARTESIAN_POINT ( 'NONE',  ( 15.00000000000000000, 23.59884966291521380, -12.14883922797262805 ) ) ;
#16158 = CARTESIAN_POINT ( 'NONE',  ( 10.00000000000000000, 41.76937507738875155, -62.50329211542393892 ) ) ;
#16159 = CARTESIAN_POINT ( 'NONE',  ( 95.00000000000000000, -207.3369185715606307, 89.64281250086715147 ) ) ;
#16160 = ORIENTED_EDGE ( 'NONE', *, *, #17455, .T. ) ;
#16161 = ORIENTED_EDGE ( 'NONE', *, *, #41198, .T. ) ;
#16162 = FACE_OUTER_BOUND ( 'NONE', #35140, .T. ) ;
#16163 = ORIENTED_EDGE ( 'NONE', *, *, #70365, .F. ) ;
#16164 = DIRECTION ( 'NONE',  ( -0.4999999999999919509, -0.8660254037844432595, 0.000000000000000000 ) ) ;
#16165 = CARTESIAN_POINT ( 'NONE',  ( 95.00000000000000000, -207.3369185715606307, 78.68906250086713783 ) ) ;
#16166 = AXIS2_PLACEMENT_3D ( 'NONE', #61906, #38972, #16406 ) ;
#16167 = ORIENTED_EDGE ( 'NONE', *, *, #55949, .T. ) ;
#16168 = CARTESIAN_POINT ( 'NONE',  ( 96.15314808468750130, -211.9973110713294489, 81.75822916753382685 ) ) ;
#16169 = VERTEX_POINT ( 'NONE', #19221 ) ;
#16170 = CARTESIAN_POINT ( 'NONE',  ( 5.000000000000002665, 3.894527615419058009, -81.90746397400384637 ) ) ;
#16171 = ORIENTED_EDGE ( 'NONE', *, *, #46524, .T. ) ;
#16172 = VECTOR ( 'NONE', #20414, 1000.000000000000000 ) ;
#16173 = CARTESIAN_POINT ( 'NONE',  ( 10.00000000000000000, -76.69515212745996280, -29.01471420065644580 ) ) ;
#16174 = EDGE_LOOP ( 'NONE', ( #35942, #39851, #66334, #23510 ) ) ;
#16175 = CARTESIAN_POINT ( 'NONE',  ( 0.000000000000000000, 68.27212725128275395, 31.46837873495001503 ) ) ;
#16176 = ORIENTED_EDGE ( 'NONE', *, *, #10612, .T. ) ;
#16177 = DIRECTION ( 'NONE',  ( -1.000000000000000000, 0.000000000000000000, 0.000000000000000000 ) ) ;
#16178 = CARTESIAN_POINT ( 'NONE',  ( 0.000000000000000000, 0.000000000000000000, 20.00000000000000000 ) ) ;
#16179 = ORIENTED_EDGE ( 'NONE', *, *, #68502, .F. ) ;
#16180 = LINE ( 'NONE', #21069, #61063 ) ;
#16181 = CIRCLE ( 'NONE', #52200, 31.99999999999999645 ) ;
#16182 = ADVANCED_FACE ( 'NONE', ( #48537 ), #71452, .T. ) ;
#16183 = ORIENTED_EDGE ( 'NONE', *, *, #41582, .F. ) ;
#16184 = CARTESIAN_POINT ( 'NONE',  ( 0.000000000000000000, 71.87247863392414615, 39.47590169984871267 ) ) ;
#16185 = ORIENTED_EDGE ( 'NONE', *, *, #25705, .F. ) ;
#16186 = AXIS2_PLACEMENT_3D ( 'NONE', #39046, #3097, #14344 ) ;
#16187 = EDGE_CURVE ( 'NONE', #66404, #26445, #65836, .T. ) ;
#16188 = VERTEX_POINT ( 'NONE', #26701 ) ;
#16189 = ORIENTED_EDGE ( 'NONE', *, *, #73983, .F. ) ;
#16190 = CARTESIAN_POINT ( 'NONE',  ( 96.15314808468748708, -208.0026889286704943, 76.09614583420047040 ) ) ;
#16191 = CARTESIAN_POINT ( 'NONE',  ( -3.000000000000000000, -13.04903810567647682, -19.60159698893442481 ) ) ;
#16193 = EDGE_CURVE ( 'NONE', #55937, #22473, #32853, .T. ) ;
#16192 = EDGE_LOOP ( 'NONE', ( #34149, #29203, #2548, #33777 ) ) ;
#16194 = VERTEX_POINT ( 'NONE', #60210 ) ;
#16195 = VERTEX_POINT ( 'NONE', #38371 ) ;
#16196 = DIRECTION ( 'NONE',  ( -0.9827303690289285187, -0.1850432970638656860, 0.000000000000000000 ) ) ;
#16197 = ADVANCED_FACE ( 'NONE', ( #60574 ), #43655, .F. ) ;
#16198 = CARTESIAN_POINT ( 'NONE',  ( 11.99999999999999822, -77.49459641780886443, 0.8261519478428549501 ) ) ;
#16199 = CARTESIAN_POINT ( 'NONE',  ( -95.00000000000002842, 92.66308142843932671, 75.03781250086714749 ) ) ;
#16200 = ORIENTED_EDGE ( 'NONE', *, *, #69412, .T. ) ;
#16201 = CARTESIAN_POINT ( 'NONE',  ( 94.99999999999998579, 87.33691857156068750, 78.37156250086714238 ) ) ;
#16202 = ORIENTED_EDGE ( 'NONE', *, *, #4115, .T. ) ;
#16203 = CYLINDRICAL_SURFACE ( 'NONE', #43175, 82.00000000000000000 ) ;
#16204 = CARTESIAN_POINT ( 'NONE',  ( -92.69370383062498320, -208.6684592857803011, 86.20322916753382003 ) ) ;
#16205 = VERTEX_POINT ( 'NONE', #61312 ) ;
#16206 = CARTESIAN_POINT ( 'NONE',  ( 1.552113441248130554, -4.877389578778822177, -0.7348938709837993244 ) ) ;
#16207 = CARTESIAN_POINT ( 'NONE',  ( 0.000000000000000000, 35.53030884539102630, -12.26510123303222599 ) ) ;
#16208 = LINE ( 'NONE', #72590, #28454 ) ;
#16209 = CARTESIAN_POINT ( 'NONE',  ( -93.84685191531248449, -208.0026889286704943, 80.54114583420046358 ) ) ;
#16210 = EDGE_CURVE ( 'NONE', #35258, #27250, #66216, .T. ) ;
#16211 = DIRECTION ( 'NONE',  ( 1.000000000000000000, 0.000000000000000000, 0.000000000000000000 ) ) ;
#16212 = CARTESIAN_POINT ( 'NONE',  ( 11.99999999999999822, -75.11764819372145041, -2.946379043147127064 ) ) ;
#16213 = ORIENTED_EDGE ( 'NONE', *, *, #25460, .F. ) ;
#16214 = CIRCLE ( 'NONE', #19801, 16.00000000000000000 ) ;
#16215 = EDGE_LOOP ( 'NONE', ( #25504, #56579, #40577, #21188 ) ) ;
#16216 = CYLINDRICAL_SURFACE ( 'NONE', #3653, 12.49999999999999645 ) ;
#16217 = CARTESIAN_POINT ( 'NONE',  ( 10.00000000000000000, 37.58145647212455032, -0.6853352020786441789 ) ) ;
#16218 = CARTESIAN_POINT ( 'NONE',  ( 10.00000000000000000, -33.71516098798684880, -74.74816331893465815 ) ) ;
#16219 = CARTESIAN_POINT ( 'NONE',  ( -93.84685191531252713, 88.00268892867056536, 83.50447916753381605 ) ) ;
#16220 = DIRECTION ( 'NONE',  ( 0.000000000000000000, 0.000000000000000000, -1.000000000000000000 ) ) ;
#16221 = DIRECTION ( 'NONE',  ( 0.000000000000000000, -0.5224985647159560154, 0.8526401643540879594 ) ) ;
#16222 = ADVANCED_FACE ( 'NONE', ( #9052 ), #31604, .F. ) ;
#16223 = AXIS2_PLACEMENT_3D ( 'NONE', #21896, #30666, #26785 ) ;
#16224 = ORIENTED_EDGE ( 'NONE', *, *, #17007, .F. ) ;
#16225 = EDGE_CURVE ( 'NONE', #31776, #45326, #29258, .T. ) ;
#16226 = AXIS2_PLACEMENT_3D ( 'NONE', #14904, #9263, #66779 ) ;
#16227 = CARTESIAN_POINT ( 'NONE',  ( -43.60332556124591008, -133.0000000000000000, -2.500000000000002220 ) ) ;
#16228 = EDGE_CURVE ( 'NONE', #4971, #49355, #5302, .T. ) ;
#16230 = DIRECTION ( 'NONE',  ( -1.000000000000000000, 0.000000000000000000, 0.000000000000000000 ) ) ;
#16229 = VECTOR ( 'NONE', #7091, 1000.000000000000000 ) ;
#16231 = CARTESIAN_POINT ( 'NONE',  ( 95.00000000000000000, -213.0599564267049857, 86.42812500173430124 ) ) ;
#16232 = FACE_OUTER_BOUND ( 'NONE', #70468, .T. ) ;
#16233 = DIRECTION ( 'NONE',  ( 1.000000000000000000, 0.000000000000000000, 0.000000000000000000 ) ) ;
#16234 = CARTESIAN_POINT ( 'NONE',  ( -96.15314808468745866, -211.9973110713294489, 77.84239583420048803 ) ) ;
#16235 = CIRCLE ( 'NONE', #35450, 31.99999999999997868 ) ;
#16236 = DIRECTION ( 'NONE',  ( 1.000000000000000000, 0.000000000000000000, 0.000000000000000000 ) ) ;
#16237 = ADVANCED_FACE ( 'NONE', ( #14689 ), #48898, .T. ) ;
#16238 = APPLICATION_CONTEXT ( 'automotive_design' ) ;
#16239 = ORIENTED_EDGE ( 'NONE', *, *, #8755, .F. ) ;
#16240 = CARTESIAN_POINT ( 'NONE',  ( 11.99999999999999822, -74.65491531819111515, -8.830959090343204920 ) ) ;
#16241 = AXIS2_PLACEMENT_3D ( 'NONE', #69018, #40069, #61896 ) ;
#16242 = FACE_OUTER_BOUND ( 'NONE', #73538, .T. ) ;
#16243 = DIRECTION ( 'NONE',  ( -1.000000000000000000, 0.000000000000000000, -0.000000000000000000 ) ) ;
#16244 = ORIENTED_EDGE ( 'NONE', *, *, #58984, .T. ) ;
#16245 = EDGE_CURVE ( 'NONE', #49792, #6124, #12457, .T. ) ;
#16246 = CARTESIAN_POINT ( 'NONE',  ( 10.00000000000000000, -33.17418723428319538, 17.67226234102814431 ) ) ;
#16247 = LINE ( 'NONE', #63884, #41401 ) ;
#16248 = CIRCLE ( 'NONE', #43849, 11.59999999999999787 ) ;
#16249 = DIRECTION ( 'NONE',  ( 0.000000000000000000, 0.000000000000000000, 1.000000000000000000 ) ) ;
#16250 = VERTEX_POINT ( 'NONE', #55657 ) ;
#16251 = DIRECTION ( 'NONE',  ( 0.000000000000000000, 0.000000000000000000, 1.000000000000000000 ) ) ;
#16252 = ORIENTED_EDGE ( 'NONE', *, *, #45421, .T. ) ;
#16253 = CARTESIAN_POINT ( 'NONE',  ( 92.69370383062501162, -209.9999999999999716, 87.10281250086714522 ) ) ;
#16254 = DIRECTION ( 'NONE',  ( -1.000000000000000000, 0.000000000000000000, -0.000000000000000000 ) ) ;
#16255 = VERTEX_POINT ( 'NONE', #25970 ) ;
#16256 = DIRECTION ( 'NONE',  ( 0.000000000000000000, -0.9723699203976740035, -0.2334453638559160216 ) ) ;
#16257 = ORIENTED_EDGE ( 'NONE', *, *, #8294, .T. ) ;
#16258 = DIRECTION ( 'NONE',  ( 3.035766082959412415E-16, 1.000000000000000000, 0.000000000000000000 ) ) ;
#16259 = ORIENTED_EDGE ( 'NONE', *, *, #49544, .T. ) ;
#16260 = AXIS2_PLACEMENT_3D ( 'NONE', #2470, #32084, #20452 ) ;
#16261 = DIRECTION ( 'NONE',  ( 0.000000000000000000, 0.000000000000000000, 1.000000000000000000 ) ) ;
#16262 = EDGE_LOOP ( 'NONE', ( #32697, #27886, #36822, #45695 ) ) ;
#16263 = VERTEX_POINT ( 'NONE', #72198 ) ;
#16264 = VERTEX_POINT ( 'NONE', #67311 ) ;
#16265 = DIRECTION ( 'NONE',  ( -1.000000000000000000, 0.000000000000000000, 0.000000000000000000 ) ) ;
#16266 = ORIENTED_EDGE ( 'NONE', *, *, #32153, .T. ) ;
#16267 = VERTEX_POINT ( 'NONE', #71823 ) ;
#16268 = CARTESIAN_POINT ( 'NONE',  ( 93.84685191531248449, 88.00268892867053694, 76.57239583420049200 ) ) ;
#16269 = LINE ( 'NONE', #73023, #47969 ) ;
#16271 = DIRECTION ( 'NONE',  ( -1.000000000000000000, -0.000000000000000000, -0.000000000000000000 ) ) ;
#16270 = AXIS2_PLACEMENT_3D ( 'NONE', #58457, #64118, #6241 ) ;
#16272 = EDGE_LOOP ( 'NONE', ( #29564, #43194, #68294, #59009 ) ) ;
#16273 = VERTEX_POINT ( 'NONE', #20332 ) ;
#16274 = EDGE_CURVE ( 'NONE', #67396, #32056, #38882, .T. ) ;
#16275 = ORIENTED_EDGE ( 'NONE', *, *, #68504, .T. ) ;
#16276 = DIRECTION ( 'NONE',  ( -0.000000000000000000, -0.000000000000000000, -1.000000000000000000 ) ) ;
#16277 = ORIENTED_EDGE ( 'NONE', *, *, #13512, .F. ) ;
#16278 = AXIS2_PLACEMENT_3D ( 'NONE', #40798, #247, #12206 ) ;
#16279 = CARTESIAN_POINT ( 'NONE',  ( 97.30629616937498838, -209.9999999999999716, 85.51531250086713953 ) ) ;
#16280 = SHAPE_DEFINITION_REPRESENTATION ( #27800, #10045 ) ;
#16281 = DIRECTION ( 'NONE',  ( 0.000000000000000000, 0.000000000000000000, 1.000000000000000000 ) ) ;
#16282 = ADVANCED_FACE ( 'NONE', ( #38744 ), #66578, .F. ) ;
#16283 = CYLINDRICAL_SURFACE ( 'NONE', #3020, 2.649999999999985700 ) ;
#16284 = FACE_OUTER_BOUND ( 'NONE', #10940, .T. ) ;
#16285 = DIRECTION ( 'NONE',  ( 0.000000000000000000, 0.000000000000000000, 1.000000000000000000 ) ) ;
#16286 = AXIS2_PLACEMENT_3D ( 'NONE', #23173, #46102, #6259 ) ;
#16287 = DIRECTION ( 'NONE',  ( 0.000000000000000000, -0.4539904997395352027, -0.8910065241883737830 ) ) ;
#16288 = EDGE_CURVE ( 'NONE', #9804, #56011, #18465, .T. ) ;
#16289 = DIRECTION ( 'NONE',  ( -1.000000000000000000, -0.000000000000000000, -0.000000000000000000 ) ) ;
#16290 = EDGE_CURVE ( 'NONE', #30983, #48336, #56858, .T. ) ;
#16291 = CARTESIAN_POINT ( 'NONE',  ( -96.15314808468745866, -211.9973110713294489, 87.84364583420047268 ) ) ;
#16292 = CARTESIAN_POINT ( 'NONE',  ( -92.69370383062502583, 91.33154071421968467, 86.99697916753382287 ) ) ;
#16293 = ORIENTED_EDGE ( 'NONE', *, *, #2511, .T. ) ;
#16294 = CIRCLE ( 'NONE', #58314, 31.99999999999998224 ) ;
#16296 = CARTESIAN_POINT ( 'NONE',  ( -97.30629616937501680, 91.33154071421968467, 85.14489583420048291 ) ) ;
#16295 = CARTESIAN_POINT ( 'NONE',  ( 93.84685191531248449, 88.00268892867053694, 88.47864583420047779 ) ) ;
#16297 = VECTOR ( 'NONE', #1651, 1000.000000000000000 ) ;
#16298 =( BOUNDED_CURVE ( )  B_SPLINE_CURVE ( 2, ( #67436, #33964, #45644, #22698, #57274, #56912, #68927 ),
 .UNSPECIFIED., .F., .F. ) 
 B_SPLINE_CURVE_WITH_KNOTS ( ( 3, 2, 2, 3 ),
 ( 0.5208333333333332593, 0.5277777777777776791, 0.5347222222222220989, 0.5416666666666665186 ),
 .UNSPECIFIED. ) 
 CURVE ( )  GEOMETRIC_REPRESENTATION_ITEM ( )  RATIONAL_B_SPLINE_CURVE ( ( 1.000000000000002220, 0.8660254037844365982, 1.000000000000000000, 0.8660254037844387076, 1.000000000000000000, 0.8660254037844408170, 0.9999999999999978906 ) ) 
 REPRESENTATION_ITEM ( '' )  );
#16299 = ORIENTED_EDGE ( 'NONE', *, *, #27899, .T. ) ;
#16300 = CARTESIAN_POINT ( 'NONE',  ( -3.000000000000000000, -1.278221433540502217, 26.51162292216071847 ) ) ;
#16301 = DIRECTION ( 'NONE',  ( -1.000000000000000000, 0.000000000000000000, -0.000000000000000000 ) ) ;
#16302 = DIRECTION ( 'NONE',  ( 1.000000000000000000, 0.000000000000000000, -0.000000000000000000 ) ) ;
#16303 = CARTESIAN_POINT ( 'NONE',  ( -119.3426274441927433, -132.5434155921188619, -5.500000000000000000 ) ) ;
#16304 = LINE ( 'NONE', #16678, #38664 ) ;
#16305 = DIRECTION ( 'NONE',  ( 0.000000000000000000, 0.8090169943749504489, -0.5877852522924689183 ) ) ;
#16306 = CARTESIAN_POINT ( 'NONE',  ( 10.00000000000000000, -6.903761155837252694, -77.19088730480530103 ) ) ;
#16307 = CYLINDRICAL_SURFACE ( 'NONE', #27058, 2.649999999999985700 ) ;
#16308 = LINE ( 'NONE', #39990, #27621 ) ;
#16309 = ORIENTED_EDGE ( 'NONE', *, *, #57724, .T. ) ;
#16310 = MECHANICAL_DESIGN_GEOMETRIC_PRESENTATION_REPRESENTATION (  '', ( #28319 ), #59517 ) ;
#16311 = EDGE_CURVE ( 'NONE', #29474, #55514, #2891, .T. ) ;
#16312 = ORIENTED_EDGE ( 'NONE', *, *, #34453, .F. ) ;
#16313 = ADVANCED_FACE ( 'NONE', ( #9797 ), #61675, .F. ) ;
#16314 = CARTESIAN_POINT ( 'NONE',  ( -93.67500000000003979, 87.70503267997129626, 81.32166666666667254 ) ) ;
#16315 = CYLINDRICAL_SURFACE ( 'NONE', #770, 16.00000000000000000 ) ;
#16316 = DIRECTION ( 'NONE',  ( 1.000000000000000000, 0.000000000000000000, 0.000000000000000000 ) ) ;
#16317 = CARTESIAN_POINT ( 'NONE',  ( 11.99999999999999822, 0.000000000000000000, 0.000000000000000000 ) ) ;
#16318 = CARTESIAN_POINT ( 'NONE',  ( 20.85212586905262100, -130.9402397935870965, -5.500000000000000000 ) ) ;
#16319 = CARTESIAN_POINT ( 'NONE',  ( 97.64999999999994884, 88.94459177146599416, 75.04099707143591047 ) ) ;
#16320 = CARTESIAN_POINT ( 'NONE',  ( -93.67499999999998295, -207.7050326799711968, 79.62833333333333030 ) ) ;
#16321 = VERTEX_POINT ( 'NONE', #11634 ) ;
#16322 = CARTESIAN_POINT ( 'NONE',  ( -93.84685191531254134, 91.99731107132950569, 83.08114583420048405 ) ) ;
#16323 = DIRECTION ( 'NONE',  ( 0.000000000000000000, -0.000000000000000000, 1.000000000000000000 ) ) ;
#16324 = ADVANCED_FACE ( 'NONE', ( #27824 ), #57896, .F. ) ;
#16325 = EDGE_CURVE ( 'NONE', #52479, #35704, #50752, .T. ) ;
#16326 = CARTESIAN_POINT ( 'NONE',  ( 11.99999999999999822, -59.75363087400113926, 56.15606465354937171 ) ) ;
#16327 = CARTESIAN_POINT ( 'NONE',  ( 10.00000000000000000, 76.66974797899852945, -11.30684508768257679 ) ) ;
#16328 = CARTESIAN_POINT ( 'NONE',  ( 95.00000000000000000, -209.9999999999999716, 90.00000000000000000 ) ) ;
#16329 = DIRECTION ( 'NONE',  ( 0.000000000000000000, 0.000000000000000000, 1.000000000000000000 ) ) ;
#16330 = CARTESIAN_POINT ( 'NONE',  ( -96.15314808468747287, -208.0026889286704943, 89.06072916753382174 ) ) ;
#16331 = FILL_AREA_STYLE ('',( #25758 ) ) ;
#16332 = AXIS2_PLACEMENT_3D ( 'NONE', #3933, #26831, #72678 ) ;
#16333 = CARTESIAN_POINT ( 'NONE',  ( 97.30629616937498838, 90.00000000000002842, 81.22906250086715829 ) ) ;
#16334 = CARTESIAN_POINT ( 'NONE',  ( -92.69370383062498320, -208.6684592857803295, 81.28197916753381946 ) ) ;
#16335 = DIRECTION ( 'NONE',  ( -0.8541291221503265474, 0.5200609990133007177, 0.000000000000000000 ) ) ;
#16336 = VERTEX_POINT ( 'NONE', #416 ) ;
#16337 = CARTESIAN_POINT ( 'NONE',  ( 97.65000000000000568, -208.4700217866474645, 80.92479166840097093 ) ) ;
#16338 = CARTESIAN_POINT ( 'NONE',  ( 10.00000000000000000, -33.17418723428294669, -17.67226234102862747 ) ) ;
#16339 = CARTESIAN_POINT ( 'NONE',  ( 10.00000000000000178, 0.000000000000000000, 12.50000000000000000 ) ) ;
#16340 = VECTOR ( 'NONE', #46715, 1000.000000000000000 ) ;
#16341 = AXIS2_PLACEMENT_3D ( 'NONE', #46675, #17361, #18459 ) ;
#16342 = VECTOR ( 'NONE', #37231, 1000.000000000000000 ) ;
#16343 = CARTESIAN_POINT ( 'NONE',  ( -95.00000000000002842, 92.66308142843932671, 79.48281250086715488 ) ) ;
#16344 = CARTESIAN_POINT ( 'NONE',  ( 96.15314808468750130, -211.9973110713294489, 79.69447916753379957 ) ) ;
#16345 = ORIENTED_EDGE ( 'NONE', *, *, #43389, .F. ) ;
#16346 = AXIS2_PLACEMENT_3D ( 'NONE', #51168, #10570, #62095 ) ;
#16347 = CARTESIAN_POINT ( 'NONE',  ( -7.499999999999968914, 79.99999999999998579, -269.9999999999999432 ) ) ;
#16348 = ORIENTED_EDGE ( 'NONE', *, *, #56947, .F. ) ;
#16349 = CIRCLE ( 'NONE', #67979, 16.00000000000000000 ) ;
#16350 = CARTESIAN_POINT ( 'NONE',  ( -23.54415474984308787, -120.4156646670583086, 5.500000000000000000 ) ) ;
#16351 = EDGE_LOOP ( 'NONE', ( #51515, #20069, #15232, #49610 ) ) ;
#16352 = CARTESIAN_POINT ( 'NONE',  ( 94.99999999999998579, 90.00000000000002842, 90.00000000000000000 ) ) ;
#16353 = AXIS2_PLACEMENT_3D ( 'NONE', #49615, #59814, #15410 ) ;
#16354 = EDGE_LOOP ( 'NONE', ( #25116, #32640, #43174, #61679 ) ) ;
#16355 = EDGE_LOOP ( 'NONE', ( #22088, #592, #74262, #11050 ) ) ;
#16356 = ORIENTED_EDGE ( 'NONE', *, *, #33885, .F. ) ;
#16357 = CARTESIAN_POINT ( 'NONE',  ( 96.66135172262728759, -211.6008015735635865, 74.79754476654878204 ) ) ;
#16358 = ORIENTED_EDGE ( 'NONE', *, *, #22748, .T. ) ;
#16359 = CARTESIAN_POINT ( 'NONE',  ( 92.35000000030105127, 90.00002455906435728, 87.53856274002153270 ) ) ;
#16360 = DIRECTION ( 'NONE',  ( 0.000000000000000000, -0.7071067811865536790, 0.7071067811865414665 ) ) ;
#16361 = CARTESIAN_POINT ( 'NONE',  ( 93.84685191531248449, 91.99731107132950569, 86.52072916753382970 ) ) ;
#16362 = CARTESIAN_POINT ( 'NONE',  ( 0.000000000000000000, -16.23288003029521320, 33.80338159004277543 ) ) ;
#16363 = CARTESIAN_POINT ( 'NONE',  ( 93.67500000000001137, -207.7050326799711968, 76.55916666666666970 ) ) ;
#16364 = ORIENTED_EDGE ( 'NONE', *, *, #17425, .F. ) ;
#16365 = ORIENTED_EDGE ( 'NONE', *, *, #64982, .F. ) ;
#16366 = EDGE_CURVE ( 'NONE', #47354, #40774, #46238, .T. ) ;
#16367 = VERTEX_POINT ( 'NONE', #69173 ) ;
#16368 = VERTEX_POINT ( 'NONE', #52238 ) ;
#16369 = CARTESIAN_POINT ( 'NONE',  ( -2.500000000000017319, -80.00000000000001421, -269.9999999999999432 ) ) ;
#16370 = AXIS2_PLACEMENT_3D ( 'NONE', #21734, #55210, #55954 ) ;
#16371 = DIRECTION ( 'NONE',  ( -1.000000000000000000, -0.000000000000000000, 0.000000000000000000 ) ) ;
#16372 = ADVANCED_FACE ( 'NONE', ( #45512 ), #19649, .T. ) ;
#16373 = DIRECTION ( 'NONE',  ( -2.628368902995175337E-16, -1.000000000000000000, 0.000000000000000000 ) ) ;
#16374 = DIRECTION ( 'NONE',  ( 0.000000000000000000, 0.9510565162951543083, -0.3090169943749448977 ) ) ;
#16375 = CARTESIAN_POINT ( 'NONE',  ( -97.64999247309853558, -211.5299825590109890, 88.22729196900363036 ) ) ;
#16376 = CARTESIAN_POINT ( 'NONE',  ( 96.32499999999998863, 87.70503267997126784, 83.94104166840097037 ) ) ;
#16378 = ORIENTED_EDGE ( 'NONE', *, *, #49468, .F. ) ;
#16377 = ADVANCED_FACE ( 'NONE', ( #46604 ), #37704, .F. ) ;
#16379 = CARTESIAN_POINT ( 'NONE',  ( -94.99999999999997158, -206.9400435732949575, 82.30062500173428930 ) ) ;
#16380 = VERTEX_POINT ( 'NONE', #62051 ) ;
#16381 = DIRECTION ( 'NONE',  ( 0.000000000000000000, -0.5224985647159380298, -0.8526401643540988395 ) ) ;
#16382 = EDGE_LOOP ( 'NONE', ( #23393, #5954, #51252, #48165 ) ) ;
#16384 = CARTESIAN_POINT ( 'NONE',  ( -96.32500000000001705, 87.70503267997129626, 78.12020833506763040 ) ) ;
#16383 = CARTESIAN_POINT ( 'NONE',  ( 97.64999999999997726, 88.47002178664753558, 83.99395833506763154 ) ) ;
#16385 = EDGE_CURVE ( 'NONE', #32140, #58910, #52074, .T. ) ;
#16386 = VERTEX_POINT ( 'NONE', #40598 ) ;
#16387 = CARTESIAN_POINT ( 'NONE',  ( 97.30629616937498838, 90.00000000000002842, 84.40406250086715545 ) ) ;
#16388 = CIRCLE ( 'NONE', #59638, 31.99999999999999289 ) ;
#16389 = CARTESIAN_POINT ( 'NONE',  ( -92.35000000000005116, -208.4700217866473793, 86.56041666666668277 ) ) ;
#16390 = CARTESIAN_POINT ( 'NONE',  ( -96.32499999999996021, -212.2949673200287179, 82.56520833506762358 ) ) ;
#16391 = CARTESIAN_POINT ( 'NONE',  ( -62.50000000000000000, 7.654042494670957804E-15, -275.0000000000000000 ) ) ;
#16392 = CARTESIAN_POINT ( 'NONE',  ( 10.00000000000000000, 0.000000000000000000, 0.000000000000000000 ) ) ;
#16393 = CARTESIAN_POINT ( 'NONE',  ( 0.000000000000000000, -120.0000000000000000, 125.0000000000000000 ) ) ;
#16394 = ORIENTED_EDGE ( 'NONE', *, *, #72729, .F. ) ;
#16395 = CARTESIAN_POINT ( 'NONE',  ( 10.00000000000000000, 37.58145647212453611, 0.6853352020791767529 ) ) ;
#16396 = CARTESIAN_POINT ( 'NONE',  ( -1.355716935723729089, -119.3581031311870362, 2.500000000000000000 ) ) ;
#16397 = LINE ( 'NONE', #10384, #8411 ) ;
#16398 = ORIENTED_EDGE ( 'NONE', *, *, #6972, .F. ) ;
#16399 = VECTOR ( 'NONE', #40331, 999.9999999999998863 ) ;
#16400 = ORIENTED_EDGE ( 'NONE', *, *, #4442, .F. ) ;
#16401 = AXIS2_PLACEMENT_3D ( 'NONE', #39830, #22159, #44347 ) ;
#16402 = EDGE_CURVE ( 'NONE', #73223, #60373, #4923, .T. ) ;
#16403 = EDGE_CURVE ( 'NONE', #45162, #65655, #71260, .T. ) ;
#16404 = DIRECTION ( 'NONE',  ( 0.000000000000000000, 0.000000000000000000, 1.000000000000000000 ) ) ;
#16405 = VECTOR ( 'NONE', #59786, 1000.000000000000000 ) ;
#16406 = DIRECTION ( 'NONE',  ( 0.000000000000000000, 0.000000000000000000, 1.000000000000000000 ) ) ;
#16407 = DIRECTION ( 'NONE',  ( -0.000000000000000000, -0.000000000000000000, -1.000000000000000000 ) ) ;
#16408 = CARTESIAN_POINT ( 'NONE',  ( -92.69370383062498320, -208.6684592857803011, 81.28197916753381946 ) ) ;
#16409 = ORIENTED_EDGE ( 'NONE', *, *, #34453, .T. ) ;
#16410 = CARTESIAN_POINT ( 'NONE',  ( -97.30629616937501680, 88.66845928578038638, 87.79072916753381151 ) ) ;
#16411 = ORIENTED_EDGE ( 'NONE', *, *, #60623, .T. ) ;
#16412 = CARTESIAN_POINT ( 'NONE',  ( -94.99999999999997158, -213.0599564267049857, 77.53812500173428646 ) ) ;
#16413 = EDGE_CURVE ( 'NONE', #71089, #53435, #6467, .T. ) ;
#16414 = ADVANCED_FACE ( 'NONE', ( #39115 ), #10915, .T. ) ;
#16415 = DIRECTION ( 'NONE',  ( -1.000000000000000000, 0.000000000000000000, 0.000000000000000000 ) ) ;
#16416 = CIRCLE ( 'NONE', #27175, 37.49900000000000233 ) ;
#16417 = DIRECTION ( 'NONE',  ( -1.000000000000000000, -0.000000000000000000, -0.000000000000000000 ) ) ;
#16418 = DIRECTION ( 'NONE',  ( -1.000000000000000000, -0.000000000000000000, -0.000000000000000000 ) ) ;
#16419 = LINE ( 'NONE', #22433, #55672 ) ;
#16420 = DIRECTION ( 'NONE',  ( -0.000000000000000000, -0.000000000000000000, 1.000000000000000000 ) ) ;
#16421 = CARTESIAN_POINT ( 'NONE',  ( -94.99999999999997158, -206.9400435732949575, 79.04624999999997215 ) ) ;
#16422 = FACE_OUTER_BOUND ( 'NONE', #7666, .T. ) ;
#16423 = DIRECTION ( 'NONE',  ( 0.08130631524010120681, -0.9966891607226784355, 0.000000000000000000 ) ) ;
#16424 = CYLINDRICAL_SURFACE ( 'NONE', #44355, 31.99999999999998579 ) ;
#16425 = CARTESIAN_POINT ( 'NONE',  ( 97.64996928176857693, -208.4700040514683224, 79.01979289519827887 ) ) ;
#16426 = DIRECTION ( 'NONE',  ( 0.3311129884571281101, 0.9435911131814402886, 0.000000000000000000 ) ) ;
#16427 = CARTESIAN_POINT ( 'NONE',  ( -93.84685191531247028, -211.9973110713294489, 89.37822916753381719 ) ) ;
#16428 = CARTESIAN_POINT ( 'NONE',  ( 10.00000000000000000, 32.34446384430010113, -26.79245525562679831 ) ) ;
#16429 = VERTEX_POINT ( 'NONE', #33453 ) ;
#16430 = DIRECTION ( 'NONE',  ( -1.000000000000000000, 0.000000000000000000, -0.000000000000000000 ) ) ;
#16431 = CARTESIAN_POINT ( 'NONE',  ( -92.69370383062505425, 91.33154071421968467, 78.58322916753381548 ) ) ;
#16432 = FACE_OUTER_BOUND ( 'NONE', #64938, .T. ) ;
#16433 = ORIENTED_EDGE ( 'NONE', *, *, #2607, .F. ) ;
#16434 = DIRECTION ( 'NONE',  ( 0.000000000000000000, 0.000000000000000000, -1.000000000000000000 ) ) ;
#16435 = CARTESIAN_POINT ( 'NONE',  ( 0.000000000000000000, -46.11716303203234446, 67.80270845531873647 ) ) ;
#16436 = AXIS2_PLACEMENT_3D ( 'NONE', #7528, #1926, #42484 ) ;
#16437 = DIRECTION ( 'NONE',  ( 1.000000000000000000, 0.000000000000000000, -0.000000000000000000 ) ) ;
#16438 = CARTESIAN_POINT ( 'NONE',  ( 0.000000000000000000, 0.000000000000000000, 53.20000000000001705 ) ) ;
#16439 = CARTESIAN_POINT ( 'NONE',  ( 92.69370383062501162, -209.9999999999999716, 75.19656250086714522 ) ) ;
#16440 = VECTOR ( 'NONE', #40574, 1000.000000000000000 ) ;
#16441 = ORIENTED_EDGE ( 'NONE', *, *, #61084, .T. ) ;
#16442 = EDGE_CURVE ( 'NONE', #11963, #8256, #29295, .T. ) ;
#16443 = VECTOR ( 'NONE', #40842, 1000.000000000000000 ) ;
#16444 = VERTEX_POINT ( 'NONE', #68053 ) ;
#16445 = EDGE_CURVE ( 'NONE', #15716, #61582, #16546, .T. ) ;
#16446 = CYLINDRICAL_SURFACE ( 'NONE', #52464, 77.49899999999999523 ) ;
#16447 = AXIS2_PLACEMENT_3D ( 'NONE', #19179, #43250, #7537 ) ;
#16448 = VECTOR ( 'NONE', #46664, 1000.000000000000000 ) ;
#16449 = CARTESIAN_POINT ( 'NONE',  ( 11.99999999999999822, 18.89407956138257205, 75.16055320797038064 ) ) ;
#16450 = EDGE_CURVE ( 'NONE', #57513, #58250, #62437, .T. ) ;
#16451 = DIRECTION ( 'NONE',  ( -1.000000000000000000, 0.000000000000000000, -0.000000000000000000 ) ) ;
#16452 = DIRECTION ( 'NONE',  ( 0.000000000000000000, 0.07845909572784530439, -0.9969173337331279638 ) ) ;
#16453 = CARTESIAN_POINT ( 'NONE',  ( 92.35000000006145626, -209.9999881787626919, 81.82400613091914465 ) ) ;
#16454 = CARTESIAN_POINT ( 'NONE',  ( 93.67500000000001137, -212.2949673200287179, 88.83583333333334053 ) ) ;
#16455 = EDGE_CURVE ( 'NONE', #69721, #31367, #49637, .T. ) ;
#16456 = ORIENTED_EDGE ( 'NONE', *, *, #19113, .F. ) ;
#16457 = PLANE ( 'NONE',  #63604 ) ;
#16458 = VERTEX_POINT ( 'NONE', #22566 ) ;
#16459 = ORIENTED_EDGE ( 'NONE', *, *, #55233, .F. ) ;
#16460 = DIRECTION ( 'NONE',  ( 0.000000000000000000, 0.000000000000000000, 1.000000000000000000 ) ) ;
#16461 = VECTOR ( 'NONE', #71634, 1000.000000000000000 ) ;
#16462 = EDGE_CURVE ( 'NONE', #70940, #41508, #28556, .T. ) ;
#16463 = DIRECTION ( 'NONE',  ( -0.000000000000000000, -0.000000000000000000, 1.000000000000000000 ) ) ;
#16464 = ORIENTED_EDGE ( 'NONE', *, *, #53786, .T. ) ;
#16465 = DIRECTION ( 'NONE',  ( 8.090853898039833646E-17, -9.269810975720164453E-17, 1.000000000000000000 ) ) ;
#16466 = CARTESIAN_POINT ( 'NONE',  ( 97.64999999999997726, -208.4700217866474645, 75.20979166840096752 ) ) ;
#16467 = CARTESIAN_POINT ( 'NONE',  ( 92.34999999999999432, 91.52997821335252127, 81.05708333333333826 ) ) ;
#16468 = CIRCLE ( 'NONE', #11618, 16.00000000000000000 ) ;
#16469 = ORIENTED_EDGE ( 'NONE', *, *, #17080, .T. ) ;
#16470 = DIRECTION ( 'NONE',  ( -1.000000000000000000, 0.000000000000000000, 0.000000000000000000 ) ) ;
#16471 = VERTEX_POINT ( 'NONE', #22949 ) ;
#16472 = CARTESIAN_POINT ( 'NONE',  ( -96.32499999999996021, -207.7050326799711968, 82.98854166840096980 ) ) ;
#16473 = ORIENTED_EDGE ( 'NONE', *, *, #44973, .T. ) ;
#16474 = DIRECTION ( 'NONE',  ( 0.000000000000000000, 0.5877852522924744694, -0.8090169943749465631 ) ) ;
#16475 = CARTESIAN_POINT ( 'NONE',  ( -96.15314808468752972, 91.99731107132950569, 84.61572916753381435 ) ) ;
#16476 = EDGE_CURVE ( 'NONE', #6402, #47170, #45078, .T. ) ;
#16477 = CARTESIAN_POINT ( 'NONE',  ( 96.15314808468748708, 88.00268892867053694, 79.05947916753380866 ) ) ;
#16478 = ORIENTED_EDGE ( 'NONE', *, *, #53163, .F. ) ;
#16479 = DIRECTION ( 'NONE',  ( -1.000000000000000000, 0.000000000000000000, -0.000000000000000000 ) ) ;
#16480 = DIRECTION ( 'NONE',  ( 0.000000000000000000, 0.000000000000000000, 1.000000000000000000 ) ) ;
#16481 = CARTESIAN_POINT ( 'NONE',  ( 0.000000000000000000, -17.67226234102801286, -33.17418723428327354 ) ) ;
#16482 = CARTESIAN_POINT ( 'NONE',  ( 11.99999999999999822, -75.16055320797016748, -18.89407956138335365 ) ) ;
#16483 = ORIENTED_EDGE ( 'NONE', *, *, #53404, .T. ) ;
#16484 = DIRECTION ( 'NONE',  ( -1.000000000000000000, 0.000000000000000000, -0.000000000000000000 ) ) ;
#16485 = CARTESIAN_POINT ( 'NONE',  ( -96.15314808468745866, -211.9973110713294489, 76.41364583420048007 ) ) ;
#16486 = ORIENTED_EDGE ( 'NONE', *, *, #59697, .T. ) ;
#16487 = VERTEX_POINT ( 'NONE', #35674 ) ;
#16488 = LINE ( 'NONE', #55967, #6118 ) ;
#16489 = ADVANCED_FACE ( 'NONE', ( #48082 ), #13849, .T. ) ;
#16490 = ORIENTED_EDGE ( 'NONE', *, *, #29547, .F. ) ;
#16491 = ADVANCED_FACE ( 'NONE', ( #25513 ), #40974, .T. ) ;
#16492 = CARTESIAN_POINT ( 'NONE',  ( 10.00000000000000000, 73.95703589263975175, 23.16143007188454206 ) ) ;
#16493 = CARTESIAN_POINT ( 'NONE',  ( 0.000000000000000000, -46.54456581323762521, -59.03342792756313884 ) ) ;
#16494 = ORIENTED_EDGE ( 'NONE', *, *, #19258, .T. ) ;
#16495 = CARTESIAN_POINT ( 'NONE',  ( -92.69370383062498320, -208.6684592857803011, 76.67822916753378593 ) ) ;
#16496 = ORIENTED_EDGE ( 'NONE', *, *, #45452, .T. ) ;
#16497 = CARTESIAN_POINT ( 'NONE',  ( -93.67500000000003979, 87.70503267997129626, 76.87666666666666515 ) ) ;
#16498 = FACE_OUTER_BOUND ( 'NONE', #66733, .T. ) ;
#16499 = DIRECTION ( 'NONE',  ( 1.000000000000000000, -7.571541139944063212E-15, -2.603472992745718826E-14 ) ) ;
#16500 = DIRECTION ( 'NONE',  ( 0.000000000000000000, -0.2079116908177532086, -0.9781476007338069101 ) ) ;
#16501 = CARTESIAN_POINT ( 'NONE',  ( 0.000000000000000000, 16.23288003029543347, -33.80338159004267595 ) ) ;
#16502 = CARTESIAN_POINT ( 'NONE',  ( 94.99999999999998579, 92.66308142843932671, 83.76906250086715033 ) ) ;
#16503 = VECTOR ( 'NONE', #29078, 1000.000000000000000 ) ;
#16504 = CARTESIAN_POINT ( 'NONE',  ( 10.00000000000000000, 12.42422080174688404, -35.38097989696498047 ) ) ;
#16505 = DIRECTION ( 'NONE',  ( -1.000000000000000000, 0.000000000000000000, 0.000000000000000000 ) ) ;
#16506 = CARTESIAN_POINT ( 'NONE',  ( 11.99999999999999822, -30.41916302227164337, 71.27951684758015460 ) ) ;
#16507 = CARTESIAN_POINT ( 'NONE',  ( 1.355716935723751293, -120.6418968688129496, 2.500000000000000000 ) ) ;
#16508 = CARTESIAN_POINT ( 'NONE',  ( 0.000000000000000000, 14.60985201121704513, 18.46759930825707841 ) ) ;
#16509 = CYLINDRICAL_SURFACE ( 'NONE', #62344, 26.50000000000552092 ) ;
#16510 = DIRECTION ( 'NONE',  ( -0.000000000000000000, -0.000000000000000000, -1.000000000000000000 ) ) ;
#16511 =( BOUNDED_SURFACE ( )  B_SPLINE_SURFACE ( 1, 2, ( 
 ( #3909, #4279, #55391, #14794, #50856, #66318, #26810, #60673, #73781, #39221, #38843, #50100, #61783, #43758, #27170, #37741, #44111, #43398, #5023, #27927, #49734, #9894, #10638, #33560, #56519, #32077, #55015, #4652, #10266, #72659, #73030, #67411, #44497, #67787, #50489, #61413, #27554, #21164, #67035, #15538, #32812, #3545, #33188, #56134, #32450, #21919, #61032, #49375, #55764, #72306, #20805, #44865, #38475, #66676, #39591, #23047, #28661, #51601, #30415, #23408, #63642, #39961, #53361, #34305, #12114, #68157, #17391, #69268, #45976, #57252, #7865, #5758, #47717, #35055, #16653, #30781, #45236, #156, #62537, #53728, #70631, #17754, #29035, #40701, #22672, #57627, #11014, #68903, #22293, #59378, #33941, #40322, #63270, #42091, #13506, #19146, #56888, #5394, #59012, #7505, #11732, #51967, #46337, #515, #65030, #1901, #34677, #24787, #6132, #36432, #28289, #51228, #74157, #45617, #68542, #62918, #17026, #11374, #20993, #14615, #61239, #72492, #3731, #31528, #37928, #19510, #3002, #8617, #54467, #9339, #3366, #43586, #19877, #32264, #14238, #66503, #48093, #71742, #49195, #25895, #37193, #9720, #60135, #26633, #14985, #60859, #32639, #48824, #20244, #8977, #72122, #55212, #25167, #43946, #66862, #2271, #31163, #43215, #54840, #42825, #15349, #36801, #25524, #49564, #38292, #71007, #20633, #42457, #66138, #54113, #71371, #65397, #37564, #60497, #13862, #59749, #8232, #2645, #31903, #26257, #48458, #65754, #26999, #56335, #4853, #67982, #11564, #55584, #38671, #45810, #4104, #67608, #44307, #61601, #50301, #22494, #45056, #21736, #73236, #16101, #16477, #39040, #10087, #68735, #49933, #61979, #67239, #33010, #44693, #45436, #39413, #10459, #33375, #27754, #62358, #50679, #72849, #63106, #21349, #73606, #15735, #55956, #28483, #28119, #10841, #51054, #4472, #33762, #27367, #22116, #56719, #17218, #40153, #5218, #73979, #41286, #68363, #51419, #16858, #39788, #62739, #11207, #34134, #57081, #5588, #22875, #58929, #41622, #52526, #18680, #69455, #35246, #17954, #23974, #57443, #41262, #58540, #705, #7036, #6322, #53278, #46908, #19054, #30336, #35977, #63834, #70178, #51798, #58177, #40899, #12309, #64560, #35607, #1452, #52161, #13039, #46528, #24339, #5959, #29581, #29962, #6675, #1080, #42005, #69817 ),
 ( #28868, #7421, #1815, #347, #24702, #18319, #52913, #64201, #47635, #63462, #46166, #23238, #12673, #70542, #29222, #69099, #17585, #47274, #23599, #64942, #34499, #40517, #11936, #34883, #57817, #54755, #59664, #66055, #42738, #32180, #3285, #49110, #55122, #3648, #8148, #31810, #26174, #36349, #8893, #72036, #25444, #42373, #31071, #26549, #65674, #37102, #49482, #20549, #43503, #66422, #54388, #14529, #14902, #14152, #59290, #60051, #8534, #25810, #43861, #13417, #70923, #72406, #7783, #48373, #2186, #19423, #54026, #37845, #2919, #2564, #71286, #19793, #48741, #31446, #30699, #20911, #53647, #71664, #25072, #48010, #60776, #60413, #20163, #9259, #13780, #43124, #65312, #37481, #36717, #28396, #51332, #27280, #33291, #11120, #56996, #39705, #55500, #4017, #28030, #10749, #4382, #73519, #16387, #44970, #16768, #73891, #10372, #50970, #50211, #67521, #73145, #56246, #15271, #22026, #39328, #32919, #62265, #38584, #34045, #4761, #74270, #62647, #68272, #21650, #22400, #9635, #16010, #44606, #38955, #45348, #67897, #33673, #9999, #5500, #61892, #56629, #38203, #27666, #5128, #50592, #22786, #66776, #61148, #32554, #26916, #49846, #72762, #21263, #44224, #67147, #15652, #61515, #55870, #12951, #64476, #45727, #263, #6239, #23888, #11842, #58837, #5867, #69013, #12595, #35526, #17131, #40812, #18237, #46442, #29139, #30252, #57734, #70097, #58454, #6951, #53192, #69371, #17867, #52438, #41179, #1369, #68649, #35889, #7337, #40064, #23154, #52077, #46824, #34793, #1728, #28777, #17498, #29876, #52829, #63024, #64115, #24260, #620, #46078, #40428, #11484, #23511, #63748, #34411, #47184, #18599, #41540, #12224, #69737, #57355, #35160, #51715, #58097, #6598, #29502, #63375, #992, #7694, #14812, #55035, #36631, #13331, #30611, #19338, #65971, #14058, #65224, #42294, #59576, #59962, #8062, #70456, #32096, #47552, #30984, #41913, #24616, #71949, #71577, #31357, #20074, #24983, #8446, #18963, #25364, #64852, #60693, #9172, #53940, #65591, #43417, #37759, #20463, #36267, #59203, #60330, #43029, #2478, #54309, #48662, #2834, #49018, #31726, #42654, #8808, #48291, #71199, #19706, #37008, #53559, #25724, #14442, #13695, #37397, #70838, #66339, #54670, #2096, #47920, #26088, #3199, #39238, #20823, #4300, #9911 ) ),
 .UNSPECIFIED., .F., .F., .F. ) 
 B_SPLINE_SURFACE_WITH_KNOTS ( ( 2, 2 ),
 ( 3, 2, 2, 2, 2, 2, 2, 2, 2, 2, 2, 2, 2, 2, 2, 2, 2, 2, 2, 2, 2, 2, 2, 2, 2, 2, 2, 2, 2, 2, 2, 2, 2, 2, 2, 2, 2, 2, 2, 2, 2, 2, 2, 2, 2, 2, 2, 2, 2, 2, 2, 2, 2, 2, 2, 2, 2, 2, 2, 2, 2, 2, 2, 2, 2, 2, 2, 2, 2, 2, 2, 2, 2, 2, 2, 2, 2, 2, 2, 2, 2, 2, 2, 2, 2, 2, 2, 2, 2, 2, 2, 2, 2, 2, 2, 2, 2, 2, 2, 2, 2, 2, 2, 2, 2, 2, 2, 2, 2, 2, 2, 2, 2, 2, 2, 2, 2, 2, 2, 2, 2, 2, 2, 2, 2, 2, 2, 2, 2, 2, 2, 2, 2, 2, 2, 2, 2, 2, 2, 2, 2, 2, 3 ),
 ( 0.000000000000000000, 1.000000000000000000 ),
 ( 0.000000000000000000, 0.006944444444444444059, 0.01388888888888888812, 0.02083333333333333218, 0.02777777777777777624, 0.03472222222222222376, 0.04166666666666666435, 0.04861111111111111188, 0.05555555555555555247, 0.06250000000000000000, 0.06944444444444444753, 0.07638888888888889506, 0.08333333333333332871, 0.09027777777777777624, 0.09722222222222222376, 0.1041666666666666713, 0.1111111111111111049, 0.1180555555555555525, 0.1250000000000000000, 0.1319444444444444475, 0.1388888888888888951, 0.1458333333333333426, 0.1527777777777777901, 0.1597222222222222099, 0.1666666666666666574, 0.1736111111111111049, 0.1805555555555555525, 0.1875000000000000000, 0.1944444444444444475, 0.2013888888888888951, 0.2083333333333333426, 0.2152777777777777901, 0.2222222222222222099, 0.2291666666666666574, 0.2361111111111111049, 0.2430555555555555525, 0.2500000000000000000, 0.2569444444444444198, 0.2638888888888888951, 0.2708333333333333148, 0.2777777777777777901, 0.2847222222222222099, 0.2916666666666666852, 0.2986111111111111049, 0.3055555555555555802, 0.3125000000000000000, 0.3194444444444444198, 0.3263888888888888951, 0.3333333333333333148, 0.3402777777777777901, 0.3472222222222222099, 0.3541666666666666852, 0.3611111111111111049, 0.3680555555555555802, 0.3750000000000000000, 0.3819444444444444198, 0.3888888888888888951, 0.3958333333333333148, 0.4027777777777777901, 0.4097222222222222099, 0.4166666666666666852, 0.4236111111111111049, 0.4305555555555555802, 0.4375000000000000000, 0.4444444444444444198, 0.4513888888888888951, 0.4583333333333333148, 0.4652777777777777901, 0.4722222222222222099, 0.4791666666666666852, 0.4861111111111111049, 0.4930555555555555802, 0.5000000000000000000, 0.5069444444444444198, 0.5138888888888888395, 0.5208333333333333703, 0.5277777777777777901, 0.5347222222222222099, 0.5416666666666666297, 0.5486111111111111605, 0.5555555555555555802, 0.5625000000000000000, 0.5694444444444444198, 0.5763888888888888395, 0.5833333333333333703, 0.5902777777777777901, 0.5972222222222222099, 0.6041666666666666297, 0.6111111111111111605, 0.6180555555555555802, 0.6250000000000000000, 0.6319444444444444198, 0.6388888888888888395, 0.6458333333333333703, 0.6527777777777777901, 0.6597222222222222099, 0.6666666666666666297, 0.6736111111111111605, 0.6805555555555555802, 0.6875000000000000000, 0.6944444444444444198, 0.7013888888888888395, 0.7083333333333333703, 0.7152777777777777901, 0.7222222222222222099, 0.7291666666666666297, 0.7361111111111111605, 0.7430555555555555802, 0.7500000000000000000, 0.7569444444444444198, 0.7638888888888888395, 0.7708333333333333703, 0.7777777777777777901, 0.7847222222222222099, 0.7916666666666666297, 0.7986111111111111605, 0.8055555555555555802, 0.8125000000000000000, 0.8194444444444444198, 0.8263888888888888395, 0.8333333333333333703, 0.8402777777777777901, 0.8472222222222222099, 0.8541666666666666297, 0.8611111111111111605, 0.8680555555555555802, 0.8750000000000000000, 0.8819444444444444198, 0.8888888888888888395, 0.8958333333333333703, 0.9027777777777777901, 0.9097222222222222099, 0.9166666666666666297, 0.9236111111111111605, 0.9305555555555555802, 0.9375000000000000000, 0.9444444444444444198, 0.9513888888888888395, 0.9583333333333333703, 0.9652777777777777901, 0.9722222222222222099, 0.9791666666666666297, 0.9842227634901433708 ),
 .UNSPECIFIED. ) 
 GEOMETRIC_REPRESENTATION_ITEM ( )  RATIONAL_B_SPLINE_SURFACE ( (
 ( 1.000000000000000000, 0.8660254037844387076, 1.000000000000000000, 0.8660254037844387076, 1.000000000000000000, 0.8660254037844387076, 1.000000000000000000, 0.8660254037844387076, 1.000000000000000000, 0.8660254037844387076, 1.000000000000000000, 0.8660254037844387076, 1.000000000000000000, 0.8660254037844387076, 1.000000000000000000, 0.8660254037844387076, 1.000000000000000000, 0.8660254037844387076, 1.000000000000000000, 0.8660254037844387076, 1.000000000000000000, 0.8660254037844387076, 1.000000000000000000, 0.8660254037844387076, 1.000000000000000000, 0.8660254037844387076, 1.000000000000000000, 0.8660254037844387076, 1.000000000000000000, 0.8660254037844387076, 1.000000000000000000, 0.8660254037844387076, 1.000000000000000000, 0.8660254037844387076, 1.000000000000000000, 0.8660254037844387076, 1.000000000000000000, 0.8660254037844387076, 1.000000000000000000, 0.8660254037844387076, 1.000000000000000000, 0.8660254037844387076, 1.000000000000000000, 0.8660254037844387076, 1.000000000000000000, 0.8660254037844387076, 1.000000000000000000, 0.8660254037844387076, 1.000000000000000000, 0.8660254037844387076, 1.000000000000000000, 0.8660254037844387076, 1.000000000000000000, 0.8660254037844387076, 1.000000000000000000, 0.8660254037844387076, 1.000000000000000000, 0.8660254037844387076, 1.000000000000000000, 0.8660254037844387076, 1.000000000000000000, 0.8660254037844387076, 1.000000000000000000, 0.8660254037844387076, 1.000000000000000000, 0.8660254037844387076, 1.000000000000000000, 0.8660254037844387076, 1.000000000000000000, 0.8660254037844387076, 1.000000000000000000, 0.8660254037844387076, 1.000000000000000000, 0.8660254037844387076, 1.000000000000000000, 0.8660254037844387076, 1.000000000000000000, 0.8660254037844387076, 1.000000000000000000, 0.8660254037844387076, 1.000000000000000000, 0.8660254037844387076, 1.000000000000000000, 0.8660254037844387076, 1.000000000000000000, 0.8660254037844387076, 1.000000000000000000, 0.8660254037844387076, 1.000000000000000000, 0.8660254037844387076, 1.000000000000000000, 0.8660254037844387076, 1.000000000000000000, 0.8660254037844387076, 1.000000000000000000, 0.8660254037844387076, 1.000000000000000000, 0.8660254037844387076, 1.000000000000000000, 0.8660254037844387076, 1.000000000000000000, 0.8660254037844387076, 1.000000000000000000, 0.8660254037844387076, 1.000000000000000000, 0.8660254037844387076, 1.000000000000000000, 0.8660254037844387076, 1.000000000000000000, 0.8660254037844387076, 1.000000000000000000, 0.8660254037844387076, 1.000000000000000000, 0.8660254037844387076, 1.000000000000000000, 0.8660254037844387076, 1.000000000000000000, 0.8660254037844387076, 1.000000000000000000, 0.8660254037844387076, 1.000000000000000000, 0.8660254037844387076, 1.000000000000000000, 0.8660254037844387076, 1.000000000000000000, 0.8660254037844387076, 1.000000000000000000, 0.8660254037844387076, 1.000000000000000000, 0.8660254037844387076, 1.000000000000000000, 0.8660254037844387076, 1.000000000000000000, 0.8660254037844387076, 1.000000000000000000, 0.8660254037844387076, 1.000000000000000000, 0.8660254037844387076, 1.000000000000000000, 0.8660254037844387076, 1.000000000000000000, 0.8660254037844387076, 1.000000000000000000, 0.8660254037844387076, 1.000000000000000000, 0.8660254037844387076, 1.000000000000000000, 0.8660254037844387076, 1.000000000000000000, 0.8660254037844387076, 1.000000000000000000, 0.8660254037844387076, 1.000000000000000000, 0.8660254037844387076, 1.000000000000000000, 0.8660254037844387076, 1.000000000000000000, 0.8660254037844387076, 1.000000000000000000, 0.8660254037844387076, 1.000000000000000000, 0.8660254037844387076, 1.000000000000000000, 0.8660254037844387076, 1.000000000000000000, 0.8660254037844387076, 1.000000000000000000, 0.8660254037844387076, 1.000000000000000000, 0.8660254037844387076, 1.000000000000000000, 0.8660254037844387076, 1.000000000000000000, 0.8660254037844387076, 1.000000000000000000, 0.8660254037844387076, 1.000000000000000000, 0.8660254037844387076, 1.000000000000000000, 0.8660254037844387076, 1.000000000000000000, 0.8660254037844387076, 1.000000000000000000, 0.8660254037844387076, 1.000000000000000000, 0.8660254037844387076, 1.000000000000000000, 0.8660254037844387076, 1.000000000000000000, 0.8660254037844387076, 1.000000000000000000, 0.8660254037844387076, 1.000000000000000000, 0.8660254037844387076, 1.000000000000000000, 0.8660254037844387076, 1.000000000000000000, 0.8660254037844387076, 1.000000000000000000, 0.8660254037844387076, 1.000000000000000000, 0.8660254037844387076, 1.000000000000000000, 0.8660254037844387076, 1.000000000000000000, 0.8660254037844387076, 1.000000000000000000, 0.8660254037844387076, 1.000000000000000000, 0.8660254037844387076, 1.000000000000000000, 0.8660254037844387076, 1.000000000000000000, 0.8660254037844387076, 1.000000000000000000, 0.8660254037844387076, 1.000000000000000000, 0.8660254037844387076, 1.000000000000000000, 0.8660254037844387076, 1.000000000000000000, 0.8660254037844387076, 1.000000000000000000, 0.8660254037844387076, 1.000000000000000000, 0.8660254037844387076, 1.000000000000000000, 0.8660254037844387076, 1.000000000000000000, 0.8660254037844387076, 1.000000000000000000, 0.8660254037844387076, 1.000000000000000000, 0.8660254037844387076, 1.000000000000000000, 0.8660254037844387076, 1.000000000000000000, 0.8660254037844387076, 1.000000000000000000, 0.8660254037844387076, 1.000000000000000000, 0.8660254037844387076, 1.000000000000000000, 0.8660254037844387076, 1.000000000000000000, 0.8660254037844387076, 1.000000000000000000, 0.8660254037844387076, 1.000000000000000000, 0.8660254037844387076, 1.000000000000000000, 0.8660254037844387076, 1.000000000000000000, 0.8660254037844387076, 1.000000000000000000, 0.8660254037844387076, 1.000000000000000000, 0.8660254037844387076, 1.000000000000000000, 0.8660254037844387076, 1.000000000000000000, 0.8660254037844387076, 1.000000000000000000, 0.8660254037844387076, 1.000000000000000000, 0.8660254037844387076, 1.000000000000000000, 0.8660254037844387076, 1.000000000000000000, 0.8660254037844387076, 1.000000000000000000, 0.8660254037844387076, 1.000000000000000000, 0.8660254037844387076, 1.000000000000000000, 0.8660254037844387076, 1.000000000000000000, 0.8660254037844387076, 1.000000000000000000, 0.8660254037844387076, 1.000000000000000000, 0.8660254037844387076, 1.000000000000000000, 0.9024560516293018697, 0.9469512977404641596),
 ( 1.000000000000000000, 0.8660254037844387076, 1.000000000000000000, 0.8660254037844387076, 1.000000000000000000, 0.8660254037844387076, 1.000000000000000000, 0.8660254037844387076, 1.000000000000000000, 0.8660254037844387076, 1.000000000000000000, 0.8660254037844387076, 1.000000000000000000, 0.8660254037844387076, 1.000000000000000000, 0.8660254037844387076, 1.000000000000000000, 0.8660254037844387076, 1.000000000000000000, 0.8660254037844387076, 1.000000000000000000, 0.8660254037844387076, 1.000000000000000000, 0.8660254037844387076, 1.000000000000000000, 0.8660254037844387076, 1.000000000000000000, 0.8660254037844387076, 1.000000000000000000, 0.8660254037844387076, 1.000000000000000000, 0.8660254037844387076, 1.000000000000000000, 0.8660254037844387076, 1.000000000000000000, 0.8660254037844387076, 1.000000000000000000, 0.8660254037844387076, 1.000000000000000000, 0.8660254037844387076, 1.000000000000000000, 0.8660254037844387076, 1.000000000000000000, 0.8660254037844387076, 1.000000000000000000, 0.8660254037844387076, 1.000000000000000000, 0.8660254037844387076, 1.000000000000000000, 0.8660254037844387076, 1.000000000000000000, 0.8660254037844387076, 1.000000000000000000, 0.8660254037844387076, 1.000000000000000000, 0.8660254037844387076, 1.000000000000000000, 0.8660254037844387076, 1.000000000000000000, 0.8660254037844387076, 1.000000000000000000, 0.8660254037844387076, 1.000000000000000000, 0.8660254037844387076, 1.000000000000000000, 0.8660254037844387076, 1.000000000000000000, 0.8660254037844387076, 1.000000000000000000, 0.8660254037844387076, 1.000000000000000000, 0.8660254037844387076, 1.000000000000000000, 0.8660254037844387076, 1.000000000000000000, 0.8660254037844387076, 1.000000000000000000, 0.8660254037844387076, 1.000000000000000000, 0.8660254037844387076, 1.000000000000000000, 0.8660254037844387076, 1.000000000000000000, 0.8660254037844387076, 1.000000000000000000, 0.8660254037844387076, 1.000000000000000000, 0.8660254037844387076, 1.000000000000000000, 0.8660254037844387076, 1.000000000000000000, 0.8660254037844387076, 1.000000000000000000, 0.8660254037844387076, 1.000000000000000000, 0.8660254037844387076, 1.000000000000000000, 0.8660254037844387076, 1.000000000000000000, 0.8660254037844387076, 1.000000000000000000, 0.8660254037844387076, 1.000000000000000000, 0.8660254037844387076, 1.000000000000000000, 0.8660254037844387076, 1.000000000000000000, 0.8660254037844387076, 1.000000000000000000, 0.8660254037844387076, 1.000000000000000000, 0.8660254037844387076, 1.000000000000000000, 0.8660254037844387076, 1.000000000000000000, 0.8660254037844387076, 1.000000000000000000, 0.8660254037844387076, 1.000000000000000000, 0.8660254037844387076, 1.000000000000000000, 0.8660254037844387076, 1.000000000000000000, 0.8660254037844387076, 1.000000000000000000, 0.8660254037844387076, 1.000000000000000000, 0.8660254037844387076, 1.000000000000000000, 0.8660254037844387076, 1.000000000000000000, 0.8660254037844387076, 1.000000000000000000, 0.8660254037844387076, 1.000000000000000000, 0.8660254037844387076, 1.000000000000000000, 0.8660254037844387076, 1.000000000000000000, 0.8660254037844387076, 1.000000000000000000, 0.8660254037844387076, 1.000000000000000000, 0.8660254037844387076, 1.000000000000000000, 0.8660254037844387076, 1.000000000000000000, 0.8660254037844387076, 1.000000000000000000, 0.8660254037844387076, 1.000000000000000000, 0.8660254037844387076, 1.000000000000000000, 0.8660254037844387076, 1.000000000000000000, 0.8660254037844387076, 1.000000000000000000, 0.8660254037844387076, 1.000000000000000000, 0.8660254037844387076, 1.000000000000000000, 0.8660254037844387076, 1.000000000000000000, 0.8660254037844387076, 1.000000000000000000, 0.8660254037844387076, 1.000000000000000000, 0.8660254037844387076, 1.000000000000000000, 0.8660254037844387076, 1.000000000000000000, 0.8660254037844387076, 1.000000000000000000, 0.8660254037844387076, 1.000000000000000000, 0.8660254037844387076, 1.000000000000000000, 0.8660254037844387076, 1.000000000000000000, 0.8660254037844387076, 1.000000000000000000, 0.8660254037844387076, 1.000000000000000000, 0.8660254037844387076, 1.000000000000000000, 0.8660254037844387076, 1.000000000000000000, 0.8660254037844387076, 1.000000000000000000, 0.8660254037844387076, 1.000000000000000000, 0.8660254037844387076, 1.000000000000000000, 0.8660254037844387076, 1.000000000000000000, 0.8660254037844387076, 1.000000000000000000, 0.8660254037844387076, 1.000000000000000000, 0.8660254037844387076, 1.000000000000000000, 0.8660254037844387076, 1.000000000000000000, 0.8660254037844387076, 1.000000000000000000, 0.8660254037844387076, 1.000000000000000000, 0.8660254037844387076, 1.000000000000000000, 0.8660254037844387076, 1.000000000000000000, 0.8660254037844387076, 1.000000000000000000, 0.8660254037844387076, 1.000000000000000000, 0.8660254037844387076, 1.000000000000000000, 0.8660254037844387076, 1.000000000000000000, 0.8660254037844387076, 1.000000000000000000, 0.8660254037844387076, 1.000000000000000000, 0.8660254037844387076, 1.000000000000000000, 0.8660254037844387076, 1.000000000000000000, 0.8660254037844387076, 1.000000000000000000, 0.8660254037844387076, 1.000000000000000000, 0.8660254037844387076, 1.000000000000000000, 0.8660254037844387076, 1.000000000000000000, 0.8660254037844387076, 1.000000000000000000, 0.8660254037844387076, 1.000000000000000000, 0.8660254037844387076, 1.000000000000000000, 0.8660254037844387076, 1.000000000000000000, 0.8660254037844387076, 1.000000000000000000, 0.8660254037844387076, 1.000000000000000000, 0.8660254037844387076, 1.000000000000000000, 0.8660254037844387076, 1.000000000000000000, 0.8660254037844387076, 1.000000000000000000, 0.8660254037844387076, 1.000000000000000000, 0.8660254037844387076, 1.000000000000000000, 0.8660254037844387076, 1.000000000000000000, 0.8660254037844387076, 1.000000000000000000, 0.8660254037844387076, 1.000000000000000000, 0.8660254037844387076, 1.000000000000000000, 0.8660254037844387076, 1.000000000000000000, 0.8660254037844387076, 1.000000000000000000, 0.8660254037844387076, 1.000000000000000000, 0.8660254037844387076, 1.000000000000000000, 0.8660254037844387076, 1.000000000000000000, 0.8660254037844387076, 1.000000000000000000, 0.8660254037844387076, 1.000000000000000000, 0.8660254037844387076, 1.000000000000000000, 0.8660254037844387076, 1.000000000000000000, 0.9024560516293018697, 0.9469512977404641596) ) ) 
 REPRESENTATION_ITEM ( '' )  SURFACE ( )  );
#16512 = DIRECTION ( 'NONE',  ( -1.000000000000000000, 0.000000000000000000, 0.000000000000000000 ) ) ;
#16513 = CARTESIAN_POINT ( 'NONE',  ( 96.32499999999998863, 87.70503267997126784, 78.78166666666666629 ) ) ;
#16514 = CARTESIAN_POINT ( 'NONE',  ( 0.000000000000000000, 29.01471420065563933, 76.69515212746026123 ) ) ;
#16515 = CARTESIAN_POINT ( 'NONE',  ( -97.30629616937501680, 88.66845928578038638, 88.42572916753381662 ) ) ;
#16516 = CARTESIAN_POINT ( 'NONE',  ( 0.000000000000000000, 35.38097989696528600, -12.42422080174602605 ) ) ;
#16517 = CARTESIAN_POINT ( 'NONE',  ( -97.64999999999994884, -211.5299782133524502, 86.24291666666665890 ) ) ;
#16518 = VECTOR ( 'NONE', #13502, 1000.000000000000000 ) ;
#16519 = EDGE_CURVE ( 'NONE', #36744, #9362, #70994, .T. ) ;
#16520 = CARTESIAN_POINT ( 'NONE',  ( 0.000000000000000000, 0.000000000000000000, 2.500000000000000000 ) ) ;
#16521 = ORIENTED_EDGE ( 'NONE', *, *, #47397, .T. ) ;
#16522 = CARTESIAN_POINT ( 'NONE',  ( 11.99999999999999822, -73.73191006444582740, 14.66109333815435889 ) ) ;
#16523 = LINE ( 'NONE', #17269, #68349 ) ;
#16524 =( NAMED_UNIT ( * ) SI_UNIT ( $, .STERADIAN. ) SOLID_ANGLE_UNIT ( ) );
#16525 = DIRECTION ( 'NONE',  ( 0.000000000000000000, 0.000000000000000000, 1.000000000000000000 ) ) ;
#16526 = CARTESIAN_POINT ( 'NONE',  ( 92.69370383062501162, -211.3315407142195852, 86.67947916753382742 ) ) ;
#16527 = VERTEX_POINT ( 'NONE', #31148 ) ;
#16528 = EDGE_CURVE ( 'NONE', #64295, #143, #67746, .T. ) ;
#16529 = ORIENTED_EDGE ( 'NONE', *, *, #15947, .F. ) ;
#16530 = EDGE_CURVE ( 'NONE', #32728, #4573, #962, .T. ) ;
#16531 = FACE_OUTER_BOUND ( 'NONE', #25165, .T. ) ;
#16532 = ORIENTED_EDGE ( 'NONE', *, *, #51632, .F. ) ;
#16533 = CARTESIAN_POINT ( 'NONE',  ( 11.99999999999999822, 63.18004540533030422, 44.88180994100399346 ) ) ;
#16534 = CARTESIAN_POINT ( 'NONE',  ( 93.84685191531251292, -211.9973110713294489, 78.95364583420047211 ) ) ;
#16535 = CIRCLE ( 'NONE', #10519, 16.00000000000000000 ) ;
#16536 = ORIENTED_EDGE ( 'NONE', *, *, #40182, .T. ) ;
#16537 = CARTESIAN_POINT ( 'NONE',  ( 93.84685191531251292, -211.9973110713294489, 84.19239583420049655 ) ) ;
#16538 = EDGE_CURVE ( 'NONE', #61399, #46926, #54534, .T. ) ;
#16539 = EDGE_CURVE ( 'NONE', #32269, #40792, #24547, .T. ) ;
#16540 = VERTEX_POINT ( 'NONE', #36418 ) ;
#16541 = DIRECTION ( 'NONE',  ( 2.603472992745699578E-14, -2.546204323184531851E-14, 1.000000000000000000 ) ) ;
#16542 = ORIENTED_EDGE ( 'NONE', *, *, #5902, .T. ) ;
#16543 = ORIENTED_EDGE ( 'NONE', *, *, #36310, .F. ) ;
#16544 = FACE_OUTER_BOUND ( 'NONE', #47564, .T. ) ;
#16545 = VECTOR ( 'NONE', #15003, 1000.000000000000000 ) ;
#16546 = LINE ( 'NONE', #39493, #62889 ) ;
#16547 = AXIS2_PLACEMENT_3D ( 'NONE', #841, #64328, #57946 ) ;
#16548 = ORIENTED_EDGE ( 'NONE', *, *, #13160, .T. ) ;
#16549 = CARTESIAN_POINT ( 'NONE',  ( 96.32499999999997442, 92.29496732002878900, 85.97833333333332462 ) ) ;
#16550 = DIRECTION ( 'NONE',  ( 0.000000000000000000, 0.000000000000000000, 1.000000000000000000 ) ) ;
#16551 = EDGE_LOOP ( 'NONE', ( #5683, #73849, #26170, #11533 ) ) ;
#16552 = DIRECTION ( 'NONE',  ( 0.000000000000000000, 0.000000000000000000, 1.000000000000000000 ) ) ;
#16553 = ORIENTED_EDGE ( 'NONE', *, *, #41317, .F. ) ;
#16554 = CARTESIAN_POINT ( 'NONE',  ( 5.000000000000000000, -22.48208911017474065, -35.47612816024548721 ) ) ;
#16555 = EDGE_CURVE ( 'NONE', #48891, #20209, #60561, .T. ) ;
#16556 = VERTEX_POINT ( 'NONE', #29656 ) ;
#16557 = VERTEX_POINT ( 'NONE', #53348 ) ;
#16558 = VERTEX_POINT ( 'NONE', #7853 ) ;
#16559 = CARTESIAN_POINT ( 'NONE',  ( 96.15314808468750130, -211.9973110713294489, 76.51947916753380241 ) ) ;
#16560 = ITEM_DEFINED_TRANSFORMATION ( 'NONE', 'NONE', #67633,  #43395 ) ;
#16561 = CARTESIAN_POINT ( 'NONE',  ( -4.999999999999999112, -1.831125658499874964, -1.158123955083390388 ) ) ;
#16562 = ORIENTED_EDGE ( 'NONE', *, *, #28166, .F. ) ;
#16563 = ORIENTED_EDGE ( 'NONE', *, *, #38260, .T. ) ;
#16564 = AXIS2_PLACEMENT_3D ( 'NONE', #47637, #70544, #19055 ) ;
#16565 = ORIENTED_EDGE ( 'NONE', *, *, #37335, .T. ) ;
#16566 = DIRECTION ( 'NONE',  ( 1.000000000000000000, 0.000000000000000000, 0.000000000000000000 ) ) ;
#16567 = CARTESIAN_POINT ( 'NONE',  ( -96.32499999999996021, -207.7050326799711968, 88.62416666666665321 ) ) ;
#16568 = VECTOR ( 'NONE', #25778, 1000.000000000000000 ) ;
#16569 = VECTOR ( 'NONE', #25302, 1000.000000000000000 ) ;
#16570 = CARTESIAN_POINT ( 'NONE',  ( -95.00000000000002842, 87.33691857156074434, 76.62531250086715318 ) ) ;
#16571 = EDGE_CURVE ( 'NONE', #67855, #41196, #52987, .T. ) ;
#16572 = ORIENTED_EDGE ( 'NONE', *, *, #46491, .F. ) ;
#16573 = CARTESIAN_POINT ( 'NONE',  ( 97.30629616937498838, 88.66845928578037217, 75.93739583420047268 ) ) ;
#16574 = PRESENTATION_LAYER_ASSIGNMENT (  '', '', ( #32177 ) ) ;
#16575 = VERTEX_POINT ( 'NONE', #18033 ) ;
#16576 = DIRECTION ( 'NONE',  ( 0.000000000000000000, 0.000000000000000000, 1.000000000000000000 ) ) ;
#16577 = CARTESIAN_POINT ( 'NONE',  ( -96.15314808468745866, -211.9973110713294489, 87.20864583420046756 ) ) ;
#16578 = EDGE_LOOP ( 'NONE', ( #54271, #65011, #23966, #27736, #3614, #65107, #26363, #21177 ) ) ;
#16579 = EDGE_CURVE ( 'NONE', #15229, #50948, #59326, .T. ) ;
#16580 = DIRECTION ( 'NONE',  ( -0.9435911131814395114, 0.3311129884571304971, 0.000000000000000000 ) ) ;
#16581 = DIRECTION ( 'NONE',  ( 1.000000000000000000, 0.000000000000000000, -0.000000000000000000 ) ) ;
#16582 = CYLINDRICAL_SURFACE ( 'NONE', #58510, 16.00000000000000000 ) ;
#16583 = CARTESIAN_POINT ( 'NONE',  ( -94.99999999999997158, -212.6630814284392557, 79.64156250086713840 ) ) ;
#16584 = LINE ( 'NONE', #44426, #23074 ) ;
#16585 = CYLINDRICAL_SURFACE ( 'NONE', #43991, 31.99999999999999289 ) ;
#16586 = CARTESIAN_POINT ( 'NONE',  ( -94.99999999999997158, -213.0599564267049857, 79.36374999999996760 ) ) ;
#16587 = DIRECTION ( 'NONE',  ( 0.000000000000000000, 0.000000000000000000, 1.000000000000000000 ) ) ;
#16588 = CARTESIAN_POINT ( 'NONE',  ( 10.00000000000000000, -37.22597642581153821, -5.202137450156795850 ) ) ;
#16589 = CARTESIAN_POINT ( 'NONE',  ( 1.243286885786405054E-17, -120.0000000000000000, -85.60000000000000853 ) ) ;
#16590 = CARTESIAN_POINT ( 'NONE',  ( -97.30629616937501680, 90.00000000000004263, 81.38781250086714181 ) ) ;
#16591 = CYLINDRICAL_SURFACE ( 'NONE', #59876, 37.49900000000000233 ) ;
#16592 = FACE_OUTER_BOUND ( 'NONE', #65027, .T. ) ;
#16593 = VECTOR ( 'NONE', #2903, 1000.000000000000000 ) ;
#16594 = VERTEX_POINT ( 'NONE', #18385 ) ;
#16595 = DIRECTION ( 'NONE',  ( -1.000000000000000000, 0.000000000000000000, 0.000000000000000000 ) ) ;
#16596 = AXIS2_PLACEMENT_3D ( 'NONE', #32862, #15207, #55060 ) ;
#16597 = CIRCLE ( 'NONE', #52594, 37.49900000000001654 ) ;
#16598 = CARTESIAN_POINT ( 'NONE',  ( -12.50000000000000000, -132.5000000000000000, -2.500000000000000000 ) ) ;
#16599 = DIRECTION ( 'NONE',  ( 0.000000000000000000, 0.2079116908177555123, -0.9781476007338064660 ) ) ;
#16601 = CIRCLE ( 'NONE', #70618, 82.00000000000000000 ) ;
#16600 = PLANE ( 'NONE',  #20226 ) ;
#16602 = FACE_OUTER_BOUND ( 'NONE', #63883, .T. ) ;
#16603 = LINE ( 'NONE', #32401, #26782 ) ;
#16604 = CARTESIAN_POINT ( 'NONE',  ( -97.30629616937497417, -211.3315407142195852, 77.78947916753381264 ) ) ;
#16605 = CIRCLE ( 'NONE', #20190, 3.000000000000000888 ) ;
#16606 = DIRECTION ( 'NONE',  ( -1.000000000000000000, 0.000000000000000000, 0.000000000000000000 ) ) ;
#16607 = ADVANCED_FACE ( 'NONE', ( #41333 ), #24406, .F. ) ;
#16608 = ORIENTED_EDGE ( 'NONE', *, *, #5627, .F. ) ;
#16609 = CARTESIAN_POINT ( 'NONE',  ( 0.000000000000000000, 0.000000000000000000, 0.000000000000000000 ) ) ;
#16610 = DIRECTION ( 'NONE',  ( 0.000000000000000000, 0.000000000000000000, 1.000000000000000000 ) ) ;
#16611 = DIRECTION ( 'NONE',  ( 0.000000000000000000, 0.000000000000000000, 1.000000000000000000 ) ) ;
#16612 = DIRECTION ( 'NONE',  ( 0.000000000000000000, 0.9510565162951544194, -0.3090169943749447867 ) ) ;
#16613 = AXIS2_PLACEMENT_3D ( 'NONE', #34354, #67460, #5442 ) ;
#16614 = DIRECTION ( 'NONE',  ( -1.000000000000000000, -0.000000000000000000, 0.000000000000000000 ) ) ;
#16615 = EDGE_CURVE ( 'NONE', #60292, #7320, #52122, .T. ) ;
#16616 = AXIS2_PLACEMENT_3D ( 'NONE', #65313, #54758, #38205 ) ;
#16617 = EDGE_CURVE ( 'NONE', #31218, #36914, #1726, .T. ) ;
#16619 = CARTESIAN_POINT ( 'NONE',  ( 6.000000000000000000, 81.50828551894240093, -8.966570791699810528 ) ) ;
#16618 = AXIS2_PLACEMENT_3D ( 'NONE', #58059, #57320, #35125 ) ;
#16620 = VERTEX_POINT ( 'NONE', #47704 ) ;
#16621 = VECTOR ( 'NONE', #70399, 1000.000000000000000 ) ;
#16622 = CARTESIAN_POINT ( 'NONE',  ( 11.99999999999999822, 75.11725578898467859, 2.956366410620910656 ) ) ;
#16623 = CARTESIAN_POINT ( 'NONE',  ( 11.99999999999999822, -2.956366410621191765, 75.11725578898467859 ) ) ;
#16624 = EDGE_LOOP ( 'NONE', ( #53532, #69174, #26505, #58707 ) ) ;
#16625 = VECTOR ( 'NONE', #55635, 1000.000000000000114 ) ;
#16626 = CARTESIAN_POINT ( 'NONE',  ( 93.84685191531249870, -208.0026889286704943, 88.90197916753380980 ) ) ;
#16627 = CARTESIAN_POINT ( 'NONE',  ( -97.64999999999994884, 91.52997821335257811, 77.88208333333332689 ) ) ;
#16628 = EDGE_LOOP ( 'NONE', ( #63848, #27149, #48258, #20139 ) ) ;
#16629 = CYLINDRICAL_SURFACE ( 'NONE', #45307, 3.299999999999969624 ) ;
#16630 = ADVANCED_FACE ( 'NONE', ( #3353 ), #54828, .F. ) ;
#16631 = ORIENTED_EDGE ( 'NONE', *, *, #12021, .T. ) ;
#16632 = DIRECTION ( 'NONE',  ( -1.000000000000000000, 0.000000000000000000, 0.000000000000000000 ) ) ;
#16633 = ORIENTED_EDGE ( 'NONE', *, *, #34539, .T. ) ;
#16634 = DIRECTION ( 'NONE',  ( 0.4796670183876317051, -0.8774505977381971134, 0.000000000000000000 ) ) ;
#16635 = ORIENTED_EDGE ( 'NONE', *, *, #56744, .T. ) ;
#16636 = ORIENTED_EDGE ( 'NONE', *, *, #2343, .T. ) ;
#16637 = ORIENTED_EDGE ( 'NONE', *, *, #8716, .F. ) ;
#16638 = DIRECTION ( 'NONE',  ( -1.000000000000000000, 0.000000000000000000, 0.000000000000000000 ) ) ;
#16639 = VERTEX_POINT ( 'NONE', #25881 ) ;
#16640 = EDGE_CURVE ( 'NONE', #50612, #16250, #23995, .T. ) ;
#16641 = VERTEX_POINT ( 'NONE', #61589 ) ;
#16642 = CARTESIAN_POINT ( 'NONE',  ( 97.64999999999997726, 88.47002178664753558, 87.08958333333333712 ) ) ;
#16643 = FACE_OUTER_BOUND ( 'NONE', #11799, .T. ) ;
#16644 = VECTOR ( 'NONE', #6580, 1000.000000000000000 ) ;
#16645 = EDGE_CURVE ( 'NONE', #69079, #10016, #50941, .T. ) ;
#16646 = FACE_OUTER_BOUND ( 'NONE', #2240, .T. ) ;
#16647 = EDGE_CURVE ( 'NONE', #69147, #67241, #18530, .T. ) ;
#16648 = CIRCLE ( 'NONE', #58673, 42.00000000000000000 ) ;
#16649 = VERTEX_POINT ( 'NONE', #4460 ) ;
#16650 = AXIS2_PLACEMENT_3D ( 'NONE', #30095, #11686, #34260 ) ;
#16651 = VERTEX_POINT ( 'NONE', #26245 ) ;
#16652 = VERTEX_POINT ( 'NONE', #43932 ) ;
#16653 = CARTESIAN_POINT ( 'NONE',  ( 93.84685191531248449, 91.99731107132950569, 85.72697916753379843 ) ) ;
#16655 = ORIENTED_EDGE ( 'NONE', *, *, #36856, .T. ) ;
#16654 = ADVANCED_FACE ( 'NONE', ( #20619 ), #9326, .T. ) ;
#16656 = CARTESIAN_POINT ( 'NONE',  ( 95.00000000000000000, -207.3369185715606307, 85.03906250086714635 ) ) ;
#16657 = SHAPE_DEFINITION_REPRESENTATION ( #25942, #23018 ) ;
#16658 = FACE_OUTER_BOUND ( 'NONE', #58234, .T. ) ;
#16659 = VECTOR ( 'NONE', #3852, 1000.000000000000000 ) ;
#16660 = DIRECTION ( 'NONE',  ( 0.000000000000000000, -0.5877852522924803536, 0.8090169943749422332 ) ) ;
#16661 = FACE_OUTER_BOUND ( 'NONE', #45902, .T. ) ;
#16662 = AXIS2_PLACEMENT_3D ( 'NONE', #21879, #51933, #30102 ) ;
#16663 = FACE_OUTER_BOUND ( 'NONE', #45829, .T. ) ;
#16664 = CARTESIAN_POINT ( 'NONE',  ( 6.000000000000000000, -2.543863470248951320, 81.96053171279901051 ) ) ;
#16665 = CARTESIAN_POINT ( 'NONE',  ( 0.000000000000000000, 81.96053171279902472, 2.543863470248677316 ) ) ;
#16666 = CARTESIAN_POINT ( 'NONE',  ( -92.69370383062498320, -211.3315407142195852, 88.63739583420047552 ) ) ;
#16667 = CARTESIAN_POINT ( 'NONE',  ( -97.30629616937501680, 88.66845928578038638, 86.67947916753382742 ) ) ;
#16668 = EDGE_CURVE ( 'NONE', #28318, #63927, #26984, .T. ) ;
#16669 = ORIENTED_EDGE ( 'NONE', *, *, #21278, .F. ) ;
#16671 = CARTESIAN_POINT ( 'NONE',  ( -95.00000000000002842, 92.66308142843932671, 84.40406250086712703 ) ) ;
#16670 = CARTESIAN_POINT ( 'NONE',  ( 97.30629616937498838, 91.33154071421968467, 83.02822916753379445 ) ) ;
#16672 = ORIENTED_EDGE ( 'NONE', *, *, #72647, .F. ) ;
#16673 = DIRECTION ( 'NONE',  ( -1.000000000000000000, 0.000000000000000000, -0.000000000000000000 ) ) ;
#16674 = CARTESIAN_POINT ( 'NONE',  ( -2.500000000000000000, 3.061616997868383141E-16, -5.624496230895140947 ) ) ;
#16675 = DIRECTION ( 'NONE',  ( 1.000000000000000000, 0.000000000000000000, 0.000000000000000000 ) ) ;
#16676 = CARTESIAN_POINT ( 'NONE',  ( 0.000000000000000000, 55.38113227695858143, -54.21277698773617715 ) ) ;
#16677 = AXIS2_PLACEMENT_3D ( 'NONE', #73440, #18158, #1292 ) ;
#16678 = CARTESIAN_POINT ( 'NONE',  ( -26.50044424985255276, 0.001194404164626844313, -64.00000000000000000 ) ) ;
#16679 = CARTESIAN_POINT ( 'NONE',  ( -95.00000000000002842, 90.00000000000004263, 90.00000000000000000 ) ) ;
#16680 = VECTOR ( 'NONE', #70279, 1000.000000000000114 ) ;
#16681 = DIRECTION ( 'NONE',  ( -1.000000000000000000, -0.000000000000000000, 0.000000000000000000 ) ) ;
#16682 = LINE ( 'NONE', #27951, #15760 ) ;
#16683 = DIRECTION ( 'NONE',  ( 0.000000000000000000, 0.7071067811865487940, -0.7071067811865462405 ) ) ;
#16684 = ORIENTED_EDGE ( 'NONE', *, *, #62980, .F. ) ;
#16685 = VECTOR ( 'NONE', #5301, 1000.000000000000114 ) ;
#16686 = ORIENTED_EDGE ( 'NONE', *, *, #31911, .T. ) ;
#16687 = VECTOR ( 'NONE', #47427, 1000.000000000000114 ) ;
#16688 = AXIS2_PLACEMENT_3D ( 'NONE', #16609, #23730, #115 ) ;
#16689 = CARTESIAN_POINT ( 'NONE',  ( -96.32500000000001705, 87.70503267997129626, 79.31083333333333485 ) ) ;
#16690 = DIRECTION ( 'NONE',  ( 0.000000000000000000, 0.000000000000000000, 1.000000000000000000 ) ) ;
#16691 = DIRECTION ( 'NONE',  ( -1.000000000000000000, -0.000000000000000000, 0.000000000000000000 ) ) ;
#16692 = FACE_BOUND ( 'NONE', #51137, .T. ) ;
#16693 = DIRECTION ( 'NONE',  ( 0.000000000000000000, 0.000000000000000000, 1.000000000000000000 ) ) ;
#16694 = CARTESIAN_POINT ( 'NONE',  ( -3.000000000000000888, 20.64000000000000057, 0.000000000000000000 ) ) ;
#16695 = DIRECTION ( 'NONE',  ( -1.000000000000000000, 0.000000000000000000, 0.000000000000000000 ) ) ;
#16696 = CIRCLE ( 'NONE', #27453, 82.00000000000000000 ) ;
#16697 = ORIENTED_EDGE ( 'NONE', *, *, #58049, .T. ) ;
#16698 = CARTESIAN_POINT ( 'NONE',  ( -92.69370383062504004, 90.00000000000004263, 77.26031250086714408 ) ) ;
#16699 = PLANE ( 'NONE',  #67969 ) ;
#16700 = LINE ( 'NONE', #45661, #26165 ) ;
#16701 = CARTESIAN_POINT ( 'NONE',  ( -20.63749999999999574, -2.946905753440916183E-14, -1.643265707205091412E-14 ) ) ;
#16702 = LINE ( 'NONE', #68207, #18905 ) ;
#16703 = DIRECTION ( 'NONE',  ( -1.000000000000000000, -0.000000000000000000, -0.000000000000000000 ) ) ;
#16704 = CARTESIAN_POINT ( 'NONE',  ( -97.30629616937495996, -209.9999999999999716, 88.53156250086716739 ) ) ;
#16705 = SURFACE_STYLE_FILL_AREA ( #27972 ) ;
#16706 = AXIS2_PLACEMENT_3D ( 'NONE', #44505, #62927, #11384 ) ;
#16707 = CARTESIAN_POINT ( 'NONE',  ( 97.30629616937498838, 88.66845928578035796, 76.09614583420048461 ) ) ;
#16708 = AXIS2_PLACEMENT_3D ( 'NONE', #48261, #25696, #19310 ) ;
#16709 = CIRCLE ( 'NONE', #11864, 31.99999999999999645 ) ;
#16710 = EDGE_CURVE ( 'NONE', #53528, #968, #32996, .T. ) ;
#16711 = CARTESIAN_POINT ( 'NONE',  ( -94.99999999999997158, -212.6630814284392557, 79.16531250086715943 ) ) ;
#16712 = CARTESIAN_POINT ( 'NONE',  ( -97.64999999996712177, 90.00000839536629371, 84.99910573348492449 ) ) ;
#16713 = ORIENTED_EDGE ( 'NONE', *, *, #64751, .F. ) ;
#16714 = CARTESIAN_POINT ( 'NONE',  ( -92.35000000000003695, 90.00002467581377630, 87.22187585518554442 ) ) ;
#16715 = CARTESIAN_POINT ( 'NONE',  ( -96.32499999999996021, -207.7050326799711968, 75.92416666666666458 ) ) ;
#16716 = EDGE_CURVE ( 'NONE', #67113, #14221, #10072, .T. ) ;
#16717 = AXIS2_PLACEMENT_3D ( 'NONE', #72412, #37486, #38209 ) ;
#16718 = DIRECTION ( 'NONE',  ( 0.000000000000000000, -0.7071067811865389130, -0.7071067811865563435 ) ) ;
#16719 = AXIS2_PLACEMENT_3D ( 'NONE', #41296, #36015, #18351 ) ;
#16720 = EDGE_CURVE ( 'NONE', #19951, #62129, #55199, .T. ) ;
#16721 = AXIS2_PLACEMENT_3D ( 'NONE', #14205, #70976, #53694 ) ;
#16722 = EDGE_CURVE ( 'NONE', #27761, #30878, #37180, .T. ) ;
#16723 = CARTESIAN_POINT ( 'NONE',  ( -93.84685191531252713, 88.00268892867056536, 77.31322916753381946 ) ) ;
#16724 = CARTESIAN_POINT ( 'NONE',  ( 92.69370383062501162, -211.3315407142195852, 81.44072916753381719 ) ) ;
#16725 = ORIENTED_EDGE ( 'NONE', *, *, #57755, .T. ) ;
#16726 = CARTESIAN_POINT ( 'NONE',  ( -20.63749999999997797, 2.238751767990224802E-13, 23.50000000000040146 ) ) ;
#16727 = VERTEX_POINT ( 'NONE', #43201 ) ;
#16728 = EDGE_CURVE ( 'NONE', #65017, #73292, #72836, .T. ) ;
#16729 = ORIENTED_EDGE ( 'NONE', *, *, #22042, .F. ) ;
#16730 = VECTOR ( 'NONE', #9659, 1000.000000000000000 ) ;
#16731 = CONICAL_SURFACE ( 'NONE', #41956, 13.71319123046128752, 0.2094395102393127317 ) ;
#16732 = CARTESIAN_POINT ( 'NONE',  ( -10.00000000000000000, 0.000000000000000000, 0.000000000000000000 ) ) ;
#16733 = AXIS2_PLACEMENT_3D ( 'NONE', #54782, #47300, #42396 ) ;
#16734 = ORIENTED_EDGE ( 'NONE', *, *, #956, .F. ) ;
#16735 = ORIENTED_EDGE ( 'NONE', *, *, #31137, .F. ) ;
#16736 = VECTOR ( 'NONE', #31143, 1000.000000000000000 ) ;
#16737 = ORIENTED_EDGE ( 'NONE', *, *, #43425, .F. ) ;
#16738 = CARTESIAN_POINT ( 'NONE',  ( 92.69370383062501162, -208.6684592857803295, 75.14364583420049826 ) ) ;
#16739 = ORIENTED_EDGE ( 'NONE', *, *, #37516, .T. ) ;
#16740 = CARTESIAN_POINT ( 'NONE',  ( 11.99999999999999822, 74.74816331893428867, 33.71516098798767302 ) ) ;
#16741 = CARTESIAN_POINT ( 'NONE',  ( 93.67500000000001137, -212.2949673200287179, 83.75583333333332803 ) ) ;
#16742 =( BOUNDED_CURVE ( )  B_SPLINE_CURVE ( 2, ( #33585, #50510, #62942, #44519, #73437, #38866, #40349 ),
 .UNSPECIFIED., .F., .F. ) 
 B_SPLINE_CURVE_WITH_KNOTS ( ( 3, 2, 2, 3 ),
 ( 0.5000000000000000000, 0.5069444444444444198, 0.5138888888888887285, 0.5208333333333332593 ),
 .UNSPECIFIED. ) 
 CURVE ( )  GEOMETRIC_REPRESENTATION_ITEM ( )  RATIONAL_B_SPLINE_CURVE ( ( 1.000000000000000000, 0.8660254037844387076, 1.000000000000000000, 0.8660254037844387076, 1.000000000000000000, 0.8660254037844408170, 0.9999999999999978906 ) ) 
 REPRESENTATION_ITEM ( '' )  );
#16743 = CARTESIAN_POINT ( 'NONE',  ( 96.15314808468748708, 88.00268892867053694, 84.93322916753382401 ) ) ;
#16744 = CARTESIAN_POINT ( 'NONE',  ( 3.000000000000000000, -3.004629197474318063E-15, -2.541999999999999815 ) ) ;
#16745 = CARTESIAN_POINT ( 'NONE',  ( 96.32499999999998863, -207.7050326799711968, 79.62833333333333030 ) ) ;
#16746 = VERTEX_POINT ( 'NONE', #19865 ) ;
#16747 = EDGE_LOOP ( 'NONE', ( #10902, #4611, #34494, #13552 ) ) ;
#16748 = ORIENTED_EDGE ( 'NONE', *, *, #36567, .T. ) ;
#16749 = ORIENTED_EDGE ( 'NONE', *, *, #36938, .T. ) ;
#16750 = SURFACE_STYLE_FILL_AREA ( #39688 ) ;
#16751 = EDGE_CURVE ( 'NONE', #60033, #66693, #70142, .T. ) ;
#16752 = EDGE_CURVE ( 'NONE', #4754, #42720, #58139, .T. ) ;
#16753 = CARTESIAN_POINT ( 'NONE',  ( 18.80329974962065265, -105.8248132807389084, -2.500000000000000000 ) ) ;
#16754 = DIRECTION ( 'NONE',  ( -1.000000000000000000, 0.000000000000000000, -0.000000000000000000 ) ) ;
#16755 = CYLINDRICAL_SURFACE ( 'NONE', #4216, 31.99999999999998579 ) ;
#16756 = CARTESIAN_POINT ( 'NONE',  ( 95.00000000000000000, -209.9999999999999716, 90.00000000000000000 ) ) ;
#16757 = DIRECTION ( 'NONE',  ( -1.000000000000000000, -0.000000000000000000, 0.000000000000000000 ) ) ;
#16758 = ORIENTED_EDGE ( 'NONE', *, *, #51683, .T. ) ;
#16759 = CARTESIAN_POINT ( 'NONE',  ( -93.67499999999998295, -207.7050326799711968, 82.88270833506763324 ) ) ;
#16760 = ORIENTED_EDGE ( 'NONE', *, *, #4001, .F. ) ;
#16761 = CARTESIAN_POINT ( 'NONE',  ( 0.000000000000000000, -37.58145647212453611, -0.6853352020794456489 ) ) ;
#16762 = EDGE_CURVE ( 'NONE', #39126, #35029, #14601, .T. ) ;
#16763 = ORIENTED_EDGE ( 'NONE', *, *, #70526, .T. ) ;
#16765 = CARTESIAN_POINT ( 'NONE',  ( -92.35000000000003695, 90.00000000000004263, 79.60187500173429953 ) ) ;
#16764 = CARTESIAN_POINT ( 'NONE',  ( 97.64999999999997726, 91.52997821335252127, 81.55979166840097605 ) ) ;
#16766 = AXIS2_PLACEMENT_3D ( 'NONE', #17321, #28589, #52640 ) ;
#16767 = ORIENTED_EDGE ( 'NONE', *, *, #17980, .F. ) ;
#16768 = CARTESIAN_POINT ( 'NONE',  ( 96.15314808468748708, 88.00268892867053694, 84.29822916753381890 ) ) ;
#16769 = CARTESIAN_POINT ( 'NONE',  ( -93.67499999999998295, -207.7050326799711968, 86.61333333333332973 ) ) ;
#16770 = DIRECTION ( 'NONE',  ( -1.000000000000000000, 0.000000000000000000, 0.000000000000000000 ) ) ;
#16771 = AXIS2_PLACEMENT_3D ( 'NONE', #51099, #74023, #51468 ) ;
#16772 = CARTESIAN_POINT ( 'NONE',  ( 11.99999999999999822, 0.000000000000000000, 0.000000000000000000 ) ) ;
#16773 = FACE_OUTER_BOUND ( 'NONE', #21696, .T. ) ;
#16774 = AXIS2_PLACEMENT_3D ( 'NONE', #41814, #31273, #53838 ) ;
#16775 = DIRECTION ( 'NONE',  ( 0.000000000000000000, 0.3090169943749480619, -0.9510565162951533091 ) ) ;
#16776 = ORIENTED_EDGE ( 'NONE', *, *, #66053, .T. ) ;
#16777 = LINE ( 'NONE', #16396, #36139 ) ;
#16778 = LINE ( 'NONE', #51342, #38413 ) ;
#16779 = ORIENTED_EDGE ( 'NONE', *, *, #70600, .T. ) ;
#16780 = ORIENTED_EDGE ( 'NONE', *, *, #52387, .T. ) ;
#16781 = AXIS2_PLACEMENT_3D ( 'NONE', #24577, #42251, #36222 ) ;
#16782 = PLANE ( 'NONE',  #33602 ) ;
#16783 = DIRECTION ( 'NONE',  ( -0.000000000000000000, -0.000000000000000000, -1.000000000000000000 ) ) ;
#16784 = DIRECTION ( 'NONE',  ( -1.000000000000000000, -0.000000000000000000, 0.000000000000000000 ) ) ;
#16785 = DIRECTION ( 'NONE',  ( 0.000000000000000000, 0.000000000000000000, 1.000000000000000000 ) ) ;
#16786 = CARTESIAN_POINT ( 'NONE',  ( -94.99999999999997158, -207.3369185715606307, 82.65781250086715204 ) ) ;
#16787 = ORIENTED_EDGE ( 'NONE', *, *, #63613, .F. ) ;
#16788 = CARTESIAN_POINT ( 'NONE',  ( -95.00000000000002842, 87.33691857156074434, 87.26156250086714294 ) ) ;
#16789 = ORIENTED_EDGE ( 'NONE', *, *, #25986, .T. ) ;
#16790 = AXIS2_PLACEMENT_3D ( 'NONE', #725, #59679, #30714 ) ;
#16791 = CARTESIAN_POINT ( 'NONE',  ( -93.67499999999998295, -212.2949673200287179, 77.59104166840097605 ) ) ;
#16792 = CIRCLE ( 'NONE', #33564, 31.99999999999998934 ) ;
#16793 = DIRECTION ( 'NONE',  ( -1.000000000000000000, -0.000000000000000000, 0.000000000000000000 ) ) ;
#16794 = CARTESIAN_POINT ( 'NONE',  ( 11.99999999999999822, 59.46389618801966037, 49.70050353004911159 ) ) ;
#16795 = CARTESIAN_POINT ( 'NONE',  ( 97.30629616937498838, 91.33154071421968467, 75.40822916753381833 ) ) ;
#16796 = CARTESIAN_POINT ( 'NONE',  ( 12.00000000000000000, 6.762365576493649222, 25.66652317338391853 ) ) ;
#16797 = CARTESIAN_POINT ( 'NONE',  ( -2.499999999999997780, 8.494897427831771708, -10.00000000000000178 ) ) ;
#16798 = CARTESIAN_POINT ( 'NONE',  ( -92.35000000000000853, -208.4700217866474929, 78.94041666666664980 ) ) ;
#16799 = FACE_OUTER_BOUND ( 'NONE', #17858, .T. ) ;
#16800 = VECTOR ( 'NONE', #32607, 1000.000000000000000 ) ;
#16801 = DIRECTION ( 'NONE',  ( -0.000000000000000000, -0.000000000000000000, 1.000000000000000000 ) ) ;
#16802 = CARTESIAN_POINT ( 'NONE',  ( -23.50044424985255276, 0.001194404164626844313, -64.00000000000000000 ) ) ;
#16803 = LINE ( 'NONE', #54517, #67005 ) ;
#16804 = CARTESIAN_POINT ( 'NONE',  ( -94.99999999999997158, -207.3369185715606307, 89.00781250086716057 ) ) ;
#16805 = CYLINDRICAL_SURFACE ( 'NONE', #40998, 31.99999999999998579 ) ;
#16806 = VERTEX_POINT ( 'NONE', #43573 ) ;
#16807 = CARTESIAN_POINT ( 'NONE',  ( 10.00000000000000000, -73.72996012237429397, -14.67089635893794508 ) ) ;
#16808 = CARTESIAN_POINT ( 'NONE',  ( -92.69370383062505425, 88.66845928578038638, 80.38239583420049428 ) ) ;
#16809 = EDGE_CURVE ( 'NONE', #21165, #63343, #60845, .T. ) ;
#16810 = EDGE_CURVE ( 'NONE', #37277, #72197, #34868, .T. ) ;
#16811 = DIRECTION ( 'NONE',  ( -1.000000000000000000, -0.000000000000000000, 0.000000000000000000 ) ) ;
#16812 = ORIENTED_EDGE ( 'NONE', *, *, #63180, .F. ) ;
#16813 = ADVANCED_FACE ( 'NONE', ( #28105 ), #45422, .T. ) ;
#16815 = FACE_OUTER_BOUND ( 'NONE', #21738, .T. ) ;
#16814 = CIRCLE ( 'NONE', #15450, 42.00000000000000000 ) ;
#16816 = CARTESIAN_POINT ( 'NONE',  ( 97.64999999999449187, -210.0000054026048701, 81.50687481489494246 ) ) ;
#16817 = FACE_OUTER_BOUND ( 'NONE', #27658, .T. ) ;
#16818 = CIRCLE ( 'NONE', #58844, 32.00000000000000000 ) ;
#16819 = DIRECTION ( 'NONE',  ( -1.000000000000000000, -0.000000000000000000, 0.000000000000000000 ) ) ;
#16820 = CARTESIAN_POINT ( 'NONE',  ( 96.66077099052525057, -211.6002630214759961, 74.80065534806806227 ) ) ;
#16821 = VECTOR ( 'NONE', #2674, 1000.000000000000000 ) ;
#16822 = VERTEX_POINT ( 'NONE', #73221 ) ;
#16823 = ORIENTED_EDGE ( 'NONE', *, *, #68445, .F. ) ;
#16824 = EDGE_CURVE ( 'NONE', #71862, #42798, #43717, .T. ) ;
#16825 = ADVANCED_FACE ( 'NONE', ( #27740 ), #57430, .T. ) ;
#16826 = FACE_OUTER_BOUND ( 'NONE', #45131, .T. ) ;
#16827 = DIRECTION ( 'NONE',  ( 0.000000000000000000, 0.000000000000000000, 1.000000000000000000 ) ) ;
#16828 = LINE ( 'NONE', #73578, #37697 ) ;
#16829 = LINE ( 'NONE', #9699, #57891 ) ;
#16830 = CARTESIAN_POINT ( 'NONE',  ( 5.000000000000000000, 59.75363087400076267, 56.15606465354979804 ) ) ;
#16831 = CARTESIAN_POINT ( 'NONE',  ( 95.00000000000000000, -206.9400435732949575, 86.66624999999999091 ) ) ;
#16832 = AXIS2_PLACEMENT_3D ( 'NONE', #27492, #50426, #44803 ) ;
#16833 = VERTEX_POINT ( 'NONE', #22479 ) ;
#16834 = ORIENTED_EDGE ( 'NONE', *, *, #36313, .F. ) ;
#16835 = CARTESIAN_POINT ( 'NONE',  ( -3.000000000000000000, 18.84667830672605859, -18.68964196561243796 ) ) ;
#16836 = ORIENTED_EDGE ( 'NONE', *, *, #71758, .T. ) ;
#16837 = AXIS2_PLACEMENT_3D ( 'NONE', #35287, #52947, #29623 ) ;
#16838 = ORIENTED_EDGE ( 'NONE', *, *, #26802, .T. ) ;
#16839 = DIRECTION ( 'NONE',  ( -1.000000000000000000, -0.000000000000000000, 0.000000000000000000 ) ) ;
#16840 = AXIS2_PLACEMENT_3D ( 'NONE', #17400, #40333, #29045 ) ;
#16841 = EDGE_CURVE ( 'NONE', #16652, #64804, #4119, .T. ) ;
#16842 = EDGE_CURVE ( 'NONE', #26720, #852, #63756, .T. ) ;
#16843 = CIRCLE ( 'NONE', #39656, 77.49899999999999523 ) ;
#16844 = CARTESIAN_POINT ( 'NONE',  ( 3.346878500200757944, 3.841181488860379911, -5.948595712916174172 ) ) ;
#16845 = CIRCLE ( 'NONE', #56461, 31.99999999999998934 ) ;
#16846 = ORIENTED_EDGE ( 'NONE', *, *, #9097, .T. ) ;
#16847 = DIRECTION ( 'NONE',  ( 0.000000000000000000, 0.000000000000000000, 1.000000000000000000 ) ) ;
#16848 = CARTESIAN_POINT ( 'NONE',  ( 95.00000000000000000, -206.9400435732949575, 77.85562500173429612 ) ) ;
#16850 = CIRCLE ( 'NONE', #46855, 31.99999999999999289 ) ;
#16849 = CARTESIAN_POINT ( 'NONE',  ( 96.32499999999998863, 87.70503267997126784, 81.32166666666667254 ) ) ;
#16851 = VERTEX_POINT ( 'NONE', #58072 ) ;
#16852 = CARTESIAN_POINT ( 'NONE',  ( 10.00000000000000000, 36.88895765772633695, 6.736453364083687667 ) ) ;
#16853 = VERTEX_POINT ( 'NONE', #4839 ) ;
#16854 = LINE ( 'NONE', #4849, #54250 ) ;
#16855 = ORIENTED_EDGE ( 'NONE', *, *, #48056, .T. ) ;
#16856 = CARTESIAN_POINT ( 'NONE',  ( -93.67500000000003979, 92.29496732002878900, 89.23270833506762756 ) ) ;
#16857 = CARTESIAN_POINT ( 'NONE',  ( -95.00000000000002842, 87.33691857156074434, 81.70531250086715147 ) ) ;
#16858 = CARTESIAN_POINT ( 'NONE',  ( 93.84685191531248449, 88.00268892867053694, 77.04864583420047097 ) ) ;
#16859 = VERTEX_POINT ( 'NONE', #11923 ) ;
#16860 = DIRECTION ( 'NONE',  ( 1.000000000000000000, 0.000000000000000000, 0.000000000000000000 ) ) ;
#16861 = DIRECTION ( 'NONE',  ( 0.000000000000000000, 0.000000000000000000, 1.000000000000000000 ) ) ;
#16862 = CARTESIAN_POINT ( 'NONE',  ( 0.000000000000000000, -40.98264845739743123, -9.188173127307734944 ) ) ;
#16863 = CARTESIAN_POINT ( 'NONE',  ( 2.369999999999999662, 0.000000000000000000, 0.000000000000000000 ) ) ;
#16864 = VERTEX_POINT ( 'NONE', #27354 ) ;
#16865 = CARTESIAN_POINT ( 'NONE',  ( 0.000000000000000000, 0.000000000000000000, 40.00000000000000000 ) ) ;
#16866 = CARTESIAN_POINT ( 'NONE',  ( -94.99999999999997158, -207.3369185715606307, 76.78406250086712248 ) ) ;
#16867 = VERTEX_POINT ( 'NONE', #73592 ) ;
#16868 = ORIENTED_EDGE ( 'NONE', *, *, #16105, .T. ) ;
#16869 = CARTESIAN_POINT ( 'NONE',  ( 0.000000000000000000, -55.16347631943085617, 60.67117009219117563 ) ) ;
#16870 = VERTEX_POINT ( 'NONE', #67596 ) ;
#16871 = CARTESIAN_POINT ( 'NONE',  ( -95.00000000000002842, 90.00000000000004263, 90.00000000000000000 ) ) ;
#16872 = CARTESIAN_POINT ( 'NONE',  ( 10.00000000000000000, 0.000000000000000000, 0.000000000000000000 ) ) ;
#16873 = ORIENTED_EDGE ( 'NONE', *, *, #40493, .T. ) ;
#16874 = CARTESIAN_POINT ( 'NONE',  ( -96.15314808468745866, -211.9973110713294489, 77.04864583420047097 ) ) ;
#16875 = ORIENTED_EDGE ( 'NONE', *, *, #19496, .F. ) ;
#16876 = DIRECTION ( 'NONE',  ( 1.000000000000000000, -0.000000000000000000, -0.000000000000000000 ) ) ;
#16877 = LINE ( 'NONE', #39810, #6823 ) ;
#16878 = DIRECTION ( 'NONE',  ( -1.000000000000000000, 0.000000000000000000, 0.000000000000000000 ) ) ;
#16879 = DIRECTION ( 'NONE',  ( -1.000000000000000000, 0.000000000000000000, 0.000000000000000000 ) ) ;
#16880 = CIRCLE ( 'NONE', #22899, 31.99999999999998934 ) ;
#16881 = CARTESIAN_POINT ( 'NONE',  ( 5.000000000000000000, -21.60688246758642705, 79.10210256391360417 ) ) ;
#16882 = CIRCLE ( 'NONE', #26471, 82.00000000000000000 ) ;
#16883 = CARTESIAN_POINT ( 'NONE',  ( 10.00000000000000000, 0.000000000000000000, 0.000000000000000000 ) ) ;
#16885 = CARTESIAN_POINT ( 'NONE',  ( 94.99999999999998579, 92.66308142843932671, 85.03906250086714635 ) ) ;
#16884 = AXIS2_PLACEMENT_3D ( 'NONE', #41095, #56251, #28035 ) ;
#16886 = LINE ( 'NONE', #27785, #16020 ) ;
#16887 = CARTESIAN_POINT ( 'NONE',  ( -92.34999999999999432, -209.9999999999999716, 90.00000000000000000 ) ) ;
#16888 = DIRECTION ( 'NONE',  ( -1.000000000000000000, -0.000000000000000000, -0.000000000000000000 ) ) ;
#16889 = CARTESIAN_POINT ( 'NONE',  ( -22.67106064244952535, -113.6342314410295842, -2.500000000000000000 ) ) ;
#16890 = CARTESIAN_POINT ( 'NONE',  ( 6.000000000000000000, -78.73519480814938731, -22.90783923731713045 ) ) ;
#16891 = CARTESIAN_POINT ( 'NONE',  ( 5.000000000000002665, -16.65972982744991882, 80.28980883073752750 ) ) ;
#16892 = EDGE_CURVE ( 'NONE', #69905, #5770, #50289, .T. ) ;
#16893 = LINE ( 'NONE', #28522, #51215 ) ;
#16894 = DIRECTION ( 'NONE',  ( -1.000000000000000000, -0.000000000000000000, -0.000000000000000000 ) ) ;
#16895 = ADVANCED_FACE ( 'NONE', ( #61963 ), #10444, .T. ) ;
#16896 = MECHANICAL_DESIGN_GEOMETRIC_PRESENTATION_REPRESENTATION (  '', ( #55299 ), #52949 ) ;
#16897 = CARTESIAN_POINT ( 'NONE',  ( -92.35000000000003695, 90.00000000000004263, 90.00000000000000000 ) ) ;
#16898 = DIRECTION ( 'NONE',  ( -1.000000000000000000, -0.000000000000000000, -0.000000000000000000 ) ) ;
#16899 = CIRCLE ( 'NONE', #56503, 42.00000000000000000 ) ;
#16900 = FACE_OUTER_BOUND ( 'NONE', #71378, .T. ) ;
#16901 = AXIS2_PLACEMENT_3D ( 'NONE', #53740, #47730, #25908 ) ;
#16902 = ADVANCED_FACE ( 'NONE', ( #33363 ), #28855, .T. ) ;
#16903 = CARTESIAN_POINT ( 'NONE',  ( -92.34999999999999432, -209.9999999999999716, 83.33250000000001023 ) ) ;
#16904 = CIRCLE ( 'NONE', #144, 16.00000000000000000 ) ;
#16905 = ADVANCED_FACE ( 'NONE', ( #68722 ), #17207, .T. ) ;
#16906 = CARTESIAN_POINT ( 'NONE',  ( -92.35000000018064270, -210.0000309433161476, 78.33187387208045038 ) ) ;
#16907 = EDGE_LOOP ( 'NONE', ( #34482, #63340, #24438, #50549 ) ) ;
#16908 = ADVANCED_FACE ( 'NONE', ( #44679 ), #46153, .F. ) ;
#16909 = DIRECTION ( 'NONE',  ( 0.000000000000000000, -0.8090169943749426773, 0.5877852522924797984 ) ) ;
#16910 = CARTESIAN_POINT ( 'NONE',  ( -6.719258119307965238, -15.35072898742050107, 0.000000000000000000 ) ) ;
#16911 = CARTESIAN_POINT ( 'NONE',  ( 12.50000000000000000, -107.5000000000000000, 40.00000000000000000 ) ) ;
#16912 = CARTESIAN_POINT ( 'NONE',  ( 97.30629616937498838, -209.9999999999999716, 84.40406250086715545 ) ) ;
#16913 = EDGE_LOOP ( 'NONE', ( #42908, #47864, #49159, #8552 ) ) ;
#16914 = ORIENTED_EDGE ( 'NONE', *, *, #25456, .T. ) ;
#16915 = ADVANCED_FACE ( 'NONE', ( #62345 ), #32890, .T. ) ;
#16916 = EDGE_CURVE ( 'NONE', #2716, #36430, #71320, .T. ) ;
#16917 = DIRECTION ( 'NONE',  ( 0.000000000000000000, -0.8090169943749402348, -0.5877852522924830181 ) ) ;
#16918 = VERTEX_POINT ( 'NONE', #30686 ) ;
#16919 = LINE ( 'NONE', #5653, #26958 ) ;
#16920 = CARTESIAN_POINT ( 'NONE',  ( 97.30629616937498838, -208.6684592857803295, 79.21822916753380639 ) ) ;
#16921 = EDGE_LOOP ( 'NONE', ( #24076, #1798, #63244, #30429 ) ) ;
#16922 = CARTESIAN_POINT ( 'NONE',  ( 92.69370383062501162, -209.9999999999999716, 82.18156250086715886 ) ) ;
#16923 = AXIS2_PLACEMENT_3D ( 'NONE', #3682, #71692, #26944 ) ;
#16924 = VECTOR ( 'NONE', #29878, 1000.000000000000000 ) ;
#16925 = ORIENTED_EDGE ( 'NONE', *, *, #4199, .T. ) ;
#16926 = CARTESIAN_POINT ( 'NONE',  ( 97.65000000000000568, 91.52997821335252127, 80.28979166840095161 ) ) ;
#16927 = VERTEX_POINT ( 'NONE', #23961 ) ;
#16928 = AXIS2_PLACEMENT_3D ( 'NONE', #31745, #8083, #59980 ) ;
#16929 = VERTEX_POINT ( 'NONE', #70530 ) ;
#16930 = CARTESIAN_POINT ( 'NONE',  ( -96.15314808468752972, 91.99731107132950569, 75.09072916753380866 ) ) ;
#16931 = CARTESIAN_POINT ( 'NONE',  ( 92.34999999999999432, 90.00000000000002842, 90.00000000000000000 ) ) ;
#16932 = ORIENTED_EDGE ( 'NONE', *, *, #53043, .F. ) ;
#16933 = CARTESIAN_POINT ( 'NONE',  ( 97.64999999999690772, -210.0000040461968638, 77.06187486178042434 ) ) ;
#16934 = CARTESIAN_POINT ( 'NONE',  ( 93.67500000000001137, -212.2949673200287179, 88.28020833506764120 ) ) ;
#16935 = ORIENTED_EDGE ( 'NONE', *, *, #31388, .F. ) ;
#16936 = DIRECTION ( 'NONE',  ( 1.000000000000000000, 0.000000000000000000, 0.000000000000000000 ) ) ;
#16937 = EDGE_LOOP ( 'NONE', ( #53996, #66981, #72927, #64723 ) ) ;
#16938 = DIRECTION ( 'NONE',  ( 0.000000000000000000, -0.1045284632676449221, 0.9945218953682741780 ) ) ;
#16939 = EDGE_LOOP ( 'NONE', ( #54384, #48173, #46378, #22807 ) ) ;
#16940 = AXIS2_PLACEMENT_3D ( 'NONE', #32666, #67268, #21016 ) ;
#16941 = EDGE_LOOP ( 'NONE', ( #60123, #50855, #27226, #30536 ) ) ;
#16942 = ORIENTED_EDGE ( 'NONE', *, *, #26124, .F. ) ;
#16943 = DIRECTION ( 'NONE',  ( 0.000000000000000000, 0.4539904997395412534, 0.8910065241883706744 ) ) ;
#16944 = FACE_OUTER_BOUND ( 'NONE', #12697, .T. ) ;
#16945 = ORIENTED_EDGE ( 'NONE', *, *, #47875, .T. ) ;
#16946 = VECTOR ( 'NONE', #360, 1000.000000000000000 ) ;
#16947 = EDGE_LOOP ( 'NONE', ( #9249, #60396, #19798, #58328 ) ) ;
#16948 = ORIENTED_EDGE ( 'NONE', *, *, #38685, .T. ) ;
#16949 = CARTESIAN_POINT ( 'NONE',  ( 10.00000000000000000, -33.80338159004273280, -16.23288003029533044 ) ) ;
#16950 = VECTOR ( 'NONE', #36382, 1000.000000000000000 ) ;
#16951 = CARTESIAN_POINT ( 'NONE',  ( 11.99999999999999822, 41.76106447765489094, 62.50884508063442269 ) ) ;
#16952 = CARTESIAN_POINT ( 'NONE',  ( -96.15314808468751551, 88.00268892867056536, 75.30239583420048177 ) ) ;
#16953 = ORIENTED_EDGE ( 'NONE', *, *, #55622, .F. ) ;
#16954 = CARTESIAN_POINT ( 'NONE',  ( 92.69370383062498320, 90.00000000000002842, 89.64281250086713726 ) ) ;
#16955 =( BOUNDED_CURVE ( )  B_SPLINE_CURVE ( 2, ( #9929, #32851, #21575, #39627, #9190, #15196, #73818 ),
 .UNSPECIFIED., .F., .F. ) 
 B_SPLINE_CURVE_WITH_KNOTS ( ( 3, 2, 2, 3 ),
 ( 0.1270039290051391268, 0.1340595452767650020, 0.1411153108176473603, 0.1481709449575277227 ),
 .UNSPECIFIED. ) 
 CURVE ( )  GEOMETRIC_REPRESENTATION_ITEM ( )  RATIONAL_B_SPLINE_CURVE ( ( 0.9999943314824810692, 0.8660282381031599863, 1.000000000000000000, 0.8660254037844387076, 1.000000000000000000, 0.8660278988214527018, 0.9999950100189032298 ) ) 
 REPRESENTATION_ITEM ( '' )  );
#16956 = ORIENTED_EDGE ( 'NONE', *, *, #56209, .T. ) ;
#16957 = CARTESIAN_POINT ( 'NONE',  ( 12.00000000000000000, 8.688484142254226938, 21.88630264137359305 ) ) ;
#16958 = CARTESIAN_POINT ( 'NONE',  ( -97.30629616937497417, -211.3315407142195852, 85.25072916753379104 ) ) ;
#16959 = EDGE_LOOP ( 'NONE', ( #67605, #67320, #25173, #29223 ) ) ;
#16960 = CARTESIAN_POINT ( 'NONE',  ( 11.99999999999999822, -46.11716303203233736, 67.80270845531873647 ) ) ;
#16961 = CARTESIAN_POINT ( 'NONE',  ( 94.37155072198216033, -212.5563123626347419, 74.98613922222766348 ) ) ;
#16962 = FACE_OUTER_BOUND ( 'NONE', #42623, .T. ) ;
#16963 = CARTESIAN_POINT ( 'NONE',  ( -93.51319757292672818, -208.1953243530631994, 74.81083481226637844 ) ) ;
#16964 = EDGE_CURVE ( 'NONE', #45506, #62606, #2954, .T. ) ;
#16965 = CARTESIAN_POINT ( 'NONE',  ( 15.00000000000000000, -20.55727247249726020, 16.78983467731313084 ) ) ;
#16966 = DIRECTION ( 'NONE',  ( 0.000000000000000000, 0.000000000000000000, 1.000000000000000000 ) ) ;
#16967 = CYLINDRICAL_SURFACE ( 'NONE', #7342, 37.49900000000000233 ) ;
#16968 = EDGE_CURVE ( 'NONE', #70509, #68784, #53633, .T. ) ;
#16969 = CARTESIAN_POINT ( 'NONE',  ( 92.34999999999999432, 90.00000000000002842, 90.00000000000000000 ) ) ;
#16970 = EDGE_CURVE ( 'NONE', #30770, #73126, #47262, .T. ) ;
#16971 = CARTESIAN_POINT ( 'NONE',  ( 11.99999999999999822, -23.16143007188479430, 73.95703589263968070 ) ) ;
#16972 = CARTESIAN_POINT ( 'NONE',  ( -92.69370383062504004, 90.00000000000004263, 81.07031250086714635 ) ) ;
#16973 = CARTESIAN_POINT ( 'NONE',  ( -12.75044424985254921, 0.001194404164626844313, -85.60000000000000853 ) ) ;
#16974 = CARTESIAN_POINT ( 'NONE',  ( 3.000000000000000000, -1.467624384280027838, 2.542000000000001592 ) ) ;
#16975 = EDGE_LOOP ( 'NONE', ( #8907, #34198, #1690, #48747 ) ) ;
#16976 = DIRECTION ( 'NONE',  ( -1.000000000000000000, -0.000000000000000000, -0.000000000000000000 ) ) ;
#16977 = ADVANCED_FACE ( 'NONE', ( #19041 ), #6664, .T. ) ;
#16978 = COLOUR_RGB ( '', 0.09019608, 0.27058824, 0.51372549) ;
#16979 = AXIS2_PLACEMENT_3D ( 'NONE', #60243, #30894, #53839 ) ;
#16980 = CIRCLE ( 'NONE', #52981, 31.99999999999999645 ) ;
#16981 = DIRECTION ( 'NONE',  ( -1.000000000000000000, -0.000000000000000000, -0.000000000000000000 ) ) ;
#16982 = CARTESIAN_POINT ( 'NONE',  ( 96.32499999999998863, -212.2949673200287179, 86.48104166840096241 ) ) ;
#16983 = CARTESIAN_POINT ( 'NONE',  ( 0.000000000000000000, -20.40083707022935400, 72.35432306680478121 ) ) ;
#16984 = CARTESIAN_POINT ( 'NONE',  ( 0.000000000000000000, -33.17418723428294669, -17.67226234102862747 ) ) ;
#16985 = CARTESIAN_POINT ( 'NONE',  ( -93.67500000000003979, 92.29496732002878900, 87.32770833506762642 ) ) ;
#16986 = CARTESIAN_POINT ( 'NONE',  ( -92.69370383062498320, -209.9999999999999716, 79.32406250086715715 ) ) ;
#16987 = AXIS2_PLACEMENT_3D ( 'NONE', #16772, #57000, #44227 ) ;
#16988 = DIRECTION ( 'NONE',  ( 0.000000000000000000, 0.000000000000000000, 1.000000000000000000 ) ) ;
#16989 = ORIENTED_EDGE ( 'NONE', *, *, #11193, .F. ) ;
#16990 = EDGE_CURVE ( 'NONE', #32331, #67112, #32954, .T. ) ;
#16991 = CARTESIAN_POINT ( 'NONE',  ( 0.000000000000000000, -16.65560815589439159, 38.55633173627004595 ) ) ;
#16992 = CARTESIAN_POINT ( 'NONE',  ( 0.000000000000000000, -27.13269053701078448, -25.88420570971428702 ) ) ;
#16993 = CARTESIAN_POINT ( 'NONE',  ( 10.00000000000000000, 34.44570377933695227, -69.42325613327405165 ) ) ;
#16994 = DIRECTION ( 'NONE',  ( -1.000000000000000000, 0.000000000000000000, 0.000000000000000000 ) ) ;
#16995 = DIRECTION ( 'NONE',  ( -1.000000000000000000, -0.000000000000000000, 0.000000000000000000 ) ) ;
#16996 = AXIS2_PLACEMENT_3D ( 'NONE', #39245, #33965, #9918 ) ;
#16997 = CIRCLE ( 'NONE', #37411, 16.00000000000000000 ) ;
#16998 = CARTESIAN_POINT ( 'NONE',  ( 0.000000000000000000, -36.13751322684434797, 21.40280677340357940 ) ) ;
#16999 = ORIENTED_EDGE ( 'NONE', *, *, #48698, .F. ) ;
#17000 = EDGE_CURVE ( 'NONE', #33943, #11010, #591, .T. ) ;
#17001 = CARTESIAN_POINT ( 'NONE',  ( 1.560000000000000053, 0.000000000000000000, 2.999999999999998668 ) ) ;
#17002 = ADVANCED_FACE ( 'NONE', ( #41250 ), #7772, .T. ) ;
#17003 = DIRECTION ( 'NONE',  ( -1.000000000000000000, -0.000000000000000000, 0.000000000000000000 ) ) ;
#17004 = ORIENTED_EDGE ( 'NONE', *, *, #1936, .F. ) ;
#17005 = CARTESIAN_POINT ( 'NONE',  ( 96.15314808468750130, -211.9973110713294489, 88.58447916753381435 ) ) ;
#17006 = DIRECTION ( 'NONE',  ( -1.000000000000000000, 0.000000000000000000, 0.000000000000000000 ) ) ;
#17007 = EDGE_CURVE ( 'NONE', #65693, #57864, #1779, .T. ) ;
#17008 = ORIENTED_EDGE ( 'NONE', *, *, #41400, .T. ) ;
#17009 = DIRECTION ( 'NONE',  ( -1.000000000000000000, 0.000000000000000000, 0.000000000000000000 ) ) ;
#17010 = ORIENTED_EDGE ( 'NONE', *, *, #53208, .F. ) ;
#17011 = CARTESIAN_POINT ( 'NONE',  ( 10.00000000000000000, -4.992566952384716927, -37.16516213103282951 ) ) ;
#17012 = ORIENTED_EDGE ( 'NONE', *, *, #35721, .F. ) ;
#17013 = CARTESIAN_POINT ( 'NONE',  ( 0.000000000000000000, -11.30684508768393570, 76.66974797899831628 ) ) ;
#17014 = ORIENTED_EDGE ( 'NONE', *, *, #31129, .T. ) ;
#17015 = LINE ( 'NONE', #55473, #54935 ) ;
#17016 = ORIENTED_EDGE ( 'NONE', *, *, #46689, .T. ) ;
#17017 = ORIENTED_EDGE ( 'NONE', *, *, #3824, .T. ) ;
#17018 = CARTESIAN_POINT ( 'NONE',  ( -0.0004442498525516064278, 0.001194404164626844313, -64.00000000000000000 ) ) ;
#17019 = VERTEX_POINT ( 'NONE', #2173 ) ;
#17020 = ORIENTED_EDGE ( 'NONE', *, *, #18098, .F. ) ;
#17021 = FACE_OUTER_BOUND ( 'NONE', #44893, .T. ) ;
#17022 = CARTESIAN_POINT ( 'NONE',  ( -8.637688417678548447, 13.69818742750669749, -55.00000000000000000 ) ) ;
#17023 = VERTEX_POINT ( 'NONE', #52149 ) ;
#17024 = AXIS2_PLACEMENT_3D ( 'NONE', #49215, #49950, #72143 ) ;
#17025 = ORIENTED_EDGE ( 'NONE', *, *, #72948, .T. ) ;
#17026 = CARTESIAN_POINT ( 'NONE',  ( 96.15314808468748708, 88.00268892867053694, 83.50447916753381605 ) ) ;
#17027 = ORIENTED_EDGE ( 'NONE', *, *, #47806, .T. ) ;
#17028 = CARTESIAN_POINT ( 'NONE',  ( 93.84685191531249870, -208.0026889286704943, 84.45697916753380241 ) ) ;
#17029 = PRODUCT_CONTEXT ( 'NONE', #41173, 'mechanical' ) ;
#17030 = LINE ( 'NONE', #74161, #28187 ) ;
#17032 = CARTESIAN_POINT ( 'NONE',  ( -93.67500000000003979, 87.70503267997129626, 84.49666666666666970 ) ) ;
#17031 = AXIS2_PLACEMENT_3D ( 'NONE', #57573, #45928, #6082 ) ;
#17033 = DIRECTION ( 'NONE',  ( 0.000000000000000000, 0.3826834323650841752, 0.9238795325112891810 ) ) ;
#17034 = CARTESIAN_POINT ( 'NONE',  ( 0.000000000000000000, 59.75363087400076267, 56.15606465354979804 ) ) ;
#17035 = CARTESIAN_POINT ( 'NONE',  ( 0.000000000000000000, -59.03961581697367933, -46.53671651294010303 ) ) ;
#17036 = CARTESIAN_POINT ( 'NONE',  ( 0.000000000000000000, 0.000000000000000000, 0.000000000000000000 ) ) ;
#17037 = CARTESIAN_POINT ( 'NONE',  ( -94.99999999999997158, -207.3369185715606307, 88.84906250086713442 ) ) ;
#17038 = CARTESIAN_POINT ( 'NONE',  ( -96.15314808468752972, 91.99731107132950569, 87.15572916753382060 ) ) ;
#17039 = VECTOR ( 'NONE', #5045, 1000.000000000000114 ) ;
#17040 = EDGE_LOOP ( 'NONE', ( #21455, #73760, #73903, #34375 ) ) ;
#17042 = CARTESIAN_POINT ( 'NONE',  ( -92.69370383062504004, 90.00000000000004263, 86.15031250086714465 ) ) ;
#17041 = CARTESIAN_POINT ( 'NONE',  ( 93.84685191531248449, 88.00268892867053694, 85.93864583420048575 ) ) ;
#17043 = CIRCLE ( 'NONE', #59225, 82.00000000000000000 ) ;
#17044 = ORIENTED_EDGE ( 'NONE', *, *, #27848, .T. ) ;
#17045 = CARTESIAN_POINT ( 'NONE',  ( -96.32500000000001705, 92.29496732002878900, 87.98916666666666231 ) ) ;
#17046 = CARTESIAN_POINT ( 'NONE',  ( 92.35000000000000853, -211.5299782133524218, 76.16229166840095388 ) ) ;
#17047 = CARTESIAN_POINT ( 'NONE',  ( 11.59999999999999787, 1.420590287010929336E-15, 53.20000000000001705 ) ) ;
#17048 = LINE ( 'NONE', #12506, #5631 ) ;
#17049 = CARTESIAN_POINT ( 'NONE',  ( -96.15314808468747287, -208.0026889286704943, 85.09197916753380753 ) ) ;
#17050 = LINE ( 'NONE', #4674, #49879 ) ;
#17051 = EDGE_CURVE ( 'NONE', #28480, #39686, #17351, .T. ) ;
#17052 = CARTESIAN_POINT ( 'NONE',  ( -99.99999999999998579, -116.0000000000000000, 39.99999999999996447 ) ) ;
#17053 = DIRECTION ( 'NONE',  ( 0.000000000000000000, 0.000000000000000000, 1.000000000000000000 ) ) ;
#17054 = VECTOR ( 'NONE', #27485, 1000.000000000000000 ) ;
#17055 = FACE_OUTER_BOUND ( 'NONE', #6423, .T. ) ;
#17056 = ORIENTED_EDGE ( 'NONE', *, *, #25152, .F. ) ;
#17057 = CIRCLE ( 'NONE', #37503, 82.00000000000000000 ) ;
#17058 = ORIENTED_EDGE ( 'NONE', *, *, #14883, .T. ) ;
#17059 = VECTOR ( 'NONE', #39277, 1000.000000000000000 ) ;
#17060 = EDGE_CURVE ( 'NONE', #40680, #5770, #62995, .T. ) ;
#17061 = CARTESIAN_POINT ( 'NONE',  ( -95.00000000000002842, 86.94004357329504273, 77.45874999999999488 ) ) ;
#17062 = ADVANCED_FACE ( 'NONE', ( #48001 ), #23582, .T. ) ;
#17063 = DIRECTION ( 'NONE',  ( 0.000000000000000000, 0.000000000000000000, 1.000000000000000000 ) ) ;
#17064 = CARTESIAN_POINT ( 'NONE',  ( 0.000000000000000000, 63.18004540533027580, 44.88180994100400056 ) ) ;
#17065 = CARTESIAN_POINT ( 'NONE',  ( -97.64999999960622290, -209.9999706925929672, 76.74344264316562203 ) ) ;
#17066 = DIRECTION ( 'NONE',  ( -1.000000000000000000, -0.000000000000000000, -0.000000000000000000 ) ) ;
#17067 = CARTESIAN_POINT ( 'NONE',  ( 0.5480546763151027401, -96.50639159107802811, 2.500000000000000000 ) ) ;
#17068 = CARTESIAN_POINT ( 'NONE',  ( -97.64999999999992042, -208.4700217866474929, 79.78708333333331382 ) ) ;
#17069 = ORIENTED_EDGE ( 'NONE', *, *, #36059, .T. ) ;
#17070 = CARTESIAN_POINT ( 'NONE',  ( -96.15314808468752972, 91.99731107132950569, 80.01197916753380923 ) ) ;
#17071 = EDGE_CURVE ( 'NONE', #30533, #15341, #65391, .T. ) ;
#17072 = FACE_OUTER_BOUND ( 'NONE', #1082, .T. ) ;
#17073 = CARTESIAN_POINT ( 'NONE',  ( 11.99999999999999822, 73.73191006444572793, -14.66109333815486515 ) ) ;
#17074 = CARTESIAN_POINT ( 'NONE',  ( 11.99999999999999822, 70.52718814184260054, 26.02418014898334420 ) ) ;
#17075 = FACE_OUTER_BOUND ( 'NONE', #66317, .T. ) ;
#17076 = CARTESIAN_POINT ( 'NONE',  ( -95.00000000000002842, 86.94004357329504273, 75.63312500173429953 ) ) ;
#17077 = CARTESIAN_POINT ( 'NONE',  ( -92.69370383062498320, -208.6684592857803011, 89.53697916753382913 ) ) ;
#17078 =( LENGTH_UNIT ( ) NAMED_UNIT ( * ) SI_UNIT ( .MILLI., .METRE. ) );
#17079 = ADVANCED_FACE ( 'NONE', ( #35965 ), #58166, .T. ) ;
#17080 = EDGE_CURVE ( 'NONE', #56648, #18566, #64189, .T. ) ;
#17081 = CARTESIAN_POINT ( 'NONE',  ( 96.15314808468748708, 88.00268892867053694, 76.67822916753381435 ) ) ;
#17082 = CARTESIAN_POINT ( 'NONE',  ( -92.69370383062498320, -209.9999999999999716, 79.95906250086714806 ) ) ;
#17083 = DIRECTION ( 'NONE',  ( -1.000000000000000000, 0.000000000000000000, 0.000000000000000000 ) ) ;
#17084 = ORIENTED_EDGE ( 'NONE', *, *, #7128, .F. ) ;
#17085 = DIRECTION ( 'NONE',  ( -2.603472992746261562E-14, -2.546204323184492723E-14, 1.000000000000000000 ) ) ;
#17086 = CIRCLE ( 'NONE', #36284, 11.59999999999999787 ) ;
#17087 = CARTESIAN_POINT ( 'NONE',  ( -92.34999999999999432, -209.9999999999999716, 75.71250000000000568 ) ) ;
#17088 = CARTESIAN_POINT ( 'NONE',  ( 97.64999999999999147, -209.9999999999999716, 78.96687500173429441 ) ) ;
#17089 = CIRCLE ( 'NONE', #26674, 31.99999999999998934 ) ;
#17090 = CARTESIAN_POINT ( 'NONE',  ( -97.30629616937501680, 90.00000000000004263, 75.19656250086714522 ) ) ;
#17091 = CARTESIAN_POINT ( 'NONE',  ( 97.30629616937498838, -208.6684592857803011, 79.21822916753380639 ) ) ;
#17092 = ORIENTED_EDGE ( 'NONE', *, *, #54722, .T. ) ;
#17093 = CIRCLE ( 'NONE', #36295, 82.00000000000000000 ) ;
#17094 = EDGE_CURVE ( 'NONE', #16458, #32536, #7024, .T. ) ;
#17095 = EDGE_CURVE ( 'NONE', #42482, #14594, #72546, .T. ) ;
#17096 = CARTESIAN_POINT ( 'NONE',  ( -95.00000000000002842, 93.05995642670504253, 75.23624999999998408 ) ) ;
#17097 = ORIENTED_EDGE ( 'NONE', *, *, #30803, .F. ) ;
#17098 = AXIS2_PLACEMENT_3D ( 'NONE', #2570, #53653, #35613 ) ;
#17099 = CARTESIAN_POINT ( 'NONE',  ( 10.00000000000000000, 0.000000000000000000, 0.000000000000000000 ) ) ;
#17100 = ORIENTED_EDGE ( 'NONE', *, *, #55491, .F. ) ;
#17101 = CARTESIAN_POINT ( 'NONE',  ( 0.000000000000000000, 0.000000000000000000, 20.00000000000000000 ) ) ;
#17102 = AXIS2_PLACEMENT_3D ( 'NONE', #11318, #17333, #57934 ) ;
#17103 = ORIENTED_EDGE ( 'NONE', *, *, #42950, .T. ) ;
#17104 = ORIENTED_EDGE ( 'NONE', *, *, #68679, .T. ) ;
#17105 = VERTEX_POINT ( 'NONE', #1803 ) ;
#17106 = CARTESIAN_POINT ( 'NONE',  ( 92.69370383062501162, -208.6684592857803295, 75.77864583420048916 ) ) ;
#17107 = VERTEX_POINT ( 'NONE', #24690 ) ;
#17108 = VERTEX_POINT ( 'NONE', #59650 ) ;
#17109 = CARTESIAN_POINT ( 'NONE',  ( 96.15314808468748708, 88.00268892867053694, 81.75822916753382685 ) ) ;
#17110 = CARTESIAN_POINT ( 'NONE',  ( 97.64999999999997726, -211.5299782133524502, 78.83458333333334167 ) ) ;
#17111 = ORIENTED_EDGE ( 'NONE', *, *, #51398, .F. ) ;
#17112 = ORIENTED_EDGE ( 'NONE', *, *, #63996, .F. ) ;
#17113 = ORIENTED_EDGE ( 'NONE', *, *, #62108, .F. ) ;
#17114 = ORIENTED_EDGE ( 'NONE', *, *, #69857, .T. ) ;
#17115 = CARTESIAN_POINT ( 'NONE',  ( 0.000000000000000000, -0.8828120875898013420, -37.48860685352291711 ) ) ;
#17116 = PRESENTATION_STYLE_ASSIGNMENT (( #61874 ) ) ;
#17117 = DIRECTION ( 'NONE',  ( 0.000000000000000000, -0.9723699203976789995, 0.2334453638558956212 ) ) ;
#17118 = LINE ( 'NONE', #64465, #50663 ) ;
#17119 = DIRECTION ( 'NONE',  ( 1.000000000000000000, 0.000000000000000000, 0.000000000000000000 ) ) ;
#17120 = CARTESIAN_POINT ( 'NONE',  ( 92.35000000000000853, -209.9999999999999716, 86.90437500173429441 ) ) ;
#17121 = DIRECTION ( 'NONE',  ( -1.000000000000000000, 0.000000000000000000, 0.000000000000000000 ) ) ;
#17122 = CARTESIAN_POINT ( 'NONE',  ( 7.399999999999993250, -1.290549110169840072E-13, -13.10000000000023057 ) ) ;
#17123 = ORIENTED_EDGE ( 'NONE', *, *, #45687, .T. ) ;
#17124 = CARTESIAN_POINT ( 'NONE',  ( -97.64999999999994884, -208.4700217866474645, 83.67645833506762187 ) ) ;
#17125 = EDGE_LOOP ( 'NONE', ( #13666, #29857, #17837, #33738 ) ) ;
#17126 = FACE_OUTER_BOUND ( 'NONE', #60760, .T. ) ;
#17127 = VERTEX_POINT ( 'NONE', #31435 ) ;
#17129 = CARTESIAN_POINT ( 'NONE',  ( -95.00000000000002842, 93.05995642670501411, 79.76062500173429726 ) ) ;
#17128 = CARTESIAN_POINT ( 'NONE',  ( 97.64999999999997726, 91.52997821335252127, 77.74979166840097378 ) ) ;
#17130 = EDGE_LOOP ( 'NONE', ( #38423, #4277, #29296, #44218 ) ) ;
#17131 = CARTESIAN_POINT ( 'NONE',  ( 94.99999999999998579, 87.33691857156068750, 81.07031250086716057 ) ) ;
#17132 = CARTESIAN_POINT ( 'NONE',  ( 97.64999999999999147, 90.00000000000002842, 83.33250000000001023 ) ) ;
#17133 = DIRECTION ( 'NONE',  ( 0.000000000000000000, 0.3090169943749480064, -0.9510565162951534202 ) ) ;
#17134 = EDGE_CURVE ( 'NONE', #26057, #73333, #4002, .T. ) ;
#17135 = CARTESIAN_POINT ( 'NONE',  ( 11.99999999999999822, -30.41916302227164337, 71.27951684758015460 ) ) ;
#17136 = DIRECTION ( 'NONE',  ( -0.000000000000000000, -0.000000000000000000, 1.000000000000000000 ) ) ;
#17137 = MECHANICAL_DESIGN_GEOMETRIC_PRESENTATION_REPRESENTATION (  '', ( #63986 ), #41183 ) ;
#17138 = ORIENTED_EDGE ( 'NONE', *, *, #60798, .T. ) ;
#17139 = LINE ( 'NONE', #40072, #8770 ) ;
#17140 = DIRECTION ( 'NONE',  ( 0.000000000000000000, 0.3826834323650904479, -0.9238795325112865164 ) ) ;
#17141 = CARTESIAN_POINT ( 'NONE',  ( 0.000000000000000000, 0.000000000000000000, 0.000000000000000000 ) ) ;
#17142 = ORIENTED_EDGE ( 'NONE', *, *, #49373, .T. ) ;
#17143 = EDGE_CURVE ( 'NONE', #33107, #72660, #37395, .T. ) ;
#17144 = CIRCLE ( 'NONE', #18303, 82.00000000000000000 ) ;
#17145 = VERTEX_POINT ( 'NONE', #48728 ) ;
#17146 = EDGE_CURVE ( 'NONE', #7677, #14321, #19779, .T. ) ;
#17147 = AXIS2_PLACEMENT_3D ( 'NONE', #39163, #27116, #62098 ) ;
#17148 = CARTESIAN_POINT ( 'NONE',  ( 15.00000000000000000, -1.278221433540507546, -26.51162292216071492 ) ) ;
#17149 = LINE ( 'NONE', #34429, #10258 ) ;
#17150 = DIRECTION ( 'NONE',  ( -0.000000000000000000, -0.000000000000000000, 1.000000000000000000 ) ) ;
#17151 = AXIS2_PLACEMENT_3D ( 'NONE', #68709, #319, #39765 ) ;
#17152 = CARTESIAN_POINT ( 'NONE',  ( -93.84685191531247028, -211.9973110713294489, 80.48822916753381662 ) ) ;
#17153 = ORIENTED_EDGE ( 'NONE', *, *, #69031, .F. ) ;
#17154 = VERTEX_POINT ( 'NONE', #26159 ) ;
#17155 = ADVANCED_FACE ( 'NONE', ( #3636 ), #37834, .F. ) ;
#17156 = CARTESIAN_POINT ( 'NONE',  ( 3.000000000000000000, 1.467624384280029837, 2.541999999999997151 ) ) ;
#17157 = VECTOR ( 'NONE', #61821, 1000.000000000000000 ) ;
#17158 = DIRECTION ( 'NONE',  ( 0.000000000000000000, 0.000000000000000000, 1.000000000000000000 ) ) ;
#17159 = SURFACE_STYLE_USAGE ( .BOTH. , #45751 ) ;
#17160 = CYLINDRICAL_SURFACE ( 'NONE', #28456, 2.649999999999985700 ) ;
#17161 = PLANE ( 'NONE',  #23280 ) ;
#17162 = CARTESIAN_POINT ( 'NONE',  ( 5.000000000000000000, 35.47612816024556537, -22.48208911017461631 ) ) ;
#17163 = CARTESIAN_POINT ( 'NONE',  ( 0.000000000000000000, -33.71516098798685590, -74.74816331893465815 ) ) ;
#17164 = CARTESIAN_POINT ( 'NONE',  ( -97.64996284860670528, -208.4700003372805384, 76.69145685134844825 ) ) ;
#17165 = LINE ( 'NONE', #51003, #59250 ) ;
#17166 = FACE_OUTER_BOUND ( 'NONE', #67513, .T. ) ;
#17167 = EDGE_CURVE ( 'NONE', #48244, #29385, #9244, .T. ) ;
#17168 = EDGE_CURVE ( 'NONE', #65977, #29431, #31059, .T. ) ;
#17169 = CARTESIAN_POINT ( 'NONE',  ( 94.99999999999998579, 92.66308142843932671, 85.83281250086717762 ) ) ;
#17170 = CARTESIAN_POINT ( 'NONE',  ( -97.30629616937497417, -208.6684592857803295, 88.47864583420047779 ) ) ;
#17171 = CARTESIAN_POINT ( 'NONE',  ( -97.64999999994212487, -210.0000112241608292, 75.47473230080855444 ) ) ;
#17172 = ORIENTED_EDGE ( 'NONE', *, *, #21030, .T. ) ;
#17173 = DIRECTION ( 'NONE',  ( 0.000000000000000000, 0.2334453638559058908, -0.9723699203976765570 ) ) ;
#17174 = CARTESIAN_POINT ( 'NONE',  ( -96.15314808468752972, 91.99731107132950569, 78.10697916753380809 ) ) ;
#17175 = EDGE_CURVE ( 'NONE', #59589, #29023, #16057, .T. ) ;
#17176 = EDGE_CURVE ( 'NONE', #56792, #15793, #61483, .T. ) ;
#17177 = DIRECTION ( 'NONE',  ( -1.000000000000000000, 0.000000000000000000, 0.000000000000000000 ) ) ;
#17178 = ADVANCED_FACE ( 'NONE', ( #60037 ), #71275, .T. ) ;
#17179 = EDGE_LOOP ( 'NONE', ( #66675, #10743, #50160, #28381 ) ) ;
#17180 =( BOUNDED_SURFACE ( )  B_SPLINE_SURFACE ( 1, 2, ( 
 ( #33088, #73683, #37999, #55293, #4180, #49634, #50004, #72926, #21430, #44388, #67314, #38747, #61678, #56029, #4551, #50382, #51879, #74056, #46242, #34960, #45516, #33843, #16934, #69176, #40229, #17293, #46982, #63179, #785, #69539, #57161, #68811, #11637, #34580, #39872, #62816, #46608, #69894, #5664, #12018, #22952, #57899, #29659, #60, #11279, #45890, #52242, #28943, #10918, #51504, #22570, #57527, #6396, #58257, #6038, #419, #51132, #52608, #18389, #63913, #1161, #68441, #41336, #23314, #23672, #17664, #40602, #6753, #63544, #12382, #18036, #28559, #40977, #29298, #35328, #56788, #24058, #5298, #28200, #34213, #7496, #14229, #36793, #36421, #13852, #42817, #52990, #70623, #19868, #65746, #71733, #59739, #25159, #7124, #53351, #19137, #20236, #54105, #42448, #48447, #35677, #31152, #13498, #2636, #59368, #58619, #53718, #37184, #64637, #30041, #1891, #24778, #25885, #7857, #30772, #1529, #48085, #8223, #24409, #12751, #70252, #70997, #42083, #65019, #48815, #2261, #25516, #71362, #36058, #47707, #19500, #65385, #18759, #41697, #60125, #64277, #59003, #8607, #31520, #54458, #2991, #47347, #13121, #30406, #10076, #61228, #43206, #9329, #31891, #15338, #38660, #16092, #49555, #32629, #8969, #61967, #27743, #21726, #10447, #26249, #50667, #72480, #55943, #3724, #32255, #39029, #26622, #44682, #4463, #37918, #38283, #4843, #20984, #67599, #55203, #73595, #43936, #60488, #43576, #20622, #15725, #9711, #66853, #21339, #55574, #33365, #72113, #14604, #4093, #3356, #66129, #72839, #26987, #37556, #56326, #54831, #61592, #66494, #14976, #32999, #67227, #49188, #60848, #49922, #44297, #27357, #50293, #73225, #51408, #11926, #6310, #68352, #5577, #28472, #55648, #28108, #51045, #57807, #6666, #16848, #23229, #34123, #46155, #40888, #11196, #73968, #57070, #63452, #40141, #22106, #62728, #10832, #68724, #17573, #69443, #22863, #11553, #62349, #63824, #29572, #696, #12297, #5208, #52514, #45801, #34872, #17209, #63096, #17946, #34489, #23586, #29213, #39779, #57432, #58168, #5949, #46517, #28858, #45046, #51787, #39402, #22483, #45425, #69087, #336, #40505, #52151, #35235, #67972, #16466, #33753, #56705, #35597, #61034, #30689, #53269, #69808, #66679, #1069, #71931, #24329, #29953, #66322, #9156, #18670 ),
 ( #37743, #14796, #49378, #49001, #9531, #32079, #64552, #55017, #60676, #3547, #13408, #20446, #43401, #59282, #1444, #26448, #64191, #52903, #72309, #20808, #12665, #41252, #13030, #58920, #47265, #58531, #70533, #23964, #32452, #43760, #41613, #7027, #46900, #3182, #1806, #18309, #70168, #35968, #15162, #19043, #24692, #53636, #7410, #38101, #30325, #47624, #41997, #64933, #36337, #26073, #7774, #49737, #45620, #55393, #50858, #4283, #9896, #45238, #62539, #73032, #73414, #11376, #27172, #5025, #56136, #50102, #21538, #5396, #27930, #27556, #73783, #33944, #44113, #61785, #11016, #56890, #62920, #22296, #16279, #72661, #44499, #10269, #3912, #68159, #33562, #39593, #26812, #16656, #4654, #28292, #50491, #21166, #44867, #51230, #55766, #67037, #67414, #15912, #17028, #21922, #67789, #15540, #39223, #74159, #38477, #61416, #32814, #62153, #33191, #10640, #39964, #56521, #22674, #68544, #38845, #17756, #40703, #12116, #40325, #63272, #69991, #18860, #6134, #35423, #46340, #58352, #53088, #23410, #11734, #69270, #1263, #52337, #34308, #517, #23049, #6495, #29764, #7227, #63645, #23774, #159, #1628, #41799, #12848, #24511, #17393, #64745, #35057, #47087, #57989, #29394, #30143, #886, #35777, #18494, #29038, #46711, #70350, #69637, #58730, #18135, #57254, #41076, #64010, #12486, #6851, #52716, #64375, #45979, #24157, #34679, #68905, #47447, #5760, #41434, #28663, #51604, #57630, #51970, #26357, #59845, #9065, #54564, #1989, #37652, #70729, #60226, #8332, #7594, #66228, #48184, #71464, #24879, #71095, #31255, #25983, #19600, #42546, #13228, #30508, #54929, #20347, #48911, #31619, #25260, #19966, #65119, #14703, #60588, #31988, #47810, #65488, #13951, #3091, #54204, #71836, #2731, #3454, #65851, #43307, #25616, #30875, #19233, #53819, #42187, #43672, #49285, #36159, #20716, #48552, #13593, #36894, #14339, #72212, #59104, #42921, #8702, #53452, #36523, #37287, #59469, #7954, #2368, #73320, #22206, #27839, #72935, #28210, #16559, #56043, #32360, #50395, #50766, #21440, #10926, #49647, #16190, #73695, #56427, #39509, #39130, #51140, #45146, #55674, #68068, #62451, #4936, #4559, #62065, #10542, #21829, #66944, #33853, #55302, #21075, #56799, #5310, #3821, #26715, #4191, #50013, #15442, #72576, #61691, #66592 ) ),
 .UNSPECIFIED., .F., .F., .F. ) 
 B_SPLINE_SURFACE_WITH_KNOTS ( ( 2, 2 ),
 ( 3, 2, 2, 2, 2, 2, 2, 2, 2, 2, 2, 2, 2, 2, 2, 2, 2, 2, 2, 2, 2, 2, 2, 2, 2, 2, 2, 2, 2, 2, 2, 2, 2, 2, 2, 2, 2, 2, 2, 2, 2, 2, 2, 2, 2, 2, 2, 2, 2, 2, 2, 2, 2, 2, 2, 2, 2, 2, 2, 2, 2, 2, 2, 2, 2, 2, 2, 2, 2, 2, 2, 2, 2, 2, 2, 2, 2, 2, 2, 2, 2, 2, 2, 2, 2, 2, 2, 2, 2, 2, 2, 2, 2, 2, 2, 2, 2, 2, 2, 2, 2, 2, 2, 2, 2, 2, 2, 2, 2, 2, 2, 2, 2, 2, 2, 2, 2, 2, 2, 2, 2, 2, 2, 2, 2, 2, 2, 2, 2, 2, 2, 2, 2, 2, 2, 2, 2, 2, 2, 2, 2, 2, 3 ),
 ( 0.000000000000000000, 1.000000000000000000 ),
 ( 0.000000000000000000, 0.006944444444444444059, 0.01388888888888888812, 0.02083333333333333218, 0.02777777777777777624, 0.03472222222222222376, 0.04166666666666666435, 0.04861111111111111188, 0.05555555555555555247, 0.06250000000000000000, 0.06944444444444444753, 0.07638888888888889506, 0.08333333333333332871, 0.09027777777777777624, 0.09722222222222222376, 0.1041666666666666713, 0.1111111111111111049, 0.1180555555555555525, 0.1250000000000000000, 0.1319444444444444475, 0.1388888888888888951, 0.1458333333333333426, 0.1527777777777777901, 0.1597222222222222099, 0.1666666666666666574, 0.1736111111111111049, 0.1805555555555555525, 0.1875000000000000000, 0.1944444444444444475, 0.2013888888888888951, 0.2083333333333333426, 0.2152777777777777901, 0.2222222222222222099, 0.2291666666666666574, 0.2361111111111111049, 0.2430555555555555525, 0.2500000000000000000, 0.2569444444444444198, 0.2638888888888888951, 0.2708333333333333148, 0.2777777777777777901, 0.2847222222222222099, 0.2916666666666666852, 0.2986111111111111049, 0.3055555555555555802, 0.3125000000000000000, 0.3194444444444444198, 0.3263888888888888951, 0.3333333333333333148, 0.3402777777777777901, 0.3472222222222222099, 0.3541666666666666852, 0.3611111111111111049, 0.3680555555555555802, 0.3750000000000000000, 0.3819444444444444198, 0.3888888888888888951, 0.3958333333333333148, 0.4027777777777777901, 0.4097222222222222099, 0.4166666666666666852, 0.4236111111111111049, 0.4305555555555555802, 0.4375000000000000000, 0.4444444444444444198, 0.4513888888888888951, 0.4583333333333333148, 0.4652777777777777901, 0.4722222222222222099, 0.4791666666666666852, 0.4861111111111111049, 0.4930555555555555802, 0.5000000000000000000, 0.5069444444444444198, 0.5138888888888888395, 0.5208333333333333703, 0.5277777777777777901, 0.5347222222222222099, 0.5416666666666666297, 0.5486111111111111605, 0.5555555555555555802, 0.5625000000000000000, 0.5694444444444444198, 0.5763888888888888395, 0.5833333333333333703, 0.5902777777777777901, 0.5972222222222222099, 0.6041666666666666297, 0.6111111111111111605, 0.6180555555555555802, 0.6250000000000000000, 0.6319444444444444198, 0.6388888888888888395, 0.6458333333333333703, 0.6527777777777777901, 0.6597222222222222099, 0.6666666666666666297, 0.6736111111111111605, 0.6805555555555555802, 0.6875000000000000000, 0.6944444444444444198, 0.7013888888888888395, 0.7083333333333333703, 0.7152777777777777901, 0.7222222222222222099, 0.7291666666666666297, 0.7361111111111111605, 0.7430555555555555802, 0.7500000000000000000, 0.7569444444444444198, 0.7638888888888888395, 0.7708333333333333703, 0.7777777777777777901, 0.7847222222222222099, 0.7916666666666666297, 0.7986111111111111605, 0.8055555555555555802, 0.8125000000000000000, 0.8194444444444444198, 0.8263888888888888395, 0.8333333333333333703, 0.8402777777777777901, 0.8472222222222222099, 0.8541666666666666297, 0.8611111111111111605, 0.8680555555555555802, 0.8750000000000000000, 0.8819444444444444198, 0.8888888888888888395, 0.8958333333333333703, 0.9027777777777777901, 0.9097222222222222099, 0.9166666666666666297, 0.9236111111111111605, 0.9305555555555555802, 0.9375000000000000000, 0.9444444444444444198, 0.9513888888888888395, 0.9583333333333333703, 0.9652777777777777901, 0.9722222222222222099, 0.9791666666666666297, 0.9842226981114289286 ),
 .UNSPECIFIED. ) 
 GEOMETRIC_REPRESENTATION_ITEM ( )  RATIONAL_B_SPLINE_SURFACE ( (
 ( 1.000000000000000000, 0.8660254037844387076, 1.000000000000000000, 0.8660254037844387076, 1.000000000000000000, 0.8660254037844387076, 1.000000000000000000, 0.8660254037844387076, 1.000000000000000000, 0.8660254037844387076, 1.000000000000000000, 0.8660254037844387076, 1.000000000000000000, 0.8660254037844387076, 1.000000000000000000, 0.8660254037844387076, 1.000000000000000000, 0.8660254037844387076, 1.000000000000000000, 0.8660254037844387076, 1.000000000000000000, 0.8660254037844387076, 1.000000000000000000, 0.8660254037844387076, 1.000000000000000000, 0.8660254037844387076, 1.000000000000000000, 0.8660254037844387076, 1.000000000000000000, 0.8660254037844387076, 1.000000000000000000, 0.8660254037844387076, 1.000000000000000000, 0.8660254037844387076, 1.000000000000000000, 0.8660254037844387076, 1.000000000000000000, 0.8660254037844387076, 1.000000000000000000, 0.8660254037844387076, 1.000000000000000000, 0.8660254037844387076, 1.000000000000000000, 0.8660254037844387076, 1.000000000000000000, 0.8660254037844387076, 1.000000000000000000, 0.8660254037844387076, 1.000000000000000000, 0.8660254037844387076, 1.000000000000000000, 0.8660254037844387076, 1.000000000000000000, 0.8660254037844387076, 1.000000000000000000, 0.8660254037844387076, 1.000000000000000000, 0.8660254037844387076, 1.000000000000000000, 0.8660254037844387076, 1.000000000000000000, 0.8660254037844387076, 1.000000000000000000, 0.8660254037844387076, 1.000000000000000000, 0.8660254037844387076, 1.000000000000000000, 0.8660254037844387076, 1.000000000000000000, 0.8660254037844387076, 1.000000000000000000, 0.8660254037844387076, 1.000000000000000000, 0.8660254037844387076, 1.000000000000000000, 0.8660254037844387076, 1.000000000000000000, 0.8660254037844387076, 1.000000000000000000, 0.8660254037844387076, 1.000000000000000000, 0.8660254037844387076, 1.000000000000000000, 0.8660254037844387076, 1.000000000000000000, 0.8660254037844387076, 1.000000000000000000, 0.8660254037844387076, 1.000000000000000000, 0.8660254037844387076, 1.000000000000000000, 0.8660254037844387076, 1.000000000000000000, 0.8660254037844387076, 1.000000000000000000, 0.8660254037844387076, 1.000000000000000000, 0.8660254037844387076, 1.000000000000000000, 0.8660254037844387076, 1.000000000000000000, 0.8660254037844387076, 1.000000000000000000, 0.8660254037844387076, 1.000000000000000000, 0.8660254037844387076, 1.000000000000000000, 0.8660254037844387076, 1.000000000000000000, 0.8660254037844387076, 1.000000000000000000, 0.8660254037844387076, 1.000000000000000000, 0.8660254037844387076, 1.000000000000000000, 0.8660254037844387076, 1.000000000000000000, 0.8660254037844387076, 1.000000000000000000, 0.8660254037844387076, 1.000000000000000000, 0.8660254037844387076, 1.000000000000000000, 0.8660254037844387076, 1.000000000000000000, 0.8660254037844387076, 1.000000000000000000, 0.8660254037844387076, 1.000000000000000000, 0.8660254037844387076, 1.000000000000000000, 0.8660254037844387076, 1.000000000000000000, 0.8660254037844387076, 1.000000000000000000, 0.8660254037844387076, 1.000000000000000000, 0.8660254037844387076, 1.000000000000000000, 0.8660254037844387076, 1.000000000000000000, 0.8660254037844387076, 1.000000000000000000, 0.8660254037844387076, 1.000000000000000000, 0.8660254037844387076, 1.000000000000000000, 0.8660254037844387076, 1.000000000000000000, 0.8660254037844387076, 1.000000000000000000, 0.8660254037844387076, 1.000000000000000000, 0.8660254037844387076, 1.000000000000000000, 0.8660254037844387076, 1.000000000000000000, 0.8660254037844387076, 1.000000000000000000, 0.8660254037844387076, 1.000000000000000000, 0.8660254037844387076, 1.000000000000000000, 0.8660254037844387076, 1.000000000000000000, 0.8660254037844387076, 1.000000000000000000, 0.8660254037844387076, 1.000000000000000000, 0.8660254037844387076, 1.000000000000000000, 0.8660254037844387076, 1.000000000000000000, 0.8660254037844387076, 1.000000000000000000, 0.8660254037844387076, 1.000000000000000000, 0.8660254037844387076, 1.000000000000000000, 0.8660254037844387076, 1.000000000000000000, 0.8660254037844387076, 1.000000000000000000, 0.8660254037844387076, 1.000000000000000000, 0.8660254037844387076, 1.000000000000000000, 0.8660254037844387076, 1.000000000000000000, 0.8660254037844387076, 1.000000000000000000, 0.8660254037844387076, 1.000000000000000000, 0.8660254037844387076, 1.000000000000000000, 0.8660254037844387076, 1.000000000000000000, 0.8660254037844387076, 1.000000000000000000, 0.8660254037844387076, 1.000000000000000000, 0.8660254037844387076, 1.000000000000000000, 0.8660254037844387076, 1.000000000000000000, 0.8660254037844387076, 1.000000000000000000, 0.8660254037844387076, 1.000000000000000000, 0.8660254037844387076, 1.000000000000000000, 0.8660254037844387076, 1.000000000000000000, 0.8660254037844387076, 1.000000000000000000, 0.8660254037844387076, 1.000000000000000000, 0.8660254037844387076, 1.000000000000000000, 0.8660254037844387076, 1.000000000000000000, 0.8660254037844387076, 1.000000000000000000, 0.8660254037844387076, 1.000000000000000000, 0.8660254037844387076, 1.000000000000000000, 0.8660254037844387076, 1.000000000000000000, 0.8660254037844387076, 1.000000000000000000, 0.8660254037844387076, 1.000000000000000000, 0.8660254037844387076, 1.000000000000000000, 0.8660254037844387076, 1.000000000000000000, 0.8660254037844387076, 1.000000000000000000, 0.8660254037844387076, 1.000000000000000000, 0.8660254037844387076, 1.000000000000000000, 0.8660254037844387076, 1.000000000000000000, 0.8660254037844387076, 1.000000000000000000, 0.8660254037844387076, 1.000000000000000000, 0.8660254037844387076, 1.000000000000000000, 0.8660254037844387076, 1.000000000000000000, 0.8660254037844387076, 1.000000000000000000, 0.8660254037844387076, 1.000000000000000000, 0.8660254037844387076, 1.000000000000000000, 0.8660254037844387076, 1.000000000000000000, 0.8660254037844387076, 1.000000000000000000, 0.8660254037844387076, 1.000000000000000000, 0.8660254037844387076, 1.000000000000000000, 0.8660254037844387076, 1.000000000000000000, 0.8660254037844387076, 1.000000000000000000, 0.8660254037844387076, 1.000000000000000000, 0.8660254037844387076, 1.000000000000000000, 0.8660254037844387076, 1.000000000000000000, 0.8660254037844387076, 1.000000000000000000, 0.8660254037844387076, 1.000000000000000000, 0.8660254037844387076, 1.000000000000000000, 0.9024573129378109515, 0.9469501470576147106),
 ( 1.000000000000000000, 0.8660254037844387076, 1.000000000000000000, 0.8660254037844387076, 1.000000000000000000, 0.8660254037844387076, 1.000000000000000000, 0.8660254037844387076, 1.000000000000000000, 0.8660254037844387076, 1.000000000000000000, 0.8660254037844387076, 1.000000000000000000, 0.8660254037844387076, 1.000000000000000000, 0.8660254037844387076, 1.000000000000000000, 0.8660254037844387076, 1.000000000000000000, 0.8660254037844387076, 1.000000000000000000, 0.8660254037844387076, 1.000000000000000000, 0.8660254037844387076, 1.000000000000000000, 0.8660254037844387076, 1.000000000000000000, 0.8660254037844387076, 1.000000000000000000, 0.8660254037844387076, 1.000000000000000000, 0.8660254037844387076, 1.000000000000000000, 0.8660254037844387076, 1.000000000000000000, 0.8660254037844387076, 1.000000000000000000, 0.8660254037844387076, 1.000000000000000000, 0.8660254037844387076, 1.000000000000000000, 0.8660254037844387076, 1.000000000000000000, 0.8660254037844387076, 1.000000000000000000, 0.8660254037844387076, 1.000000000000000000, 0.8660254037844387076, 1.000000000000000000, 0.8660254037844387076, 1.000000000000000000, 0.8660254037844387076, 1.000000000000000000, 0.8660254037844387076, 1.000000000000000000, 0.8660254037844387076, 1.000000000000000000, 0.8660254037844387076, 1.000000000000000000, 0.8660254037844387076, 1.000000000000000000, 0.8660254037844387076, 1.000000000000000000, 0.8660254037844387076, 1.000000000000000000, 0.8660254037844387076, 1.000000000000000000, 0.8660254037844387076, 1.000000000000000000, 0.8660254037844387076, 1.000000000000000000, 0.8660254037844387076, 1.000000000000000000, 0.8660254037844387076, 1.000000000000000000, 0.8660254037844387076, 1.000000000000000000, 0.8660254037844387076, 1.000000000000000000, 0.8660254037844387076, 1.000000000000000000, 0.8660254037844387076, 1.000000000000000000, 0.8660254037844387076, 1.000000000000000000, 0.8660254037844387076, 1.000000000000000000, 0.8660254037844387076, 1.000000000000000000, 0.8660254037844387076, 1.000000000000000000, 0.8660254037844387076, 1.000000000000000000, 0.8660254037844387076, 1.000000000000000000, 0.8660254037844387076, 1.000000000000000000, 0.8660254037844387076, 1.000000000000000000, 0.8660254037844387076, 1.000000000000000000, 0.8660254037844387076, 1.000000000000000000, 0.8660254037844387076, 1.000000000000000000, 0.8660254037844387076, 1.000000000000000000, 0.8660254037844387076, 1.000000000000000000, 0.8660254037844387076, 1.000000000000000000, 0.8660254037844387076, 1.000000000000000000, 0.8660254037844387076, 1.000000000000000000, 0.8660254037844387076, 1.000000000000000000, 0.8660254037844387076, 1.000000000000000000, 0.8660254037844387076, 1.000000000000000000, 0.8660254037844387076, 1.000000000000000000, 0.8660254037844387076, 1.000000000000000000, 0.8660254037844387076, 1.000000000000000000, 0.8660254037844387076, 1.000000000000000000, 0.8660254037844387076, 1.000000000000000000, 0.8660254037844387076, 1.000000000000000000, 0.8660254037844387076, 1.000000000000000000, 0.8660254037844387076, 1.000000000000000000, 0.8660254037844387076, 1.000000000000000000, 0.8660254037844387076, 1.000000000000000000, 0.8660254037844387076, 1.000000000000000000, 0.8660254037844387076, 1.000000000000000000, 0.8660254037844387076, 1.000000000000000000, 0.8660254037844387076, 1.000000000000000000, 0.8660254037844387076, 1.000000000000000000, 0.8660254037844387076, 1.000000000000000000, 0.8660254037844387076, 1.000000000000000000, 0.8660254037844387076, 1.000000000000000000, 0.8660254037844387076, 1.000000000000000000, 0.8660254037844387076, 1.000000000000000000, 0.8660254037844387076, 1.000000000000000000, 0.8660254037844387076, 1.000000000000000000, 0.8660254037844387076, 1.000000000000000000, 0.8660254037844387076, 1.000000000000000000, 0.8660254037844387076, 1.000000000000000000, 0.8660254037844387076, 1.000000000000000000, 0.8660254037844387076, 1.000000000000000000, 0.8660254037844387076, 1.000000000000000000, 0.8660254037844387076, 1.000000000000000000, 0.8660254037844387076, 1.000000000000000000, 0.8660254037844387076, 1.000000000000000000, 0.8660254037844387076, 1.000000000000000000, 0.8660254037844387076, 1.000000000000000000, 0.8660254037844387076, 1.000000000000000000, 0.8660254037844387076, 1.000000000000000000, 0.8660254037844387076, 1.000000000000000000, 0.8660254037844387076, 1.000000000000000000, 0.8660254037844387076, 1.000000000000000000, 0.8660254037844387076, 1.000000000000000000, 0.8660254037844387076, 1.000000000000000000, 0.8660254037844387076, 1.000000000000000000, 0.8660254037844387076, 1.000000000000000000, 0.8660254037844387076, 1.000000000000000000, 0.8660254037844387076, 1.000000000000000000, 0.8660254037844387076, 1.000000000000000000, 0.8660254037844387076, 1.000000000000000000, 0.8660254037844387076, 1.000000000000000000, 0.8660254037844387076, 1.000000000000000000, 0.8660254037844387076, 1.000000000000000000, 0.8660254037844387076, 1.000000000000000000, 0.8660254037844387076, 1.000000000000000000, 0.8660254037844387076, 1.000000000000000000, 0.8660254037844387076, 1.000000000000000000, 0.8660254037844387076, 1.000000000000000000, 0.8660254037844387076, 1.000000000000000000, 0.8660254037844387076, 1.000000000000000000, 0.8660254037844387076, 1.000000000000000000, 0.8660254037844387076, 1.000000000000000000, 0.8660254037844387076, 1.000000000000000000, 0.8660254037844387076, 1.000000000000000000, 0.8660254037844387076, 1.000000000000000000, 0.8660254037844387076, 1.000000000000000000, 0.8660254037844387076, 1.000000000000000000, 0.8660254037844387076, 1.000000000000000000, 0.8660254037844387076, 1.000000000000000000, 0.8660254037844387076, 1.000000000000000000, 0.8660254037844387076, 1.000000000000000000, 0.8660254037844387076, 1.000000000000000000, 0.8660254037844387076, 1.000000000000000000, 0.8660254037844387076, 1.000000000000000000, 0.8660254037844387076, 1.000000000000000000, 0.8660254037844387076, 1.000000000000000000, 0.8660254037844387076, 1.000000000000000000, 0.8660254037844387076, 1.000000000000000000, 0.8660254037844387076, 1.000000000000000000, 0.8660254037844387076, 1.000000000000000000, 0.8660254037844387076, 1.000000000000000000, 0.8660254037844387076, 1.000000000000000000, 0.8660254037844387076, 1.000000000000000000, 0.8660254037844387076, 1.000000000000000000, 0.8660254037844387076, 1.000000000000000000, 0.9024573129378109515, 0.9469501470576147106) ) ) 
 REPRESENTATION_ITEM ( '' )  SURFACE ( )  );
#17181 = FACE_OUTER_BOUND ( 'NONE', #40222, .T. ) ;
#17182 = DIRECTION ( 'NONE',  ( 0.000000000000000000, -0.4067366430757897722, -0.9135454576426056406 ) ) ;
#17183 = CARTESIAN_POINT ( 'NONE',  ( -10.00000000000000000, 0.000000000000000000, 0.000000000000000000 ) ) ;
#17184 = EDGE_CURVE ( 'NONE', #47180, #10365, #63898, .T. ) ;
#17185 = AXIS2_PLACEMENT_3D ( 'NONE', #1714, #34396, #51697 ) ;
#17186 = FACE_OUTER_BOUND ( 'NONE', #25647, .T. ) ;
#17187 = CARTESIAN_POINT ( 'NONE',  ( 97.30629616937498838, -208.6684592857803011, 76.83697916753382628 ) ) ;
#17188 = CIRCLE ( 'NONE', #65234, 31.99999999999998579 ) ;
#17189 = EDGE_LOOP ( 'NONE', ( #70713, #61160, #28392, #11904 ) ) ;
#17190 = ORIENTED_EDGE ( 'NONE', *, *, #31496, .T. ) ;
#17191 = CARTESIAN_POINT ( 'NONE',  ( 97.30629616937498838, -208.6684592857803295, 86.36197916753383197 ) ) ;
#17192 = CARTESIAN_POINT ( 'NONE',  ( 5.000000000000000000, -15.48615015657610705, 39.04073710021338428 ) ) ;
#17193 = LINE ( 'NONE', #67583, #47151 ) ;
#17194 = CIRCLE ( 'NONE', #30379, 31.99999999999999645 ) ;
#17195 = CARTESIAN_POINT ( 'NONE',  ( 0.000000000000000000, -11.95096189432312350, -23.69967320028773372 ) ) ;
#17196 = DIRECTION ( 'NONE',  ( -1.000000000000000000, -0.000000000000000000, 0.000000000000000000 ) ) ;
#17197 = AXIS2_PLACEMENT_3D ( 'NONE', #70395, #30555, #18903 ) ;
#17198 = CARTESIAN_POINT ( 'NONE',  ( 10.00000000000000000, 0.000000000000000000, 0.000000000000000000 ) ) ;
#17199 = CARTESIAN_POINT ( 'NONE',  ( 97.64999999999997726, -208.4700217866474645, 87.83041666666666458 ) ) ;
#17200 = ORIENTED_EDGE ( 'NONE', *, *, #8574, .F. ) ;
#17201 = ORIENTED_EDGE ( 'NONE', *, *, #21047, .F. ) ;
#17202 = ORIENTED_EDGE ( 'NONE', *, *, #59343, .F. ) ;
#17203 = ORIENTED_EDGE ( 'NONE', *, *, #6945, .T. ) ;
#17204 = VECTOR ( 'NONE', #39918, 1000.000000000000000 ) ;
#17205 = AXIS2_PLACEMENT_3D ( 'NONE', #2593, #17988, #7075 ) ;
#17206 = SURFACE_STYLE_FILL_AREA ( #22859 ) ;
#17207 = CYLINDRICAL_SURFACE ( 'NONE', #13693, 16.00000000000000000 ) ;
#17208 = DIRECTION ( 'NONE',  ( -1.000000000000000000, -0.000000000000000000, -0.000000000000000000 ) ) ;
#17209 = CARTESIAN_POINT ( 'NONE',  ( 97.64999999999999147, -209.9999999999999716, 76.42687500173430237 ) ) ;
#17210 = CARTESIAN_POINT ( 'NONE',  ( 92.34999999999999432, 88.47002178664753558, 79.25791666666665947 ) ) ;
#17211 = ORIENTED_EDGE ( 'NONE', *, *, #13913, .F. ) ;
#17212 = FACE_OUTER_BOUND ( 'NONE', #44016, .T. ) ;
#17213 = ORIENTED_EDGE ( 'NONE', *, *, #15947, .T. ) ;
#17214 = DIRECTION ( 'NONE',  ( -0.000000000000000000, -0.000000000000000000, -1.000000000000000000 ) ) ;
#17215 = ORIENTED_EDGE ( 'NONE', *, *, #73567, .F. ) ;
#17216 = CARTESIAN_POINT ( 'NONE',  ( 97.64999999994533653, -210.0000170172949367, 88.49187441316098557 ) ) ;
#17217 = CARTESIAN_POINT ( 'NONE',  ( -95.00000000000002842, 92.66308142843932671, 82.65781250086715204 ) ) ;
#17218 = CARTESIAN_POINT ( 'NONE',  ( 94.99999999999998579, 92.66308142843935514, 77.41906250086714181 ) ) ;
#17219 = ORIENTED_EDGE ( 'NONE', *, *, #25725, .T. ) ;
#17220 = CYLINDRICAL_SURFACE ( 'NONE', #51385, 31.99999999999998579 ) ;
#17221 = CARTESIAN_POINT ( 'NONE',  ( 11.99999999999999822, -71.27951684758005513, -30.41916302227188851 ) ) ;
#17222 = CARTESIAN_POINT ( 'NONE',  ( 15.70000000000274909, -120.0000000000000568, -70.59999999999959641 ) ) ;
#17223 = EDGE_CURVE ( 'NONE', #59860, #7101, #19144, .T. ) ;
#17224 = DIRECTION ( 'NONE',  ( -1.000000000000000000, 0.000000000000000000, 0.000000000000000000 ) ) ;
#17225 = ORIENTED_EDGE ( 'NONE', *, *, #31760, .T. ) ;
#17226 = LINE ( 'NONE', #22882, #56715 ) ;
#17227 = CARTESIAN_POINT ( 'NONE',  ( -97.30629616937497417, -211.3315407142195852, 77.63072916753380071 ) ) ;
#17228 = VERTEX_POINT ( 'NONE', #43489 ) ;
#17229 = EDGE_CURVE ( 'NONE', #32135, #71894, #21250, .T. ) ;
#17230 = EDGE_LOOP ( 'NONE', ( #18205, #57327, #50182, #15825 ) ) ;
#17231 = FACE_OUTER_BOUND ( 'NONE', #33462, .T. ) ;
#17232 = EDGE_CURVE ( 'NONE', #58994, #19312, #34515, .T. ) ;
#17233 = EDGE_CURVE ( 'NONE', #39724, #66486, #49445, .T. ) ;
#17234 = ORIENTED_EDGE ( 'NONE', *, *, #65020, .F. ) ;
#17235 = DIRECTION ( 'NONE',  ( -0.000000000000000000, -0.000000000000000000, 1.000000000000000000 ) ) ;
#17236 =( REPRESENTATION_RELATIONSHIP ('NONE','NONE', #31117, #27826 ) REPRESENTATION_RELATIONSHIP_WITH_TRANSFORMATION ( #72213 )SHAPE_REPRESENTATION_RELATIONSHIP( ) );
#17237 = VECTOR ( 'NONE', #73184, 1000.000000000000000 ) ;
#17238 = CARTESIAN_POINT ( 'NONE',  ( 0.000000000000000000, -44.99326035066007279, -68.55367621811190304 ) ) ;
#17239 = ORIENTED_EDGE ( 'NONE', *, *, #50674, .T. ) ;
#17240 = CARTESIAN_POINT ( 'NONE',  ( -97.30629616937497417, -208.6684592857803011, 75.61989583420047722 ) ) ;
#17241 = ORIENTED_EDGE ( 'NONE', *, *, #55692, .F. ) ;
#17242 = DIRECTION ( 'NONE',  ( -1.000000000000000000, 0.000000000000000000, -0.000000000000000000 ) ) ;
#17243 = CARTESIAN_POINT ( 'NONE',  ( 5.000000000000002665, 78.73519480814985627, -22.90783923731548199 ) ) ;
#17244 = CARTESIAN_POINT ( 'NONE',  ( 0.000000000000000000, -10.74501242461258244, -35.92658777277521409 ) ) ;
#17245 = DIRECTION ( 'NONE',  ( 0.000000000000000000, 0.000000000000000000, 1.000000000000000000 ) ) ;
#17246 = CARTESIAN_POINT ( 'NONE',  ( -96.15314808468747287, -208.0026889286704943, 76.20197916753380696 ) ) ;
#17247 = CARTESIAN_POINT ( 'NONE',  ( -92.35000000010070664, 90.00002309722640348, 83.41187580057902551 ) ) ;
#17248 = AXIS2_PLACEMENT_3D ( 'NONE', #34109, #49904, #5562 ) ;
#17249 = FILL_AREA_STYLE ('',( #22902 ) ) ;
#17250 = CARTESIAN_POINT ( 'NONE',  ( 93.84685191531248449, 88.00268892867053694, 85.93864583420048575 ) ) ;
#17251 = DIRECTION ( 'NONE',  ( 0.000000000000000000, 0.000000000000000000, 1.000000000000000000 ) ) ;
#17252 = FACE_OUTER_BOUND ( 'NONE', #64578, .T. ) ;
#17253 = LINE ( 'NONE', #56370, #20469 ) ;
#17254 = CARTESIAN_POINT ( 'NONE',  ( 10.00000000000000000, -30.41916302227060598, -71.27951684758059514 ) ) ;
#17255 = EDGE_CURVE ( 'NONE', #67978, #16108, #38669, .T. ) ;
#17256 = CARTESIAN_POINT ( 'NONE',  ( 10.00000000000000000, 55.20638768913831029, -51.02545421589267960 ) ) ;
#17257 = CARTESIAN_POINT ( 'NONE',  ( 2.618768541235299896, 4.261555969668734178, -0.5078976954042870862 ) ) ;
#17258 = CARTESIAN_POINT ( 'NONE',  ( 11.99999999999999822, -5.256550761632340141, -77.32052557432847095 ) ) ;
#17259 = AXIS2_PLACEMENT_3D ( 'NONE', #4547, #10161, #50379 ) ;
#17260 = CARTESIAN_POINT ( 'NONE',  ( 0.000000000000000000, -34.94270380257586339, -74.18225833017926618 ) ) ;
#17261 = CARTESIAN_POINT ( 'NONE',  ( -5.565113727472255967, 10.17789316117534248, -54.99999999999998579 ) ) ;
#17262 = VECTOR ( 'NONE', #26201, 1000.000000000000000 ) ;
#17263 = CARTESIAN_POINT ( 'NONE',  ( -96.15314808468752972, 91.99731107132950569, 88.90197916753380980 ) ) ;
#17264 = EDGE_CURVE ( 'NONE', #26699, #28789, #17043, .T. ) ;
#17265 = EDGE_CURVE ( 'NONE', #28789, #808, #40049, .T. ) ;
#17266 = DIRECTION ( 'NONE',  ( 0.000000000000000000, 0.000000000000000000, 1.000000000000000000 ) ) ;
#17267 = CARTESIAN_POINT ( 'NONE',  ( 11.99999999999999822, 0.000000000000000000, 0.000000000000000000 ) ) ;
#17268 = FACE_OUTER_BOUND ( 'NONE', #11715, .T. ) ;
#17269 = CARTESIAN_POINT ( 'NONE',  ( 5.000000000000000000, -60.67117009219176538, 55.16347631943019536 ) ) ;
#17270 =( LENGTH_UNIT ( ) NAMED_UNIT ( * ) SI_UNIT ( .MILLI., .METRE. ) );
#17271 = CIRCLE ( 'NONE', #66482, 16.00000000000000000 ) ;
#17272 = CARTESIAN_POINT ( 'NONE',  ( 0.000000000000000000, -12.26510123303234501, -35.53030884539098366 ) ) ;
#17273 = LINE ( 'NONE', #52216, #74024 ) ;
#17274 = CARTESIAN_POINT ( 'NONE',  ( 93.84685191531251292, -211.9973110713294489, 84.19239583420049655 ) ) ;
#17275 = ORIENTED_EDGE ( 'NONE', *, *, #9989, .F. ) ;
#17276 = VERTEX_POINT ( 'NONE', #51701 ) ;
#17277 = CARTESIAN_POINT ( 'NONE',  ( -97.65000000000001990, 90.00000000000004263, 90.00000000000000000 ) ) ;
#17278 = ORIENTED_EDGE ( 'NONE', *, *, #42102, .T. ) ;
#17279 = AXIS2_PLACEMENT_3D ( 'NONE', #56356, #57099, #10474 ) ;
#17280 = CARTESIAN_POINT ( 'NONE',  ( 10.00000000000000000, 0.000000000000000000, 0.000000000000000000 ) ) ;
#17281 = CARTESIAN_POINT ( 'NONE',  ( 97.30629616937498838, -208.6684592857803295, 77.31322916753380525 ) ) ;
#17282 = VERTEX_POINT ( 'NONE', #27266 ) ;
#17283 = CARTESIAN_POINT ( 'NONE',  ( 95.00000000000000000, -207.3369185715606307, 83.29281250086717137 ) ) ;
#17284 = ORIENTED_EDGE ( 'NONE', *, *, #31670, .T. ) ;
#17285 = CARTESIAN_POINT ( 'NONE',  ( -93.67499999999998295, -212.2949673200287179, 88.30666666666665776 ) ) ;
#17286 = ORIENTED_EDGE ( 'NONE', *, *, #23694, .T. ) ;
#17287 = ORIENTED_EDGE ( 'NONE', *, *, #44259, .F. ) ;
#17288 =( NAMED_UNIT ( * ) SI_UNIT ( $, .STERADIAN. ) SOLID_ANGLE_UNIT ( ) );
#17289 = AXIS2_PLACEMENT_3D ( 'NONE', #20706, #3443, #26346 ) ;
#17290 = DIRECTION ( 'NONE',  ( -0.000000000000000000, 0.9781476007338042455, -0.2079116908177663092 ) ) ;
#17291 = ORIENTED_EDGE ( 'NONE', *, *, #12366, .T. ) ;
#17292 = CYLINDRICAL_SURFACE ( 'NONE', #46122, 2.649999999999985700 ) ;
#17293 = CARTESIAN_POINT ( 'NONE',  ( 92.35000000000002274, -208.4700217866474645, 88.12145833506762926 ) ) ;
#17294 = EDGE_LOOP ( 'NONE', ( #44961, #67940, #56505, #28191 ) ) ;
#17295 = CARTESIAN_POINT ( 'NONE',  ( 0.000000000000000000, -75.11764819372145041, -2.946379043147127064 ) ) ;
#17296 = AXIS2_PLACEMENT_3D ( 'NONE', #41694, #6750, #7120 ) ;
#17297 = ORIENTED_EDGE ( 'NONE', *, *, #66105, .T. ) ;
#17298 = DIRECTION ( 'NONE',  ( -1.000000000000000000, 0.000000000000000000, -0.000000000000000000 ) ) ;
#17299 = AXIS2_PLACEMENT_3D ( 'NONE', #36673, #66374, #25765 ) ;
#17300 = ORIENTED_EDGE ( 'NONE', *, *, #31126, .F. ) ;
#17301 = ADVANCED_FACE ( 'NONE', ( #74253 ), #50578, .F. ) ;
#17302 = EDGE_CURVE ( 'NONE', #51617, #17407, #29481, .T. ) ;
#17303 = EDGE_LOOP ( 'NONE', ( #55852, #61883 ) ) ;
#17304 = AXIS2_PLACEMENT_3D ( 'NONE', #37039, #72353, #36289 ) ;
#17305 = ORIENTED_EDGE ( 'NONE', *, *, #2741, .T. ) ;
#17306 = DIRECTION ( 'NONE',  ( -1.000000000000000000, -0.000000000000000000, 0.000000000000000000 ) ) ;
#17307 = CIRCLE ( 'NONE', #29266, 31.99999999999998934 ) ;
#17308 = CARTESIAN_POINT ( 'NONE',  ( -5.000000000000000000, -0.6964580643377609181, -0.6026403643956899092 ) ) ;
#17309 = EDGE_LOOP ( 'NONE', ( #22047, #18362, #10695, #36367 ) ) ;
#17310 = EDGE_LOOP ( 'NONE', ( #36534, #36142, #19118, #39578 ) ) ;
#17311 = EDGE_CURVE ( 'NONE', #23404, #57225, #11469, .T. ) ;
#17312 = ORIENTED_EDGE ( 'NONE', *, *, #9518, .F. ) ;
#17313 = CARTESIAN_POINT ( 'NONE',  ( 92.35000000000000853, -209.9999999999999716, 76.03000000000000114 ) ) ;
#17314 = DIRECTION ( 'NONE',  ( -0.000000000000000000, -0.000000000000000000, 1.000000000000000000 ) ) ;
#17315 = EDGE_CURVE ( 'NONE', #70504, #53075, #10358, .T. ) ;
#17316 = CARTESIAN_POINT ( 'NONE',  ( -97.65000000000001990, 91.52997821335253548, 86.77208333333334167 ) ) ;
#17317 = ORIENTED_EDGE ( 'NONE', *, *, #70232, .F. ) ;
#17318 = CARTESIAN_POINT ( 'NONE',  ( 0.000000000000000000, 30.00120703465236716, -22.64427369931138756 ) ) ;
#17319 = CIRCLE ( 'NONE', #7713, 16.00000000000000000 ) ;
#17320 = ORIENTED_EDGE ( 'NONE', *, *, #35904, .T. ) ;
#17321 = CARTESIAN_POINT ( 'NONE',  ( 0.000000000000000000, 59.03342792756328095, -46.54456581323744757 ) ) ;
#17322 = CARTESIAN_POINT ( 'NONE',  ( -94.99999999999997158, -212.6630814284392557, 87.26156250086714294 ) ) ;
#17324 = ORIENTED_EDGE ( 'NONE', *, *, #11964, .F. ) ;
#17323 = ADVANCED_FACE ( 'NONE', ( #68256 ), #68997, .T. ) ;
#17325 = DIRECTION ( 'NONE',  ( -1.000000000000000000, -0.000000000000000000, -0.000000000000000000 ) ) ;
#17326 = DIRECTION ( 'NONE',  ( -1.000000000000000000, 0.000000000000000000, 0.000000000000000000 ) ) ;
#17327 = CARTESIAN_POINT ( 'NONE',  ( 93.67500000000001137, -207.7050326799711968, 87.98916666666666231 ) ) ;
#17328 = CARTESIAN_POINT ( 'NONE',  ( -93.84685191531247028, -211.9973110713294489, 75.24947916753380639 ) ) ;
#17329 = CIRCLE ( 'NONE', #50912, 16.00000000000000355 ) ;
#17330 = FACE_OUTER_BOUND ( 'NONE', #66485, .T. ) ;
#17331 = CARTESIAN_POINT ( 'NONE',  ( 10.00000000000000000, 41.76106447765580043, -62.50884508063379741 ) ) ;
#17332 = DIRECTION ( 'NONE',  ( -1.000000000000000000, -0.000000000000000000, 0.000000000000000000 ) ) ;
#17333 = DIRECTION ( 'NONE',  ( 1.000000000000000000, -0.000000000000000000, -0.000000000000000000 ) ) ;
#17334 = EDGE_CURVE ( 'NONE', #21312, #27851, #22387, .T. ) ;
#17335 = DIRECTION ( 'NONE',  ( 0.000000000000000000, -1.000000000000000000, 0.000000000000000000 ) ) ;
#17336 = EDGE_CURVE ( 'NONE', #68357, #71000, #22013, .T. ) ;
#17337 = CARTESIAN_POINT ( 'NONE',  ( -97.30629616937501680, 90.00000000000004263, 78.84781250086714977 ) ) ;
#17338 = CYLINDRICAL_SURFACE ( 'NONE', #32249, 42.00000000000000000 ) ;
#17339 = CYLINDRICAL_SURFACE ( 'NONE', #25457, 62.50000000000000000 ) ;
#17340 = ORIENTED_EDGE ( 'NONE', *, *, #28496, .F. ) ;
#17341 = CARTESIAN_POINT ( 'NONE',  ( 0.000000000000000000, 46.54456581323805153, 59.03342792756280488 ) ) ;
#17342 = CYLINDRICAL_SURFACE ( 'NONE', #53321, 2.649999999999985700 ) ;
#17343 = CARTESIAN_POINT ( 'NONE',  ( 92.35002600474523149, -211.5299932271990428, 86.32229270695526679 ) ) ;
#17344 = EDGE_CURVE ( 'NONE', #25482, #61033, #26631, .T. ) ;
#17345 = EDGE_CURVE ( 'NONE', #56703, #47902, #39692, .T. ) ;
#17346 = VECTOR ( 'NONE', #7026, 1000.000000000000000 ) ;
#17347 = DIRECTION ( 'NONE',  ( -1.000000000000000000, -3.907985046680551022E-14, 0.000000000000000000 ) ) ;
#17348 = CARTESIAN_POINT ( 'NONE',  ( 0.000000000000000000, -0.8299999999999999600, 0.000000000000000000 ) ) ;
#17349 = CARTESIAN_POINT ( 'NONE',  ( -94.99999999999997158, -207.3369185715606307, 75.03781250086714749 ) ) ;
#17350 = LINE ( 'NONE', #27885, #40489 ) ;
#17351 = CIRCLE ( 'NONE', #59373, 2.541999999999999815 ) ;
#17352 = VERTEX_POINT ( 'NONE', #68636 ) ;
#17353 = AXIS2_PLACEMENT_3D ( 'NONE', #68503, #47050, #35742 ) ;
#17354 = DIRECTION ( 'NONE',  ( 0.000000000000000000, 0.000000000000000000, 1.000000000000000000 ) ) ;
#17355 = CARTESIAN_POINT ( 'NONE',  ( 0.000000000000000000, -0.9646360437375309793, 23.52805723605590416 ) ) ;
#17356 = DIRECTION ( 'NONE',  ( -2.603472992746261562E-14, -2.546204323184492723E-14, 1.000000000000000000 ) ) ;
#17357 = DIRECTION ( 'NONE',  ( -3.035766082959412415E-16, -1.000000000000000000, -0.000000000000000000 ) ) ;
#17358 = CIRCLE ( 'NONE', #43783, 82.00000000000000000 ) ;
#17359 = VECTOR ( 'NONE', #49796, 1000.000000000000000 ) ;
#17360 = AXIS2_PLACEMENT_3D ( 'NONE', #18805, #42498, #7904 ) ;
#17361 = DIRECTION ( 'NONE',  ( -1.000000000000000000, 0.000000000000000000, 0.000000000000000000 ) ) ;
#17362 = ORIENTED_EDGE ( 'NONE', *, *, #41607, .F. ) ;
#17363 = DIRECTION ( 'NONE',  ( 1.000000000000000000, 0.000000000000000000, 0.000000000000000000 ) ) ;
#17364 = FACE_OUTER_BOUND ( 'NONE', #54274, .T. ) ;
#17365 = ORIENTED_EDGE ( 'NONE', *, *, #64006, .T. ) ;
#17366 = CIRCLE ( 'NONE', #59394, 12.75000000000265388 ) ;
#17367 = CARTESIAN_POINT ( 'NONE',  ( 97.30629616937498838, -209.9999999999999716, 89.32531250086714181 ) ) ;
#17368 = DIRECTION ( 'NONE',  ( -1.000000000000000000, 0.000000000000000000, -0.000000000000000000 ) ) ;
#17369 = ORIENTED_EDGE ( 'NONE', *, *, #37591, .F. ) ;
#17370 = EDGE_CURVE ( 'NONE', #39963, #10633, #60306, .T. ) ;
#17371 = LINE ( 'NONE', #40303, #22485 ) ;
#17372 = EDGE_LOOP ( 'NONE', ( #73593, #42343 ) ) ;
#17373 = CYLINDRICAL_SURFACE ( 'NONE', #52679, 37.49900000000000233 ) ;
#17374 = ORIENTED_EDGE ( 'NONE', *, *, #10449, .T. ) ;
#17375 = CARTESIAN_POINT ( 'NONE',  ( 0.000000000000000000, 0.000000000000000000, 0.000000000000000000 ) ) ;
#17376 = VERTEX_POINT ( 'NONE', #5116 ) ;
#17377 = FACE_OUTER_BOUND ( 'NONE', #70090, .T. ) ;
#17378 = ORIENTED_EDGE ( 'NONE', *, *, #45699, .T. ) ;
#17379 = ADVANCED_FACE ( 'NONE', ( #73131 ), #73879, .F. ) ;
#17380 = ORIENTED_EDGE ( 'NONE', *, *, #12066, .T. ) ;
#17381 = CARTESIAN_POINT ( 'NONE',  ( 1.243286885786405054E-17, -120.0000000000000000, 127.5000000000000000 ) ) ;
#17382 = EDGE_CURVE ( 'NONE', #56343, #37995, #23064, .T. ) ;
#17383 = ORIENTED_EDGE ( 'NONE', *, *, #29092, .F. ) ;
#17384 = EDGE_CURVE ( 'NONE', #1863, #21262, #46065, .T. ) ;
#17385 = VERTEX_POINT ( 'NONE', #15997 ) ;
#17386 =( BOUNDED_CURVE ( )  B_SPLINE_CURVE ( 2, ( #30991, #25733, #43038, #71584, #43423, #26095, #37015 ),
 .UNSPECIFIED., .F., .F. ) 
 B_SPLINE_CURVE_WITH_KNOTS ( ( 3, 2, 2, 3 ),
 ( 0.6458333333333334814, 0.6527777777777779011, 0.6597222222222223209, 0.6666666666666667407 ),
 .UNSPECIFIED. ) 
 CURVE ( )  GEOMETRIC_REPRESENTATION_ITEM ( )  RATIONAL_B_SPLINE_CURVE ( ( 0.9999999999999978906, 0.8660254037844408170, 1.000000000000000000, 0.8660254037844387076, 1.000000000000000000, 0.8660254037844365982, 1.000000000000002220 ) ) 
 REPRESENTATION_ITEM ( '' )  );
#17387 = CARTESIAN_POINT ( 'NONE',  ( 10.00000000000000000, -50.95692526931286181, -58.39081064771806240 ) ) ;
#17388 = ORIENTED_EDGE ( 'NONE', *, *, #46335, .T. ) ;
#17389 = EDGE_CURVE ( 'NONE', #9311, #70940, #56230, .T. ) ;
#17390 = VERTEX_POINT ( 'NONE', #12939 ) ;
#17391 = CARTESIAN_POINT ( 'NONE',  ( 97.30629616937498838, 90.00000000000002842, 86.15031250086714465 ) ) ;
#17392 = ORIENTED_EDGE ( 'NONE', *, *, #29769, .F. ) ;
#17393 = CARTESIAN_POINT ( 'NONE',  ( 92.69370383062501162, -208.6684592857803011, 81.96989583420048575 ) ) ;
#17394 = AXIS2_PLACEMENT_3D ( 'NONE', #58919, #64551, #35234 ) ;
#17395 = PRODUCT_CONTEXT ( 'NONE', #29621, 'mechanical' ) ;
#17396 = CYLINDRICAL_SURFACE ( 'NONE', #37813, 82.00000000000000000 ) ;
#17397 = CARTESIAN_POINT ( 'NONE',  ( 97.64999999999999147, 90.00000000000002842, 85.87249999999998806 ) ) ;
#17398 = DIRECTION ( 'NONE',  ( 0.000000000000000000, 0.5877852522924685852, 0.8090169943749506709 ) ) ;
#17399 = CARTESIAN_POINT ( 'NONE',  ( 12.00000000000000000, -26.23277895567245466, 4.042438405570107918 ) ) ;
#17400 = CARTESIAN_POINT ( 'NONE',  ( 0.000000000000000000, -20.41045688087876897, 72.35160999960810102 ) ) ;
#17401 = DIRECTION ( 'NONE',  ( 0.000000000000000000, 0.000000000000000000, 1.000000000000000000 ) ) ;
#17402 = CARTESIAN_POINT ( 'NONE',  ( -93.84685191531248449, -208.0026889286704943, 84.35114583420048007 ) ) ;
#17403 = CARTESIAN_POINT ( 'NONE',  ( -93.84685191531254134, 91.99731107132950569, 81.96989583420048575 ) ) ;
#17404 = ORIENTED_EDGE ( 'NONE', *, *, #38347, .F. ) ;
#17406 = CARTESIAN_POINT ( 'NONE',  ( -92.69370383062502583, 91.33154071421968467, 84.93322916753379559 ) ) ;
#17405 = CARTESIAN_POINT ( 'NONE',  ( 94.99999999999998579, 87.33691857156068750, 84.72156250086713669 ) ) ;
#17407 = VERTEX_POINT ( 'NONE', #46430 ) ;
#17408 = LINE ( 'NONE', #12863, #43122 ) ;
#17409 = VECTOR ( 'NONE', #21042, 1000.000000000000000 ) ;
#17410 = ADVANCED_FACE ( 'NONE', ( #53181 ), #64102, .T. ) ;
#17411 = DIRECTION ( 'NONE',  ( 0.000000000000000000, 0.000000000000000000, 1.000000000000000000 ) ) ;
#17412 = VECTOR ( 'NONE', #23686, 1000.000000000000000 ) ;
#17413 = FACE_OUTER_BOUND ( 'NONE', #56316, .T. ) ;
#17414 = CARTESIAN_POINT ( 'NONE',  ( 97.65000000000003411, -208.4700217866474929, 85.29041666666665833 ) ) ;
#17415 = CARTESIAN_POINT ( 'NONE',  ( -94.99999999999997158, -207.3369185715606307, 86.30906250086714238 ) ) ;
#17416 = DIRECTION ( 'NONE',  ( 0.000000000000000000, -0.5877852522924689183, -0.8090169943749504489 ) ) ;
#17417 = LINE ( 'NONE', #28689, #53007 ) ;
#17418 = DIRECTION ( 'NONE',  ( -1.000000000000000000, 0.000000000000000000, -0.000000000000000000 ) ) ;
#17419 = AXIS2_PLACEMENT_3D ( 'NONE', #12906, #64068, #23466 ) ;
#17420 = DIRECTION ( 'NONE',  ( -1.000000000000000000, 0.000000000000000000, -0.000000000000000000 ) ) ;
#17421 = ORIENTED_EDGE ( 'NONE', *, *, #14660, .F. ) ;
#17422 = VERTEX_POINT ( 'NONE', #35875 ) ;
#17423 = AXIS2_PLACEMENT_3D ( 'NONE', #19078, #42764, #25096 ) ;
#17424 = CARTESIAN_POINT ( 'NONE',  ( -93.67500000000003979, 92.29496732002878900, 79.62833333333333030 ) ) ;
#17425 = EDGE_CURVE ( 'NONE', #37277, #19782, #21865, .T. ) ;
#17426 = CARTESIAN_POINT ( 'NONE',  ( 10.00000000000000000, 68.67312586194995561, 35.91791733033500122 ) ) ;
#17427 = EDGE_CURVE ( 'NONE', #50699, #53610, #292, .T. ) ;
#17428 = CARTESIAN_POINT ( 'NONE',  ( -94.22990255303811580, -207.7668333712727531, 74.81945665767622700 ) ) ;
#17429 = CARTESIAN_POINT ( 'NONE',  ( -95.00000000000002842, 93.05995642670504253, 79.76062500173429726 ) ) ;
#17430 = CARTESIAN_POINT ( 'NONE',  ( 95.00000000002596323, -209.9999999999999147, -64.99999999999349143 ) ) ;
#17431 = CARTESIAN_POINT ( 'NONE',  ( 10.00000000000000000, -81.34940948281344220, 10.30890764327356557 ) ) ;
#17432 = DIRECTION ( 'NONE',  ( 0.000000000000000000, 0.000000000000000000, 1.000000000000000000 ) ) ;
#17433 = EDGE_CURVE ( 'NONE', #21187, #69267, #47542, .T. ) ;
#17434 = VERTEX_POINT ( 'NONE', #52063 ) ;
#17435 = CARTESIAN_POINT ( 'NONE',  ( -95.00000000000002842, 92.66308142843932671, 79.95906250086713385 ) ) ;
#17436 = AXIS2_PLACEMENT_3D ( 'NONE', #35530, #35164, #23515 ) ;
#17437 = DIRECTION ( 'NONE',  ( 1.000000000000000000, 0.000000000000000000, 0.000000000000000000 ) ) ;
#17438 = CYLINDRICAL_SURFACE ( 'NONE', #37833, 37.49900000000000233 ) ;
#17439 = DIRECTION ( 'NONE',  ( 1.000000000000000000, 1.427937372958405461E-15, 7.962523111839130290E-16 ) ) ;
#17440 = DIRECTION ( 'NONE',  ( 0.000000000000000000, 0.000000000000000000, 1.000000000000000000 ) ) ;
#17441 = AXIS2_PLACEMENT_3D ( 'NONE', #73456, #21961, #37422 ) ;
#17442 = CARTESIAN_POINT ( 'NONE',  ( -92.35000000000179909, 90.00000306648279036, 75.79187510780352000 ) ) ;
#17443 = CARTESIAN_POINT ( 'NONE',  ( -97.30629616937497417, -211.3315407142195852, 88.58447916753382856 ) ) ;
#17444 = CARTESIAN_POINT ( 'NONE',  ( 92.69370383062498320, 88.66845928578035796, 75.88447916753382572 ) ) ;
#17445 = CARTESIAN_POINT ( 'NONE',  ( -94.99999999999997158, -207.3369185715606307, 78.21281250086717307 ) ) ;
#17446 = DIRECTION ( 'NONE',  ( -1.000000000000000000, 0.000000000000000000, 0.000000000000000000 ) ) ;
#17447 = VERTEX_POINT ( 'NONE', #69355 ) ;
#17448 = CARTESIAN_POINT ( 'NONE',  ( 92.34999999999999432, 88.47002178664752137, 87.59229166840096070 ) ) ;
#17449 = CARTESIAN_POINT ( 'NONE',  ( 0.000000000000000000, 21.53537804866081373, 30.80686688397018358 ) ) ;
#17450 = CARTESIAN_POINT ( 'NONE',  ( 97.64999999946594755, -209.9999467985095976, 78.96687695417307395 ) ) ;
#17451 = AXIS2_PLACEMENT_3D ( 'NONE', #14801, #3187, #70447 ) ;
#17452 = CARTESIAN_POINT ( 'NONE',  ( -93.84685191531254134, 91.99731107132950569, 75.61989583420049144 ) ) ;
#17453 = CARTESIAN_POINT ( 'NONE',  ( 93.84685191531251292, -211.9973110713294489, 75.77864583420047495 ) ) ;
#17454 = VERTEX_POINT ( 'NONE', #52814 ) ;
#17455 = EDGE_CURVE ( 'NONE', #50464, #54897, #47907, .T. ) ;
#17456 = CARTESIAN_POINT ( 'NONE',  ( 0.000000000000000000, 0.000000000000000000, 0.000000000000000000 ) ) ;
#17457 = ORIENTED_EDGE ( 'NONE', *, *, #67815, .F. ) ;
#17458 = AXIS2_PLACEMENT_3D ( 'NONE', #35944, #69418, #28831 ) ;
#17459 = DIRECTION ( 'NONE',  ( -0.000000000000000000, -0.000000000000000000, 1.000000000000000000 ) ) ;
#17460 = AXIS2_PLACEMENT_3D ( 'NONE', #34795, #69015, #40431 ) ;
#17461 = ORIENTED_EDGE ( 'NONE', *, *, #3327, .T. ) ;
#17462 = CARTESIAN_POINT ( 'NONE',  ( -0.0004442498505991059293, 0.001194404164628348752, -75.00000000000000000 ) ) ;
#17463 = VECTOR ( 'NONE', #69059, 1000.000000000000000 ) ;
#17464 = EDGE_LOOP ( 'NONE', ( #42096, #62076, #49672, #3098, #50951 ) ) ;
#17465 = ORIENTED_EDGE ( 'NONE', *, *, #903, .F. ) ;
#17466 = ADVANCED_FACE ( 'NONE', ( #7324 ), #70446, .F. ) ;
#17467 = CIRCLE ( 'NONE', #59500, 82.00000000000000000 ) ;
#17468 = ORIENTED_EDGE ( 'NONE', *, *, #66198, .T. ) ;
#17469 = DIRECTION ( 'NONE',  ( -0.7585478161175723821, -0.6516173805718057377, 0.000000000000000000 ) ) ;
#17470 = EDGE_CURVE ( 'NONE', #67105, #633, #36237, .T. ) ;
#17471 = VERTEX_POINT ( 'NONE', #24973 ) ;
#17472 = ORIENTED_EDGE ( 'NONE', *, *, #19373, .F. ) ;
#17473 = CARTESIAN_POINT ( 'NONE',  ( 97.30629616937498838, 91.33154071421968467, 84.45697916753383083 ) ) ;
#17474 = DIRECTION ( 'NONE',  ( -0.000000000000000000, -0.000000000000000000, -1.000000000000000000 ) ) ;
#17475 = VECTOR ( 'NONE', #29061, 1000.000000000000000 ) ;
#17476 = VERTEX_POINT ( 'NONE', #11827 ) ;
#17477 = ADVANCED_FACE ( 'NONE', ( #41900 ), #605, .F. ) ;
#17478 = VERTEX_POINT ( 'NONE', #17851 ) ;
#17479 = EDGE_CURVE ( 'NONE', #47114, #62549, #50677, .T. ) ;
#17480 = ORIENTED_EDGE ( 'NONE', *, *, #53128, .F. ) ;
#17481 = ORIENTED_EDGE ( 'NONE', *, *, #43471, .F. ) ;
#17482 = LINE ( 'NONE', #56977, #40696 ) ;
#17483 = DIRECTION ( 'NONE',  ( -2.066836644578058110E-15, -4.863384870155099979E-15, -1.000000000000000000 ) ) ;
#17484 = CARTESIAN_POINT ( 'NONE',  ( -93.67499999999998295, -207.7050326799711968, 85.34333333333333371 ) ) ;
#17485 = DIRECTION ( 'NONE',  ( 1.000000000000000000, 0.000000000000000000, 0.000000000000000000 ) ) ;
#17486 = CARTESIAN_POINT ( 'NONE',  ( 5.000000000000000000, 63.97538442413426907, 51.29473840253247374 ) ) ;
#17487 = CARTESIAN_POINT ( 'NONE',  ( 92.35000000000000853, -209.9999678301211361, 82.45937388908919274 ) ) ;
#17488 = LINE ( 'NONE', #40052, #64773 ) ;
#17489 = DIRECTION ( 'NONE',  ( -0.000000000000000000, -0.000000000000000000, 1.000000000000000000 ) ) ;
#17490 = ORIENTED_EDGE ( 'NONE', *, *, #37594, .F. ) ;
#17491 = CARTESIAN_POINT ( 'NONE',  ( -92.34999999999999432, -209.9999999999999716, 82.77687500173431090 ) ) ;
#17492 = VERTEX_POINT ( 'NONE', #12209 ) ;
#17493 = CARTESIAN_POINT ( 'NONE',  ( 0.000000000000000000, 10.96151621346540317, -35.95386929396244113 ) ) ;
#17494 = VERTEX_POINT ( 'NONE', #7685 ) ;
#17496 = CARTESIAN_POINT ( 'NONE',  ( -96.32500000000001705, 92.29496732002878900, 81.08354166840096866 ) ) ;
#17495 = CARTESIAN_POINT ( 'NONE',  ( 96.32499999999998863, 87.70503267997126784, 79.49604166840096298 ) ) ;
#17497 = ORIENTED_EDGE ( 'NONE', *, *, #5640, .T. ) ;
#17498 = CARTESIAN_POINT ( 'NONE',  ( 92.69370383062498320, 88.66845928578037217, 79.69447916753381378 ) ) ;
#17499 = ADVANCED_FACE ( 'NONE', ( #64841 ), #42268, .F. ) ;
#17500 = DIRECTION ( 'NONE',  ( -0.000000000000000000, -0.000000000000000000, -1.000000000000000000 ) ) ;
#17501 = DIRECTION ( 'NONE',  ( -1.000000000000000000, 0.000000000000000000, 0.000000000000000000 ) ) ;
#17502 = CARTESIAN_POINT ( 'NONE',  ( -97.64998927488493052, 91.52998440550061332, 86.85145790673756494 ) ) ;
#17503 = CARTESIAN_POINT ( 'NONE',  ( 96.32499999999997442, 92.29496732002878900, 81.61270833506763722 ) ) ;
#17504 = VERTEX_POINT ( 'NONE', #23870 ) ;
#17505 = DIRECTION ( 'NONE',  ( 1.000000000000000000, 0.000000000000000000, 0.000000000000000000 ) ) ;
#17506 = CARTESIAN_POINT ( 'NONE',  ( 95.00000000000000000, -206.9400435732949575, 77.14124999999999943 ) ) ;
#17507 = CYLINDRICAL_SURFACE ( 'NONE', #3610, 37.49900000000000233 ) ;
#17508 = ORIENTED_EDGE ( 'NONE', *, *, #22577, .T. ) ;
#17509 = VERTEX_POINT ( 'NONE', #29126 ) ;
#17510 = EDGE_CURVE ( 'NONE', #27833, #57544, #29862, .T. ) ;
#17511 = EDGE_CURVE ( 'NONE', #56318, #50947, #63362, .T. ) ;
#17512 = CARTESIAN_POINT ( 'NONE',  ( 0.000000000000000000, 0.000000000000000000, 0.000000000000000000 ) ) ;
#17513 = DIRECTION ( 'NONE',  ( 0.000000000000000000, -0.4067366430757887730, -0.9135454576426059736 ) ) ;
#17514 = DIRECTION ( 'NONE',  ( -1.000000000000000000, -0.000000000000000000, -0.000000000000000000 ) ) ;
#17515 = CARTESIAN_POINT ( 'NONE',  ( -93.84685191531248449, -208.0026889286704943, 78.15989583420049769 ) ) ;
#17516 = EDGE_CURVE ( 'NONE', #60365, #8457, #36395, .T. ) ;
#17517 = CIRCLE ( 'NONE', #59542, 12.50000000000000000 ) ;
#17518 = EDGE_LOOP ( 'NONE', ( #18409, #21807, #70706, #3177 ) ) ;
#17519 = CARTESIAN_POINT ( 'NONE',  ( 1.250000000000000000, -12.36245420541525597, -1.199999999999999956 ) ) ;
#17520 = VECTOR ( 'NONE', #72750, 1000.000000000000114 ) ;
#17521 = DIRECTION ( 'NONE',  ( -0.1276937514489679404, -0.9918136447140103451, 0.000000000000000000 ) ) ;
#17522 = CYLINDRICAL_SURFACE ( 'NONE', #63353, 31.99999999999998579 ) ;
#17523 = CARTESIAN_POINT ( 'NONE',  ( 92.69370383062498320, 91.33154071421968467, 76.25489583420049655 ) ) ;
#17524 = FACE_OUTER_BOUND ( 'NONE', #73466, .T. ) ;
#17525 = CARTESIAN_POINT ( 'NONE',  ( 97.64998213368511415, 88.47001147152583655, 78.27895762153869441 ) ) ;
#17526 = CIRCLE ( 'NONE', #35552, 11.59999999999999787 ) ;
#17527 = CARTESIAN_POINT ( 'NONE',  ( 25.81725066941077529, -113.8380548628854854, 5.500000000000000000 ) ) ;
#17528 = LINE ( 'NONE', #11511, #36461 ) ;
#17529 = CARTESIAN_POINT ( 'NONE',  ( -10.00000000000000000, 0.000000000000000000, 0.000000000000000000 ) ) ;
#17530 = LINE ( 'NONE', #5165, #27370 ) ;
#17531 = CIRCLE ( 'NONE', #60741, 12.83284365640956182 ) ;
#17532 = CIRCLE ( 'NONE', #21111, 31.99999999999999289 ) ;
#17533 = CARTESIAN_POINT ( 'NONE',  ( 96.15314808468748708, 88.00268892867053694, 86.20322916753382003 ) ) ;
#17534 = CARTESIAN_POINT ( 'NONE',  ( 10.00000000000000000, 33.00180498840046539, 17.80606268964551120 ) ) ;
#17535 = DIRECTION ( 'NONE',  ( 0.000000000000000000, -0.8910065241883627918, -0.4539904997395568520 ) ) ;
#17536 = VERTEX_POINT ( 'NONE', #18588 ) ;
#17537 = DIRECTION ( 'NONE',  ( 2.603472992746261562E-14, 2.546204323184492723E-14, -1.000000000000000000 ) ) ;
#17538 = CARTESIAN_POINT ( 'NONE',  ( -97.30629616937501680, 90.00000000000004263, 80.75281250086715090 ) ) ;
#17539 = CIRCLE ( 'NONE', #51181, 15.06715634359041900 ) ;
#17540 = CARTESIAN_POINT ( 'NONE',  ( 97.30629616937498838, -209.9999999999999716, 89.32531250086714181 ) ) ;
#17541 = EDGE_CURVE ( 'NONE', #67241, #51687, #46033, .T. ) ;
#17542 = ORIENTED_EDGE ( 'NONE', *, *, #41427, .T. ) ;
#17543 = CARTESIAN_POINT ( 'NONE',  ( 0.000000000000000000, -50.95692526931372157, 58.39081064771733054 ) ) ;
#17544 = CYLINDRICAL_SURFACE ( 'NONE', #66014, 62.50000000000000000 ) ;
#17545 = PLANE ( 'NONE',  #13164 ) ;
#17546 = EDGE_CURVE ( 'NONE', #26445, #44855, #13589, .T. ) ;
#17547 = CARTESIAN_POINT ( 'NONE',  ( 0.000000000000000000, -0.8660254037844384856, -1.500000000000000000 ) ) ;
#17548 = CARTESIAN_POINT ( 'NONE',  ( 96.15314808468750130, -211.9973110713294489, 76.04322916753382344 ) ) ;
#17549 = ADVANCED_FACE ( 'NONE', ( #25353 ), #43406, .F. ) ;
#17550 = FACE_OUTER_BOUND ( 'NONE', #7671, .T. ) ;
#17551 = VERTEX_POINT ( 'NONE', #9161 ) ;
#17552 = EDGE_CURVE ( 'NONE', #60251, #42384, #52303, .T. ) ;
#17553 = VERTEX_POINT ( 'NONE', #43018 ) ;
#17554 = CARTESIAN_POINT ( 'NONE',  ( 97.30629616937498838, -209.9999999999999716, 82.49906250086715431 ) ) ;
#17555 = CARTESIAN_POINT ( 'NONE',  ( 10.00000000000000000, 0.000000000000000000, 0.000000000000000000 ) ) ;
#17556 = CARTESIAN_POINT ( 'NONE',  ( 0.000000000000000000, -51.29473840253177030, -63.97538442413482329 ) ) ;
#17557 = CARTESIAN_POINT ( 'NONE',  ( 5.000000000000000888, 0.5616961504262232285, -0.5576671450146228892 ) ) ;
#17558 = CARTESIAN_POINT ( 'NONE',  ( 10.00000000000000000, -62.50329211542407393, -41.76937507738853839 ) ) ;
#17559 = AXIS2_PLACEMENT_3D ( 'NONE', #6781, #11668, #22982 ) ;
#17560 = DIRECTION ( 'NONE',  ( -0.000000000000000000, -0.000000000000000000, -1.000000000000000000 ) ) ;
#17561 = CARTESIAN_POINT ( 'NONE',  ( 95.00000000000000000, -213.0599564267049857, 88.88875000000000171 ) ) ;
#17562 = ORIENTED_EDGE ( 'NONE', *, *, #56033, .T. ) ;
#17563 = EDGE_CURVE ( 'NONE', #18038, #70403, #19327, .T. ) ;
#17564 = ORIENTED_EDGE ( 'NONE', *, *, #13215, .T. ) ;
#17565 = ORIENTED_EDGE ( 'NONE', *, *, #57221, .F. ) ;
#17566 = ORIENTED_EDGE ( 'NONE', *, *, #52866, .T. ) ;
#17567 = FILL_AREA_STYLE_COLOUR ( '', #43005 ) ;
#17568 = CARTESIAN_POINT ( 'NONE',  ( -97.30629616937501680, 91.33154071421968467, 87.20864583420049598 ) ) ;
#17569 = AXIS2_PLACEMENT_3D ( 'NONE', #50865, #26817, #44117 ) ;
#17570 = DIRECTION ( 'NONE',  ( 1.000000000000000000, 0.000000000000000000, 0.000000000000000000 ) ) ;
#17571 = AXIS2_PLACEMENT_3D ( 'NONE', #54379, #3640, #55490 ) ;
#17572 = CARTESIAN_POINT ( 'NONE',  ( 97.64999999981932888, -210.0000309431867436, 78.33187387208516839 ) ) ;
#17573 = CARTESIAN_POINT ( 'NONE',  ( 97.64999999999997726, -208.4700217866474645, 77.11479166840095445 ) ) ;
#17574 = CARTESIAN_POINT ( 'NONE',  ( 92.34999999999999432, 88.47002178664753558, 77.35291666666665833 ) ) ;
#17575 = ORIENTED_EDGE ( 'NONE', *, *, #61828, .T. ) ;
#17576 = CARTESIAN_POINT ( 'NONE',  ( 5.000000000000000000, -36.13751322684404244, -21.40280677340410165 ) ) ;
#17577 = ORIENTED_EDGE ( 'NONE', *, *, #23037, .F. ) ;
#17578 = CARTESIAN_POINT ( 'NONE',  ( 95.00000000000000000, -209.9999999999999716, 90.00000000000000000 ) ) ;
#17579 = VECTOR ( 'NONE', #17335, 1000.000000000000000 ) ;
#17580 = EDGE_CURVE ( 'NONE', #22270, #62061, #48280, .T. ) ;
#17581 = ORIENTED_EDGE ( 'NONE', *, *, #43340, .F. ) ;
#17582 = VECTOR ( 'NONE', #35367, 1000.000000000000000 ) ;
#17583 = CARTESIAN_POINT ( 'NONE',  ( -95.00000000000002842, 93.05995642670501411, 88.65062500173431204 ) ) ;
#17584 = CARTESIAN_POINT ( 'NONE',  ( -92.69370383062504004, 90.00000000000004263, 80.59406250086715318 ) ) ;
#17585 = CARTESIAN_POINT ( 'NONE',  ( 96.15314808468748708, 91.99731107132950569, 88.95489583420049939 ) ) ;
#17586 = ADVANCED_FACE ( 'NONE', ( #36621 ), #14432, .F. ) ;
#17587 = ORIENTED_EDGE ( 'NONE', *, *, #38449, .F. ) ;
#17588 = CARTESIAN_POINT ( 'NONE',  ( 0.000000000000000000, 21.32104025579114648, 30.84782396557224970 ) ) ;
#17589 = LINE ( 'NONE', #57820, #16036 ) ;
#17590 = DIRECTION ( 'NONE',  ( 0.000000000000000000, 0.000000000000000000, -1.000000000000000000 ) ) ;
#17591 = CARTESIAN_POINT ( 'NONE',  ( -97.64999999999997726, -210.0000225208801794, 86.26937578065384571 ) ) ;
#17592 = ORIENTED_EDGE ( 'NONE', *, *, #23202, .T. ) ;
#17593 = DIRECTION ( 'NONE',  ( 0.000000000000000000, -0.4067366430757908269, 0.9135454576426049744 ) ) ;
#17594 = EDGE_CURVE ( 'NONE', #19214, #73443, #66327, .T. ) ;
#17595 = CARTESIAN_POINT ( 'NONE',  ( -93.84685191531247028, -211.9973110713294489, 77.15447916753380753 ) ) ;
#17596 = EDGE_LOOP ( 'NONE', ( #11116, #70140, #71739, #1168 ) ) ;
#17597 = AXIS2_PLACEMENT_3D ( 'NONE', #36040, #34940, #58986 ) ;
#17598 = ORIENTED_EDGE ( 'NONE', *, *, #12997, .F. ) ;
#17599 = FACE_OUTER_BOUND ( 'NONE', #56125, .T. ) ;
#17600 = ORIENTED_EDGE ( 'NONE', *, *, #32172, .T. ) ;
#17601 = ADVANCED_FACE ( 'NONE', ( #31348 ), #59949, .T. ) ;
#17602 = CARTESIAN_POINT ( 'NONE',  ( 10.00000000000000000, 81.34940948281349904, -10.30890764327296871 ) ) ;
#17603 = CARTESIAN_POINT ( 'NONE',  ( 0.000000000000000000, 16.00000000000000000, 2.500000000000000000 ) ) ;
#17604 = ORIENTED_EDGE ( 'NONE', *, *, #69501, .F. ) ;
#17605 = CARTESIAN_POINT ( 'NONE',  ( -94.99999999999997158, -207.3369185715606307, 74.87906250086713555 ) ) ;
#17606 = ORIENTED_EDGE ( 'NONE', *, *, #37516, .F. ) ;
#17607 = CARTESIAN_POINT ( 'NONE',  ( 0.000000000000000000, 0.000000000000000000, 0.000000000000000000 ) ) ;
#17608 = EDGE_CURVE ( 'NONE', #20975, #17752, #72314, .T. ) ;
#17609 = CARTESIAN_POINT ( 'NONE',  ( 0.000000000000000000, -12.26510123303234501, -35.53030884539098366 ) ) ;
#17610 = CARTESIAN_POINT ( 'NONE',  ( -97.64999999980591383, 89.99998015720542810, 86.27002759516649633 ) ) ;
#17611 = ORIENTED_EDGE ( 'NONE', *, *, #73163, .T. ) ;
#17612 = EDGE_CURVE ( 'NONE', #28566, #28744, #8796, .T. ) ;
#17613 = ORIENTED_EDGE ( 'NONE', *, *, #70345, .T. ) ;
#17614 = LINE ( 'NONE', #64582, #73860 ) ;
#17615 = LINE ( 'NONE', #29249, #70904 ) ;
#17616 = CARTESIAN_POINT ( 'NONE',  ( 94.99999999999998579, 92.66308142843932671, 85.67406250086715147 ) ) ;
#17617 = CARTESIAN_POINT ( 'NONE',  ( -97.64999999999986358, -211.5299782133525071, 83.70291666666668107 ) ) ;
#17618 = CYLINDRICAL_SURFACE ( 'NONE', #22998, 31.99999999999998579 ) ;
#17619 = DIRECTION ( 'NONE',  ( 1.000000000000000000, 0.000000000000000000, 0.000000000000000000 ) ) ;
#17620 = CARTESIAN_POINT ( 'NONE',  ( 11.99999999999999822, -75.11764819372145041, 29.05362095685286050 ) ) ;
#17621 = CARTESIAN_POINT ( 'NONE',  ( 0.000000000000000000, 0.000000000000000000, 0.000000000000000000 ) ) ;
#17622 = CARTESIAN_POINT ( 'NONE',  ( 11.99999999999999822, 56.15606465355041621, -59.75363087400016582 ) ) ;
#17623 = CYLINDRICAL_SURFACE ( 'NONE', #72288, 77.49899999999999523 ) ;
#17624 =( BOUNDED_CURVE ( )  B_SPLINE_CURVE ( 2, ( #48465, #60141, #37198, #43222, #71379, #47363, #31533 ),
 .UNSPECIFIED., .F., .F. ) 
 B_SPLINE_CURVE_WITH_KNOTS ( ( 3, 2, 2, 3 ),
 ( 0.7708333333333328152, 0.7777777777777775681, 0.7847222222222222099, 0.7916666666666669627 ),
 .UNSPECIFIED. ) 
 CURVE ( )  GEOMETRIC_REPRESENTATION_ITEM ( )  RATIONAL_B_SPLINE_CURVE ( ( 1.000000000000010658, 0.8660254037844280495, 1.000000000000000000, 0.8660254037844387076, 1.000000000000000000, 0.8660254037844322683, 1.000000000000006439 ) ) 
 REPRESENTATION_ITEM ( '' )  );
#17625 = AXIS2_PLACEMENT_3D ( 'NONE', #41009, #35709, #51905 ) ;
#17626 = CYLINDRICAL_SURFACE ( 'NONE', #44478, 16.00000000000000000 ) ;
#17627 = LINE ( 'NONE', #45479, #55361 ) ;
#17628 = CARTESIAN_POINT ( 'NONE',  ( 11.99999999999999822, 59.03342792756328095, -46.54456581323744757 ) ) ;
#17629 = DIRECTION ( 'NONE',  ( 1.000000000000000000, -0.000000000000000000, -0.000000000000000000 ) ) ;
#17630 = AXIS2_PLACEMENT_3D ( 'NONE', #18879, #41818, #25281 ) ;
#17631 = VECTOR ( 'NONE', #68262, 1000.000000000000000 ) ;
#17632 = DIRECTION ( 'NONE',  ( 0.000000000000000000, 0.9510565162951521989, 0.3090169943749515591 ) ) ;
#17633 = PRODUCT_DEFINITION_SHAPE ( 'NONE', 'NONE',  #74379 ) ;
#17634 = CIRCLE ( 'NONE', #22420, 82.00000000000000000 ) ;
#17635 = EDGE_LOOP ( 'NONE', ( #43641, #6474, #62671, #8317 ) ) ;
#17636 = DIRECTION ( 'NONE',  ( 0.7950889364178796992, -0.6064928550163511956, 0.000000000000000000 ) ) ;
#17637 = CIRCLE ( 'NONE', #4449, 42.00000000000000000 ) ;
#17638 = CARTESIAN_POINT ( 'NONE',  ( 0.000000000000000000, 23.16143007188426850, 73.95703589263983702 ) ) ;
#17639 = CARTESIAN_POINT ( 'NONE',  ( 11.99999999999999822, 51.02545421589324803, 55.20638768913779870 ) ) ;
#17640 = CARTESIAN_POINT ( 'NONE',  ( 10.00000000000000000, 16.45098606841173705, -33.79645857604496229 ) ) ;
#17641 = ADVANCED_FACE ( 'NONE', ( #66683 ), #54515, .F. ) ;
#17642 = CARTESIAN_POINT ( 'NONE',  ( 2.500000000000005773, 4.330127018922191873, -6.000000000000000000 ) ) ;
#17643 = CARTESIAN_POINT ( 'NONE',  ( 92.69370383062501162, -211.3315407142195852, 84.77447916753381207 ) ) ;
#17644 = EDGE_CURVE ( 'NONE', #66693, #36199, #8052, .T. ) ;
#17645 = CIRCLE ( 'NONE', #4458, 20.69999999999999929 ) ;
#17646 = ORIENTED_EDGE ( 'NONE', *, *, #66895, .F. ) ;
#17647 = EDGE_CURVE ( 'NONE', #28395, #56198, #17329, .T. ) ;
#17648 = ORIENTED_EDGE ( 'NONE', *, *, #34115, .T. ) ;
#17649 = AXIS2_PLACEMENT_3D ( 'NONE', #20439, #30591, #14423 ) ;
#17650 = FACE_OUTER_BOUND ( 'NONE', #42170, .T. ) ;
#17651 = ORIENTED_EDGE ( 'NONE', *, *, #52515, .F. ) ;
#17652 = CARTESIAN_POINT ( 'NONE',  ( 2.500000000000000000, 0.000000000000000000, -6.000000000000000000 ) ) ;
#17653 = CARTESIAN_POINT ( 'NONE',  ( 93.84685191531249870, -208.0026889286704943, 76.20197916753380696 ) ) ;
#17654 = ORIENTED_EDGE ( 'NONE', *, *, #24386, .F. ) ;
#17655 = CARTESIAN_POINT ( 'NONE',  ( 96.15314808468748708, -208.0026889286704943, 81.96989583420048575 ) ) ;
#17656 = ORIENTED_EDGE ( 'NONE', *, *, #44412, .T. ) ;
#17657 = LINE ( 'NONE', #35669, #17912 ) ;
#17658 = ORIENTED_EDGE ( 'NONE', *, *, #12066, .F. ) ;
#17659 = ORIENTED_EDGE ( 'NONE', *, *, #33857, .F. ) ;
#17660 = CARTESIAN_POINT ( 'NONE',  ( 0.000000000000000000, 41.81611651403861885, 3.925862922256313503 ) ) ;
#17661 = DIRECTION ( 'NONE',  ( 1.000000000000000000, -0.000000000000000000, -0.000000000000000000 ) ) ;
#17662 = ORIENTED_EDGE ( 'NONE', *, *, #28608, .T. ) ;
#17663 = CYLINDRICAL_SURFACE ( 'NONE', #71310, 31.99999999999998579 ) ;
#17664 = CARTESIAN_POINT ( 'NONE',  ( 97.64999999999997726, -208.4700217866474645, 86.00479166840096923 ) ) ;
#17665 = EDGE_LOOP ( 'NONE', ( #66146, #73966 ) ) ;
#17666 = PLANE ( 'NONE',  #63430 ) ;
#17667 = ORIENTED_EDGE ( 'NONE', *, *, #32824, .F. ) ;
#17668 = CARTESIAN_POINT ( 'NONE',  ( -14.53333333333331545, 1.812507246801946101E-15, -1.466666666666671670 ) ) ;
#17669 = CIRCLE ( 'NONE', #27206, 77.49899999999999523 ) ;
#17670 = VERTEX_POINT ( 'NONE', #37747 ) ;
#17671 = AXIS2_PLACEMENT_3D ( 'NONE', #26263, #73613, #67990 ) ;
#17672 = VERTEX_POINT ( 'NONE', #55397 ) ;
#17673 = ORIENTED_EDGE ( 'NONE', *, *, #70842, .F. ) ;
#17674 = LINE ( 'NONE', #52254, #5725 ) ;
#17675 = EDGE_CURVE ( 'NONE', #58263, #67308, #41311, .T. ) ;
#17676 = EDGE_CURVE ( 'NONE', #7138, #19308, #65582, .T. ) ;
#17677 = FACE_OUTER_BOUND ( 'NONE', #9469, .T. ) ;
#17678 = ORIENTED_EDGE ( 'NONE', *, *, #62211, .F. ) ;
#17679 = ORIENTED_EDGE ( 'NONE', *, *, #23092, .F. ) ;
#17680 = AXIS2_PLACEMENT_3D ( 'NONE', #2297, #59041, #24813 ) ;
#17681 = ORIENTED_EDGE ( 'NONE', *, *, #34531, .T. ) ;
#17682 = CIRCLE ( 'NONE', #21251, 42.00000000000000000 ) ;
#17683 = CYLINDRICAL_SURFACE ( 'NONE', #32492, 77.49899999999999523 ) ;
#17684 = CARTESIAN_POINT ( 'NONE',  ( 26.49955575014745079, 0.001194404164630089764, -64.00000000000000000 ) ) ;
#17685 = CARTESIAN_POINT ( 'NONE',  ( -96.32500000000001705, 92.29496732002878900, 88.62416666666665321 ) ) ;
#17686 = ORIENTED_EDGE ( 'NONE', *, *, #15502, .T. ) ;
#17687 = ADVANCED_FACE ( 'NONE', ( #32819 ), #15917, .F. ) ;
#17688 = CARTESIAN_POINT ( 'NONE',  ( 94.99999999999998579, 87.33691857156068750, 75.83156250086715033 ) ) ;
#17689 = VECTOR ( 'NONE', #48509, 1000.000000000000000 ) ;
#17690 = EDGE_LOOP ( 'NONE', ( #16838, #58558, #26936, #13654 ) ) ;
#17691 = CARTESIAN_POINT ( 'NONE',  ( -8.637688417678550223, 13.69818742750669749, -44.99999999999998579 ) ) ;
#17692 = CARTESIAN_POINT ( 'NONE',  ( -92.69370383062498320, -211.3315407142195852, 85.46239583420047836 ) ) ;
#17693 = ORIENTED_EDGE ( 'NONE', *, *, #28562, .F. ) ;
#17694 = CARTESIAN_POINT ( 'NONE',  ( -96.32499999999996021, -212.2949673200287179, 79.39020833506762642 ) ) ;
#17695 = DIRECTION ( 'NONE',  ( 0.000000000000000000, 0.000000000000000000, 1.000000000000000000 ) ) ;
#17696 = CARTESIAN_POINT ( 'NONE',  ( -94.99999999999997158, -212.6630814284392557, 75.83156250086715033 ) ) ;
#17697 = DIRECTION ( 'NONE',  ( 0.000000000000000000, 0.000000000000000000, 1.000000000000000000 ) ) ;
#17698 = DIRECTION ( 'NONE',  ( 1.000000000000000000, 0.000000000000000000, -0.000000000000000000 ) ) ;
#17699 = CIRCLE ( 'NONE', #29699, 10.00000000000000178 ) ;
#17700 = CYLINDRICAL_SURFACE ( 'NONE', #40939, 77.49899999999999523 ) ;
#17701 = CARTESIAN_POINT ( 'NONE',  ( 11.99999999999999822, 77.16300072079661732, 27.74655509720698277 ) ) ;
#17702 = VECTOR ( 'NONE', #44493, 1000.000000000000000 ) ;
#17703 = CARTESIAN_POINT ( 'NONE',  ( 92.34999999999993747, 88.47002178664756400, 88.14791666666667425 ) ) ;
#17704 = CARTESIAN_POINT ( 'NONE',  ( -92.69370383062504004, 90.00000000000004263, 78.53031250086714010 ) ) ;
#17705 = DIRECTION ( 'NONE',  ( -0.000000000000000000, 0.000000000000000000, 1.000000000000000000 ) ) ;
#17706 = CARTESIAN_POINT ( 'NONE',  ( 0.000000000000000000, 5.835314593368772229, -22.81335362449846826 ) ) ;
#17707 = VERTEX_POINT ( 'NONE', #4287 ) ;
#17708 = CARTESIAN_POINT ( 'NONE',  ( -93.67499999999998295, -207.7050326799711968, 80.34270833506762699 ) ) ;
#17709 = CARTESIAN_POINT ( 'NONE',  ( -1.250000000000000000, -12.36245420541525597, -1.199999999999999956 ) ) ;
#17710 = DIRECTION ( 'NONE',  ( 0.000000000000000000, -0.1564344650402381132, 0.9876883405951365491 ) ) ;
#17711 = DIRECTION ( 'NONE',  ( 0.000000000000000000, -0.9723699203976740035, -0.2334453638559161881 ) ) ;
#17712 = LINE ( 'NONE', #35013, #33330 ) ;
#17713 = DIRECTION ( 'NONE',  ( 0.000000000000000000, -1.000000000000000000, 1.156482317317870936E-15 ) ) ;
#17714 = CARTESIAN_POINT ( 'NONE',  ( -94.99999999999997158, -206.9400435732949575, 89.84125000000000227 ) ) ;
#17715 = DIRECTION ( 'NONE',  ( -1.000000000000000000, 0.000000000000000000, 0.000000000000000000 ) ) ;
#17716 = ORIENTED_EDGE ( 'NONE', *, *, #11865, .T. ) ;
#17717 = CYLINDRICAL_SURFACE ( 'NONE', #15492, 35.50000000000000711 ) ;
#17718 = CARTESIAN_POINT ( 'NONE',  ( -12.00000000000000000, 0.000000000000000000, 0.000000000000000000 ) ) ;
#17719 = DIRECTION ( 'NONE',  ( 0.000000000000000000, 0.000000000000000000, -1.000000000000000000 ) ) ;
#17720 = EDGE_CURVE ( 'NONE', #36390, #39841, #11021, .T. ) ;
#17721 = AXIS2_PLACEMENT_3D ( 'NONE', #9365, #25920, #38693 ) ;
#17722 = ADVANCED_FACE ( 'NONE', ( #5403 ), #33568, .T. ) ;
#17723 = AXIS2_PLACEMENT_3D ( 'NONE', #7181, #1947, #18092 ) ;
#17724 = DIRECTION ( 'NONE',  ( 0.000000000000000000, 0.000000000000000000, -1.000000000000000000 ) ) ;
#17725 = ORIENTED_EDGE ( 'NONE', *, *, #58584, .F. ) ;
#17726 = EDGE_CURVE ( 'NONE', #70845, #61965, #42543, .T. ) ;
#17727 = DIRECTION ( 'NONE',  ( 0.000000000000000000, 0.000000000000000000, -1.000000000000000000 ) ) ;
#17728 = CARTESIAN_POINT ( 'NONE',  ( -97.64999999999996305, -209.9999999999999716, 90.00000000000000000 ) ) ;
#17729 = ORIENTED_EDGE ( 'NONE', *, *, #57315, .T. ) ;
#17730 = EDGE_CURVE ( 'NONE', #36199, #58686, #10129, .T. ) ;
#17731 = CARTESIAN_POINT ( 'NONE',  ( 97.30629616937498838, -208.6684592857803295, 85.56822916753380071 ) ) ;
#17732 = CARTESIAN_POINT ( 'NONE',  ( -92.35001333515619137, -208.4700140875914371, 83.46479220096853169 ) ) ;
#17733 = VERTEX_POINT ( 'NONE', #44116 ) ;
#17734 = CARTESIAN_POINT ( 'NONE',  ( 93.67500000000001137, -212.2949673200287179, 89.47083333333333144 ) ) ;
#17735 = ORIENTED_EDGE ( 'NONE', *, *, #40584, .F. ) ;
#17736 = CARTESIAN_POINT ( 'NONE',  ( 92.35000000000000853, -211.5299782133524218, 85.05229166840096866 ) ) ;
#17737 = EDGE_LOOP ( 'NONE', ( #73718, #34304, #47330, #54382 ) ) ;
#17738 = CARTESIAN_POINT ( 'NONE',  ( -95.00000000000002842, 87.33691857156074434, 79.80031250086715033 ) ) ;
#17739 = ORIENTED_EDGE ( 'NONE', *, *, #17822, .T. ) ;
#17740 = VERTEX_POINT ( 'NONE', #73037 ) ;
#17741 = CIRCLE ( 'NONE', #58587, 31.99999999999999645 ) ;
#17742 = VECTOR ( 'NONE', #9963, 1000.000000000000000 ) ;
#17743 = ORIENTED_EDGE ( 'NONE', *, *, #60536, .T. ) ;
#17744 = DIRECTION ( 'NONE',  ( 0.000000000000000000, -0.5224985647159561264, 0.8526401643540878483 ) ) ;
#17745 = EDGE_CURVE ( 'NONE', #2059, #7320, #67794, .T. ) ;
#17746 = VECTOR ( 'NONE', #8747, 1000.000000000000000 ) ;
#17747 = EDGE_CURVE ( 'NONE', #55747, #32327, #25689, .T. ) ;
#17748 = ORIENTED_EDGE ( 'NONE', *, *, #19748, .F. ) ;
#17749 = ORIENTED_EDGE ( 'NONE', *, *, #20208, .T. ) ;
#17750 = AXIS2_PLACEMENT_3D ( 'NONE', #69957, #47411, #52308 ) ;
#17751 = DIRECTION ( 'NONE',  ( -1.000000000000000000, 0.000000000000000000, 0.000000000000000000 ) ) ;
#17752 = VERTEX_POINT ( 'NONE', #27934 ) ;
#17753 = VERTEX_POINT ( 'NONE', #28296 ) ;
#17754 = CARTESIAN_POINT ( 'NONE',  ( 94.99999999999998579, 87.33691857156068750, 85.35656250086714181 ) ) ;
#17755 = ORIENTED_EDGE ( 'NONE', *, *, #59865, .F. ) ;
#17756 = CARTESIAN_POINT ( 'NONE',  ( 97.30629616937498838, -211.3315407142195852, 83.55739583420047722 ) ) ;
#17757 = EDGE_CURVE ( 'NONE', #20440, #10439, #64136, .T. ) ;
#17758 = ADVANCED_FACE ( 'NONE', ( #16661 ), #73419, .F. ) ;
#17759 = APPLICATION_PROTOCOL_DEFINITION ( 'draft international standard', 'automotive_design', 1998, #6592 ) ;
#17760 = CARTESIAN_POINT ( 'NONE',  ( 0.000000000000000000, 0.000000000000000000, -189.9999999999999147 ) ) ;
#17761 = FACE_OUTER_BOUND ( 'NONE', #66771, .T. ) ;
#17762 = CYLINDRICAL_SURFACE ( 'NONE', #31690, 12.49999999999999645 ) ;
#17763 = CARTESIAN_POINT ( 'NONE',  ( 12.75000000000000000, -120.0000000000000000, -85.60000000000000853 ) ) ;
#17764 = DIRECTION ( 'NONE',  ( 1.000000000000000000, 0.000000000000000000, 0.000000000000000000 ) ) ;
#17765 = CARTESIAN_POINT ( 'NONE',  ( 11.99999999999999822, 0.000000000000000000, 0.000000000000000000 ) ) ;
#17766 = CARTESIAN_POINT ( 'NONE',  ( -96.15314808468745866, -211.9973110713294489, 82.76364583420047438 ) ) ;
#17767 = CARTESIAN_POINT ( 'NONE',  ( -97.30629616937501680, 91.33154071421968467, 82.12864583420048348 ) ) ;
#17768 = ORIENTED_EDGE ( 'NONE', *, *, #4967, .T. ) ;
#17769 = CARTESIAN_POINT ( 'NONE',  ( 93.84685191531248449, 88.00268892867053694, 83.39864583420047950 ) ) ;
#17770 = ORIENTED_EDGE ( 'NONE', *, *, #25215, .F. ) ;
#17771 = DIRECTION ( 'NONE',  ( 0.000000000000000000, 0.9135454576426055295, 0.4067366430757899387 ) ) ;
#17772 = AXIS2_PLACEMENT_3D ( 'NONE', #42444, #45420, #21722 ) ;
#17773 = CARTESIAN_POINT ( 'NONE',  ( -7.499999999999968914, 79.99999999999998579, -189.9999999999999147 ) ) ;
#17774 = CARTESIAN_POINT ( 'NONE',  ( 0.000000000000000000, -46.11716303203136391, -67.80270845531939017 ) ) ;
#17775 = DIRECTION ( 'NONE',  ( -0.000000000000000000, -0.000000000000000000, 1.000000000000000000 ) ) ;
#17776 = CARTESIAN_POINT ( 'NONE',  ( -92.69370383062498320, -209.9999999999999716, 86.78531250086714977 ) ) ;
#17777 = CIRCLE ( 'NONE', #59809, 31.99999999999999645 ) ;
#17778 = CARTESIAN_POINT ( 'NONE',  ( 0.000000000000000000, 0.000000000000000000, 0.000000000000000000 ) ) ;
#17779 = LINE ( 'NONE', #46001, #13382 ) ;
#17780 = DIRECTION ( 'NONE',  ( -1.000000000000000000, -0.000000000000000000, 0.000000000000000000 ) ) ;
#17781 = FACE_OUTER_BOUND ( 'NONE', #53470, .T. ) ;
#17782 = EDGE_LOOP ( 'NONE', ( #49937, #42938, #40239, #10465 ) ) ;
#17783 = AXIS2_PLACEMENT_3D ( 'NONE', #14825, #37776, #60709 ) ;
#17784 = ORIENTED_EDGE ( 'NONE', *, *, #39423, .T. ) ;
#17785 = CARTESIAN_POINT ( 'NONE',  ( -96.32500000000001705, 92.29496732002878900, 77.19416666666666060 ) ) ;
#17786 = CARTESIAN_POINT ( 'NONE',  ( 0.000000000000000000, -0.9646360437375307573, 23.52805723605590060 ) ) ;
#17787 = CARTESIAN_POINT ( 'NONE',  ( 0.000000000000000000, -59.03342792756231461, -46.54456581323868392 ) ) ;
#17788 = CARTESIAN_POINT ( 'NONE',  ( 0.000000000000000000, -14.54903810567645195, -22.19967320028775504 ) ) ;
#17789 = LINE ( 'NONE', #47124, #32579 ) ;
#17790 = CARTESIAN_POINT ( 'NONE',  ( 25.81725066941077529, -113.8380548628854854, 5.500000000000000000 ) ) ;
#17791 = EDGE_LOOP ( 'NONE', ( #6606, #52069, #42845, #67023 ) ) ;
#17792 = CARTESIAN_POINT ( 'NONE',  ( -97.30629616937501680, 88.66845928578038638, 78.26572916753380582 ) ) ;
#17793 = DIRECTION ( 'NONE',  ( -0.4999999999999919509, -0.8660254037844432595, 0.000000000000000000 ) ) ;
#17794 = DIRECTION ( 'NONE',  ( -1.000000000000000000, -0.000000000000000000, 0.000000000000000000 ) ) ;
#17795 = AXIS2_PLACEMENT_3D ( 'NONE', #73685, #28945, #39874 ) ;
#17796 = CYLINDRICAL_SURFACE ( 'NONE', #7039, 37.49900000000000233 ) ;
#17797 = CARTESIAN_POINT ( 'NONE',  ( 10.00000000000000000, -75.16055320797043748, 18.89407956138229494 ) ) ;
#17798 = CARTESIAN_POINT ( 'NONE',  ( 11.99999999999999822, 68.55367621811204515, -44.99326035065983120 ) ) ;
#17799 = CARTESIAN_POINT ( 'NONE',  ( -93.84685191531248449, -208.0026889286704943, 85.14489583420048291 ) ) ;
#17800 = EDGE_CURVE ( 'NONE', #29971, #47446, #50494, .T. ) ;
#17801 = CIRCLE ( 'NONE', #22590, 31.99999999999998224 ) ;
#17803 = EDGE_CURVE ( 'NONE', #10768, #57809, #32922, .T. ) ;
#17802 = AXIS2_PLACEMENT_3D ( 'NONE', #1945, #12436, #65071 ) ;
#17804 = CARTESIAN_POINT ( 'NONE',  ( 96.32499999999998863, -207.7050326799711968, 79.07270833506763097 ) ) ;
#17805 = ADVANCED_FACE ( 'NONE', ( #16284 ), #49742, .T. ) ;
#17806 = AXIS2_PLACEMENT_3D ( 'NONE', #40204, #6371, #28916 ) ;
#17807 = CARTESIAN_POINT ( 'NONE',  ( 92.69370383062498320, 90.00000000000002842, 75.83156250086716454 ) ) ;
#17808 = EDGE_CURVE ( 'NONE', #37620, #69189, #8615, .T. ) ;
#17809 = CARTESIAN_POINT ( 'NONE',  ( -92.69370383062498320, -211.3315407142195852, 78.00114583420049996 ) ) ;
#17810 = LINE ( 'NONE', #30200, #68692 ) ;
#17811 = ORIENTED_EDGE ( 'NONE', *, *, #7025, .F. ) ;
#17812 = CARTESIAN_POINT ( 'NONE',  ( 3.000000000000000000, 2.935248768560057897, -3.252606517456513302E-15 ) ) ;
#17813 = CARTESIAN_POINT ( 'NONE',  ( 0.000000000000000000, -55.19960302592029677, -51.03279382321147750 ) ) ;
#17814 = FACE_OUTER_BOUND ( 'NONE', #37679, .T. ) ;
#17815 = EDGE_CURVE ( 'NONE', #37548, #4632, #29333, .T. ) ;
#17816 = CARTESIAN_POINT ( 'NONE',  ( 0.000000000000000000, -6.555932627142143865, -37.01155633439065440 ) ) ;
#17817 = CARTESIAN_POINT ( 'NONE',  ( 95.00000000000000000, -212.6630814284392557, 78.37156250086714238 ) ) ;
#17818 = ORIENTED_EDGE ( 'NONE', *, *, #25911, .T. ) ;
#17819 = DIRECTION ( 'NONE',  ( -1.000000000000000000, -0.000000000000000000, 0.000000000000000000 ) ) ;
#17820 = ORIENTED_EDGE ( 'NONE', *, *, #6123, .F. ) ;
#17821 =( BOUNDED_CURVE ( )  B_SPLINE_CURVE ( 2, ( #46499, #12278, #13015, #24314, #41978, #17926, #46139 ),
 .UNSPECIFIED., .F., .F. ) 
 B_SPLINE_CURVE_WITH_KNOTS ( ( 3, 2, 2, 3 ),
 ( 0.000000000000000000, 0.006944444444444406762, 0.01388888888888881352, 0.02083333333333322115 ),
 .UNSPECIFIED. ) 
 CURVE ( )  GEOMETRIC_REPRESENTATION_ITEM ( )  RATIONAL_B_SPLINE_CURVE ( ( 1.000000000000000000, 0.8660254037844387076, 1.000000000000000000, 0.8660254037844387076, 1.000000000000000000, 0.8660254037844408170, 0.9999999999999978906 ) ) 
 REPRESENTATION_ITEM ( '' )  );
#17822 = EDGE_CURVE ( 'NONE', #50481, #37253, #39969, .T. ) ;
#17823 = PRESENTATION_LAYER_ASSIGNMENT (  '', '', ( #68227 ) ) ;
#17824 = CARTESIAN_POINT ( 'NONE',  ( -2.499999999999974243, 62.44997998398397954, -275.0000000000000000 ) ) ;
#17825 = ORIENTED_EDGE ( 'NONE', *, *, #8586, .F. ) ;
#17826 = AXIS2_PLACEMENT_3D ( 'NONE', #9109, #30920, #71880 ) ;
#17827 = CIRCLE ( 'NONE', #27423, 62.50000000000000000 ) ;
#17828 = DIRECTION ( 'NONE',  ( -1.000000000000000000, 0.000000000000000000, 0.000000000000000000 ) ) ;
#17829 = VECTOR ( 'NONE', #55708, 1000.000000000000000 ) ;
#17830 = ORIENTED_EDGE ( 'NONE', *, *, #25023, .T. ) ;
#17831 = ORIENTED_EDGE ( 'NONE', *, *, #45168, .T. ) ;
#17832 = VECTOR ( 'NONE', #42148, 1000.000000000000000 ) ;
#17833 = EDGE_LOOP ( 'NONE', ( #25458, #67095 ) ) ;
#17834 = DIRECTION ( 'NONE',  ( -1.000000000000000000, 0.000000000000000000, 0.000000000000000000 ) ) ;
#17835 = ADVANCED_FACE ( 'NONE', ( #53094 ), #51975, .T. ) ;
#17836 = EDGE_CURVE ( 'NONE', #58803, #52520, #49714, .T. ) ;
#17837 = ORIENTED_EDGE ( 'NONE', *, *, #72162, .T. ) ;
#17838 = ORIENTED_EDGE ( 'NONE', *, *, #11068, .T. ) ;
#17839 = CARTESIAN_POINT ( 'NONE',  ( 94.99999999999998579, 92.66308142843935514, 84.56281250086716739 ) ) ;
#17840 = CYLINDRICAL_SURFACE ( 'NONE', #18870, 42.00000000000000000 ) ;
#17841 = ORIENTED_EDGE ( 'NONE', *, *, #3860, .F. ) ;
#17843 = EDGE_LOOP ( 'NONE', ( #29594, #47996, #64349, #25770 ) ) ;
#17842 = VECTOR ( 'NONE', #23465, 1000.000000000000000 ) ;
#17844 = EDGE_LOOP ( 'NONE', ( #39959, #63265, #9421, #35864 ) ) ;
#17845 = ORIENTED_EDGE ( 'NONE', *, *, #7054, .T. ) ;
#17846 = FACE_OUTER_BOUND ( 'NONE', #43383, .T. ) ;
#17847 = CIRCLE ( 'NONE', #35871, 77.49899999999999523 ) ;
#17848 = DIRECTION ( 'NONE',  ( 0.000000000000000000, 0.000000000000000000, 1.000000000000000000 ) ) ;
#17849 = DIRECTION ( 'NONE',  ( -0.000000000000000000, -0.000000000000000000, 1.000000000000000000 ) ) ;
#17850 = DIRECTION ( 'NONE',  ( -1.000000000000000000, 0.000000000000000000, -0.000000000000000000 ) ) ;
#17851 = CARTESIAN_POINT ( 'NONE',  ( 0.000000000000000000, -5.256550761632340141, -77.32052557432847095 ) ) ;
#17852 = CARTESIAN_POINT ( 'NONE',  ( 97.65000000000000568, -211.5299782133524218, 87.16895833506762870 ) ) ;
#17853 = DIRECTION ( 'NONE',  ( 0.000000000000000000, 0.000000000000000000, 1.000000000000000000 ) ) ;
#17854 = AXIS2_PLACEMENT_3D ( 'NONE', #45962, #136, #69617 ) ;
#17855 = B_SPLINE_CURVE_WITH_KNOTS ( 'NONE', 3,
 ( #48126, #65062, #30814, #68575, #2301, #1566, #59409, #47747 ),
 .UNSPECIFIED., .F., .F.,
 ( 4, 2, 2, 4 ),
 ( 0.001653806717454348388, 0.002539064216006851459, 0.002981692965283072420, 0.003424321714559292948 ),
 .UNSPECIFIED. ) ;
#17856 = FACE_OUTER_BOUND ( 'NONE', #43938, .T. ) ;
#17857 = AXIS2_PLACEMENT_3D ( 'NONE', #71518, #24209, #47136 ) ;
#17858 = EDGE_LOOP ( 'NONE', ( #9647, #35507, #17114, #44952 ) ) ;
#17859 = CARTESIAN_POINT ( 'NONE',  ( -94.99999999999997158, -213.0599564267049857, 80.07812500173432113 ) ) ;
#17860 = ORIENTED_EDGE ( 'NONE', *, *, #74106, .T. ) ;
#17861 = CARTESIAN_POINT ( 'NONE',  ( 5.377855484467702900E-15, 4.693886760319831848E-15, 52.00000000000002132 ) ) ;
#17862 = EDGE_LOOP ( 'NONE', ( #26155, #58949 ) ) ;
#17864 = CARTESIAN_POINT ( 'NONE',  ( -97.65000000000001990, 90.00000000000004263, 78.64937500173429896 ) ) ;
#17863 = CARTESIAN_POINT ( 'NONE',  ( 97.64999999999997726, 88.47002178664753558, 78.91395833506763324 ) ) ;
#17865 = AXIS2_PLACEMENT_3D ( 'NONE', #61847, #27627, #33250 ) ;
#17866 = ORIENTED_EDGE ( 'NONE', *, *, #16668, .T. ) ;
#17867 = CARTESIAN_POINT ( 'NONE',  ( 94.99999999999998579, 87.33691857156068750, 80.43531250086715545 ) ) ;
#17868 = CARTESIAN_POINT ( 'NONE',  ( 11.99999999999999822, 23.16143007188530589, -73.95703589263951017 ) ) ;
#17869 = DIRECTION ( 'NONE',  ( -1.000000000000000000, 0.000000000000000000, 0.000000000000000000 ) ) ;
#17870 = DIRECTION ( 'NONE',  ( 0.3853207896976547087, -0.9227826878668540234, 0.000000000000000000 ) ) ;
#17871 = LINE ( 'NONE', #52082, #22203 ) ;
#17872 = ORIENTED_EDGE ( 'NONE', *, *, #52908, .T. ) ;
#17873 = CARTESIAN_POINT ( 'NONE',  ( 10.00000000000000000, -80.55351364060599906, 15.33399622253456940 ) ) ;
#17874 = DIRECTION ( 'NONE',  ( -1.000000000000000000, -0.000000000000000000, -0.000000000000000000 ) ) ;
#17875 = LINE ( 'NONE', #1000, #40780 ) ;
#17876 = VERTEX_POINT ( 'NONE', #1634 ) ;
#17877 = ORIENTED_EDGE ( 'NONE', *, *, #653, .F. ) ;
#17878 = AXIS2_PLACEMENT_3D ( 'NONE', #5032, #27936, #17401 ) ;
#17879 = EDGE_CURVE ( 'NONE', #38198, #25988, #58157, .T. ) ;
#17880 = DIRECTION ( 'NONE',  ( 0.000000000000000000, -0.9510565162951565288, 0.3090169943749383474 ) ) ;
#17881 = DIRECTION ( 'NONE',  ( 0.000000000000000000, 0.000000000000000000, 1.000000000000000000 ) ) ;
#17882 = CARTESIAN_POINT ( 'NONE',  ( -3.000000000000000000, 16.61724383029390140, -20.69703378468903665 ) ) ;
#17883 = CARTESIAN_POINT ( 'NONE',  ( -93.84685191531248449, -208.0026889286704943, 76.88989583420048746 ) ) ;
#17884 = ORIENTED_EDGE ( 'NONE', *, *, #25407, .T. ) ;
#17885 = AXIS2_PLACEMENT_3D ( 'NONE', #31330, #7668, #60663 ) ;
#17886 = DIRECTION ( 'NONE',  ( -1.000000000000000000, 0.000000000000000000, 0.000000000000000000 ) ) ;
#17887 = FACE_OUTER_BOUND ( 'NONE', #50852, .T. ) ;
#17888 = VECTOR ( 'NONE', #5254, 1000.000000000000000 ) ;
#17889 = CARTESIAN_POINT ( 'NONE',  ( 11.99999999999999822, 68.26794271651262136, 31.47745569255165066 ) ) ;
#17890 = LINE ( 'NONE', #64880, #870 ) ;
#17891 = CIRCLE ( 'NONE', #63585, 11.59999999999999787 ) ;
#17892 = DIRECTION ( 'NONE',  ( -0.000000000000000000, -0.000000000000000000, 1.000000000000000000 ) ) ;
#17893 = DIRECTION ( 'NONE',  ( -1.000000000000000000, -0.000000000000000000, -0.000000000000000000 ) ) ;
#17894 = ADVANCED_FACE ( 'NONE', ( #521 ), #17762, .T. ) ;
#17895 = CARTESIAN_POINT ( 'NONE',  ( 14.59956846177685996, -138.4757300459248484, -5.500000000000000000 ) ) ;
#17896 = CYLINDRICAL_SURFACE ( 'NONE', #30444, 31.99999999999998579 ) ;
#17897 = CARTESIAN_POINT ( 'NONE',  ( 10.00000000000000000, 0.000000000000000000, 0.000000000000000000 ) ) ;
#17898 = EDGE_CURVE ( 'NONE', #4009, #65017, #42228, .T. ) ;
#17899 = FACE_OUTER_BOUND ( 'NONE', #7847, .T. ) ;
#17900 = CARTESIAN_POINT ( 'NONE',  ( 93.84685191531248449, 91.99731107132950569, 87.15572916753382060 ) ) ;
#17901 = AXIS2_PLACEMENT_3D ( 'NONE', #33122, #67724, #73345 ) ;
#17902 = EDGE_CURVE ( 'NONE', #68616, #55213, #48549, .T. ) ;
#17903 = DIRECTION ( 'NONE',  ( 0.000000000000000000, 0.000000000000000000, 1.000000000000000000 ) ) ;
#17904 = DIRECTION ( 'NONE',  ( 0.000000000000000000, 0.000000000000000000, 1.000000000000000000 ) ) ;
#17905 = AXIS2_PLACEMENT_3D ( 'NONE', #25180, #13879, #36818 ) ;
#17906 = EDGE_LOOP ( 'NONE', ( #51175, #56031, #72921, #17915 ) ) ;
#17907 = ADVANCED_FACE ( 'NONE', ( #63651 ), #12853, .T. ) ;
#17908 = CARTESIAN_POINT ( 'NONE',  ( 2.600855584879231068E-12, -120.0000000000000000, -65.00000000000000000 ) ) ;
#17909 = CARTESIAN_POINT ( 'NONE',  ( -95.00000000000002842, 92.66308142843932671, 79.95906250086713385 ) ) ;
#17910 = CIRCLE ( 'NONE', #46740, 42.00000000000000000 ) ;
#17911 = CIRCLE ( 'NONE', #59945, 12.49999999999999645 ) ;
#17912 = VECTOR ( 'NONE', #28935, 1000.000000000000000 ) ;
#17913 = AXIS2_PLACEMENT_3D ( 'NONE', #6811, #29723, #1225 ) ;
#17914 = CARTESIAN_POINT ( 'NONE',  ( 95.00000000000000000, -212.6630814284392557, 88.53156250086713897 ) ) ;
#17915 = ORIENTED_EDGE ( 'NONE', *, *, #68375, .T. ) ;
#17916 = CIRCLE ( 'NONE', #21494, 77.49899999999999523 ) ;
#17917 = DIRECTION ( 'NONE',  ( 1.000000000000000000, 5.778480238264233142E-17, -0.000000000000000000 ) ) ;
#17918 = EDGE_CURVE ( 'NONE', #58363, #60133, #68959, .T. ) ;
#17919 = ORIENTED_EDGE ( 'NONE', *, *, #34857, .T. ) ;
#17920 = DIRECTION ( 'NONE',  ( 1.000000000000000000, 0.000000000000000000, 0.000000000000000000 ) ) ;
#17921 = FACE_OUTER_BOUND ( 'NONE', #31873, .T. ) ;
#17922 = VERTEX_POINT ( 'NONE', #891 ) ;
#17923 = EDGE_LOOP ( 'NONE', ( #7855, #4616, #48390, #11288 ) ) ;
#17924 = CARTESIAN_POINT ( 'NONE',  ( 92.69370383062501162, -211.3315407142195852, 82.86947916753379673 ) ) ;
#17925 = EDGE_CURVE ( 'NONE', #16651, #72554, #1752, .T. ) ;
#17926 = CARTESIAN_POINT ( 'NONE',  ( 97.64999999999997726, 91.52997821335253548, 89.73541666666663730 ) ) ;
#17927 = CARTESIAN_POINT ( 'NONE',  ( 10.00000000000000000, -74.65374052328654386, 8.840884882374837161 ) ) ;
#17928 = CARTESIAN_POINT ( 'NONE',  ( -92.34999999999999432, -208.4700217866474645, 77.11479166840095445 ) ) ;
#17929 = LINE ( 'NONE', #12650, #3910 ) ;
#17930 = CIRCLE ( 'NONE', #4759, 15.77977592589476608 ) ;
#17931 = EDGE_CURVE ( 'NONE', #41327, #15281, #52759, .T. ) ;
#17932 = CARTESIAN_POINT ( 'NONE',  ( 0.000000000000000000, 36.13751322684419165, 21.40280677340384585 ) ) ;
#17933 = CARTESIAN_POINT ( 'NONE',  ( 97.64999999999997726, -208.4700217866474645, 85.29041666666665833 ) ) ;
#17934 = AXIS2_PLACEMENT_3D ( 'NONE', #55002, #71547, #65196 ) ;
#17935 = CIRCLE ( 'NONE', #20342, 16.00000000000000000 ) ;
#17936 = ORIENTED_EDGE ( 'NONE', *, *, #41577, .F. ) ;
#17937 = VERTEX_POINT ( 'NONE', #11738 ) ;
#17938 = AXIS2_PLACEMENT_3D ( 'NONE', #57002, #5505, #74275 ) ;
#17939 = VERTEX_POINT ( 'NONE', #24160 ) ;
#17940 = ORIENTED_EDGE ( 'NONE', *, *, #51458, .F. ) ;
#17941 = DIRECTION ( 'NONE',  ( 1.000000000000000000, 0.000000000000000000, 0.000000000000000000 ) ) ;
#17942 = FILL_AREA_STYLE_COLOUR ( '', #26671 ) ;
#17943 = CARTESIAN_POINT ( 'NONE',  ( -92.69370383062502583, 91.33154071421968467, 86.36197916753383197 ) ) ;
#17944 = CARTESIAN_POINT ( 'NONE',  ( 15.00000000000000000, -10.45096189432344502, -21.10159698893425784 ) ) ;
#17945 = LINE ( 'NONE', #69807, #63045 ) ;
#17946 = CARTESIAN_POINT ( 'NONE',  ( 96.32499999999998863, -212.2949673200287179, 76.32104166840096582 ) ) ;
#17947 = CARTESIAN_POINT ( 'NONE',  ( 92.34999999999999432, 90.00000000000002842, 77.29999999999999716 ) ) ;
#17948 = EDGE_LOOP ( 'NONE', ( #71916, #27359, #25876, #60329 ) ) ;
#17949 = CARTESIAN_POINT ( 'NONE',  ( -94.99999999999997158, -213.0599564267049857, 88.96812500173430749 ) ) ;
#17950 = ORIENTED_EDGE ( 'NONE', *, *, #22835, .F. ) ;
#17951 = DIRECTION ( 'NONE',  ( -1.000000000000000000, 0.000000000000000000, 0.000000000000000000 ) ) ;
#17952 = ORIENTED_EDGE ( 'NONE', *, *, #43202, .F. ) ;
#17953 = CARTESIAN_POINT ( 'NONE',  ( -95.00000000000002842, 92.66308142843932671, 80.11781250086714579 ) ) ;
#17954 = CARTESIAN_POINT ( 'NONE',  ( 92.69370383062498320, 90.00000000000002842, 76.30781250086714351 ) ) ;
#17955 = EDGE_LOOP ( 'NONE', ( #57031, #48737, #67294, #35434 ) ) ;
#17956 = DIRECTION ( 'NONE',  ( 1.000000000000000000, 0.000000000000000000, 0.000000000000000000 ) ) ;
#17957 = CARTESIAN_POINT ( 'NONE',  ( 10.00000000000000000, 24.73286445877703699, 73.44644590900070114 ) ) ;
#17958 = AXIS2_PLACEMENT_3D ( 'NONE', #31541, #54484, #37576 ) ;
#17959 = DIRECTION ( 'NONE',  ( -1.000000000000000000, 0.000000000000000000, 0.000000000000000000 ) ) ;
#17960 = DIRECTION ( 'NONE',  ( -1.000000000000000000, 0.000000000000000000, -0.000000000000000000 ) ) ;
#17961 = ORIENTED_EDGE ( 'NONE', *, *, #68323, .F. ) ;
#17962 = DIRECTION ( 'NONE',  ( -1.000000000000000000, 0.000000000000000000, 0.000000000000000000 ) ) ;
#17963 = CIRCLE ( 'NONE', #60002, 1.000000000000000000 ) ;
#17965 = CARTESIAN_POINT ( 'NONE',  ( -96.15314808468747287, -208.0026889286704943, 78.74197916753381321 ) ) ;
#17964 = AXIS2_PLACEMENT_3D ( 'NONE', #14539, #8904, #63032 ) ;
#17966 = ORIENTED_EDGE ( 'NONE', *, *, #43968, .F. ) ;
#17967 = ORIENTED_EDGE ( 'NONE', *, *, #20573, .T. ) ;
#17968 = FACE_BOUND ( 'NONE', #36519, .T. ) ;
#17969 = AXIS2_PLACEMENT_3D ( 'NONE', #68537, #55758, #10259 ) ;
#17970 = AXIS2_PLACEMENT_3D ( 'NONE', #25128, #64993, #58227 ) ;
#17971 = ORIENTED_EDGE ( 'NONE', *, *, #6556, .T. ) ;
#17972 = CARTESIAN_POINT ( 'NONE',  ( 0.000000000000000000, 0.000000000000000000, 0.000000000000000000 ) ) ;
#17973 = DIRECTION ( 'NONE',  ( -2.603472992746261562E-14, -2.546204323184492723E-14, 1.000000000000000000 ) ) ;
#17974 = ORIENTED_EDGE ( 'NONE', *, *, #63035, .T. ) ;
#17975 = CARTESIAN_POINT ( 'NONE',  ( -96.15314808468745866, -211.9973110713294489, 87.36739583420049371 ) ) ;
#17976 = VERTEX_POINT ( 'NONE', #28669 ) ;
#17977 = CARTESIAN_POINT ( 'NONE',  ( -97.64999999999997726, -208.4700217866474645, 81.69208333333332916 ) ) ;
#17978 = CARTESIAN_POINT ( 'NONE',  ( 11.99999999999999822, 0.000000000000000000, 0.000000000000000000 ) ) ;
#17979 = ORIENTED_EDGE ( 'NONE', *, *, #49533, .T. ) ;
#17980 = EDGE_CURVE ( 'NONE', #34136, #17385, #20914, .T. ) ;
#17981 = ORIENTED_EDGE ( 'NONE', *, *, #24948, .T. ) ;
#17982 = CARTESIAN_POINT ( 'NONE',  ( 0.000000000000000000, 36.88895765772642221, -6.736453364083161865 ) ) ;
#17983 = CARTESIAN_POINT ( 'NONE',  ( 93.84685191531248449, 88.00268892867053694, 86.57364583420047666 ) ) ;
#17984 = DIRECTION ( 'NONE',  ( -1.000000000000000000, -0.000000000000000000, -0.000000000000000000 ) ) ;
#17985 = CARTESIAN_POINT ( 'NONE',  ( -95.00000000000002842, 86.94004357329504273, 75.55375000000000796 ) ) ;
#17986 = EDGE_CURVE ( 'NONE', #34058, #49826, #29768, .T. ) ;
#17987 = FACE_OUTER_BOUND ( 'NONE', #35152, .T. ) ;
#17988 = DIRECTION ( 'NONE',  ( -1.000000000000000000, -0.000000000000000000, 0.000000000000000000 ) ) ;
#17989 = DIRECTION ( 'NONE',  ( 0.000000000000000000, 0.9238795325112851842, 0.3826834323650938341 ) ) ;
#17990 = ADVANCED_FACE ( 'NONE', ( #51610 ), #47092, .F. ) ;
#17991 = CARTESIAN_POINT ( 'NONE',  ( 2.184357737007946383E-12, -120.0000000000000000, -48.99999999999997158 ) ) ;
#17992 = DIRECTION ( 'NONE',  ( -1.000000000000000000, 0.000000000000000000, 0.000000000000000000 ) ) ;
#17993 = CARTESIAN_POINT ( 'NONE',  ( 0.000000000000000000, 30.84782396557248418, -21.32104025579081252 ) ) ;
#17994 = EDGE_CURVE ( 'NONE', #58503, #4038, #30505, .T. ) ;
#17995 = CYLINDRICAL_SURFACE ( 'NONE', #34929, 77.49899999999999523 ) ;
#17996 = CIRCLE ( 'NONE', #21631, 82.00000000000000000 ) ;
#17997 = CARTESIAN_POINT ( 'NONE',  ( 6.000000000000001776, 0.000000000000000000, 0.000000000000000000 ) ) ;
#17998 = CARTESIAN_POINT ( 'NONE',  ( 97.64999999999999147, -209.9999999999999716, 90.00000000000000000 ) ) ;
#17999 = AXIS2_PLACEMENT_3D ( 'NONE', #17183, #69061, #40116 ) ;
#18000 = DIRECTION ( 'NONE',  ( 1.000000000000000000, 0.000000000000000000, 0.000000000000000000 ) ) ;
#18001 = EDGE_CURVE ( 'NONE', #19615, #29989, #48190, .T. ) ;
#18002 = ORIENTED_EDGE ( 'NONE', *, *, #30449, .F. ) ;
#18003 = CARTESIAN_POINT ( 'NONE',  ( 92.34999999999999432, 90.00000000000002842, 85.55499999999999261 ) ) ;
#18004 = ADVANCED_FACE ( 'NONE', ( #10092 ), #44697, .T. ) ;
#18005 = ADVANCED_FACE ( 'NONE', ( #65858 ), #30513, .T. ) ;
#18006 = CARTESIAN_POINT ( 'NONE',  ( 93.67499999999998295, 92.29496732002878900, 77.19416666666666060 ) ) ;
#18007 = CARTESIAN_POINT ( 'NONE',  ( 11.99999999999999822, 35.91791733033476675, 68.67312586195008350 ) ) ;
#18008 = DIRECTION ( 'NONE',  ( 1.000000000000000000, 0.000000000000000000, 0.000000000000000000 ) ) ;
#18009 = VECTOR ( 'NONE', #26186, 1000.000000000000000 ) ;
#18010 = DIRECTION ( 'NONE',  ( -1.000000000000000000, 0.000000000000000000, 0.000000000000000000 ) ) ;
#18011 = CIRCLE ( 'NONE', #51603, 57.50000000000000000 ) ;
#18012 = AXIS2_PLACEMENT_3D ( 'NONE', #67422, #56142, #38106 ) ;
#18013 = VECTOR ( 'NONE', #40352, 1000.000000000000000 ) ;
#18014 = CARTESIAN_POINT ( 'NONE',  ( 95.00000000000000000, -212.6630814284392557, 84.88031250086714863 ) ) ;
#18015 = ORIENTED_EDGE ( 'NONE', *, *, #31999, .T. ) ;
#18016 = AXIS2_PLACEMENT_3D ( 'NONE', #15822, #10171, #62444 ) ;
#18017 = ORIENTED_EDGE ( 'NONE', *, *, #5727, .T. ) ;
#18018 = VECTOR ( 'NONE', #8300, 1000.000000000000000 ) ;
#18019 = EDGE_CURVE ( 'NONE', #10962, #59827, #40197, .T. ) ;
#18020 = CARTESIAN_POINT ( 'NONE',  ( 10.00000000000000000, 0.000000000000000000, 0.000000000000000000 ) ) ;
#18021 = ORIENTED_EDGE ( 'NONE', *, *, #4124, .T. ) ;
#18022 = DIRECTION ( 'NONE',  ( -1.000000000000000000, -0.000000000000000000, 0.000000000000000000 ) ) ;
#18023 = CARTESIAN_POINT ( 'NONE',  ( 93.84685191531251292, -211.9973110713294489, 75.77864583420047495 ) ) ;
#18024 = ORIENTED_EDGE ( 'NONE', *, *, #35816, .T. ) ;
#18025 = CARTESIAN_POINT ( 'NONE',  ( 97.30629616937498838, -211.3315407142195852, 79.27114583420048177 ) ) ;
#18026 = EDGE_LOOP ( 'NONE', ( #43464, #59454, #31055, #1335 ) ) ;
#18027 = DIRECTION ( 'NONE',  ( 0.1276937514489694392, 0.9918136447140102341, -0.000000000000000000 ) ) ;
#18028 = VERTEX_POINT ( 'NONE', #65494 ) ;
#18029 = AXIS2_PLACEMENT_3D ( 'NONE', #46950, #8190, #64990 ) ;
#18030 = EDGE_LOOP ( 'NONE', ( #72684, #59082 ) ) ;
#18031 = FACE_BOUND ( 'NONE', #35522, .T. ) ;
#18032 =( NAMED_UNIT ( * ) SI_UNIT ( $, .STERADIAN. ) SOLID_ANGLE_UNIT ( ) );
#18033 = CARTESIAN_POINT ( 'NONE',  ( 10.00000000000000000, 16.65560815589464028, -38.55633173626993937 ) ) ;
#18034 = ORIENTED_EDGE ( 'NONE', *, *, #56694, .T. ) ;
#18035 = CARTESIAN_POINT ( 'NONE',  ( 0.000000000000000000, 0.000000000000000000, 0.000000000000000000 ) ) ;
#18036 = CARTESIAN_POINT ( 'NONE',  ( 93.67500000000001137, -212.2949673200287179, 85.74020833506763495 ) ) ;
#18037 = CARTESIAN_POINT ( 'NONE',  ( 93.67499999999999716, 87.70503267997126784, 89.47083333333333144 ) ) ;
#18038 = VERTEX_POINT ( 'NONE', #54570 ) ;
#18039 = CARTESIAN_POINT ( 'NONE',  ( 19.29194287201271862, -133.5026271600380880, 5.500000000000000000 ) ) ;
#18040 = EDGE_LOOP ( 'NONE', ( #25914, #42891, #17600, #68885 ) ) ;
#18041 = VERTEX_POINT ( 'NONE', #54211 ) ;
#18042 = CYLINDRICAL_SURFACE ( 'NONE', #6075, 16.00000000000000000 ) ;
#18043 = ORIENTED_EDGE ( 'NONE', *, *, #4441, .T. ) ;
#18044 = CARTESIAN_POINT ( 'NONE',  ( 92.34999999999999432, 91.52997821335252127, 84.94645833506763211 ) ) ;
#18045 = VECTOR ( 'NONE', #18715, 1000.000000000000000 ) ;
#18046 = ORIENTED_EDGE ( 'NONE', *, *, #46181, .F. ) ;
#18047 = PRESENTATION_STYLE_ASSIGNMENT (( #24072 ) ) ;
#18048 = ORIENTED_EDGE ( 'NONE', *, *, #56789, .F. ) ;
#18049 = CYLINDRICAL_SURFACE ( 'NONE', #47719, 31.99999999999998579 ) ;
#18050 = AXIS2_PLACEMENT_3D ( 'NONE', #41563, #64504, #12979 ) ;
#18051 = LINE ( 'NONE', #63926, #57082 ) ;
#18052 = ORIENTED_EDGE ( 'NONE', *, *, #6715, .T. ) ;
#18053 = ORIENTED_EDGE ( 'NONE', *, *, #21142, .T. ) ;
#18054 = VECTOR ( 'NONE', #60861, 1000.000000000000000 ) ;
#18055 = ORIENTED_EDGE ( 'NONE', *, *, #35237, .F. ) ;
#18056 = DIRECTION ( 'NONE',  ( 1.000000000000000000, 0.000000000000000000, 0.000000000000000000 ) ) ;
#18057 = DIRECTION ( 'NONE',  ( 0.000000000000000000, 0.4539904997395412534, 0.8910065241883706744 ) ) ;
#18058 = CARTESIAN_POINT ( 'NONE',  ( -93.67500000000003979, 92.29496732002878900, 87.88333333333332575 ) ) ;
#18059 = ORIENTED_EDGE ( 'NONE', *, *, #60727, .T. ) ;
#18060 = CARTESIAN_POINT ( 'NONE',  ( 92.35000000000000853, -208.4700217866474645, 89.94708333333332462 ) ) ;
#18061 = ORIENTED_EDGE ( 'NONE', *, *, #20866, .F. ) ;
#18062 =( BOUNDED_CURVE ( )  B_SPLINE_CURVE ( 2, ( #9753, #54871, #4503, #50337, #73267, #65158, #37954, #9374, #21381 ),
 .UNSPECIFIED., .F., .F. ) 
 B_SPLINE_CURVE_WITH_KNOTS ( ( 3, 2, 2, 2, 3 ),
 ( 0.5291824299508944840, 0.5362381811070600079, 0.5432939466479423940, 0.5503497121888247801, 0.5503499107226623721 ),
 .UNSPECIFIED. ) 
 CURVE ( )  GEOMETRIC_REPRESENTATION_ITEM ( )  RATIONAL_B_SPLINE_CURVE ( ( 1.000000000000000000, 0.8660254037844387076, 1.000000000000000000, 0.8660254037844387076, 1.000000000000000000, 0.8660254037844387076, 1.000000000000000000, 0.9999962302473670572, 0.9999924607068793048 ) ) 
 REPRESENTATION_ITEM ( '' )  );
#18063 = FACE_OUTER_BOUND ( 'NONE', #26262, .T. ) ;
#18064 = CARTESIAN_POINT ( 'NONE',  ( -96.15314808468745866, -211.9973110713294489, 82.12864583420046927 ) ) ;
#18065 = ORIENTED_EDGE ( 'NONE', *, *, #72647, .T. ) ;
#18066 = LINE ( 'NONE', #28593, #47610 ) ;
#18067 = CARTESIAN_POINT ( 'NONE',  ( 5.000000000000002665, 71.87247863392414615, 39.47590169984871267 ) ) ;
#18068 = CARTESIAN_POINT ( 'NONE',  ( -94.99999999999997158, -207.3369185715606307, 75.51406250086714067 ) ) ;
#18069 = EDGE_CURVE ( 'NONE', #55521, #10549, #8948, .T. ) ;
#18070 = AXIS2_PLACEMENT_3D ( 'NONE', #33303, #5514, #56258 ) ;
#18071 = CARTESIAN_POINT ( 'NONE',  ( 0.000000000000000000, 0.000000000000000000, 0.000000000000000000 ) ) ;
#18072 = CARTESIAN_POINT ( 'NONE',  ( 12.49999999999999645, 1.530808498934191127E-15, 125.0000000000000000 ) ) ;
#18073 = AXIS2_PLACEMENT_3D ( 'NONE', #59853, #19243, #30883 ) ;
#18074 = ADVANCED_FACE ( 'NONE', ( #70735 ), #36902, .T. ) ;
#18075 = DIRECTION ( 'NONE',  ( 1.000000000000000000, 0.000000000000000000, 0.000000000000000000 ) ) ;
#18076 = EDGE_CURVE ( 'NONE', #57242, #52714, #29377, .T. ) ;
#18077 = LINE ( 'NONE', #68195, #20357 ) ;
#18078 = AXIS2_PLACEMENT_3D ( 'NONE', #30937, #24939, #53515 ) ;
#18079 = ADVANCED_FACE ( 'NONE', ( #25991 ), #59851, .T. ) ;
#18080 = CARTESIAN_POINT ( 'NONE',  ( -92.35000000000009379, 91.52997821335256390, 76.40041666666667197 ) ) ;
#18081 = DIRECTION ( 'NONE',  ( 0.000000000000000000, 0.000000000000000000, 1.000000000000000000 ) ) ;
#18082 = CARTESIAN_POINT ( 'NONE',  ( -96.15314808468752972, 91.99731107132950569, 76.83697916753381207 ) ) ;
#18083 = DIRECTION ( 'NONE',  ( -1.000000000000000000, 0.000000000000000000, -0.000000000000000000 ) ) ;
#18084 = DIRECTION ( 'NONE',  ( 0.000000000000000000, 0.000000000000000000, 1.000000000000000000 ) ) ;
#18085 = ADVANCED_FACE ( 'NONE', ( #2374 ), #30881, .F. ) ;
#18086 = ORIENTED_EDGE ( 'NONE', *, *, #50570, .T. ) ;
#18087 = CYLINDRICAL_SURFACE ( 'NONE', #34170, 16.00000000000000000 ) ;
#18088 = ADVANCED_FACE ( 'NONE', ( #31262 ), #33014, .T. ) ;
#18089 = DIRECTION ( 'NONE',  ( 0.000000000000000000, 0.9969173337331276308, 0.07845909572784874608 ) ) ;
#18090 = DIRECTION ( 'NONE',  ( -1.000000000000000000, -0.000000000000000000, -0.000000000000000000 ) ) ;
#18091 = CARTESIAN_POINT ( 'NONE',  ( 10.00000000000000000, -16.23288003029473359, -33.80338159004301701 ) ) ;
#18092 = DIRECTION ( 'NONE',  ( 0.000000000000000000, 0.000000000000000000, 1.000000000000000000 ) ) ;
#18093 = CARTESIAN_POINT ( 'NONE',  ( 5.999999999999998224, 0.000000000000000000, 0.000000000000000000 ) ) ;
#18094 = CARTESIAN_POINT ( 'NONE',  ( -96.15314808468745866, -211.9973110713294489, 76.57239583420049200 ) ) ;
#18095 = DIRECTION ( 'NONE',  ( -0.000000000000000000, -0.000000000000000000, 1.000000000000000000 ) ) ;
#18096 = ORIENTED_EDGE ( 'NONE', *, *, #17427, .T. ) ;
#18097 = CARTESIAN_POINT ( 'NONE',  ( 11.99999999999999822, 0.000000000000000000, 0.000000000000000000 ) ) ;
#18098 = EDGE_CURVE ( 'NONE', #38802, #42705, #48918, .T. ) ;
#18099 = EDGE_CURVE ( 'NONE', #35608, #71243, #60010, .T. ) ;
#18100 = CARTESIAN_POINT ( 'NONE',  ( 0.000000000000000000, 2.543863470248389103, 81.96053171279903893 ) ) ;
#18101 = CARTESIAN_POINT ( 'NONE',  ( -17.26469406256017791, -140.1601175325492648, 5.500000000000000000 ) ) ;
#18102 = DIRECTION ( 'NONE',  ( -1.000000000000000000, 0.000000000000000000, -0.000000000000000000 ) ) ;
#18103 = VECTOR ( 'NONE', #23446, 1000.000000000000000 ) ;
#18104 = EDGE_CURVE ( 'NONE', #25146, #23811, #53391, .T. ) ;
#18105 = EDGE_CURVE ( 'NONE', #64362, #21174, #63027, .T. ) ;
#18106 = PLANE ( 'NONE',  #12726 ) ;
#18107 = ORIENTED_EDGE ( 'NONE', *, *, #6731, .T. ) ;
#18108 = CARTESIAN_POINT ( 'NONE',  ( -10.00000000000000000, 0.000000000000000000, 0.000000000000000000 ) ) ;
#18109 = EDGE_CURVE ( 'NONE', #67219, #30790, #21555, .T. ) ;
#18110 = VERTEX_POINT ( 'NONE', #10845 ) ;
#18111 = CARTESIAN_POINT ( 'NONE',  ( 93.84685191531251292, -211.9973110713294489, 83.39864583420047950 ) ) ;
#18112 = CARTESIAN_POINT ( 'NONE',  ( -7.500000000000015099, -73.00000000000001421, -255.0000000000000000 ) ) ;
#18113 = ORIENTED_EDGE ( 'NONE', *, *, #43748, .T. ) ;
#18114 = CARTESIAN_POINT ( 'NONE',  ( -93.67500000000003979, 92.29496732002878900, 79.62833333333333030 ) ) ;
#18115 = AXIS2_PLACEMENT_3D ( 'NONE', #19539, #64677, #31190 ) ;
#18116 = ORIENTED_EDGE ( 'NONE', *, *, #47115, .F. ) ;
#18117 = CARTESIAN_POINT ( 'NONE',  ( 92.35000000000000853, -209.9999999999999716, 84.99937500173429328 ) ) ;
#18118 = VERTEX_POINT ( 'NONE', #34139 ) ;
#18119 = VECTOR ( 'NONE', #12769, 1000.000000000000000 ) ;
#18120 = CARTESIAN_POINT ( 'NONE',  ( -92.69370383062502583, 91.33154071421968467, 80.64697916753382856 ) ) ;
#18121 = AXIS2_PLACEMENT_3D ( 'NONE', #34232, #39887, #32731 ) ;
#18122 = VERTEX_POINT ( 'NONE', #4857 ) ;
#18123 = EDGE_LOOP ( 'NONE', ( #22762, #26755, #37911, #32636 ) ) ;
#18124 = CYLINDRICAL_SURFACE ( 'NONE', #441, 42.00000000000000000 ) ;
#18125 = ORIENTED_EDGE ( 'NONE', *, *, #57591, .T. ) ;
#18126 = DIRECTION ( 'NONE',  ( 0.000000000000000000, -1.000000000000000000, -0.000000000000000000 ) ) ;
#18127 = DIRECTION ( 'NONE',  ( -0.000000000000000000, -0.000000000000000000, -1.000000000000000000 ) ) ;
#18128 = VERTEX_POINT ( 'NONE', #63468 ) ;
#18129 = CARTESIAN_POINT ( 'NONE',  ( 96.32499999999998863, 87.70503267997126784, 80.76604166840097321 ) ) ;
#18130 = ORIENTED_EDGE ( 'NONE', *, *, #56958, .T. ) ;
#18131 = LINE ( 'NONE', #64004, #6019 ) ;
#18132 = ORIENTED_EDGE ( 'NONE', *, *, #70498, .F. ) ;
#18133 = ORIENTED_EDGE ( 'NONE', *, *, #66239, .F. ) ;
#18134 = VERTEX_POINT ( 'NONE', #5592 ) ;
#18135 = CARTESIAN_POINT ( 'NONE',  ( 96.15314808468748708, -208.0026889286704943, 81.17614583420048291 ) ) ;
#18136 = APPLICATION_PROTOCOL_DEFINITION ( 'draft international standard', 'automotive_design', 1998, #44125 ) ;
#18137 = CYLINDRICAL_SURFACE ( 'NONE', #31775, 3.000000000000000000 ) ;
#18138 = CYLINDRICAL_SURFACE ( 'NONE', #64079, 42.00000000000000000 ) ;
#18139 = CARTESIAN_POINT ( 'NONE',  ( -11.99999999999999645, 0.000000000000000000, -20.69999999999999929 ) ) ;
#18140 = CARTESIAN_POINT ( 'NONE',  ( 5.000000000000002665, 80.28980883073758434, 16.65972982744963460 ) ) ;
#18141 = CARTESIAN_POINT ( 'NONE',  ( -96.15314808468745866, -211.9973110713294489, 84.66864583420047552 ) ) ;
#18142 = CARTESIAN_POINT ( 'NONE',  ( -95.00000000000002842, 92.66308142843932671, 80.75281250086715090 ) ) ;
#18143 = VERTEX_POINT ( 'NONE', #33766 ) ;
#18144 = CARTESIAN_POINT ( 'NONE',  ( 93.84685191531248449, 91.99731107132950569, 83.18697916753382060 ) ) ;
#18145 = ORIENTED_EDGE ( 'NONE', *, *, #67148, .F. ) ;
#18146 = CARTESIAN_POINT ( 'NONE',  ( 10.00000000000000000, -55.19960302592029677, -51.03279382321147750 ) ) ;
#18147 = DIRECTION ( 'NONE',  ( 0.000000000000000000, 0.6691306063588675634, -0.7431448254773856954 ) ) ;
#18148 = CARTESIAN_POINT ( 'NONE',  ( 10.00000000000000000, 76.41127070299292257, -12.93880638057232346 ) ) ;
#18149 = DIRECTION ( 'NONE',  ( 0.000000000000000000, -0.3090169943749349057, -0.9510565162951576390 ) ) ;
#18150 = DIRECTION ( 'NONE',  ( -0.000000000000000000, -0.000000000000000000, 1.000000000000000000 ) ) ;
#18151 = CARTESIAN_POINT ( 'NONE',  ( -96.15314808468747287, -208.0026889286704943, 87.63197916753379957 ) ) ;
#18152 = CARTESIAN_POINT ( 'NONE',  ( 15.00000000000000000, 16.83928648764945635, 16.46020748918027010 ) ) ;
#18153 = VECTOR ( 'NONE', #52439, 1000.000000000000114 ) ;
#18154 = EDGE_CURVE ( 'NONE', #42672, #32448, #59404, .T. ) ;
#18155 = CYLINDRICAL_SURFACE ( 'NONE', #15759, 2.649999999999985700 ) ;
#18156 = CARTESIAN_POINT ( 'NONE',  ( 0.000000000000000000, 68.26794271651262136, 31.47745569255165066 ) ) ;
#18157 = VECTOR ( 'NONE', #43972, 1000.000000000000000 ) ;
#18158 = DIRECTION ( 'NONE',  ( -1.000000000000000000, 0.000000000000000000, -0.000000000000000000 ) ) ;
#18159 = EDGE_LOOP ( 'NONE', ( #33688, #45733, #61619, #27516 ) ) ;
#18160 = EDGE_CURVE ( 'NONE', #3179, #9784, #64182, .T. ) ;
#18161 = VERTEX_POINT ( 'NONE', #28123 ) ;
#18162 = EDGE_CURVE ( 'NONE', #37377, #232, #51802, .T. ) ;
#18163 = EDGE_CURVE ( 'NONE', #23521, #67020, #623, .T. ) ;
#18164 = CARTESIAN_POINT ( 'NONE',  ( -93.67500000000003979, 92.29496732002878900, 77.08833333333332405 ) ) ;
#18165 = CARTESIAN_POINT ( 'NONE',  ( 0.3000000000000016542, 0.000000000000000000, 4.700000000000000178 ) ) ;
#18166 = CARTESIAN_POINT ( 'NONE',  ( -96.15314808468752972, 91.99731107132950569, 86.99697916753380866 ) ) ;
#18167 = CARTESIAN_POINT ( 'NONE',  ( 96.32499999999998863, -207.7050326799711968, 80.89833333333332632 ) ) ;
#18168 = CARTESIAN_POINT ( 'NONE',  ( 10.00000000000000000, -64.81221759200306565, -50.23322058963418613 ) ) ;
#18169 = CARTESIAN_POINT ( 'NONE',  ( 10.00000000000000000, -30.84782396557201878, -21.32104025579148399 ) ) ;
#18170 = DIRECTION ( 'NONE',  ( -1.000000000000000000, -0.000000000000000000, -0.000000000000000000 ) ) ;
#18171 = ORIENTED_EDGE ( 'NONE', *, *, #70966, .F. ) ;
#18172 = CARTESIAN_POINT ( 'NONE',  ( -97.30629616937501680, 88.66845928578038638, 79.53572916753380184 ) ) ;
#18173 = CARTESIAN_POINT ( 'NONE',  ( 0.000000000000000000, 6.762365576493645669, -25.66652317338392209 ) ) ;
#18174 = DIRECTION ( 'NONE',  ( -1.000000000000000000, -0.000000000000000000, -0.000000000000000000 ) ) ;
#18175 = AXIS2_PLACEMENT_3D ( 'NONE', #43518, #70553, #3297 ) ;
#18176 = CARTESIAN_POINT ( 'NONE',  ( -12.50000000000000000, -107.5000000000000000, 40.00000000000000000 ) ) ;
#18177 = LINE ( 'NONE', #42234, #16503 ) ;
#18178 = CARTESIAN_POINT ( 'NONE',  ( -20.30386590532152979, -102.9045904027214959, 5.500000000000000000 ) ) ;
#18179 = CARTESIAN_POINT ( 'NONE',  ( -93.84685191531247028, -211.9973110713294489, 87.47322916753381605 ) ) ;
#18180 = PRESENTATION_STYLE_ASSIGNMENT (( #52384 ) ) ;
#18181 = VECTOR ( 'NONE', #73555, 1000.000000000000000 ) ;
#18182 = EDGE_CURVE ( 'NONE', #69810, #31889, #49877, .T. ) ;
#18183 = DIRECTION ( 'NONE',  ( 0.000000000000000000, 0.4067366430757887730, 0.9135454576426059736 ) ) ;
#18184 = CARTESIAN_POINT ( 'NONE',  ( 97.30629616937498838, 90.00000000000002842, 77.41906250086715602 ) ) ;
#18185 = CARTESIAN_POINT ( 'NONE',  ( -92.69370383062498320, -209.9999999999999716, 76.14906250086716000 ) ) ;
#18186 = DIRECTION ( 'NONE',  ( -1.000000000000000000, 0.000000000000000000, -0.000000000000000000 ) ) ;
#18187 = VERTEX_POINT ( 'NONE', #68369 ) ;
#18188 = DIRECTION ( 'NONE',  ( 0.000000000000000000, 0.000000000000000000, 1.000000000000000000 ) ) ;
#18189 = PLANE ( 'NONE',  #10597 ) ;
#18190 = CARTESIAN_POINT ( 'NONE',  ( 5.000000000000002665, 16.65972982744934683, 80.28980883073764119 ) ) ;
#18191 = EDGE_CURVE ( 'NONE', #23472, #31131, #28161, .T. ) ;
#18192 = ADVANCED_FACE ( 'NONE', ( #69461 ), #5965, .T. ) ;
#18193 = CARTESIAN_POINT ( 'NONE',  ( -97.30629616937501680, 88.66845928578038638, 76.51947916753381662 ) ) ;
#18194 = CARTESIAN_POINT ( 'NONE',  ( 92.69370383062501162, -211.3315407142195852, 78.26572916753380582 ) ) ;
#18195 = ORIENTED_EDGE ( 'NONE', *, *, #12391, .F. ) ;
#18196 = DIRECTION ( 'NONE',  ( -1.000000000000000000, 0.000000000000000000, 0.000000000000000000 ) ) ;
#18197 = ORIENTED_EDGE ( 'NONE', *, *, #29100, .F. ) ;
#18198 = DIRECTION ( 'NONE',  ( 0.000000000000000000, 0.07845909572783797692, 0.9969173337331285190 ) ) ;
#18199 = ORIENTED_EDGE ( 'NONE', *, *, #17265, .T. ) ;
#18200 = CIRCLE ( 'NONE', #44626, 16.00000000000000355 ) ;
#18202 = AXIS2_PLACEMENT_3D ( 'NONE', #49143, #32207, #21294 ) ;
#18201 = DIRECTION ( 'NONE',  ( -1.000000000000000000, 0.000000000000000000, -0.000000000000000000 ) ) ;
#18203 = VECTOR ( 'NONE', #7900, 1000.000000000000000 ) ;
#18204 = ORIENTED_EDGE ( 'NONE', *, *, #44205, .T. ) ;
#18205 = ORIENTED_EDGE ( 'NONE', *, *, #12579, .F. ) ;
#18206 = VERTEX_POINT ( 'NONE', #17222 ) ;
#18207 = DIRECTION ( 'NONE',  ( 0.000000000000000000, -0.000000000000000000, 1.000000000000000000 ) ) ;
#18208 = AXIS2_PLACEMENT_3D ( 'NONE', #46169, #24342, #34887 ) ;
#18209 = ORIENTED_EDGE ( 'NONE', *, *, #51777, .T. ) ;
#18210 = ORIENTED_EDGE ( 'NONE', *, *, #17931, .F. ) ;
#18211 = CARTESIAN_POINT ( 'NONE',  ( 93.84685191531248449, 91.99731107132950569, 84.61572916753381435 ) ) ;
#18212 = CARTESIAN_POINT ( 'NONE',  ( 90.00000000000000000, 95.00000000000002842, 90.00000000000000000 ) ) ;
#18213 = CARTESIAN_POINT ( 'NONE',  ( 95.00000000000000000, -206.9400435732949575, 75.23624999999999829 ) ) ;
#18214 = ORIENTED_EDGE ( 'NONE', *, *, #30146, .T. ) ;
#18215 = ORIENTED_EDGE ( 'NONE', *, *, #22515, .T. ) ;
#18216 = EDGE_LOOP ( 'NONE', ( #9846, #52235, #51969, #62930 ) ) ;
#18217 = ORIENTED_EDGE ( 'NONE', *, *, #26924, .T. ) ;
#18218 = DIRECTION ( 'NONE',  ( 0.000000000000000000, 0.000000000000000000, 1.000000000000000000 ) ) ;
#18219 = VECTOR ( 'NONE', #55697, 999.9999999999998863 ) ;
#18220 = EDGE_LOOP ( 'NONE', ( #20483, #48672, #14701, #64275 ) ) ;
#18221 = AXIS2_PLACEMENT_3D ( 'NONE', #45806, #33370, #68730 ) ;
#18222 = CARTESIAN_POINT ( 'NONE',  ( 0.000000000000000000, -120.0000000000000000, 42.00000000000000000 ) ) ;
#18223 = DIRECTION ( 'NONE',  ( 0.000000000000000000, 0.000000000000000000, 1.000000000000000000 ) ) ;
#18224 = DIRECTION ( 'NONE',  ( -1.000000000000000000, 0.000000000000000000, -0.000000000000000000 ) ) ;
#18225 = CARTESIAN_POINT ( 'NONE',  ( 23.41451323550360186, -132.5004227906269989, 5.500000000000000000 ) ) ;
#18226 = AXIS2_PLACEMENT_3D ( 'NONE', #64427, #13646, #70046 ) ;
#18227 = CARTESIAN_POINT ( 'NONE',  ( 97.65000000000000568, -209.9999753241869200, 87.22187585518551600 ) ) ;
#18228 = LINE ( 'NONE', #41167, #10773 ) ;
#18229 = CARTESIAN_POINT ( 'NONE',  ( 0.000000000000000000, -73.73191006444582740, 14.66109333815435889 ) ) ;
#18230 = CARTESIAN_POINT ( 'NONE',  ( -93.67499999999998295, -212.2949673200287179, 77.59104166840097605 ) ) ;
#18231 = VERTEX_POINT ( 'NONE', #16862 ) ;
#18232 = DIRECTION ( 'NONE',  ( 7.962523111839282146E-16, -1.065814103640130873E-14, -1.000000000000000000 ) ) ;
#18233 = EDGE_LOOP ( 'NONE', ( #20652, #2980, #73029, #35326 ) ) ;
#18235 = CARTESIAN_POINT ( 'NONE',  ( -95.00000000000002842, 93.05995642670501411, 77.22062500173429100 ) ) ;
#18234 = CARTESIAN_POINT ( 'NONE',  ( 92.34999999999999432, 90.00000000000002842, 78.64937500173429896 ) ) ;
#18236 = VERTEX_POINT ( 'NONE', #11940 ) ;
#18237 = CARTESIAN_POINT ( 'NONE',  ( 92.69370383062498320, 88.66845928578037217, 80.96447916753382401 ) ) ;
#18238 = DIRECTION ( 'NONE',  ( 0.000000000000000000, 0.7071067811865437980, 0.7071067811865512365 ) ) ;
#18239 = PRODUCT_RELATED_PRODUCT_CATEGORY ( 'part', '', ( #37366 ) ) ;
#18240 = LINE ( 'NONE', #35528, #65506 ) ;
#18241 = EDGE_CURVE ( 'NONE', #15423, #44183, #10463, .T. ) ;
#18242 = CARTESIAN_POINT ( 'NONE',  ( 11.99999999999999822, 6.903761155838878061, -77.19088730480517313 ) ) ;
#18243 = FACE_OUTER_BOUND ( 'NONE', #35695, .T. ) ;
#18244 = ORIENTED_EDGE ( 'NONE', *, *, #33938, .T. ) ;
#18245 = DIRECTION ( 'NONE',  ( 0.000000000000000000, 0.1564344650402244852, 0.9876883405951387696 ) ) ;
#18246 = CARTESIAN_POINT ( 'NONE',  ( -2.500000000000003997, 4.330127018922192761, -6.000000000000000000 ) ) ;
#18247 = ORIENTED_EDGE ( 'NONE', *, *, #35293, .F. ) ;
#18248 = EDGE_CURVE ( 'NONE', #7152, #32052, #7766, .T. ) ;
#18249 = ORIENTED_EDGE ( 'NONE', *, *, #11965, .F. ) ;
#18250 = ADVANCED_FACE ( 'NONE', ( #52165 ), #27758, .T. ) ;
#18251 = CARTESIAN_POINT ( 'NONE',  ( 10.00000000000000000, 38.55633173627010990, 16.65560815589424593 ) ) ;
#18252 = CARTESIAN_POINT ( 'NONE',  ( 0.000000000000000000, 0.000000000000000000, 0.000000000000000000 ) ) ;
#18253 = CARTESIAN_POINT ( 'NONE',  ( -97.30629616937497417, -208.6684592857803011, 76.41364583420049428 ) ) ;
#18254 = ADVANCED_FACE ( 'NONE', ( #39792 ), #51059, .T. ) ;
#18255 = ORIENTED_EDGE ( 'NONE', *, *, #11683, .F. ) ;
#18256 = AXIS2_PLACEMENT_3D ( 'NONE', #65421, #59772, #18787 ) ;
#18257 = FACE_OUTER_BOUND ( 'NONE', #44857, .T. ) ;
#18258 = DIRECTION ( 'NONE',  ( 1.000000000000000000, 0.000000000000000000, 0.000000000000000000 ) ) ;
#18259 = AXIS2_PLACEMENT_3D ( 'NONE', #51317, #46810, #46064 ) ;
#18260 = CARTESIAN_POINT ( 'NONE',  ( 0.000000000000000000, 0.000000000000000000, 0.000000000000000000 ) ) ;
#18261 = CARTESIAN_POINT ( 'NONE',  ( 10.00000000000000000, 25.88420570971438650, -27.13269053701069566 ) ) ;
#18262 = CARTESIAN_POINT ( 'NONE',  ( 92.34999999999999432, 90.00000000000002842, 85.55499999999999261 ) ) ;
#18263 = CARTESIAN_POINT ( 'NONE',  ( 11.59999999999999787, 1.420590287010929336E-15, -54.99999999999998579 ) ) ;
#18264 = DIRECTION ( 'NONE',  ( -0.000000000000000000, -0.000000000000000000, 1.000000000000000000 ) ) ;
#18265 = CARTESIAN_POINT ( 'NONE',  ( 10.00000000000000000, 70.52718814184260054, 26.02418014898334420 ) ) ;
#18266 = CARTESIAN_POINT ( 'NONE',  ( 19.12409105625795291, -101.5943176906707919, -5.500000000000000000 ) ) ;
#18267 = ADVANCED_FACE ( 'NONE', ( #22879 ), #48376, .F. ) ;
#18268 = FACE_OUTER_BOUND ( 'NONE', #44837, .T. ) ;
#18269 = AXIS2_PLACEMENT_3D ( 'NONE', #54497, #19534, #42486 ) ;
#18270 = EDGE_CURVE ( 'NONE', #55143, #73780, #6680, .T. ) ;
#18271 = AXIS2_PLACEMENT_3D ( 'NONE', #6585, #53549, #6937 ) ;
#18272 =( BOUNDED_CURVE ( )  B_SPLINE_CURVE ( 2, ( #1970, #42165, #48890, #65100, #13570, #25240, #71446 ),
 .UNSPECIFIED., .F., .F. ) 
 B_SPLINE_CURVE_WITH_KNOTS ( ( 3, 2, 2, 3 ),
 ( 0.6041666666666670737, 0.6111111111111116045, 0.6180555555555559133, 0.6250000000000003331 ),
 .UNSPECIFIED. ) 
 CURVE ( )  GEOMETRIC_REPRESENTATION_ITEM ( )  RATIONAL_B_SPLINE_CURVE ( ( 0.9999999999999914513, 0.8660254037844472563, 1.000000000000000000, 0.8660254037844387076, 1.000000000000000000, 0.8660254037844322683, 1.000000000000006439 ) ) 
 REPRESENTATION_ITEM ( '' )  );
#18273 = CARTESIAN_POINT ( 'NONE',  ( 96.15314808468748708, 91.99731107132950569, 87.68489583420048916 ) ) ;
#18274 = CARTESIAN_POINT ( 'NONE',  ( -93.84685191531247028, -211.9973110713294489, 85.56822916753381492 ) ) ;
#18275 = DIRECTION ( 'NONE',  ( 0.000000000000000000, 0.000000000000000000, -1.000000000000000000 ) ) ;
#18276 = ORIENTED_EDGE ( 'NONE', *, *, #17071, .T. ) ;
#18277 = CARTESIAN_POINT ( 'NONE',  ( 92.35000000046504454, -210.0000309987310061, 83.09538598081256566 ) ) ;
#18278 = CARTESIAN_POINT ( 'NONE',  ( -96.32499999999996021, -212.2949673200287179, 80.58083333333331666 ) ) ;
#18279 = CARTESIAN_POINT ( 'NONE',  ( -93.84685191531254134, 91.99731107132950569, 76.09614583420047040 ) ) ;
#18280 = EDGE_CURVE ( 'NONE', #21000, #2294, #55161, .T. ) ;
#18281 = CIRCLE ( 'NONE', #30294, 37.49900000000000233 ) ;
#18282 = CARTESIAN_POINT ( 'NONE',  ( 93.84685191531249870, -208.0026889286704943, 85.72697916753379843 ) ) ;
#18283 = ORIENTED_EDGE ( 'NONE', *, *, #34360, .F. ) ;
#18284 = ORIENTED_EDGE ( 'NONE', *, *, #1037, .F. ) ;
#18285 = CARTESIAN_POINT ( 'NONE',  ( 97.65000000000000568, 88.47002178664752137, 87.16895833506762870 ) ) ;
#18286 = ORIENTED_EDGE ( 'NONE', *, *, #51928, .T. ) ;
#18287 = DIRECTION ( 'NONE',  ( -1.000000000000000000, 0.000000000000000000, 0.000000000000000000 ) ) ;
#18288 = DIRECTION ( 'NONE',  ( 1.000000000000000000, -0.000000000000000000, 0.000000000000000000 ) ) ;
#18289 = ORIENTED_EDGE ( 'NONE', *, *, #28436, .F. ) ;
#18290 = VERTEX_POINT ( 'NONE', #18324 ) ;
#18291 = CARTESIAN_POINT ( 'NONE',  ( 92.69370383062501162, -209.9999999999999716, 80.27656250086714351 ) ) ;
#18292 = CARTESIAN_POINT ( 'NONE',  ( -2.499999999999997780, 8.494897427831771708, -10.00000000000000178 ) ) ;
#18293 = CARTESIAN_POINT ( 'NONE',  ( 97.64999999999999147, 90.00000000000002842, 80.79249999999998977 ) ) ;
#18294 = CARTESIAN_POINT ( 'NONE',  ( -23.54415474984308787, -120.4156646670583086, 5.500000000000000000 ) ) ;
#18295 = CYLINDRICAL_SURFACE ( 'NONE', #56178, 2.649999999999985700 ) ;
#18296 = CARTESIAN_POINT ( 'NONE',  ( 97.64999999999997726, -211.5299782133524502, 85.81958333333331268 ) ) ;
#18297 = EDGE_CURVE ( 'NONE', #2620, #16169, #10173, .T. ) ;
#18298 = EDGE_LOOP ( 'NONE', ( #3573, #21163, #64998, #42622 ) ) ;
#18299 = ORIENTED_EDGE ( 'NONE', *, *, #33440, .F. ) ;
#18300 = VERTEX_POINT ( 'NONE', #12313 ) ;
#18301 = VERTEX_POINT ( 'NONE', #29585 ) ;
#18302 = LINE ( 'NONE', #52896, #69454 ) ;
#18303 = AXIS2_PLACEMENT_3D ( 'NONE', #36225, #36594, #25329 ) ;
#18304 =( NAMED_UNIT ( * ) SI_UNIT ( $, .STERADIAN. ) SOLID_ANGLE_UNIT ( ) );
#18305 = CARTESIAN_POINT ( 'NONE',  ( -96.15314808468751551, 88.00268892867056536, 86.09739583420049769 ) ) ;
#18306 = DIRECTION ( 'NONE',  ( 1.000000000000000000, 0.000000000000000000, 0.000000000000000000 ) ) ;
#18307 = EDGE_CURVE ( 'NONE', #28408, #42171, #13045, .T. ) ;
#18308 = LINE ( 'NONE', #41251, #24583 ) ;
#18309 = CARTESIAN_POINT ( 'NONE',  ( 92.69370383062501162, -211.3315407142195852, 87.79072916753381151 ) ) ;
#18310 = CARTESIAN_POINT ( 'NONE',  ( 92.34999999999999432, 88.47002178664753558, 77.98791666666664923 ) ) ;
#18311 = EDGE_CURVE ( 'NONE', #38823, #18520, #54560, .T. ) ;
#18312 = VERTEX_POINT ( 'NONE', #31076 ) ;
#18313 = CARTESIAN_POINT ( 'NONE',  ( 97.64999999999999147, 90.00000000000002842, 79.52249999999999375 ) ) ;
#18314 = AXIS2_PLACEMENT_3D ( 'NONE', #14826, #32111, #42668 ) ;
#18315 = EDGE_LOOP ( 'NONE', ( #41329, #1462, #61379, #11004 ) ) ;
#18316 = DIRECTION ( 'NONE',  ( -0.000000000000000000, -0.000000000000000000, 1.000000000000000000 ) ) ;
#18317 = ORIENTED_EDGE ( 'NONE', *, *, #57732, .T. ) ;
#18318 = CARTESIAN_POINT ( 'NONE',  ( -93.67500000000003979, 87.70503267997129626, 89.02104166840096866 ) ) ;
#18319 = CARTESIAN_POINT ( 'NONE',  ( 97.30629616937498838, 91.33154071421968467, 89.53697916753382913 ) ) ;
#18320 = ORIENTED_EDGE ( 'NONE', *, *, #1254, .F. ) ;
#18321 = DIRECTION ( 'NONE',  ( -1.000000000000000000, -0.000000000000000000, -0.000000000000000000 ) ) ;
#18322 = ADVANCED_FACE ( 'NONE', ( #19426 ), #23979, .F. ) ;
#18323 = CARTESIAN_POINT ( 'NONE',  ( 15.00000000000000000, -18.13022148937263012, -15.02647892043543898 ) ) ;
#18324 = CARTESIAN_POINT ( 'NONE',  ( -92.35000000000006537, -209.9999992849074317, 85.31687502647974952 ) ) ;
#18325 = LINE ( 'NONE', #52532, #45553 ) ;
#18326 = ORIENTED_EDGE ( 'NONE', *, *, #69684, .T. ) ;
#18327 = CARTESIAN_POINT ( 'NONE',  ( -5.000000000000000000, -0.9724665692850904541, -5.958069561147902427 ) ) ;
#18328 = CIRCLE ( 'NONE', #57987, 31.99999999999999645 ) ;
#18329 = CIRCLE ( 'NONE', #35126, 37.49900000000000944 ) ;
#18330 = CARTESIAN_POINT ( 'NONE',  ( -96.15314808468747287, -208.0026889286704943, 74.93197916753379673 ) ) ;
#18331 = ORIENTED_EDGE ( 'NONE', *, *, #38217, .F. ) ;
#18332 = EDGE_LOOP ( 'NONE', ( #69923, #69346 ) ) ;
#18333 = FACE_OUTER_BOUND ( 'NONE', #7837, .T. ) ;
#18334 = CARTESIAN_POINT ( 'NONE',  ( -95.00000000002617639, -209.9999999999999432, -74.99999999999349143 ) ) ;
#18335 = DIRECTION ( 'NONE',  ( 0.000000000000000000, 0.8090169943749486725, -0.5877852522924714718 ) ) ;
#18336 = ORIENTED_EDGE ( 'NONE', *, *, #51082, .T. ) ;
#18337 = CARTESIAN_POINT ( 'NONE',  ( -93.84685191531248449, -208.0026889286704943, 88.95489583420049939 ) ) ;
#18338 = ORIENTED_EDGE ( 'NONE', *, *, #58926, .F. ) ;
#18339 = EDGE_CURVE ( 'NONE', #45327, #24118, #52203, .T. ) ;
#18340 = VERTEX_POINT ( 'NONE', #46912 ) ;
#18341 = VERTEX_POINT ( 'NONE', #41626 ) ;
#18342 = DIRECTION ( 'NONE',  ( 0.000000000000000000, 0.000000000000000000, 1.000000000000000000 ) ) ;
#18343 = DIRECTION ( 'NONE',  ( 0.9966891607226785466, 0.08130631524010119293, -0.000000000000000000 ) ) ;
#18344 = CARTESIAN_POINT ( 'NONE',  ( 94.99999999999998579, 87.33691857156068750, 81.54656250086713953 ) ) ;
#18345 = CARTESIAN_POINT ( 'NONE',  ( 11.99999999999999822, 75.11764819372142199, 2.946379043147685728 ) ) ;
#18346 = CARTESIAN_POINT ( 'NONE',  ( -95.00000000000002842, 93.05995642670504253, 80.39562500173430237 ) ) ;
#18347 = CARTESIAN_POINT ( 'NONE',  ( 22.08297821871651934, -111.8242998470044540, 5.500000000000000000 ) ) ;
#18348 = FACE_OUTER_BOUND ( 'NONE', #2489, .T. ) ;
#18349 = CARTESIAN_POINT ( 'NONE',  ( 12.13205353604972991, -140.1820037904669789, 2.500000000000000000 ) ) ;
#18350 = EDGE_CURVE ( 'NONE', #36873, #27913, #43800, .T. ) ;
#18351 = DIRECTION ( 'NONE',  ( 0.000000000000000000, 0.000000000000000000, 1.000000000000000000 ) ) ;
#18352 = CARTESIAN_POINT ( 'NONE',  ( 0.000000000000000000, 0.000000000000000000, 0.000000000000000000 ) ) ;
#18353 = EDGE_CURVE ( 'NONE', #65113, #28369, #41267, .T. ) ;
#18354 = EDGE_CURVE ( 'NONE', #9960, #73246, #58181, .T. ) ;
#18355 = CARTESIAN_POINT ( 'NONE',  ( 0.000000000000000000, -58.39081064771713869, -50.95692526931392052 ) ) ;
#18356 = AXIS2_PLACEMENT_3D ( 'NONE', #1355, #23494, #12935 ) ;
#18357 = CARTESIAN_POINT ( 'NONE',  ( 99.99999999999998579, 95.00000000000002842, 90.00000000000000000 ) ) ;
#18358 = CARTESIAN_POINT ( 'NONE',  ( -93.84685191531252713, 88.00268892867056536, 85.40947916753380298 ) ) ;
#18359 = DIRECTION ( 'NONE',  ( -0.9580045777625456616, -0.2867529058022021404, 0.000000000000000000 ) ) ;
#18360 = AXIS2_PLACEMENT_3D ( 'NONE', #17099, #40030, #27991 ) ;
#18361 = CARTESIAN_POINT ( 'NONE',  ( 5.999999999999999112, -21.60688246758642705, 79.10210256391358996 ) ) ;
#18362 = ORIENTED_EDGE ( 'NONE', *, *, #53751, .F. ) ;
#18363 = VECTOR ( 'NONE', #39335, 1000.000000000000000 ) ;
#18364 = DIRECTION ( 'NONE',  ( 0.000000000000000000, 0.4539904997395476927, -0.8910065241883674547 ) ) ;
#18365 = FACE_OUTER_BOUND ( 'NONE', #66509, .T. ) ;
#18366 = DIRECTION ( 'NONE',  ( -1.000000000000000000, -0.000000000000000000, -0.000000000000000000 ) ) ;
#18367 = DIRECTION ( 'NONE',  ( 0.000000000000000000, 0.000000000000000000, 1.000000000000000000 ) ) ;
#18368 = AXIS2_PLACEMENT_3D ( 'NONE', #35630, #7071, #46198 ) ;
#18369 = VECTOR ( 'NONE', #1116, 1000.000000000000000 ) ;
#18370 = CARTESIAN_POINT ( 'NONE',  ( 92.69370383062501162, -211.3315407142195852, 82.86947916753382515 ) ) ;
#18371 = ORIENTED_EDGE ( 'NONE', *, *, #30848, .F. ) ;
#18372 = ORIENTED_EDGE ( 'NONE', *, *, #48145, .T. ) ;
#18373 =( LENGTH_UNIT ( ) NAMED_UNIT ( * ) SI_UNIT ( .MILLI., .METRE. ) );
#18374 = ORIENTED_EDGE ( 'NONE', *, *, #35627, .T. ) ;
#18375 = CARTESIAN_POINT ( 'NONE',  ( 15.00000000000000000, -10.45096189432314127, 21.10159698893440350 ) ) ;
#18376 = CARTESIAN_POINT ( 'NONE',  ( 4.999999999999999112, 40.68715046381927891, 10.41901085202092858 ) ) ;
#18377 = ORIENTED_EDGE ( 'NONE', *, *, #25545, .F. ) ;
#18378 = CARTESIAN_POINT ( 'NONE',  ( 95.00000000000000000, -207.3369185715606307, 78.21281250086717307 ) ) ;
#18379 = EDGE_CURVE ( 'NONE', #35029, #67113, #35251, .T. ) ;
#18380 = ORIENTED_EDGE ( 'NONE', *, *, #69914, .F. ) ;
#18381 = CARTESIAN_POINT ( 'NONE',  ( -94.99999999999997158, -213.0599564267049857, 88.25374999999999659 ) ) ;
#18382 = ORIENTED_EDGE ( 'NONE', *, *, #7663, .F. ) ;
#18383 = ORIENTED_EDGE ( 'NONE', *, *, #29547, .T. ) ;
#18384 = DIRECTION ( 'NONE',  ( 0.000000000000000000, 0.9510565162951503115, -0.3090169943749573878 ) ) ;
#18385 = CARTESIAN_POINT ( 'NONE',  ( 0.000000000000000000, 1.530808498934191521E-15, -12.50000000000000000 ) ) ;
#18386 = EDGE_CURVE ( 'NONE', #8860, #72017, #19771, .T. ) ;
#18387 = ORIENTED_EDGE ( 'NONE', *, *, #31715, .F. ) ;
#18388 = DIRECTION ( 'NONE',  ( -1.000000000000000000, 0.000000000000000000, -0.000000000000000000 ) ) ;
#18389 = CARTESIAN_POINT ( 'NONE',  ( 93.67500000000001137, -212.2949673200287179, 86.37520833506764006 ) ) ;
#18390 = CARTESIAN_POINT ( 'NONE',  ( 94.99999999999998579, 93.05995642670504253, 87.30124999999999602 ) ) ;
#18391 = ADVANCED_FACE ( 'NONE', ( #64205 ), #24343, .T. ) ;
#18392 = ORIENTED_EDGE ( 'NONE', *, *, #6123, .T. ) ;
#18393 = DIRECTION ( 'NONE',  ( 1.000000000000000000, 0.000000000000000000, 0.000000000000000000 ) ) ;
#18394 = DIRECTION ( 'NONE',  ( 0.000000000000000000, 0.000000000000000000, 1.000000000000000000 ) ) ;
#18395 = AXIS2_PLACEMENT_3D ( 'NONE', #26206, #72437, #15300 ) ;
#18396 = ORIENTED_EDGE ( 'NONE', *, *, #47143, .F. ) ;
#18397 = ORIENTED_EDGE ( 'NONE', *, *, #28357, .T. ) ;
#18398 = DIRECTION ( 'NONE',  ( 0.000000000000000000, 0.000000000000000000, 1.000000000000000000 ) ) ;
#18399 = ORIENTED_EDGE ( 'NONE', *, *, #51550, .F. ) ;
#18400 = CARTESIAN_POINT ( 'NONE',  ( 94.99999999999998579, 93.05995642670504253, 84.84062500173429555 ) ) ;
#18401 = EDGE_CURVE ( 'NONE', #57350, #41695, #44974, .T. ) ;
#18402 = PRODUCT_DEFINITION_FORMATION_WITH_SPECIFIED_SOURCE ( 'ANY', '', #49365, .NOT_KNOWN. ) ;
#18403 = ORIENTED_EDGE ( 'NONE', *, *, #13483, .F. ) ;
#18404 = SHAPE_REPRESENTATION_RELATIONSHIP ( 'NONE' , 'NONE' ,  #42128, #3205 ) ;
#18405 = ORIENTED_EDGE ( 'NONE', *, *, #69497, .T. ) ;
#18406 = PLANE ( 'NONE',  #22520 ) ;
#18407 = CONTEXT_DEPENDENT_SHAPE_REPRESENTATION ( #60915, #42308 ) ;
#18408 = CARTESIAN_POINT ( 'NONE',  ( 10.00000000000000000, 12.42422080174639021, 35.38097989696516521 ) ) ;
#18409 = ORIENTED_EDGE ( 'NONE', *, *, #59924, .T. ) ;
#18410 = VECTOR ( 'NONE', #41323, 1000.000000000000000 ) ;
#18411 = VERTEX_POINT ( 'NONE', #42009 ) ;
#18412 = ORIENTED_EDGE ( 'NONE', *, *, #63922, .T. ) ;
#18413 = DIRECTION ( 'NONE',  ( -1.000000000000000000, 0.000000000000000000, 0.000000000000000000 ) ) ;
#18414 = DIRECTION ( 'NONE',  ( -0.000000000000000000, -0.000000000000000000, -1.000000000000000000 ) ) ;
#18415 = CARTESIAN_POINT ( 'NONE',  ( -93.67500000000003979, 87.70503267997129626, 86.40166666666667084 ) ) ;
#18416 = ORIENTED_EDGE ( 'NONE', *, *, #70585, .T. ) ;
#18417 = DIRECTION ( 'NONE',  ( -1.000000000000000000, -0.000000000000000000, -0.000000000000000000 ) ) ;
#18418 = VECTOR ( 'NONE', #70516, 1000.000000000000000 ) ;
#18419 = DIRECTION ( 'NONE',  ( -1.000000000000000000, 0.000000000000000000, 0.000000000000000000 ) ) ;
#18420 = ORIENTED_EDGE ( 'NONE', *, *, #67960, .T. ) ;
#18421 = LINE ( 'NONE', #31544, #52826 ) ;
#18422 = CARTESIAN_POINT ( 'NONE',  ( -96.15314808468747287, -208.0026889286704943, 83.18697916753382060 ) ) ;
#18423 = ORIENTED_EDGE ( 'NONE', *, *, #62568, .T. ) ;
#18424 = AXIS2_PLACEMENT_3D ( 'NONE', #9386, #32312, #22072 ) ;
#18426 = EDGE_CURVE ( 'NONE', #42081, #15645, #57043, .T. ) ;
#18425 = DIRECTION ( 'NONE',  ( -1.000000000000000000, 0.000000000000000000, 0.000000000000000000 ) ) ;
#18427 = CARTESIAN_POINT ( 'NONE',  ( 10.00000000000000000, 68.27212725128275395, -31.46837873495001503 ) ) ;
#18428 = CARTESIAN_POINT ( 'NONE',  ( 0.000000000000000000, -59.03961581697367933, -46.53671651294010303 ) ) ;
#18429 = CARTESIAN_POINT ( 'NONE',  ( -92.69370383062498320, -211.3315407142195852, 75.93739583420050110 ) ) ;
#18430 = DIRECTION ( 'NONE',  ( 0.000000000000000000, 0.000000000000000000, 1.000000000000000000 ) ) ;
#18431 = AXIS2_PLACEMENT_3D ( 'NONE', #49511, #72433, #20936 ) ;
#18432 = AXIS2_PLACEMENT_3D ( 'NONE', #30455, #47398, #19550 ) ;
#18433 = AXIS2_PLACEMENT_3D ( 'NONE', #52470, #7365, #52107 ) ;
#18434 = CYLINDRICAL_SURFACE ( 'NONE', #20525, 16.00000000000000000 ) ;
#18435 = CYLINDRICAL_SURFACE ( 'NONE', #21638, 82.00000000000000000 ) ;
#18436 = CARTESIAN_POINT ( 'NONE',  ( 0.000000000000000000, 0.000000000000000000, 0.000000000000000000 ) ) ;
#18437 = CARTESIAN_POINT ( 'NONE',  ( 0.000000000000000000, -49.70050353004931054, 59.46389618801946142 ) ) ;
#18438 = EDGE_CURVE ( 'NONE', #58910, #57911, #27284, .T. ) ;
#18439 = CARTESIAN_POINT ( 'NONE',  ( -93.84685191531252713, 88.00268892867056536, 79.05947916753380866 ) ) ;
#18440 = DIRECTION ( 'NONE',  ( 0.000000000000000000, -0.6494480483301903195, 0.7604059656000252687 ) ) ;
#18441 = FACE_OUTER_BOUND ( 'NONE', #29493, .T. ) ;
#18442 = EDGE_CURVE ( 'NONE', #35854, #73994, #671, .T. ) ;
#18443 = DIRECTION ( 'NONE',  ( 0.000000000000000000, -0.9510565162951510887, 0.3090169943749551673 ) ) ;
#18444 = CIRCLE ( 'NONE', #69833, 77.49899999999999523 ) ;
#18445 = DIRECTION ( 'NONE',  ( 0.000000000000000000, 0.000000000000000000, 1.000000000000000000 ) ) ;
#18446 = CYLINDRICAL_SURFACE ( 'NONE', #41851, 42.00000000000000000 ) ;
#18447 = LINE ( 'NONE', #64327, #29896 ) ;
#18448 = FACE_OUTER_BOUND ( 'NONE', #46424, .T. ) ;
#18449 = CARTESIAN_POINT ( 'NONE',  ( -97.65000000000003411, 89.99996406754254963, 85.63437624451402996 ) ) ;
#18450 = CARTESIAN_POINT ( 'NONE',  ( -93.84685191531248449, -208.0026889286704943, 74.98489583420048632 ) ) ;
#18451 = CARTESIAN_POINT ( 'NONE',  ( 14.59956846177685996, -138.4757300459248484, 5.500000000000000000 ) ) ;
#18452 = AXIS2_PLACEMENT_3D ( 'NONE', #25759, #30643, #1397 ) ;
#18453 = ORIENTED_EDGE ( 'NONE', *, *, #72287, .F. ) ;
#18454 = CARTESIAN_POINT ( 'NONE',  ( 10.00000000000000000, 17.67226234102826510, 33.17418723428314564 ) ) ;
#18455 = DIRECTION ( 'NONE',  ( -1.000000000000000000, -0.000000000000000000, -0.000000000000000000 ) ) ;
#18456 = CARTESIAN_POINT ( 'NONE',  ( 0.000000000000000000, 14.67089635893713684, 73.72996012237443608 ) ) ;
#18457 = DIRECTION ( 'NONE',  ( 1.000000000000000000, 0.000000000000000000, 0.000000000000000000 ) ) ;
#18458 = AXIS2_PLACEMENT_3D ( 'NONE', #45032, #44282, #51394 ) ;
#18459 = DIRECTION ( 'NONE',  ( 0.000000000000000000, 0.000000000000000000, 1.000000000000000000 ) ) ;
#18460 = VERTEX_POINT ( 'NONE', #14907 ) ;
#18461 = LINE ( 'NONE', #41405, #31097 ) ;
#18462 = DIRECTION ( 'NONE',  ( -0.000000000000000000, -0.000000000000000000, 1.000000000000000000 ) ) ;
#18463 = ORIENTED_EDGE ( 'NONE', *, *, #30279, .F. ) ;
#18464 = EDGE_CURVE ( 'NONE', #65294, #71076, #43129, .T. ) ;
#18465 = CIRCLE ( 'NONE', #42477, 0.9999999999999991118 ) ;
#18466 =( BOUNDED_CURVE ( )  B_SPLINE_CURVE ( 2, ( #59362, #37177, #60120, #31514, #37912, #43198, #8963 ),
 .UNSPECIFIED., .F., .F. ) 
 B_SPLINE_CURVE_WITH_KNOTS ( ( 3, 2, 2, 3 ),
 ( 0.4374999999999994449, 0.4444444444444441422, 0.4513888888888888951, 0.4583333333333335924 ),
 .UNSPECIFIED. ) 
 CURVE ( )  GEOMETRIC_REPRESENTATION_ITEM ( )  RATIONAL_B_SPLINE_CURVE ( ( 1.000000000000010658, 0.8660254037844280495, 1.000000000000000000, 0.8660254037844387076, 1.000000000000000000, 0.8660254037844333785, 1.000000000000005329 ) ) 
 REPRESENTATION_ITEM ( '' )  );
#18467 = CARTESIAN_POINT ( 'NONE',  ( 96.15314808468748708, -208.0026889286704943, 85.62114583420046188 ) ) ;
#18468 = CARTESIAN_POINT ( 'NONE',  ( 92.69370383062501162, -208.6684592857803295, 87.84364583420048689 ) ) ;
#18469 = CIRCLE ( 'NONE', #13696, 37.49900000000000944 ) ;
#18470 = ORIENTED_EDGE ( 'NONE', *, *, #60385, .F. ) ;
#18471 = EDGE_CURVE ( 'NONE', #22009, #63717, #31814, .T. ) ;
#18472 = DIRECTION ( 'NONE',  ( 0.000000000000000000, 0.000000000000000000, 1.000000000000000000 ) ) ;
#18473 = ORIENTED_EDGE ( 'NONE', *, *, #28803, .T. ) ;
#18474 = VECTOR ( 'NONE', #15210, 1000.000000000000000 ) ;
#18475 = CARTESIAN_POINT ( 'NONE',  ( 93.67500000000001137, -212.2949673200287179, 85.10520833506762983 ) ) ;
#18476 = ORIENTED_EDGE ( 'NONE', *, *, #46671, .T. ) ;
#18477 = CARTESIAN_POINT ( 'NONE',  ( -92.69370383062504004, 90.00000000000004263, 81.86406250086714920 ) ) ;
#18478 = EDGE_CURVE ( 'NONE', #19205, #57325, #24620, .T. ) ;
#18479 = VERTEX_POINT ( 'NONE', #19796 ) ;
#18480 = ORIENTED_EDGE ( 'NONE', *, *, #20763, .T. ) ;
#18481 = DIRECTION ( 'NONE',  ( -0.8774505977381983346, -0.4796670183876294291, 0.000000000000000000 ) ) ;
#18482 = EDGE_CURVE ( 'NONE', #42263, #65194, #53431, .T. ) ;
#18483 = ORIENTED_EDGE ( 'NONE', *, *, #9754, .T. ) ;
#18484 = CARTESIAN_POINT ( 'NONE',  ( -10.00000000000000000, 0.000000000000000000, 0.000000000000000000 ) ) ;
#18485 = FACE_OUTER_BOUND ( 'NONE', #18298, .T. ) ;
#18486 = VERTEX_POINT ( 'NONE', #20166 ) ;
#18487 = CARTESIAN_POINT ( 'NONE',  ( -92.35000000000003695, 90.00000000000004263, 75.71250000000000568 ) ) ;
#18488 = ORIENTED_EDGE ( 'NONE', *, *, #65963, .T. ) ;
#18489 =( BOUNDED_CURVE ( )  B_SPLINE_CURVE ( 2, ( #56445, #4956, #27855 ),
 .UNSPECIFIED., .F., .F. ) 
 B_SPLINE_CURVE_WITH_KNOTS ( ( 3, 3 ),
 ( 0.000000000000000000, 2.334341054613931057E-05 ),
 .UNSPECIFIED. ) 
 CURVE ( )  GEOMETRIC_REPRESENTATION_ITEM ( )  RATIONAL_B_SPLINE_CURVE ( ( 0.9459494467533609008, 0.9464399322878827014, 0.9469490141588213783 ) ) 
 REPRESENTATION_ITEM ( '' )  );
#18490 = EDGE_LOOP ( 'NONE', ( #59643, #59511, #20023, #46369 ) ) ;
#18491 = EDGE_CURVE ( 'NONE', #1246, #39261, #44228, .T. ) ;
#18492 = ORIENTED_EDGE ( 'NONE', *, *, #50859, .T. ) ;
#18493 = ORIENTED_EDGE ( 'NONE', *, *, #71995, .T. ) ;
#18494 = CARTESIAN_POINT ( 'NONE',  ( 93.84685191531251292, -211.9973110713294489, 81.49364583420047836 ) ) ;
#18495 = PRODUCT_CONTEXT ( 'NONE', #40285, 'mechanical' ) ;
#18496 = CARTESIAN_POINT ( 'NONE',  ( 6.000000000000000000, 15.33399622253482697, 80.55351364060595643 ) ) ;
#18497 = CARTESIAN_POINT ( 'NONE',  ( 10.00000000000000000, 0.000000000000000000, 0.000000000000000000 ) ) ;
#18498 = DIRECTION ( 'NONE',  ( -1.000000000000000000, 0.000000000000000000, 0.000000000000000000 ) ) ;
#18499 = DIRECTION ( 'NONE',  ( 0.000000000000000000, 0.000000000000000000, 1.000000000000000000 ) ) ;
#18500 = FACE_OUTER_BOUND ( 'NONE', #31880, .T. ) ;
#18501 = DIRECTION ( 'NONE',  ( 0.000000000000000000, 0.000000000000000000, 1.000000000000000000 ) ) ;
#18502 = CARTESIAN_POINT ( 'NONE',  ( -97.30629616937497417, -211.3315407142195852, 83.34572916753380412 ) ) ;
#18503 = CARTESIAN_POINT ( 'NONE',  ( -97.30629616937501680, 91.33154071421968467, 80.85864583420048746 ) ) ;
#18504 = EDGE_LOOP ( 'NONE', ( #38455, #32346, #43103, #22266 ) ) ;
#18505 = AXIS2_PLACEMENT_3D ( 'NONE', #25826, #71679, #15670 ) ;
#18506 = EDGE_CURVE ( 'NONE', #71848, #36383, #54719, .T. ) ;
#18507 = CARTESIAN_POINT ( 'NONE',  ( 93.84685191531248449, 91.99731107132950569, 81.28197916753380525 ) ) ;
#18508 = ORIENTED_EDGE ( 'NONE', *, *, #9435, .F. ) ;
#18509 = CARTESIAN_POINT ( 'NONE',  ( -3.000000000000000000, -3.948201729842038432, -23.21447184625298021 ) ) ;
#18511 = ADVANCED_FACE ( 'NONE', ( #9265 ), #52249, .F. ) ;
#18510 = LINE ( 'NONE', #18148, #63840 ) ;
#18512 = DIRECTION ( 'NONE',  ( -1.000000000000000000, -0.000000000000000000, 0.000000000000000000 ) ) ;
#18513 = PLANE ( 'NONE',  #56048 ) ;
#18514 = CARTESIAN_POINT ( 'NONE',  ( -97.30629616937495996, -209.9999999999999716, 85.83281250086714920 ) ) ;
#18515 = CARTESIAN_POINT ( 'NONE',  ( 5.000000000000002665, -80.28980883073747066, -16.65972982745018172 ) ) ;
#18516 = DIRECTION ( 'NONE',  ( 0.9918136447140101231, -0.1276937514489694114, 0.000000000000000000 ) ) ;
#18517 = CARTESIAN_POINT ( 'NONE',  ( 5.000000000000000000, -26.79245525562738095, 32.34446384429961796 ) ) ;
#18518 = EDGE_CURVE ( 'NONE', #2055, #8165, #55127, .T. ) ;
#18519 = DIRECTION ( 'NONE',  ( -0.000000000000000000, -0.000000000000000000, -1.000000000000000000 ) ) ;
#18520 = VERTEX_POINT ( 'NONE', #54761 ) ;
#18521 = VECTOR ( 'NONE', #9800, 1000.000000000000000 ) ;
#18522 = ORIENTED_EDGE ( 'NONE', *, *, #51104, .T. ) ;
#18523 = CARTESIAN_POINT ( 'NONE',  ( 2.499999999999984457, -73.00000000000001421, -258.2999999999999545 ) ) ;
#18524 = CARTESIAN_POINT ( 'NONE',  ( -3.000000000000002665, 0.000000000000000000, 0.000000000000000000 ) ) ;
#18525 = ADVANCED_FACE ( 'NONE', ( #37107 ), #32559, .T. ) ;
#18526 = CARTESIAN_POINT ( 'NONE',  ( -96.15314808468752972, 91.99731107132950569, 87.63197916753379957 ) ) ;
#18527 = DIRECTION ( 'NONE',  ( -1.000000000000000000, 0.000000000000000000, 0.000000000000000000 ) ) ;
#18528 = CARTESIAN_POINT ( 'NONE',  ( 0.000000000000000000, -81.90746397400386059, -3.894527615418766242 ) ) ;
#18529 = DIRECTION ( 'NONE',  ( -1.000000000000000000, -0.000000000000000000, -0.000000000000000000 ) ) ;
#18530 = CIRCLE ( 'NONE', #48520, 31.99999999999998934 ) ;
#18531 = CYLINDRICAL_SURFACE ( 'NONE', #67265, 31.99999999999998579 ) ;
#18532 = AXIS2_PLACEMENT_3D ( 'NONE', #12448, #24478, #52309 ) ;
#18533 = ORIENTED_EDGE ( 'NONE', *, *, #35725, .T. ) ;
#18534 = FACE_OUTER_BOUND ( 'NONE', #25258, .T. ) ;
#18535 = EDGE_CURVE ( 'NONE', #56042, #10200, #26554, .T. ) ;
#18536 = CIRCLE ( 'NONE', #60568, 0.2999999999999981570 ) ;
#18537 = AXIS2_PLACEMENT_3D ( 'NONE', #385, #16898, #23281 ) ;
#18538 = DIRECTION ( 'NONE',  ( 0.000000000000000000, 0.7431448254773862505, -0.6691306063588671194 ) ) ;
#18539 = FACE_OUTER_BOUND ( 'NONE', #21260, .T. ) ;
#18540 = DIRECTION ( 'NONE',  ( 0.000000000000000000, -0.9135454576426055295, -0.4067366430757899942 ) ) ;
#18541 = FACE_OUTER_BOUND ( 'NONE', #7113, .T. ) ;
#18542 = CARTESIAN_POINT ( 'NONE',  ( -94.99999999999997158, -207.3369185715606307, 87.73781250086715033 ) ) ;
#18543 = SHAPE_REPRESENTATION_RELATIONSHIP ( 'NONE' , 'NONE' ,  #36835, #58845 ) ;
#18544 = CIRCLE ( 'NONE', #60575, 82.00000000000000000 ) ;
#18545 = DIRECTION ( 'NONE',  ( 0.000000000000000000, 0.000000000000000000, -1.000000000000000000 ) ) ;
#18546 = AXIS2_PLACEMENT_3D ( 'NONE', #70604, #65371, #52588 ) ;
#18547 = CARTESIAN_POINT ( 'NONE',  ( 0.000000000000000000, -41.76937507738745836, -62.50329211542482710 ) ) ;
#18548 = AXIS2_PLACEMENT_3D ( 'NONE', #1995, #13959, #20354 ) ;
#18549 = CARTESIAN_POINT ( 'NONE',  ( -92.69370383062498320, -208.6684592857803295, 75.56697916753383026 ) ) ;
#18550 = DIRECTION ( 'NONE',  ( -1.000000000000000000, 0.000000000000000000, -0.000000000000000000 ) ) ;
#18551 = ORIENTED_EDGE ( 'NONE', *, *, #19439, .T. ) ;
#18552 = CARTESIAN_POINT ( 'NONE',  ( 21.85433023846371370, -135.0628101570779620, 5.500000000000000000 ) ) ;
#18553 = CARTESIAN_POINT ( 'NONE',  ( 0.000000000000000000, 54.21277698773675979, 55.38113227695801299 ) ) ;
#18554 = CARTESIAN_POINT ( 'NONE',  ( 95.00000000002597744, 90.00000000000007105, -75.00000000000000000 ) ) ;
#18555 = CARTESIAN_POINT ( 'NONE',  ( -96.15314808468751551, 88.00268892867056536, 75.93739583420048689 ) ) ;
#18556 = CARTESIAN_POINT ( 'NONE',  ( 92.69370383062501162, -209.9999999999999716, 76.30781250086714351 ) ) ;
#18557 = ORIENTED_EDGE ( 'NONE', *, *, #26560, .F. ) ;
#18558 = CYLINDRICAL_SURFACE ( 'NONE', #6704, 77.49899999999999523 ) ;
#18559 = ORIENTED_EDGE ( 'NONE', *, *, #41656, .F. ) ;
#18560 = DIRECTION ( 'NONE',  ( -0.000000000000000000, -0.000000000000000000, 1.000000000000000000 ) ) ;
#18561 = ORIENTED_EDGE ( 'NONE', *, *, #60726, .T. ) ;
#18562 = EDGE_CURVE ( 'NONE', #44941, #15992, #4022, .T. ) ;
#18563 = CARTESIAN_POINT ( 'NONE',  ( 10.00000000000000000, 22.64427369931212297, -30.00120703465181293 ) ) ;
#18564 = AXIS2_PLACEMENT_3D ( 'NONE', #56704, #67971, #16847 ) ;
#18565 = EDGE_CURVE ( 'NONE', #30584, #55375, #26920, .T. ) ;
#18566 = VERTEX_POINT ( 'NONE', #60055 ) ;
#18567 = ORIENTED_EDGE ( 'NONE', *, *, #56601, .T. ) ;
#18569 = ORIENTED_EDGE ( 'NONE', *, *, #32978, .F. ) ;
#18568 = EDGE_CURVE ( 'NONE', #19673, #41269, #38588, .T. ) ;
#18570 = EDGE_CURVE ( 'NONE', #18520, #38823, #63070, .T. ) ;
#18571 = ORIENTED_EDGE ( 'NONE', *, *, #16990, .F. ) ;
#18572 = VERTEX_POINT ( 'NONE', #33294 ) ;
#18573 = CARTESIAN_POINT ( 'NONE',  ( 96.15314808468748708, 91.99731107132950569, 78.79489583420048859 ) ) ;
#18574 = VECTOR ( 'NONE', #64706, 1000.000000000000000 ) ;
#18575 = CARTESIAN_POINT ( 'NONE',  ( 22.94323693612312809, -114.6983135802921083, 5.500000000000000000 ) ) ;
#18577 = FACE_OUTER_BOUND ( 'NONE', #66580, .T. ) ;
#18576 = AXIS2_PLACEMENT_3D ( 'NONE', #45982, #68907, #35059 ) ;
#18578 = VERTEX_POINT ( 'NONE', #57001 ) ;
#18579 = ORIENTED_EDGE ( 'NONE', *, *, #49535, .T. ) ;
#18580 = ORIENTED_EDGE ( 'NONE', *, *, #12819, .F. ) ;
#18581 = CARTESIAN_POINT ( 'NONE',  ( 11.99999999999999822, -35.91791733033525702, 68.67312586194982771 ) ) ;
#18582 = EDGE_LOOP ( 'NONE', ( #38224, #8322, #960, #31703 ) ) ;
#18583 = CIRCLE ( 'NONE', #6582, 31.99999999999998934 ) ;
#18584 = SHAPE_REPRESENTATION_RELATIONSHIP ( 'NONE' , 'NONE' ,  #33525, #37264 ) ;
#18585 = DIRECTION ( 'NONE',  ( -1.000000000000000000, 0.000000000000000000, 0.000000000000000000 ) ) ;
#18586 = CYLINDRICAL_SURFACE ( 'NONE', #2736, 16.00000000000000000 ) ;
#18587 = EDGE_CURVE ( 'NONE', #40037, #40781, #71443, .T. ) ;
#18588 = CARTESIAN_POINT ( 'NONE',  ( 0.000000000000000000, -35.38097989696503021, -12.42422080174676147 ) ) ;
#18589 = DIRECTION ( 'NONE',  ( 0.000000000000000000, 0.000000000000000000, -1.000000000000000000 ) ) ;
#18590 = LINE ( 'NONE', #23500, #22811 ) ;
#18591 = EDGE_CURVE ( 'NONE', #57700, #66667, #70070, .T. ) ;
#18592 = CARTESIAN_POINT ( 'NONE',  ( 10.00000000000000000, -11.30684508768395524, 76.66974797899831628 ) ) ;
#18593 = CARTESIAN_POINT ( 'NONE',  ( -96.32499999999996021, -212.2949673200287179, 80.66020833506763665 ) ) ;
#18594 = LINE ( 'NONE', #59199, #50690 ) ;
#18595 = VERTEX_POINT ( 'NONE', #46084 ) ;
#18597 = CARTESIAN_POINT ( 'NONE',  ( -97.65000000000001990, 90.00000000000004263, 77.37937500173428873 ) ) ;
#18596 = CARTESIAN_POINT ( 'NONE',  ( 97.64999999999996305, 88.93103996628909158, 74.48490336299444436 ) ) ;
#18598 = ORIENTED_EDGE ( 'NONE', *, *, #11879, .F. ) ;
#18599 = CARTESIAN_POINT ( 'NONE',  ( 92.69370383062498320, 91.33154071421968467, 78.95364583420048632 ) ) ;
#18600 = CARTESIAN_POINT ( 'NONE',  ( 92.34999999999999432, 90.00000000000002842, 90.00000000000000000 ) ) ;
#18601 = DIRECTION ( 'NONE',  ( 0.000000000000000000, -0.8526401643540970632, 0.5224985647159410274 ) ) ;
#18602 = AXIS2_PLACEMENT_3D ( 'NONE', #29142, #22031, #74274 ) ;
#18603 = CARTESIAN_POINT ( 'NONE',  ( -97.64999999996715019, 90.00000839192523472, 86.90410584365564262 ) ) ;
#18604 = DIRECTION ( 'NONE',  ( 0.000000000000000000, -0.5877852522924689183, 0.8090169943749504489 ) ) ;
#18605 = ORIENTED_EDGE ( 'NONE', *, *, #65880, .F. ) ;
#18606 = CARTESIAN_POINT ( 'NONE',  ( -92.35000000000003695, 90.00000015433754186, 79.60187500750917877 ) ) ;
#18607 = EDGE_CURVE ( 'NONE', #61409, #27461, #11488, .T. ) ;
#18608 = EDGE_CURVE ( 'NONE', #35348, #22766, #5873, .T. ) ;
#18609 = FACE_OUTER_BOUND ( 'NONE', #62239, .T. ) ;
#18610 = VERTEX_POINT ( 'NONE', #27671 ) ;
#18611 = CIRCLE ( 'NONE', #18649, 31.99999999999998934 ) ;
#18612 = ORIENTED_EDGE ( 'NONE', *, *, #54268, .T. ) ;
#18613 =( BOUNDED_CURVE ( )  B_SPLINE_CURVE ( 2, ( #21497, #68119, #34269, #51188, #44454, #22630, #61745 ),
 .UNSPECIFIED., .F., .F. ) 
 B_SPLINE_CURVE_WITH_KNOTS ( ( 3, 2, 2, 3 ),
 ( 0.8466920362367555963, 0.8537476304467667143, 0.8608033959876489893, 0.8678591737214816915 ),
 .UNSPECIFIED. ) 
 CURVE ( )  GEOMETRIC_REPRESENTATION_ITEM ( )  RATIONAL_B_SPLINE_CURVE ( ( 0.9999934937104166810, 0.8660286570082263990, 1.000000000000000000, 0.8660254037844387076, 1.000000000000000000, 0.8660254037844387076, 1.000000000000000000 ) ) 
 REPRESENTATION_ITEM ( '' )  );
#18614 = CARTESIAN_POINT ( 'NONE',  ( 0.000000000000000000, 0.000000000000000000, 0.000000000000000000 ) ) ;
#18615 = DIRECTION ( 'NONE',  ( -0.000000000000000000, -0.000000000000000000, 1.000000000000000000 ) ) ;
#18616 = CARTESIAN_POINT ( 'NONE',  ( 10.00000000000000000, 35.47612816024523141, 22.48208911017513145 ) ) ;
#18617 = CARTESIAN_POINT ( 'NONE',  ( -96.15314808468747287, -208.0026889286704943, 77.63072916753381492 ) ) ;
#18618 = EDGE_LOOP ( 'NONE', ( #66123, #19249, #6820, #38831 ) ) ;
#18619 = DIRECTION ( 'NONE',  ( 0.000000000000000000, -0.8910065241883721177, 0.4539904997395382003 ) ) ;
#18620 = CIRCLE ( 'NONE', #60658, 13.36666666666666536 ) ;
#18621 = CARTESIAN_POINT ( 'NONE',  ( 0.000000000000000000, -12.42422080174614862, -35.38097989696524337 ) ) ;
#18622 = DIRECTION ( 'NONE',  ( -1.000000000000000000, 0.000000000000000000, 0.000000000000000000 ) ) ;
#18623 = DIRECTION ( 'NONE',  ( 1.000000000000000000, 0.000000000000000000, 0.000000000000000000 ) ) ;
#18624 = DIRECTION ( 'NONE',  ( 0.7533909544171996098, 0.6575728627325955200, -7.625282249115660656E-32 ) ) ;
#18625 = DIRECTION ( 'NONE',  ( -1.000000000000000000, 0.000000000000000000, -0.000000000000000000 ) ) ;
#18626 = DIRECTION ( 'NONE',  ( 0.000000000000000000, 0.3090169943749480064, -0.9510565162951534202 ) ) ;
#18627 = CARTESIAN_POINT ( 'NONE',  ( -96.32499999999996021, -212.2949673200287179, 85.10520833506762983 ) ) ;
#18628 = DIRECTION ( 'NONE',  ( -1.343011723336883198E-16, 1.000000000000000000, 0.000000000000000000 ) ) ;
#18629 = DIRECTION ( 'NONE',  ( 0.000000000000000000, 0.3090169943749480064, -0.9510565162951534202 ) ) ;
#18630 = AXIS2_PLACEMENT_3D ( 'NONE', #73390, #66658, #73011 ) ;
#18631 = AXIS2_PLACEMENT_3D ( 'NONE', #10928, #1177, #40992 ) ;
#18632 = CARTESIAN_POINT ( 'NONE',  ( 94.99999999999998579, 87.33691857156068750, 83.61031250086715261 ) ) ;
#18633 = CARTESIAN_POINT ( 'NONE',  ( -92.69370383062498320, -209.9999999999999716, 88.21406250086714351 ) ) ;
#18634 = DIRECTION ( 'NONE',  ( 1.000000000000000000, 0.000000000000000000, 0.000000000000000000 ) ) ;
#18635 = EDGE_LOOP ( 'NONE', ( #29830, #23329, #68263, #7300 ) ) ;
#18636 = CARTESIAN_POINT ( 'NONE',  ( -97.64999999999994884, -211.5299782133524502, 82.43291666666665662 ) ) ;
#18637 = CARTESIAN_POINT ( 'NONE',  ( -97.30629616937501680, 91.33154071421968467, 75.61989583420047722 ) ) ;
#18638 = VECTOR ( 'NONE', #66465, 1000.000000000000000 ) ;
#18639 = AXIS2_PLACEMENT_3D ( 'NONE', #7065, #1839, #40926 ) ;
#18640 = CARTESIAN_POINT ( 'NONE',  ( 97.30629616937498838, -209.9999999999999716, 85.51531250086713953 ) ) ;
#18641 = ORIENTED_EDGE ( 'NONE', *, *, #30393, .T. ) ;
#18642 =( REPRESENTATION_RELATIONSHIP ('NONE','NONE', #31117, #27826 ) REPRESENTATION_RELATIONSHIP_WITH_TRANSFORMATION ( #37656 )SHAPE_REPRESENTATION_RELATIONSHIP( ) );
#18643 = ORIENTED_EDGE ( 'NONE', *, *, #57470, .F. ) ;
#18644 = AXIS2_PLACEMENT_3D ( 'NONE', #3569, #20829, #20468 ) ;
#18645 = ORIENTED_EDGE ( 'NONE', *, *, #33530, .T. ) ;
#18646 = CARTESIAN_POINT ( 'NONE',  ( 0.000000000000000000, -35.47612816024539484, 22.48208911017487921 ) ) ;
#18647 = CYLINDRICAL_SURFACE ( 'NONE', #4271, 3.299999999999997158 ) ;
#18648 = ADVANCED_FACE ( 'NONE', ( #34416 ), #45352, .T. ) ;
#18649 = AXIS2_PLACEMENT_3D ( 'NONE', #13720, #36286, #59987 ) ;
#18650 = VERTEX_POINT ( 'NONE', #39332 ) ;
#18651 = ORIENTED_EDGE ( 'NONE', *, *, #30135, .F. ) ;
#18652 = DIRECTION ( 'NONE',  ( 0.000000000000000000, 0.000000000000000000, 1.000000000000000000 ) ) ;
#18653 = ADVANCED_FACE ( 'NONE', ( #63379 ), #62269, .T. ) ;
#18654 = CARTESIAN_POINT ( 'NONE',  ( 92.69370383062501162, -209.9999999999999716, 83.45156250086715488 ) ) ;
#18655 = CARTESIAN_POINT ( 'NONE',  ( 10.00000000000000000, -81.50828551894232987, 8.966570791700396725 ) ) ;
#18656 = DIRECTION ( 'NONE',  ( -1.000000000000000000, 0.000000000000000000, 0.000000000000000000 ) ) ;
#18657 = CARTESIAN_POINT ( 'NONE',  ( 5.000000000000000000, 1.831554690317580780, -1.158389257021584795 ) ) ;
#18658 = DIRECTION ( 'NONE',  ( -1.000000000000000000, -0.000000000000000000, -0.000000000000000000 ) ) ;
#18659 = ADVANCED_FACE ( 'NONE', ( #73151 ), #16016, .T. ) ;
#18660 = CYLINDRICAL_SURFACE ( 'NONE', #12962, 82.00000000000000000 ) ;
#18661 = CARTESIAN_POINT ( 'NONE',  ( 96.32499999999998863, -207.7050326799711968, 83.43833333333333258 ) ) ;
#18662 = ORIENTED_EDGE ( 'NONE', *, *, #2011, .T. ) ;
#18663 = VERTEX_POINT ( 'NONE', #73896 ) ;
#18664 = EDGE_LOOP ( 'NONE', ( #55512, #45638, #37758, #22366, #22130, #37936, #31456 ) ) ;
#18665 = ORIENTED_EDGE ( 'NONE', *, *, #22497, .T. ) ;
#18666 = CARTESIAN_POINT ( 'NONE',  ( 0.000000000000000000, 59.03961581697465277, -46.53671651293886669 ) ) ;
#18667 = CARTESIAN_POINT ( 'NONE',  ( -93.84685191531254134, 91.99731107132950569, 88.31989583420048007 ) ) ;
#18668 = CARTESIAN_POINT ( 'NONE',  ( 10.00000000000000000, 0.000000000000000000, 0.000000000000000000 ) ) ;
#18669 = DIRECTION ( 'NONE',  ( 1.000000000000000000, -0.000000000000000000, -0.000000000000000000 ) ) ;
#18670 = CARTESIAN_POINT ( 'NONE',  ( 96.90829146052659837, -211.8387288276635729, 74.44346887015069569 ) ) ;
#18671 = CARTESIAN_POINT ( 'NONE',  ( 92.34999999999999432, 91.52997821335252127, 78.51708333333334622 ) ) ;
#18672 = EDGE_CURVE ( 'NONE', #19363, #33442, #51719, .T. ) ;
#18673 = ORIENTED_EDGE ( 'NONE', *, *, #41249, .F. ) ;
#18674 = CARTESIAN_POINT ( 'NONE',  ( 96.32499999999997442, 92.29496732002878900, 79.62833333333333030 ) ) ;
#18675 = EDGE_LOOP ( 'NONE', ( #44595, #47616, #37190, #11708 ) ) ;
#18676 = EDGE_CURVE ( 'NONE', #67705, #54680, #10377, .T. ) ;
#18677 = CARTESIAN_POINT ( 'NONE',  ( -97.64999999999996305, -209.9999999999999716, 84.92000000000000171 ) ) ;
#18678 = ORIENTED_EDGE ( 'NONE', *, *, #68054, .F. ) ;
#18679 = CARTESIAN_POINT ( 'NONE',  ( -92.35000000000005116, 91.52997821335253548, 86.63979166840097434 ) ) ;
#18680 = CARTESIAN_POINT ( 'NONE',  ( 94.99999999999998579, 87.33691857156068750, 76.46656250086712703 ) ) ;
#18681 = AXIS2_PLACEMENT_3D ( 'NONE', #10002, #47554, #63377 ) ;
#18682 = ORIENTED_EDGE ( 'NONE', *, *, #49704, .F. ) ;
#18683 = DIRECTION ( 'NONE',  ( -1.000000000000000000, 0.000000000000000000, 0.000000000000000000 ) ) ;
#18684 = DIRECTION ( 'NONE',  ( 0.000000000000000000, 0.000000000000000000, -1.000000000000000000 ) ) ;
#18685 = DIRECTION ( 'NONE',  ( -1.000000000000000000, 0.000000000000000000, 0.000000000000000000 ) ) ;
#18686 = CARTESIAN_POINT ( 'NONE',  ( 11.99999999999999822, 26.02418014898310261, 70.52718814184268581 ) ) ;
#18687 = EDGE_LOOP ( 'NONE', ( #37980, #29383, #13741, #25335 ) ) ;
#18688 = CARTESIAN_POINT ( 'NONE',  ( 2.287832656137188447, -4.452621892014642313, -5.999999999999999112 ) ) ;
#18689 = AXIS2_PLACEMENT_3D ( 'NONE', #10357, #16371, #33275 ) ;
#18690 = ADVANCED_FACE ( 'NONE', ( #6243 ), #33679, .T. ) ;
#18691 = ADVANCED_FACE ( 'NONE', ( #21656 ), #67902, .T. ) ;
#18692 = CARTESIAN_POINT ( 'NONE',  ( -16.06301359042743115, -102.7814171781257357, 5.500000000000000000 ) ) ;
#18693 = ORIENTED_EDGE ( 'NONE', *, *, #22703, .T. ) ;
#18694 = ORIENTED_EDGE ( 'NONE', *, *, #42771, .F. ) ;
#18696 = DIRECTION ( 'NONE',  ( 0.000000000000000000, -0.7604059656000368150, 0.6494480483301767748 ) ) ;
#18695 = AXIS2_PLACEMENT_3D ( 'NONE', #22810, #12974, #52848 ) ;
#18697 = DIRECTION ( 'NONE',  ( 0.000000000000000000, -0.9969173337331287410, 0.07845909572783489605 ) ) ;
#18698 = VECTOR ( 'NONE', #69298, 1000.000000000000000 ) ;
#18699 = CIRCLE ( 'NONE', #5537, 42.00000000000000000 ) ;
#18700 = PLANE ( 'NONE',  #19679 ) ;
#18701 = EDGE_LOOP ( 'NONE', ( #63607, #5987, #39483, #5834 ) ) ;
#18702 =( BOUNDED_CURVE ( )  B_SPLINE_CURVE ( 2, ( #46800, #28100, #24238, #24592, #53537, #47894, #69715, #45417, #62721 ),
 .UNSPECIFIED., .F., .F. ) 
 B_SPLINE_CURVE_WITH_KNOTS ( ( 3, 2, 2, 2, 3 ),
 ( 0.5291824299508929297, 0.5362381811070600079, 0.5432939466479423940, 0.5503497121888247801, 0.5503499107226623721 ),
 .UNSPECIFIED. ) 
 CURVE ( )  GEOMETRIC_REPRESENTATION_ITEM ( )  RATIONAL_B_SPLINE_CURVE ( ( 1.000000000000000000, 0.8660254037844387076, 1.000000000000000000, 0.8660254037844387076, 1.000000000000000000, 0.8660254037844387076, 1.000000000000000000, 0.9999962302473670572, 0.9999924607068793048 ) ) 
 REPRESENTATION_ITEM ( '' )  );
#18703 = CARTESIAN_POINT ( 'NONE',  ( -93.84685191531248449, -208.0026889286704943, 88.31989583420048007 ) ) ;
#18704 = ORIENTED_EDGE ( 'NONE', *, *, #36170, .T. ) ;
#18705 = DIRECTION ( 'NONE',  ( -1.000000000000000000, 0.000000000000000000, 0.000000000000000000 ) ) ;
#18706 = VERTEX_POINT ( 'NONE', #5133 ) ;
#18707 = ORIENTED_EDGE ( 'NONE', *, *, #31719, .T. ) ;
#18708 = CARTESIAN_POINT ( 'NONE',  ( -93.67500000000003979, 92.29496732002878900, 83.51770833506763836 ) ) ;
#18709 = DIRECTION ( 'NONE',  ( -1.000000000000000000, -0.000000000000000000, 0.000000000000000000 ) ) ;
#18710 = VECTOR ( 'NONE', #2796, 1000.000000000000000 ) ;
#18711 = CARTESIAN_POINT ( 'NONE',  ( 10.00000000000000000, 51.02545421589324803, 55.20638768913779870 ) ) ;
#18712 = CARTESIAN_POINT ( 'NONE',  ( 97.30629616937498838, 88.66845928578035796, 81.65239583420047609 ) ) ;
#18713 = CARTESIAN_POINT ( 'NONE',  ( 10.00000000000000000, -16.45098606841149902, 33.79645857604508308 ) ) ;
#18714 = CARTESIAN_POINT ( 'NONE',  ( 10.00000000000000000, -20.41045688087876897, 72.35160999960810102 ) ) ;
#18715 = DIRECTION ( 'NONE',  ( -1.000000000000000000, 0.000000000000000000, -0.000000000000000000 ) ) ;
#18716 = CYLINDRICAL_SURFACE ( 'NONE', #6376, 5.000000000000000000 ) ;
#18717 = DIRECTION ( 'NONE',  ( -0.000000000000000000, -0.000000000000000000, -1.000000000000000000 ) ) ;
#18718 = CARTESIAN_POINT ( 'NONE',  ( 0.000000000000000000, 79.10210256391398786, -21.60688246758504505 ) ) ;
#18719 = CARTESIAN_POINT ( 'NONE',  ( 11.99999999999999822, 55.20638768913831029, -51.02545421589267960 ) ) ;
#18720 = CARTESIAN_POINT ( 'NONE',  ( 92.35000000049298308, -210.0000320324309939, 85.63541623677062375 ) ) ;
#18721 = DIRECTION ( 'NONE',  ( 0.000000000000000000, -0.000000000000000000, 1.000000000000000000 ) ) ;
#18722 = CARTESIAN_POINT ( 'NONE',  ( -96.15314808468751551, 88.00268892867056536, 87.84364583420047268 ) ) ;
#18723 = LINE ( 'NONE', #13087, #39569 ) ;
#18724 = EDGE_CURVE ( 'NONE', #15718, #57786, #69062, .T. ) ;
#18725 = ADVANCED_FACE ( 'NONE', ( #16773 ), #1856, .F. ) ;
#18726 = CARTESIAN_POINT ( 'NONE',  ( 10.00000000000000000, -6.736453364083817341, 36.88895765772630142 ) ) ;
#18727 = EDGE_CURVE ( 'NONE', #53818, #359, #45085, .T. ) ;
#18728 = ORIENTED_EDGE ( 'NONE', *, *, #17336, .F. ) ;
#18729 = FACE_OUTER_BOUND ( 'NONE', #52922, .T. ) ;
#18730 = LINE ( 'NONE', #47683, #69596 ) ;
#18731 = AXIS2_PLACEMENT_3D ( 'NONE', #51625, #23068, #1285 ) ;
#18732 = CYLINDRICAL_SURFACE ( 'NONE', #10701, 82.00000000000000000 ) ;
#18733 = ADVANCED_FACE ( 'NONE', ( #29507 ), #6955, .T. ) ;
#18734 = LINE ( 'NONE', #7096, #51163 ) ;
#18735 = CARTESIAN_POINT ( 'NONE',  ( 92.69370383062501162, -208.6684592857803011, 81.49364583420047836 ) ) ;
#18736 = CIRCLE ( 'NONE', #72773, 31.99999999999999289 ) ;
#18737 = EDGE_CURVE ( 'NONE', #43844, #10067, #23892, .T. ) ;
#18738 = VERTEX_POINT ( 'NONE', #63755 ) ;
#18739 = AXIS2_PLACEMENT_3D ( 'NONE', #15583, #61076, #55434 ) ;
#18740 = ORIENTED_EDGE ( 'NONE', *, *, #60062, .T. ) ;
#18741 =( NAMED_UNIT ( * ) PLANE_ANGLE_UNIT ( ) SI_UNIT ( $, .RADIAN. ) );
#18742 = EDGE_LOOP ( 'NONE', ( #23862, #56963, #61412, #28493 ) ) ;
#18743 = VECTOR ( 'NONE', #54507, 1000.000000000000000 ) ;
#18744 = DIRECTION ( 'NONE',  ( -0.000000000000000000, -0.000000000000000000, 1.000000000000000000 ) ) ;
#18745 = VECTOR ( 'NONE', #40636, 1000.000000000000000 ) ;
#18746 = CARTESIAN_POINT ( 'NONE',  ( 92.69370383062501162, -208.6684592857803295, 74.98489583420048632 ) ) ;
#18747 = EDGE_CURVE ( 'NONE', #32813, #21432, #17871, .T. ) ;
#18748 = ORIENTED_EDGE ( 'NONE', *, *, #19948, .T. ) ;
#18749 = CARTESIAN_POINT ( 'NONE',  ( 96.15314808468750130, -211.9973110713294489, 78.58322916753382970 ) ) ;
#18750 = ORIENTED_EDGE ( 'NONE', *, *, #50263, .T. ) ;
#18751 = DIRECTION ( 'NONE',  ( -1.000000000000000000, 0.000000000000000000, 0.000000000000000000 ) ) ;
#18752 = ORIENTED_EDGE ( 'NONE', *, *, #31388, .T. ) ;
#18753 = VERTEX_POINT ( 'NONE', #64120 ) ;
#18754 = CARTESIAN_POINT ( 'NONE',  ( -97.64999999950698850, -210.0000320324311076, 85.63541623677365067 ) ) ;
#18755 =( NAMED_UNIT ( * ) SI_UNIT ( $, .STERADIAN. ) SOLID_ANGLE_UNIT ( ) );
#18756 = CARTESIAN_POINT ( 'NONE',  ( 0.000000000000000000, 20.40083707022882820, 72.35432306680490910 ) ) ;
#18757 = ORIENTED_EDGE ( 'NONE', *, *, #67886, .T. ) ;
#18758 = CARTESIAN_POINT ( 'NONE',  ( 11.99999999999999822, 70.53064760720316428, -26.01480285779861035 ) ) ;
#18759 = CARTESIAN_POINT ( 'NONE',  ( 92.35000000000000853, -209.9999999999999716, 82.45937500173430124 ) ) ;
#18760 = CARTESIAN_POINT ( 'NONE',  ( 93.67499999999998295, 92.29496732002878900, 89.25916666666667254 ) ) ;
#18761 = EDGE_CURVE ( 'NONE', #1076, #48015, #59208, .T. ) ;
#18762 = EDGE_LOOP ( 'NONE', ( #60773, #52325, #48265, #64449 ) ) ;
#18763 = CARTESIAN_POINT ( 'NONE',  ( 0.000000000000000000, 46.54456581323888997, -59.03342792756214408 ) ) ;
#18764 = ADVANCED_FACE ( 'NONE', ( #1374 ), #2103, .F. ) ;
#18765 = CARTESIAN_POINT ( 'NONE',  ( 10.00000000000000000, 51.29473840253223926, 63.97538442413446091 ) ) ;
#18766 = ORIENTED_EDGE ( 'NONE', *, *, #14958, .F. ) ;
#18767 = VERTEX_POINT ( 'NONE', #64857 ) ;
#18768 = CARTESIAN_POINT ( 'NONE',  ( -96.15314808468751551, 88.00268892867056536, 88.00239583420048461 ) ) ;
#18769 = ORIENTED_EDGE ( 'NONE', *, *, #31985, .T. ) ;
#18770 = CARTESIAN_POINT ( 'NONE',  ( 94.99999999999998579, 93.05995642670504253, 85.47562500173431488 ) ) ;
#18771 = VERTEX_POINT ( 'NONE', #47189 ) ;
#18772 = CARTESIAN_POINT ( 'NONE',  ( 10.00000000000000000, 3.925862922256769583, -41.81611651403858332 ) ) ;
#18773 = LINE ( 'NONE', #41713, #35441 ) ;
#18774 = EDGE_LOOP ( 'NONE', ( #57072, #7849, #2141, #26927 ) ) ;
#18775 = ORIENTED_EDGE ( 'NONE', *, *, #9761, .T. ) ;
#18776 = ORIENTED_EDGE ( 'NONE', *, *, #65667, .T. ) ;
#18777 = PLANE ( 'NONE',  #14468 ) ;
#18778 = CARTESIAN_POINT ( 'NONE',  ( 92.34999999999996589, 91.52997821335250705, 81.69208333333332916 ) ) ;
#18779 = CARTESIAN_POINT ( 'NONE',  ( -97.65000000000001990, 91.52997821335253548, 86.13708333333332234 ) ) ;
#18780 = ORIENTED_EDGE ( 'NONE', *, *, #12987, .F. ) ;
#18781 = DIRECTION ( 'NONE',  ( -0.6575728627325957421, 0.7533909544171993877, 1.230411769795008318E-16 ) ) ;
#18782 = DIRECTION ( 'NONE',  ( 0.000000000000000000, 0.000000000000000000, 1.000000000000000000 ) ) ;
#18783 = ORIENTED_EDGE ( 'NONE', *, *, #13487, .F. ) ;
#18784 = DIRECTION ( 'NONE',  ( -1.000000000000000000, 0.000000000000000000, -0.000000000000000000 ) ) ;
#18785 = CARTESIAN_POINT ( 'NONE',  ( -92.69370383062498320, -211.3315407142195852, 82.92239583420045790 ) ) ;
#18786 = ORIENTED_EDGE ( 'NONE', *, *, #23005, .T. ) ;
#18787 = DIRECTION ( 'NONE',  ( 0.000000000000000000, 0.000000000000000000, -1.000000000000000000 ) ) ;
#18788 = CIRCLE ( 'NONE', #22401, 16.00000000000000000 ) ;
#18789 = FACE_OUTER_BOUND ( 'NONE', #14247, .T. ) ;
#18790 = CARTESIAN_POINT ( 'NONE',  ( 97.65000000000000568, 91.52997821335252127, 89.17979166840096639 ) ) ;
#18791 = CARTESIAN_POINT ( 'NONE',  ( 0.000000000000000000, -3.948201729842348850, 23.21447184625293048 ) ) ;
#18792 = LINE ( 'NONE', #453, #17582 ) ;
#18793 = CIRCLE ( 'NONE', #32043, 37.49900000000001654 ) ;
#18794 = CARTESIAN_POINT ( 'NONE',  ( 10.00000000000000000, 0.000000000000000000, 0.000000000000000000 ) ) ;
#18795 = FACE_OUTER_BOUND ( 'NONE', #48475, .T. ) ;
#18796 = AXIS2_PLACEMENT_3D ( 'NONE', #2911, #26539, #49472 ) ;
#18797 = CARTESIAN_POINT ( 'NONE',  ( 11.99999999999999822, -46.21855187248585395, -62.20884554314068993 ) ) ;
#18798 = CARTESIAN_POINT ( 'NONE',  ( 97.65000000000000568, 91.52997821335252127, 82.82979166840095786 ) ) ;
#18799 = CARTESIAN_POINT ( 'NONE',  ( -93.67499999999998295, -207.7050326799711968, 86.69270833506763552 ) ) ;
#18800 = ADVANCED_FACE ( 'NONE', ( #36272 ), #13337, .F. ) ;
#18801 = CARTESIAN_POINT ( 'NONE',  ( -96.15314808468751551, 88.00268892867056536, 77.68364583420047609 ) ) ;
#18802 = DIRECTION ( 'NONE',  ( 0.000000000000000000, 0.000000000000000000, 1.000000000000000000 ) ) ;
#18803 = CARTESIAN_POINT ( 'NONE',  ( -3.249999999999999556, -13.95926121303099343, 0.000000000000000000 ) ) ;
#18804 = AXIS2_PLACEMENT_3D ( 'NONE', #51834, #23271, #69138 ) ;
#18805 = CARTESIAN_POINT ( 'NONE',  ( 0.000000000000000000, 0.000000000000000000, 0.000000000000000000 ) ) ;
#18806 = DIRECTION ( 'NONE',  ( 1.000000000000000000, 1.427937372958405461E-15, 7.962523111839130290E-16 ) ) ;
#18807 = DIRECTION ( 'NONE',  ( -0.000000000000000000, -0.000000000000000000, -1.000000000000000000 ) ) ;
#18808 = DIRECTION ( 'NONE',  ( -1.000000000000000000, 0.000000000000000000, 0.000000000000000000 ) ) ;
#18809 = DIRECTION ( 'NONE',  ( -1.000000000000000000, 0.000000000000000000, 0.000000000000000000 ) ) ;
#18810 = COLOUR_RGB ( '', 0.66274510, 0.83137255, 0.94901961) ;
#18811 = FACE_OUTER_BOUND ( 'NONE', #15537, .T. ) ;
#18812 = CARTESIAN_POINT ( 'NONE',  ( -96.32499999999996021, -207.7050326799711968, 89.89416666666666345 ) ) ;
#18813 = ADVANCED_FACE ( 'NONE', ( #47557 ), #58460, .T. ) ;
#18815 = EDGE_CURVE ( 'NONE', #52797, #6335, #8069, .T. ) ;
#18814 = AXIS2_PLACEMENT_3D ( 'NONE', #65572, #48268, #31702 ) ;
#18816 = CARTESIAN_POINT ( 'NONE',  ( 5.000000000000000888, -1.936377641173859798, -5.802630826755080129 ) ) ;
#18817 = VERTEX_POINT ( 'NONE', #626 ) ;
#18818 = CARTESIAN_POINT ( 'NONE',  ( 0.000000000000000000, -69.42325613327466272, 34.44570377933573724 ) ) ;
#18819 = FACE_OUTER_BOUND ( 'NONE', #38095, .T. ) ;
#18820 = DIRECTION ( 'NONE',  ( 0.000000000000000000, 0.000000000000000000, 1.000000000000000000 ) ) ;
#18821 = ADVANCED_FACE ( 'NONE', ( #18243 ), #12228, .T. ) ;
#18822 = CARTESIAN_POINT ( 'NONE',  ( 5.000000000000000000, 68.55367621811141987, 44.99326035066078333 ) ) ;
#18823 = ADVANCED_FACE ( 'NONE', ( #53564 ), #30617, .T. ) ;
#18824 = AXIS2_PLACEMENT_3D ( 'NONE', #3858, #50437, #42963 ) ;
#18825 = CARTESIAN_POINT ( 'NONE',  ( -7.469491406282094736, 4.756046723998911929, 32.98187577049606745 ) ) ;
#18826 = ORIENTED_EDGE ( 'NONE', *, *, #71341, .T. ) ;
#18827 = CARTESIAN_POINT ( 'NONE',  ( -2.500000000000017319, -80.00000000000001421, -189.9999999999999147 ) ) ;
#18828 = CARTESIAN_POINT ( 'NONE',  ( 10.00000000000000000, 37.01155633439059756, 6.555932627142549762 ) ) ;
#18829 = VERTEX_POINT ( 'NONE', #46829 ) ;
#18830 = CARTESIAN_POINT ( 'NONE',  ( 96.15314808468748708, -208.0026889286704943, 86.25614583420048120 ) ) ;
#18831 = CARTESIAN_POINT ( 'NONE',  ( 96.15314808468748708, -208.0026889286704943, 88.95489583420049939 ) ) ;
#18832 = EDGE_CURVE ( 'NONE', #11001, #70989, #58102, .T. ) ;
#18833 = AXIS2_PLACEMENT_3D ( 'NONE', #21762, #62001, #67261 ) ;
#18834 = VERTEX_POINT ( 'NONE', #19344 ) ;
#18835 = CARTESIAN_POINT ( 'NONE',  ( -97.65000000000001990, 90.00000000000004263, 79.83999999999998920 ) ) ;
#18836 = CIRCLE ( 'NONE', #48849, 31.99999999999998934 ) ;
#18837 = ORIENTED_EDGE ( 'NONE', *, *, #68054, .T. ) ;
#18838 = LINE ( 'NONE', #53798, #19024 ) ;
#18839 = ORIENTED_EDGE ( 'NONE', *, *, #26976, .F. ) ;
#18840 = CARTESIAN_POINT ( 'NONE',  ( -92.69370383062504004, 90.00000000000004263, 80.59406250086715318 ) ) ;
#18841 = ORIENTED_EDGE ( 'NONE', *, *, #1144, .F. ) ;
#18842 = VECTOR ( 'NONE', #12420, 1000.000000000000000 ) ;
#18843 = ORIENTED_EDGE ( 'NONE', *, *, #66224, .F. ) ;
#18844 = LINE ( 'NONE', #25247, #38819 ) ;
#18845 = VECTOR ( 'NONE', #9750, 1000.000000000000000 ) ;
#18846 = VERTEX_POINT ( 'NONE', #40817 ) ;
#18847 = CARTESIAN_POINT ( 'NONE',  ( 0.000000000000000000, 0.000000000000000000, 0.000000000000000000 ) ) ;
#18848 = CARTESIAN_POINT ( 'NONE',  ( 92.35000000000006537, -211.5299782133524786, 79.25791666666667368 ) ) ;
#18849 = EDGE_CURVE ( 'NONE', #49532, #38633, #59582, .T. ) ;
#18850 = ORIENTED_EDGE ( 'NONE', *, *, #73188, .F. ) ;
#18852 = CARTESIAN_POINT ( 'NONE',  ( 5.000000000000000000, -46.11716303203234446, 67.80270845531873647 ) ) ;
#18851 = PRODUCT_DEFINITION_SHAPE ( 'NONE', 'NONE',  #74373 ) ;
#18853 = VECTOR ( 'NONE', #19925, 1000.000000000000000 ) ;
#18854 = VERTEX_POINT ( 'NONE', #42300 ) ;
#18855 = CARTESIAN_POINT ( 'NONE',  ( 93.74200686866046794, 87.71227518788542454, 74.97309184317514053 ) ) ;
#18856 = EDGE_CURVE ( 'NONE', #10445, #24628, #15005, .T. ) ;
#18857 = ORIENTED_EDGE ( 'NONE', *, *, #41544, .F. ) ;
#18858 = ORIENTED_EDGE ( 'NONE', *, *, #40686, .F. ) ;
#18859 = VERTEX_POINT ( 'NONE', #7343 ) ;
#18860 = CARTESIAN_POINT ( 'NONE',  ( 92.69370383062501162, -208.6684592857803011, 83.23989583420046756 ) ) ;
#18861 = DIRECTION ( 'NONE',  ( 0.000000000000000000, 0.000000000000000000, 1.000000000000000000 ) ) ;
#18862 = LINE ( 'NONE', #25987, #23376 ) ;
#18863 = AXIS2_PLACEMENT_3D ( 'NONE', #43918, #66838, #15322 ) ;
#18864 = DIRECTION ( 'NONE',  ( -0.000000000000000000, -0.000000000000000000, 1.000000000000000000 ) ) ;
#18865 = CARTESIAN_POINT ( 'NONE',  ( 93.67499999999999716, 87.70503267997126784, 85.02583333333332405 ) ) ;
#18866 = LINE ( 'NONE', #24886, #24754 ) ;
#18867 = CARTESIAN_POINT ( 'NONE',  ( 0.000000000000000000, 22.07842321921481243, 8.187992925817422218 ) ) ;
#18868 = CARTESIAN_POINT ( 'NONE',  ( 10.00000000000000000, -12.42422080174614862, -35.38097989696524337 ) ) ;
#18869 = CARTESIAN_POINT ( 'NONE',  ( -92.69370383062498320, -208.6684592857803011, 83.02822916753379445 ) ) ;
#18870 = AXIS2_PLACEMENT_3D ( 'NONE', #63722, #23858, #20054 ) ;
#18871 = CARTESIAN_POINT ( 'NONE',  ( -93.84685191531252713, 88.00268892867056536, 83.02822916753380866 ) ) ;
#18872 = EDGE_LOOP ( 'NONE', ( #2706, #20154, #9732, #272 ) ) ;
#18873 = CARTESIAN_POINT ( 'NONE',  ( 92.69370383062498320, 90.00000000000002842, 82.02281250086714692 ) ) ;
#18874 = ORIENTED_EDGE ( 'NONE', *, *, #24472, .T. ) ;
#18875 = DIRECTION ( 'NONE',  ( 0.000000000000000000, 0.000000000000000000, 1.000000000000000000 ) ) ;
#18876 = CARTESIAN_POINT ( 'NONE',  ( 5.000000000000000000, -33.71516098798685590, -74.74816331893465815 ) ) ;
#18877 = DIRECTION ( 'NONE',  ( -1.000000000000000000, -0.000000000000000000, -0.000000000000000000 ) ) ;
#18878 = CARTESIAN_POINT ( 'NONE',  ( -0.2999999999999947153, 0.000000000000000000, 0.000000000000000000 ) ) ;
#18879 = CARTESIAN_POINT ( 'NONE',  ( 10.00000000000000000, 51.03279382321166224, -55.19960302592011914 ) ) ;
#18880 = CARTESIAN_POINT ( 'NONE',  ( -97.30629616937497417, -208.6684592857803295, 84.50989583420049200 ) ) ;
#18881 = DIRECTION ( 'NONE',  ( -1.000000000000000000, -0.000000000000000000, -0.000000000000000000 ) ) ;
#18882 = FACE_OUTER_BOUND ( 'NONE', #10558, .T. ) ;
#18883 = FACE_OUTER_BOUND ( 'NONE', #42101, .T. ) ;
#18884 = CARTESIAN_POINT ( 'NONE',  ( 11.99999999999999822, 56.15606465354957777, 59.75363087400094031 ) ) ;
#18885 = ORIENTED_EDGE ( 'NONE', *, *, #51632, .T. ) ;
#18886 = ORIENTED_EDGE ( 'NONE', *, *, #59252, .T. ) ;
#18887 = CARTESIAN_POINT ( 'NONE',  ( -93.67500000000003979, 87.70503267997129626, 76.24166666666666003 ) ) ;
#18888 = CARTESIAN_POINT ( 'NONE',  ( -93.67499999999998295, -212.2949673200287179, 78.78166666666666629 ) ) ;
#18889 = CARTESIAN_POINT ( 'NONE',  ( -92.69370383062502583, 91.33154071421968467, 89.37822916753381719 ) ) ;
#18890 = CARTESIAN_POINT ( 'NONE',  ( 11.99999999999999822, 75.54627589209970040, -17.28742895386005785 ) ) ;
#18891 = DIRECTION ( 'NONE',  ( -1.000000000000000000, -0.000000000000000000, -0.000000000000000000 ) ) ;
#18892 = CARTESIAN_POINT ( 'NONE',  ( 92.35000000000000853, -209.9999999999999716, 78.01437500173430806 ) ) ;
#18893 = CARTESIAN_POINT ( 'NONE',  ( 0.000000000000000000, -22.48208911017474065, -35.47612816024548721 ) ) ;
#18894 = AXIS2_PLACEMENT_3D ( 'NONE', #53666, #2204, #56264 ) ;
#18895 = ORIENTED_EDGE ( 'NONE', *, *, #14922, .T. ) ;
#18896 = DIRECTION ( 'NONE',  ( 0.000000000000000000, 0.000000000000000000, 1.000000000000000000 ) ) ;
#18897 = AXIS2_PLACEMENT_3D ( 'NONE', #74068, #38386, #67700 ) ;
#18898 = DIRECTION ( 'NONE',  ( 0.000000000000000000, 0.000000000000000000, 1.000000000000000000 ) ) ;
#18899 = EDGE_CURVE ( 'NONE', #2154, #19352, #46140, .T. ) ;
#18900 = DIRECTION ( 'NONE',  ( 1.000000000000000000, 0.000000000000000000, 0.000000000000000000 ) ) ;
#18901 = CONICAL_SURFACE ( 'NONE', #2110, 12.83284365640956182, 0.3490658503988688377 ) ;
#18902 = DIRECTION ( 'NONE',  ( 0.000000000000000000, -0.9510565162951543083, -0.3090169943749448977 ) ) ;
#18903 = DIRECTION ( 'NONE',  ( 0.000000000000000000, 0.000000000000000000, 1.000000000000000000 ) ) ;
#18904 = CARTESIAN_POINT ( 'NONE',  ( -92.69370383062498320, -211.3315407142195852, 86.89114583420050053 ) ) ;
#18905 = VECTOR ( 'NONE', #39641, 1000.000000000000114 ) ;
#18906 = EDGE_CURVE ( 'NONE', #15896, #34394, #41474, .T. ) ;
#18907 = DIRECTION ( 'NONE',  ( -1.000000000000000000, -0.000000000000000000, -0.000000000000000000 ) ) ;
#18908 =( BOUNDED_CURVE ( )  B_SPLINE_CURVE ( 2, ( #60168, #72156, #21022, #43614, #26663, #15014, #31560, #61634, #60892, #27403, #27028 ),
 .UNSPECIFIED., .F., .F. ) 
 B_SPLINE_CURVE_WITH_KNOTS ( ( 3, 2, 2, 2, 2, 3 ),
 ( 0.04233441017594418571, 0.04233459324529416368, 0.04939035878617631381, 0.05644612432705845700, 0.06350188986794061408, 0.06350193517735455706 ),
 .UNSPECIFIED. ) 
 CURVE ( )  GEOMETRIC_REPRESENTATION_ITEM ( )  RATIONAL_B_SPLINE_CURVE ( ( 0.9999930479532715966, 0.9999965238864443329, 1.000000000000000000, 0.8660254037844387076, 1.000000000000000000, 0.8660254037844387076, 1.000000000000000000, 0.8660254037844387076, 1.000000000000000000, 0.9999991396666452204, 0.9999982793443398243 ) ) 
 REPRESENTATION_ITEM ( '' )  );
#18909 = FACE_OUTER_BOUND ( 'NONE', #67697, .T. ) ;
#18910 = CARTESIAN_POINT ( 'NONE',  ( -96.15314808468745866, -211.9973110713294489, 77.20739583420048291 ) ) ;
#18911 = LINE ( 'NONE', #41856, #49452 ) ;
#18912 = ORIENTED_EDGE ( 'NONE', *, *, #23458, .F. ) ;
#18913 = EDGE_CURVE ( 'NONE', #26714, #10762, #40288, .T. ) ;
#18914 = CYLINDRICAL_SURFACE ( 'NONE', #53315, 4.750000000000000000 ) ;
#18915 = DIRECTION ( 'NONE',  ( -1.000000000000000000, 0.000000000000000000, 0.000000000000000000 ) ) ;
#18916 = DIRECTION ( 'NONE',  ( 0.000000000000000000, -0.8090169943749531134, 0.5877852522924653655 ) ) ;
#18917 = AXIS2_PLACEMENT_3D ( 'NONE', #3984, #6120, #23398 ) ;
#18918 = CARTESIAN_POINT ( 'NONE',  ( -10.00000000000000000, 0.000000000000000000, 0.000000000000000000 ) ) ;
#18919 = CARTESIAN_POINT ( 'NONE',  ( 95.00000000000000000, -207.3369185715606307, 78.68906250086713783 ) ) ;
#18920 = ORIENTED_EDGE ( 'NONE', *, *, #2181, .T. ) ;
#18921 = AXIS2_PLACEMENT_3D ( 'NONE', #32446, #22289, #62146 ) ;
#18922 = DIRECTION ( 'NONE',  ( -1.000000000000000000, -0.000000000000000000, -0.000000000000000000 ) ) ;
#18923 = ADVANCED_FACE ( 'NONE', ( #43782 ), #42660, .T. ) ;
#18924 = ORIENTED_EDGE ( 'NONE', *, *, #32995, .F. ) ;
#18925 = CARTESIAN_POINT ( 'NONE',  ( 0.000000000000000000, 0.000000000000000000, 0.000000000000000000 ) ) ;
#18926 = EDGE_CURVE ( 'NONE', #21615, #43377, #28253, .T. ) ;
#18927 = ADVANCED_FACE ( 'NONE', ( #8813 ), #8451, .T. ) ;
#18928 = ORIENTED_EDGE ( 'NONE', *, *, #18482, .F. ) ;
#18929 = PLANE ( 'NONE',  #45471 ) ;
#18930 = EDGE_CURVE ( 'NONE', #46225, #69079, #39106, .T. ) ;
#18931 = ORIENTED_EDGE ( 'NONE', *, *, #5129, .T. ) ;
#18932 = EDGE_LOOP ( 'NONE', ( #43384, #46215, #1980, #62842 ) ) ;
#18933 = ORIENTED_EDGE ( 'NONE', *, *, #42762, .F. ) ;
#18934 = LINE ( 'NONE', #40398, #64738 ) ;
#18935 = EDGE_CURVE ( 'NONE', #55001, #2989, #38497, .T. ) ;
#18936 = EDGE_LOOP ( 'NONE', ( #158, #8047, #50016, #58200 ) ) ;
#18937 = VERTEX_POINT ( 'NONE', #2839 ) ;
#18938 = CARTESIAN_POINT ( 'NONE',  ( 93.84685191531248449, 88.00268892867053694, 81.01739583420049939 ) ) ;
#18939 = LINE ( 'NONE', #10821, #57588 ) ;
#18940 = AXIS2_PLACEMENT_3D ( 'NONE', #59734, #60484, #72107 ) ;
#18941 = CARTESIAN_POINT ( 'NONE',  ( 92.35000000000000853, -209.9999999999999716, 76.03000000000000114 ) ) ;
#18942 = AXIS2_PLACEMENT_3D ( 'NONE', #50996, #57381, #5158 ) ;
#18943 = ORIENTED_EDGE ( 'NONE', *, *, #53709, .F. ) ;
#18944 = CIRCLE ( 'NONE', #60980, 32.00000000000000000 ) ;
#18945 = ORIENTED_EDGE ( 'NONE', *, *, #48790, .F. ) ;
#18946 = EDGE_LOOP ( 'NONE', ( #47148, #2663, #21004, #28967 ) ) ;
#18947 = CARTESIAN_POINT ( 'NONE',  ( 0.000000000000000000, 0.000000000000000000, 0.000000000000000000 ) ) ;
#18948 = EDGE_LOOP ( 'NONE', ( #30388, #71278, #47600, #37175 ) ) ;
#18949 = DIRECTION ( 'NONE',  ( 0.000000000000000000, 0.000000000000000000, 1.000000000000000000 ) ) ;
#18950 = LINE ( 'NONE', #48648, #54711 ) ;
#18951 = VECTOR ( 'NONE', #31741, 1000.000000000000000 ) ;
#18952 = DIRECTION ( 'NONE',  ( -1.000000000000000000, 0.000000000000000000, -0.000000000000000000 ) ) ;
#18953 = CARTESIAN_POINT ( 'NONE',  ( -3.000000000000000000, -0.9646360437375307573, 23.52805723605590060 ) ) ;
#18954 = CIRCLE ( 'NONE', #35744, 12.75000000000265388 ) ;
#18955 = CARTESIAN_POINT ( 'NONE',  ( -92.34999999999999432, -210.0000000255707278, 84.04687500080852658 ) ) ;
#18956 = LINE ( 'NONE', #42646, #10826 ) ;
#18957 = CARTESIAN_POINT ( 'NONE',  ( 0.000000000000000000, -37.48860685352291711, 0.8828120875899322373 ) ) ;
#18958 = CARTESIAN_POINT ( 'NONE',  ( -93.67499999999998295, -207.7050326799711968, 79.07270833506763097 ) ) ;
#18959 = LINE ( 'NONE', #41907, #21871 ) ;
#18961 = CARTESIAN_POINT ( 'NONE',  ( -96.32500000000001705, 87.70503267997129626, 74.94520833506761903 ) ) ;
#18960 = CARTESIAN_POINT ( 'NONE',  ( 92.34999999999999432, 90.00000000000002842, 76.10937500173430692 ) ) ;
#18962 = EDGE_LOOP ( 'NONE', ( #51214, #60345, #1987, #71360 ) ) ;
#18963 = CARTESIAN_POINT ( 'NONE',  ( 94.99999999999998579, 92.66308142843935514, 76.94281250086714863 ) ) ;
#18964 = CARTESIAN_POINT ( 'NONE',  ( 97.65000000000009095, 88.47002178664756400, 75.65958333333333030 ) ) ;
#18965 = CARTESIAN_POINT ( 'NONE',  ( 10.00000000000000000, -35.38097989696520074, 12.42422080174625520 ) ) ;
#18966 = CARTESIAN_POINT ( 'NONE',  ( 92.35000000000000853, -210.0000348529810310, 77.37937620717862330 ) ) ;
#18967 = DIRECTION ( 'NONE',  ( 0.000000000000000000, 1.000000000000000000, -9.787530781167598712E-16 ) ) ;
#18968 = CARTESIAN_POINT ( 'NONE',  ( 15.00000000000000000, -10.45096189432314127, 21.10159698893440350 ) ) ;
#18969 = VERTEX_POINT ( 'NONE', #25730 ) ;
#18970 = CARTESIAN_POINT ( 'NONE',  ( -3.000000000000000000, 22.07842321921481243, 8.187992925817422218 ) ) ;
#18971 = CARTESIAN_POINT ( 'NONE',  ( 11.99999999999999822, 34.94270380257639630, 74.18225833017902460 ) ) ;
#18972 = ORIENTED_EDGE ( 'NONE', *, *, #70318, .T. ) ;
#18973 = CIRCLE ( 'NONE', #8131, 16.00000000000000000 ) ;
#18974 = EDGE_LOOP ( 'NONE', ( #57902, #37363, #12573, #43298 ) ) ;
#18975 = CIRCLE ( 'NONE', #39449, 31.99999999999999289 ) ;
#18976 = VECTOR ( 'NONE', #72254, 1000.000000000000000 ) ;
#18977 = CARTESIAN_POINT ( 'NONE',  ( 15.00000000000000000, 5.835314593368470248, -22.81335362449854642 ) ) ;
#18978 = CARTESIAN_POINT ( 'NONE',  ( 10.00000000000000000, -2.663952781846440576, 41.91543099594817789 ) ) ;
#18979 = CARTESIAN_POINT ( 'NONE',  ( 0.1219594728601484379, -121.4950337410840149, -2.500000000000000000 ) ) ;
#18980 = DIRECTION ( 'NONE',  ( 0.000000000000000000, 0.000000000000000000, 1.000000000000000000 ) ) ;
#18981 = CARTESIAN_POINT ( 'NONE',  ( -93.84685191531248449, -208.0026889286704943, 78.79489583420048859 ) ) ;
#18982 = AXIS2_PLACEMENT_3D ( 'NONE', #47769, #35740, #47049 ) ;
#18983 = EDGE_LOOP ( 'NONE', ( #29563, #33343, #50949, #38076 ) ) ;
#18984 = EDGE_CURVE ( 'NONE', #63724, #24340, #7867, .T. ) ;
#18985 = CARTESIAN_POINT ( 'NONE',  ( 10.00000000000000000, 0.000000000000000000, 0.000000000000000000 ) ) ;
#18986 = CARTESIAN_POINT ( 'NONE',  ( 10.00000000000000000, -26.01480285779785362, -70.53064760720343429 ) ) ;
#18987 = EDGE_CURVE ( 'NONE', #35888, #43637, #3936, .T. ) ;
#18988 = CARTESIAN_POINT ( 'NONE',  ( 94.99999999999998579, 86.94004357329502852, 85.79312500173431033 ) ) ;
#18989 = CARTESIAN_POINT ( 'NONE',  ( 5.000000000000002665, -81.96053171279901051, -2.543863470249246195 ) ) ;
#18990 = CARTESIAN_POINT ( 'NONE',  ( 0.000000000000000000, -120.0000000000000000, 5.500000000000000888 ) ) ;
#18991 = DIRECTION ( 'NONE',  ( -1.000000000000000000, 0.000000000000000000, 0.000000000000000000 ) ) ;
#18992 = DIRECTION ( 'NONE',  ( -0.000000000000000000, -0.000000000000000000, 1.000000000000000000 ) ) ;
#18993 = CARTESIAN_POINT ( 'NONE',  ( 11.99999999999999822, -75.11764819372145041, -2.946379043147127064 ) ) ;
#18994 = EDGE_CURVE ( 'NONE', #55743, #67887, #14817, .T. ) ;
#18995 = CARTESIAN_POINT ( 'NONE',  ( -96.32499999999996021, -207.7050326799711968, 77.90854166840097150 ) ) ;
#18996 = DIRECTION ( 'NONE',  ( -0.000000000000000000, -0.000000000000000000, -1.000000000000000000 ) ) ;
#18997 = EDGE_CURVE ( 'NONE', #73020, #48094, #17319, .T. ) ;
#18998 = VECTOR ( 'NONE', #31433, 1000.000000000000000 ) ;
#18999 = CARTESIAN_POINT ( 'NONE',  ( 94.99999999999998579, 87.33691857156068750, 82.34031250086714238 ) ) ;
#19000 = AXIS2_PLACEMENT_3D ( 'NONE', #73457, #23093, #21963 ) ;
#19001 = CIRCLE ( 'NONE', #25017, 31.99999999999998934 ) ;
#19002 = CARTESIAN_POINT ( 'NONE',  ( -96.15314808468745866, -211.9973110713294489, 85.46239583420047836 ) ) ;
#19003 = CARTESIAN_POINT ( 'NONE',  ( 97.64999999999999147, -210.0000000255706709, 84.04687500080852658 ) ) ;
#19004 = ORIENTED_EDGE ( 'NONE', *, *, #52973, .T. ) ;
#19005 = EDGE_CURVE ( 'NONE', #9070, #14968, #36934, .T. ) ;
#19006 = LINE ( 'NONE', #41958, #71221 ) ;
#19007 = CARTESIAN_POINT ( 'NONE',  ( -92.34999999999999432, -211.5299782133524502, 82.64458333333331552 ) ) ;
#19008 = CARTESIAN_POINT ( 'NONE',  ( -92.69370383062505425, 91.33154071421968467, 76.67822916753378593 ) ) ;
#19009 = CIRCLE ( 'NONE', #61037, 82.00000000000000000 ) ;
#19010 = CIRCLE ( 'NONE', #63475, 82.00000000000000000 ) ;
#19011 = CARTESIAN_POINT ( 'NONE',  ( 96.15314808468748708, -208.0026889286704943, 88.79614583420047325 ) ) ;
#19012 = ORIENTED_EDGE ( 'NONE', *, *, #9838, .T. ) ;
#19013 = EDGE_LOOP ( 'NONE', ( #31689, #36309, #13296, #45215 ) ) ;
#19014 = EDGE_CURVE ( 'NONE', #7348, #54917, #1903, .T. ) ;
#19015 = ORIENTED_EDGE ( 'NONE', *, *, #37536, .T. ) ;
#19016 = AXIS2_PLACEMENT_3D ( 'NONE', #52778, #58408, #59530 ) ;
#19017 = CYLINDRICAL_SURFACE ( 'NONE', #42987, 77.49899999999999523 ) ;
#19018 = EDGE_CURVE ( 'NONE', #3129, #67030, #43422, .T. ) ;
#19019 = EDGE_CURVE ( 'NONE', #38362, #21255, #66345, .T. ) ;
#19020 = DIRECTION ( 'NONE',  ( -0.000000000000000000, -0.000000000000000000, 1.000000000000000000 ) ) ;
#19021 = AXIS2_PLACEMENT_3D ( 'NONE', #53081, #71087, #1256 ) ;
#19022 = VERTEX_POINT ( 'NONE', #38121 ) ;
#19023 = ORIENTED_EDGE ( 'NONE', *, *, #57956, .T. ) ;
#19024 = VECTOR ( 'NONE', #53434, 1000.000000000000000 ) ;
#19025 = CARTESIAN_POINT ( 'NONE',  ( 10.00000000000000000, 16.45098606841126454, 33.79645857604518966 ) ) ;
#19026 = CARTESIAN_POINT ( 'NONE',  ( 97.30629616937498838, -211.3315407142195852, 82.44614583420049314 ) ) ;
#19027 = CARTESIAN_POINT ( 'NONE',  ( 10.00000000000000000, 16.95692799528845640, -2.500000000000000000 ) ) ;
#19028 = EDGE_CURVE ( 'NONE', #73248, #71157, #37013, .T. ) ;
#19029 = DIRECTION ( 'NONE',  ( -0.000000000000000000, -0.000000000000000000, 1.000000000000000000 ) ) ;
#19030 = AXIS2_PLACEMENT_3D ( 'NONE', #10508, #10896, #51107 ) ;
#19031 = CARTESIAN_POINT ( 'NONE',  ( 10.00000000000000000, 75.11725578898472122, -2.956366410619845730 ) ) ;
#19032 = CARTESIAN_POINT ( 'NONE',  ( 97.65000000000000568, 88.47002178664752137, 76.92958333333332632 ) ) ;
#19033 = DIRECTION ( 'NONE',  ( 1.000000000000000000, -0.000000000000000000, -0.000000000000000000 ) ) ;
#19034 = CARTESIAN_POINT ( 'NONE',  ( 97.64999999999999147, -209.9999999999999716, 86.50750000000000739 ) ) ;
#19035 = EDGE_LOOP ( 'NONE', ( #43775, #52289, #73779, #50401 ) ) ;
#19036 = ORIENTED_EDGE ( 'NONE', *, *, #40981, .F. ) ;
#19037 = ORIENTED_EDGE ( 'NONE', *, *, #50225, .T. ) ;
#19038 = VERTEX_POINT ( 'NONE', #67059 ) ;
#19039 = FACE_OUTER_BOUND ( 'NONE', #20541, .T. ) ;
#19040 = CARTESIAN_POINT ( 'NONE',  ( -95.00000000000002842, 92.66308142843932671, 87.10281250086715943 ) ) ;
#19041 = FACE_OUTER_BOUND ( 'NONE', #63553, .T. ) ;
#19042 = CARTESIAN_POINT ( 'NONE',  ( -95.00000000000002842, 86.94004357329504273, 83.80875000000000341 ) ) ;
#19043 = CARTESIAN_POINT ( 'NONE',  ( 95.00000000000000000, -207.3369185715606307, 87.57906250086713840 ) ) ;
#19044 =( BOUNDED_CURVE ( )  B_SPLINE_CURVE ( 2, ( #13554, #24838, #30470, #58319, #64703, #46304, #29724 ),
 .UNSPECIFIED., .F., .T. ) 
 B_SPLINE_CURVE_WITH_KNOTS ( ( 3, 2, 2, 3 ),
 ( 0.1041666666666670182, 0.1111111111111114103, 0.1180555555555558161, 0.1250000000000002220 ),
 .UNSPECIFIED. ) 
 CURVE ( )  GEOMETRIC_REPRESENTATION_ITEM ( )  RATIONAL_B_SPLINE_CURVE ( ( 0.9999999999999933387, 0.8660254037844453689, 1.000000000000000000, 0.8660254037844387076, 1.000000000000000000, 0.8660254037844343777, 1.000000000000004219 ) ) 
 REPRESENTATION_ITEM ( '' )  );
#19045 = DIRECTION ( 'NONE',  ( -1.000000000000000000, 0.000000000000000000, 0.000000000000000000 ) ) ;
#19046 = ORIENTED_EDGE ( 'NONE', *, *, #62327, .T. ) ;
#19047 = VECTOR ( 'NONE', #10277, 999.9999999999998863 ) ;
#19048 = FACE_OUTER_BOUND ( 'NONE', #12197, .T. ) ;
#19049 = VERTEX_POINT ( 'NONE', #53946 ) ;
#19050 = CARTESIAN_POINT ( 'NONE',  ( -96.32499999999996021, -212.2949673200287179, 85.02583333333332405 ) ) ;
#19051 = VERTEX_POINT ( 'NONE', #51628 ) ;
#19052 = CARTESIAN_POINT ( 'NONE',  ( -92.35000000000005116, 88.47002178664754979, 87.16895833506762870 ) ) ;
#19053 = AXIS2_PLACEMENT_3D ( 'NONE', #38493, #27187, #61432 ) ;
#19054 = CARTESIAN_POINT ( 'NONE',  ( 93.84685191531248449, 88.00268892867053694, 75.77864583420047495 ) ) ;
#19055 = DIRECTION ( 'NONE',  ( 0.000000000000000000, 0.7071067811865439090, 0.7071067811865512365 ) ) ;
#19056 = VECTOR ( 'NONE', #49329, 1000.000000000000000 ) ;
#19057 = VECTOR ( 'NONE', #63146, 1000.000000000000000 ) ;
#19058 = DIRECTION ( 'NONE',  ( -0.5000000000000039968, 0.8660254037844363761, 0.000000000000000000 ) ) ;
#19059 = DIRECTION ( 'NONE',  ( 1.000000000000000000, 0.000000000000000000, 0.000000000000000000 ) ) ;
#19060 = CARTESIAN_POINT ( 'NONE',  ( 11.99999999999999822, 0.000000000000000000, 0.000000000000000000 ) ) ;
#19061 = ORIENTED_EDGE ( 'NONE', *, *, #29963, .T. ) ;
#19062 = DIRECTION ( 'NONE',  ( -1.000000000000000000, 0.000000000000000000, 0.000000000000000000 ) ) ;
#19063 = CARTESIAN_POINT ( 'NONE',  ( -93.67500000000003979, 92.29496732002878900, 81.61270833506763722 ) ) ;
#19064 = ORIENTED_EDGE ( 'NONE', *, *, #18297, .T. ) ;
#19065 = CIRCLE ( 'NONE', #40652, 42.00000000000000000 ) ;
#19066 = ORIENTED_EDGE ( 'NONE', *, *, #13235, .F. ) ;
#19067 = CIRCLE ( 'NONE', #65888, 15.99999999999999467 ) ;
#19068 = CARTESIAN_POINT ( 'NONE',  ( 0.000000000000000000, 26.50000000000000000, -1.500000000000001332 ) ) ;
#19069 = DIRECTION ( 'NONE',  ( 0.000000000000000000, 0.000000000000000000, 1.000000000000000000 ) ) ;
#19070 = DIRECTION ( 'NONE',  ( -1.000000000000000000, 0.000000000000000000, 0.000000000000000000 ) ) ;
#19071 = CARTESIAN_POINT ( 'NONE',  ( -97.30629616937495996, -209.9999999999999716, 86.62656250086715204 ) ) ;
#19072 = VERTEX_POINT ( 'NONE', #74184 ) ;
#19073 = DIRECTION ( 'NONE',  ( -0.000000000000000000, -0.000000000000000000, -1.000000000000000000 ) ) ;
#19074 = ORIENTED_EDGE ( 'NONE', *, *, #44736, .F. ) ;
#19075 = VECTOR ( 'NONE', #70379, 1000.000000000000000 ) ;
#19076 = CIRCLE ( 'NONE', #61109, 42.00000000000000000 ) ;
#19077 = ORIENTED_EDGE ( 'NONE', *, *, #53580, .T. ) ;
#19078 = CARTESIAN_POINT ( 'NONE',  ( 0.000000000000000000, 31.47745569255140552, 68.26794271651274926 ) ) ;
#19079 = CIRCLE ( 'NONE', #5913, 2.650000000000540812 ) ;
#19080 = AXIS2_PLACEMENT_3D ( 'NONE', #51508, #62, #45892 ) ;
#19081 = CARTESIAN_POINT ( 'NONE',  ( 96.32499999999997442, 92.29496732002878900, 86.61333333333332973 ) ) ;
#19082 = EDGE_CURVE ( 'NONE', #69246, #26229, #16298, .T. ) ;
#19083 = PLANE ( 'NONE',  #967 ) ;
#19084 = CARTESIAN_POINT ( 'NONE',  ( 96.15314808468748708, 91.99731107132950569, 83.08114583420048405 ) ) ;
#19085 = DIRECTION ( 'NONE',  ( 0.000000000000000000, 0.7604059656000322631, -0.6494480483301821039 ) ) ;
#19086 = DIRECTION ( 'NONE',  ( -1.000000000000000000, 0.000000000000000000, 0.000000000000000000 ) ) ;
#19087 = DIRECTION ( 'NONE',  ( -1.000000000000000000, 0.000000000000000000, -0.000000000000000000 ) ) ;
#19088 = VECTOR ( 'NONE', #30033, 1000.000000000000000 ) ;
#19089 = DIRECTION ( 'NONE',  ( 0.000000000000000000, 0.000000000000000000, 1.000000000000000000 ) ) ;
#19090 = VECTOR ( 'NONE', #39178, 1000.000000000000000 ) ;
#19092 = ADVANCED_FACE ( 'NONE', ( #179 ), #44888, .T. ) ;
#19091 = CARTESIAN_POINT ( 'NONE',  ( -92.35000000000312070, 89.99999595380251094, 77.06187486178039592 ) ) ;
#19093 = CARTESIAN_POINT ( 'NONE',  ( -10.90473778262209414, 1.679381574647996852E-15, 13.71319123046128752 ) ) ;
#19094 = CARTESIAN_POINT ( 'NONE',  ( -92.35000000000003695, 89.99999988321006583, 84.68187499741277691 ) ) ;
#19095 = CIRCLE ( 'NONE', #46682, 77.49899999999999523 ) ;
#19096 = EDGE_CURVE ( 'NONE', #40132, #53667, #17050, .T. ) ;
#19097 = DIRECTION ( 'NONE',  ( -0.000000000000000000, -0.000000000000000000, 1.000000000000000000 ) ) ;
#19098 = LINE ( 'NONE', #41301, #28960 ) ;
#19099 = ORIENTED_EDGE ( 'NONE', *, *, #30013, .T. ) ;
#19100 = CARTESIAN_POINT ( 'NONE',  ( -97.30629616937501680, 88.66845928578038638, 85.25072916753379104 ) ) ;
#19101 = CARTESIAN_POINT ( 'NONE',  ( 100.0000000000260201, 95.00000000000001421, -75.00000000000000000 ) ) ;
#19102 = ADVANCED_FACE ( 'NONE', ( #39985 ), #23071, .F. ) ;
#19103 = CARTESIAN_POINT ( 'NONE',  ( 10.00000000000000000, 0.000000000000000000, 0.000000000000000000 ) ) ;
#19104 = EDGE_CURVE ( 'NONE', #54754, #7371, #11459, .T. ) ;
#19105 = ORIENTED_EDGE ( 'NONE', *, *, #32566, .T. ) ;
#19107 = CARTESIAN_POINT ( 'NONE',  ( 15.00000000000000000, -23.29833615347104470, 3.418703333116808629 ) ) ;
#19106 = AXIS2_PLACEMENT_3D ( 'NONE', #3834, #22598, #5323 ) ;
#19108 = CYLINDRICAL_SURFACE ( 'NONE', #61163, 12.50000000000000000 ) ;
#19109 = AXIS2_PLACEMENT_3D ( 'NONE', #55472, #51302, #74236 ) ;
#19110 = AXIS2_PLACEMENT_3D ( 'NONE', #70460, #24986, #53195 ) ;
#19111 = CIRCLE ( 'NONE', #66099, 31.99999999999998579 ) ;
#19112 = FACE_OUTER_BOUND ( 'NONE', #7037, .T. ) ;
#19113 = EDGE_CURVE ( 'NONE', #17976, #57167, #16742, .T. ) ;
#19114 = EDGE_CURVE ( 'NONE', #70845, #25521, #33211, .T. ) ;
#19115 = CARTESIAN_POINT ( 'NONE',  ( 95.00000000000000000, -212.6630814284392557, 82.97531250086716170 ) ) ;
#19116 = VECTOR ( 'NONE', #28155, 1000.000000000000000 ) ;
#19117 = CIRCLE ( 'NONE', #35917, 82.00000000000000000 ) ;
#19118 = ORIENTED_EDGE ( 'NONE', *, *, #20949, .F. ) ;
#19119 = ORIENTED_EDGE ( 'NONE', *, *, #10951, .F. ) ;
#19120 = DIRECTION ( 'NONE',  ( -1.000000000000000000, -0.000000000000000000, -0.000000000000000000 ) ) ;
#19121 = ORIENTED_EDGE ( 'NONE', *, *, #20303, .F. ) ;
#19122 = CARTESIAN_POINT ( 'NONE',  ( 10.00000000000000000, 35.53030884539102630, -12.26510123303222599 ) ) ;
#19123 = CARTESIAN_POINT ( 'NONE',  ( 92.69370383062501162, -211.3315407142195852, 76.36072916753381890 ) ) ;
#19124 = ORIENTED_EDGE ( 'NONE', *, *, #11186, .F. ) ;
#19125 = CARTESIAN_POINT ( 'NONE',  ( 92.69370383062501162, -208.6684592857803011, 79.58864583420047722 ) ) ;
#19126 = VECTOR ( 'NONE', #63124, 1000.000000000000114 ) ;
#19127 = VERTEX_POINT ( 'NONE', #28687 ) ;
#19128 = CARTESIAN_POINT ( 'NONE',  ( 93.67499999999999716, 87.70503267997126784, 79.31083333333333485 ) ) ;
#19129 = ORIENTED_EDGE ( 'NONE', *, *, #22169, .T. ) ;
#19130 = ORIENTED_EDGE ( 'NONE', *, *, #73732, .T. ) ;
#19131 = CYLINDRICAL_SURFACE ( 'NONE', #60976, 82.00000000000000000 ) ;
#19132 = CIRCLE ( 'NONE', #38348, 15.99999999999999822 ) ;
#19133 = DIRECTION ( 'NONE',  ( -1.000000000000000000, -0.000000000000000000, -0.000000000000000000 ) ) ;
#19134 = CIRCLE ( 'NONE', #7184, 82.00000000000000000 ) ;
#19135 = ORIENTED_EDGE ( 'NONE', *, *, #41227, .F. ) ;
#19136 = DIRECTION ( 'NONE',  ( 1.000000000000000000, 0.000000000000000000, -0.000000000000000000 ) ) ;
#19137 = CARTESIAN_POINT ( 'NONE',  ( 92.35000000000002274, -211.5299782133524502, 84.41729166840097776 ) ) ;
#19139 = AXIS2_PLACEMENT_3D ( 'NONE', #3053, #72897, #4523 ) ;
#19138 = CARTESIAN_POINT ( 'NONE',  ( 97.64999999999997726, 91.52997821335252127, 87.83041666666666458 ) ) ;
#19140 = ORIENTED_EDGE ( 'NONE', *, *, #36913, .T. ) ;
#19141 = DIRECTION ( 'NONE',  ( -1.000000000000000000, -0.000000000000000000, -0.000000000000000000 ) ) ;
#19142 = ORIENTED_EDGE ( 'NONE', *, *, #30753, .F. ) ;
#19143 = ORIENTED_EDGE ( 'NONE', *, *, #22939, .F. ) ;
#19144 =( BOUNDED_CURVE ( )  B_SPLINE_CURVE ( 2, ( #49097, #49469, #15258, #72021, #20535, #15638, #26902, #42726, #67133 ),
 .UNSPECIFIED., .F., .F. ) 
 B_SPLINE_CURVE_WITH_KNOTS ( ( 3, 2, 2, 2, 3 ),
 ( 0.4868478063929145838, 0.4939035878617653585, 0.5009593534026471895, 0.5080151189435290204, 0.5080151867253830389 ),
 .UNSPECIFIED. ) 
 CURVE ( )  GEOMETRIC_REPRESENTATION_ITEM ( )  RATIONAL_B_SPLINE_CURVE ( ( 1.000000000000000000, 0.8660254037844387076, 1.000000000000000000, 0.8660254037844387076, 1.000000000000000000, 0.8660254037844387076, 1.000000000000000000, 0.9999987129608440828, 0.9999974259464162740 ) ) 
 REPRESENTATION_ITEM ( '' )  );
#19145 = CARTESIAN_POINT ( 'NONE',  ( -93.84685191531252713, 88.00268892867056536, 88.74322916753382628 ) ) ;
#19146 = CARTESIAN_POINT ( 'NONE',  ( 92.69370383062498320, 88.66845928578037217, 84.61572916753380014 ) ) ;
#19147 = ORIENTED_EDGE ( 'NONE', *, *, #13259, .T. ) ;
#19148 = CARTESIAN_POINT ( 'NONE',  ( 96.32499999999998863, 87.70503267997126784, 87.75104166840095843 ) ) ;
#19149 = VERTEX_POINT ( 'NONE', #21944 ) ;
#19150 = CARTESIAN_POINT ( 'NONE',  ( -92.35000000000005116, 88.47002178664754979, 85.89895833506763267 ) ) ;
#19151 = ORIENTED_EDGE ( 'NONE', *, *, #18587, .T. ) ;
#19152 = EDGE_LOOP ( 'NONE', ( #32799, #27186, #16942, #65820 ) ) ;
#19153 = ORIENTED_EDGE ( 'NONE', *, *, #667, .F. ) ;
#19154 = CARTESIAN_POINT ( 'NONE',  ( -6.782329983125270800, 10.49999999999999467, -145.0000000000000000 ) ) ;
#19155 = CARTESIAN_POINT ( 'NONE',  ( 93.67499999999998295, 92.29496732002878900, 75.36854166840096525 ) ) ;
#19156 = CARTESIAN_POINT ( 'NONE',  ( -92.35000000000005116, 91.52997821335253548, 84.02041666666667652 ) ) ;
#19157 = EDGE_LOOP ( 'NONE', ( #60200, #56211, #43815, #6386 ) ) ;
#19158 = CARTESIAN_POINT ( 'NONE',  ( -97.64999999999996305, -209.9999999999999716, 90.00000000000000000 ) ) ;
#19159 = CARTESIAN_POINT ( 'NONE',  ( 10.00000000000000000, -73.73191006444582740, 14.66109333815435889 ) ) ;
#19160 = ORIENTED_EDGE ( 'NONE', *, *, #41446, .F. ) ;
#19161 = CARTESIAN_POINT ( 'NONE',  ( 93.67500000000001137, -212.2949673200287179, 85.02583333333332405 ) ) ;
#19162 = CARTESIAN_POINT ( 'NONE',  ( -97.30629616937497417, -208.6684592857803011, 81.33489583420048064 ) ) ;
#19163 = EDGE_LOOP ( 'NONE', ( #53467, #957, #5201, #19891 ) ) ;
#19164 = AXIS2_PLACEMENT_3D ( 'NONE', #68286, #43959, #66158 ) ;
#19165 = CARTESIAN_POINT ( 'NONE',  ( 0.000000000000000000, 33.17418723428333749, -17.67226234102790272 ) ) ;
#19166 = DIRECTION ( 'NONE',  ( 0.000000000000000000, 0.000000000000000000, 1.000000000000000000 ) ) ;
#19167 = DIRECTION ( 'NONE',  ( 0.000000000000000000, 0.000000000000000000, 1.000000000000000000 ) ) ;
#19168 = CARTESIAN_POINT ( 'NONE',  ( 0.000000000000000000, -23.16143007188376757, -73.95703589263997912 ) ) ;
#19169 = AXIS2_PLACEMENT_3D ( 'NONE', #72328, #3934, #20826 ) ;
#19170 = EDGE_CURVE ( 'NONE', #237, #61251, #36685, .T. ) ;
#19171 = VECTOR ( 'NONE', #35438, 1000.000000000000000 ) ;
#19172 = DIRECTION ( 'NONE',  ( 0.000000000000000000, 0.000000000000000000, 1.000000000000000000 ) ) ;
#19173 = ADVANCED_FACE ( 'NONE', ( #39244 ), #55788, .F. ) ;
#19174 = DIRECTION ( 'NONE',  ( -1.000000000000000000, 0.000000000000000000, 0.000000000000000000 ) ) ;
#19176 = VECTOR ( 'NONE', #30575, 1000.000000000000000 ) ;
#19175 = DIRECTION ( 'NONE',  ( 0.000000000000000000, 0.000000000000000000, 1.000000000000000000 ) ) ;
#19177 = DIRECTION ( 'NONE',  ( 0.000000000000000000, 0.3090169943749482839, -0.9510565162951533091 ) ) ;
#19178 = DIRECTION ( 'NONE',  ( -0.000000000000000000, -0.000000000000000000, -1.000000000000000000 ) ) ;
#19180 = EDGE_CURVE ( 'NONE', #729, #13831, #27192, .T. ) ;
#19179 = CARTESIAN_POINT ( 'NONE',  ( 0.000000000000000000, -0.8299999999999999600, -1.199999999999999956 ) ) ;
#19181 = CARTESIAN_POINT ( 'NONE',  ( -95.00000000000002842, 92.66308142843932671, 75.51406250086714067 ) ) ;
#19182 = DIRECTION ( 'NONE',  ( 1.000000000000000000, 0.000000000000000000, 0.000000000000000000 ) ) ;
#19183 = DIRECTION ( 'NONE',  ( -1.000000000000000000, -0.000000000000000000, -0.000000000000000000 ) ) ;
#19184 = EDGE_CURVE ( 'NONE', #1614, #633, #56542, .T. ) ;
#19185 = CARTESIAN_POINT ( 'NONE',  ( 0.000000000000000000, 0.000000000000000000, 0.000000000000000000 ) ) ;
#19186 = AXIS2_PLACEMENT_3D ( 'NONE', #72777, #14166, #38598 ) ;
#19187 = CYLINDRICAL_SURFACE ( 'NONE', #6478, 32.00000000000000000 ) ;
#19189 = DIRECTION ( 'NONE',  ( 0.000000000000000000, 0.000000000000000000, 1.000000000000000000 ) ) ;
#19188 = CIRCLE ( 'NONE', #16840, 31.99999999999999289 ) ;
#19190 = DIRECTION ( 'NONE',  ( -1.000000000000000000, 0.000000000000000000, -0.000000000000000000 ) ) ;
#19191 = DIRECTION ( 'NONE',  ( 0.000000000000000000, 0.000000000000000000, -1.000000000000000000 ) ) ;
#19192 = CARTESIAN_POINT ( 'NONE',  ( 0.000000000000000000, -16.65972982744991882, 80.28980883073752750 ) ) ;
#19193 = CARTESIAN_POINT ( 'NONE',  ( -93.67499999999998295, -207.7050326799711968, 87.88333333333332575 ) ) ;
#19194 = VECTOR ( 'NONE', #32715, 1000.000000000000000 ) ;
#19195 = AXIS2_PLACEMENT_3D ( 'NONE', #2968, #66103, #71709 ) ;
#19196 = EDGE_CURVE ( 'NONE', #23559, #24993, #10293, .T. ) ;
#19197 = CARTESIAN_POINT ( 'NONE',  ( 11.99999999999999822, 55.16347631943042984, 60.67117009219156643 ) ) ;
#19198 = ADVANCED_FACE ( 'NONE', ( #73055 ), #21563, .F. ) ;
#19199 = VERTEX_POINT ( 'NONE', #11041 ) ;
#19200 = DIRECTION ( 'NONE',  ( -1.000000000000000000, 0.000000000000000000, 0.000000000000000000 ) ) ;
#19201 = DIRECTION ( 'NONE',  ( -1.000000000000000000, -0.000000000000000000, -0.000000000000000000 ) ) ;
#19202 = DIRECTION ( 'NONE',  ( 0.000000000000000000, -0.1564344650402170189, -0.9876883405951399908 ) ) ;
#19203 = CARTESIAN_POINT ( 'NONE',  ( 10.00000000000000000, 77.49459641780886443, -0.8261519478433788644 ) ) ;
#19204 = CARTESIAN_POINT ( 'NONE',  ( 97.65000000000000568, 88.47002178664752137, 83.35895833506764063 ) ) ;
#19205 = VERTEX_POINT ( 'NONE', #28314 ) ;
#19206 = LINE ( 'NONE', #59813, #18018 ) ;
#19207 = VERTEX_POINT ( 'NONE', #51248 ) ;
#19208 = AXIS2_PLACEMENT_3D ( 'NONE', #17375, #62523, #10618 ) ;
#19209 = CARTESIAN_POINT ( 'NONE',  ( 93.84685191531249870, -208.0026889286704943, 83.82197916753381151 ) ) ;
#19210 = CARTESIAN_POINT ( 'NONE',  ( 93.84685191531249870, -208.0026889286704943, 89.06072916753382174 ) ) ;
#19211 = EDGE_LOOP ( 'NONE', ( #51948, #74242 ) ) ;
#19212 = CARTESIAN_POINT ( 'NONE',  ( 93.84685191531249870, -208.0026889286704943, 89.06072916753382174 ) ) ;
#19213 = CIRCLE ( 'NONE', #37221, 82.00000000000000000 ) ;
#19214 = VERTEX_POINT ( 'NONE', #24174 ) ;
#19215 = CARTESIAN_POINT ( 'NONE',  ( 0.000000000000000000, 33.17418723428333749, -17.67226234102790272 ) ) ;
#19216 = ORIENTED_EDGE ( 'NONE', *, *, #61962, .T. ) ;
#19217 = CARTESIAN_POINT ( 'NONE',  ( -93.84685191531252713, 88.00268892867056536, 80.48822916753381662 ) ) ;
#19218 = ORIENTED_EDGE ( 'NONE', *, *, #15788, .T. ) ;
#19219 = ORIENTED_EDGE ( 'NONE', *, *, #993, .T. ) ;
#19220 = AXIS2_PLACEMENT_3D ( 'NONE', #43220, #49198, #72128 ) ;
#19221 = CARTESIAN_POINT ( 'NONE',  ( 10.00000000000000000, -22.48208911017525580, 35.47612816024516036 ) ) ;
#19222 = EDGE_LOOP ( 'NONE', ( #44710, #66706, #14043, #53446 ) ) ;
#19223 = DIRECTION ( 'NONE',  ( 0.000000000000000000, 0.000000000000000000, -1.000000000000000000 ) ) ;
#19224 = VERTEX_POINT ( 'NONE', #51988 ) ;
#19225 = CARTESIAN_POINT ( 'NONE',  ( 10.00000000000000000, 37.01155633439059756, 6.555932627142549762 ) ) ;
#19226 = VERTEX_POINT ( 'NONE', #63667 ) ;
#19227 = DIRECTION ( 'NONE',  ( -1.000000000000000000, -0.000000000000000000, -0.000000000000000000 ) ) ;
#19228 = VERTEX_POINT ( 'NONE', #41457 ) ;
#19229 = EDGE_CURVE ( 'NONE', #45970, #32140, #6513, .T. ) ;
#19230 = VECTOR ( 'NONE', #66972, 1000.000000000000000 ) ;
#19231 = ORIENTED_EDGE ( 'NONE', *, *, #40951, .T. ) ;
#19232 = EDGE_LOOP ( 'NONE', ( #17830, #7844 ) ) ;
#19233 = CARTESIAN_POINT ( 'NONE',  ( 97.30629616937498838, -209.9999999999999716, 77.89531250086714920 ) ) ;
#19234 = CIRCLE ( 'NONE', #138, 12.49999999999999645 ) ;
#19235 = DIRECTION ( 'NONE',  ( -1.000000000000000000, 0.000000000000000000, 0.000000000000000000 ) ) ;
#19236 = ITEM_DEFINED_TRANSFORMATION ( 'NONE', 'NONE', #17185,  #43395 ) ;
#19237 = LINE ( 'NONE', #70353, #55784 ) ;
#19238 = VERTEX_POINT ( 'NONE', #1648 ) ;
#19239 = CARTESIAN_POINT ( 'NONE',  ( -21.33958957442910886, -129.9559990355020034, 5.500000000000000000 ) ) ;
#19240 = DIRECTION ( 'NONE',  ( -1.000000000000000000, 0.000000000000000000, 0.000000000000000000 ) ) ;
#19241 = CARTESIAN_POINT ( 'NONE',  ( 0.000000000000000000, -22.48208911017525580, 35.47612816024516036 ) ) ;
#19242 = EDGE_CURVE ( 'NONE', #18486, #64128, #52739, .T. ) ;
#19243 = DIRECTION ( 'NONE',  ( -1.000000000000000000, -0.000000000000000000, -0.000000000000000000 ) ) ;
#19244 = CARTESIAN_POINT ( 'NONE',  ( 92.34999999999998010, -208.4700217866475214, 76.61208333333333087 ) ) ;
#19245 = AXIS2_PLACEMENT_3D ( 'NONE', #17001, #12089, #23738 ) ;
#19246 = CARTESIAN_POINT ( 'NONE',  ( -96.15314808468747287, -208.0026889286704943, 80.64697916753381435 ) ) ;
#19247 = EDGE_CURVE ( 'NONE', #34378, #28286, #58374, .T. ) ;
#19248 = CARTESIAN_POINT ( 'NONE',  ( -93.84685191531252713, 88.00268892867056536, 79.21822916753382060 ) ) ;
#19249 = ORIENTED_EDGE ( 'NONE', *, *, #68606, .T. ) ;
#19250 = CARTESIAN_POINT ( 'NONE',  ( 96.15314808468748708, 88.00268892867053694, 82.23447916753380582 ) ) ;
#19251 = VERTEX_POINT ( 'NONE', #536 ) ;
#19252 = CARTESIAN_POINT ( 'NONE',  ( 2.500000000000000000, 16.00000000000000000, -19.01812422950394676 ) ) ;
#19253 = CARTESIAN_POINT ( 'NONE',  ( 10.00000000000000000, -5.256550761633413060, 77.32052557432841411 ) ) ;
#19254 = CARTESIAN_POINT ( 'NONE',  ( 97.64999999999996305, 90.00000034979572661, 77.69687501385438111 ) ) ;
#19255 = CARTESIAN_POINT ( 'NONE',  ( 0.000000000000000000, -74.65491531819124305, 8.830959090342128448 ) ) ;
#19256 = DIRECTION ( 'NONE',  ( -1.000000000000000000, 0.000000000000000000, -0.000000000000000000 ) ) ;
#19257 = CARTESIAN_POINT ( 'NONE',  ( -97.30629616937497417, -208.6684592857803295, 81.96989583420047154 ) ) ;
#19258 = EDGE_CURVE ( 'NONE', #45911, #70771, #63294, .T. ) ;
#19259 = DIRECTION ( 'NONE',  ( -1.000000000000000000, -0.000000000000000000, -0.000000000000000000 ) ) ;
#19260 = DIRECTION ( 'NONE',  ( 0.000000000000000000, 0.000000000000000000, 1.000000000000000000 ) ) ;
#19261 = FACE_OUTER_BOUND ( 'NONE', #66970, .T. ) ;
#19262 = ORIENTED_EDGE ( 'NONE', *, *, #18832, .F. ) ;
#19263 = EDGE_LOOP ( 'NONE', ( #32727, #33696, #5708, #29117 ) ) ;
#19264 = DIRECTION ( 'NONE',  ( -1.000000000000000000, -0.000000000000000000, 0.000000000000000000 ) ) ;
#19265 = CARTESIAN_POINT ( 'NONE',  ( 10.00000000000000000, 0.000000000000000000, 0.000000000000000000 ) ) ;
#19266 = LINE ( 'NONE', #65154, #71611 ) ;
#19267 = CARTESIAN_POINT ( 'NONE',  ( -97.30629616937501680, 91.33154071421968467, 84.50989583420046358 ) ) ;
#19268 = CARTESIAN_POINT ( 'NONE',  ( -95.78927932462332251, -207.7213858236420947, 74.85481846778735360 ) ) ;
#19269 = CARTESIAN_POINT ( 'NONE',  ( -100.0000000000260059, -214.9999999999999716, -64.99999999999350564 ) ) ;
#19270 = DIRECTION ( 'NONE',  ( 0.000000000000000000, -0.3826834323650774583, -0.9238795325112919565 ) ) ;
#19271 = DIRECTION ( 'NONE',  ( 0.000000000000000000, 0.000000000000000000, 1.000000000000000000 ) ) ;
#19272 = EDGE_CURVE ( 'NONE', #30261, #10249, #23432, .T. ) ;
#19273 = ORIENTED_EDGE ( 'NONE', *, *, #65187, .T. ) ;
#19274 = CARTESIAN_POINT ( 'NONE',  ( -95.00000000000002842, 92.66308142843932671, 76.14906250086716000 ) ) ;
#19275 = AXIS2_PLACEMENT_3D ( 'NONE', #57478, #33799, #17619 ) ;
#19276 = AXIS2_PLACEMENT_3D ( 'NONE', #51741, #11508, #5161 ) ;
#19277 = DIRECTION ( 'NONE',  ( 1.000000000000000000, 0.000000000000000000, -0.000000000000000000 ) ) ;
#19278 = CARTESIAN_POINT ( 'NONE',  ( 1.355716935723751293, -120.6418968688129496, -2.500000000000000000 ) ) ;
#19279 = LINE ( 'NONE', #24559, #14074 ) ;
#19280 = AXIS2_PLACEMENT_3D ( 'NONE', #8901, #53651, #8538 ) ;
#19281 = CARTESIAN_POINT ( 'NONE',  ( -97.64998344411672804, -208.4700122281038261, 79.23145767387356386 ) ) ;
#19282 = CARTESIAN_POINT ( 'NONE',  ( -96.15314808468747287, -208.0026889286704943, 87.15572916753382060 ) ) ;
#19283 = SURFACE_STYLE_FILL_AREA ( #14748 ) ;
#19284 = EDGE_CURVE ( 'NONE', #59685, #5395, #22256, .T. ) ;
#19285 = DIRECTION ( 'NONE',  ( 1.000000000000000000, -0.000000000000000000, 0.000000000000000000 ) ) ;
#19286 = EDGE_CURVE ( 'NONE', #11835, #53383, #69659, .T. ) ;
#19287 = EDGE_CURVE ( 'NONE', #44028, #33537, #15049, .T. ) ;
#19288 = DIRECTION ( 'NONE',  ( -1.000000000000000000, 0.000000000000000000, 0.000000000000000000 ) ) ;
#19289 = CARTESIAN_POINT ( 'NONE',  ( -97.30629616937497417, -208.6684592857803295, 76.41364583420049428 ) ) ;
#19290 = DIRECTION ( 'NONE',  ( -1.000000000000000000, -0.000000000000000000, -0.000000000000000000 ) ) ;
#19291 = ORIENTED_EDGE ( 'NONE', *, *, #49289, .T. ) ;
#19292 = CARTESIAN_POINT ( 'NONE',  ( -97.64999999999997726, -209.9999872712514275, 81.82437456149081356 ) ) ;
#19293 = CARTESIAN_POINT ( 'NONE',  ( 97.64999999999999147, 90.00000000000002842, 75.71250000000000568 ) ) ;
#19294 = CARTESIAN_POINT ( 'NONE',  ( -95.00000000000002842, 86.94004357329504273, 88.33312500173431658 ) ) ;
#19295 = CIRCLE ( 'NONE', #27719, 37.49900000000000944 ) ;
#19296 = CIRCLE ( 'NONE', #68524, 12.75000000000000000 ) ;
#19297 = AXIS2_PLACEMENT_3D ( 'NONE', #69545, #35337, #18398 ) ;
#19298 = FACE_OUTER_BOUND ( 'NONE', #65101, .T. ) ;
#19299 = CARTESIAN_POINT ( 'NONE',  ( 95.00000000000000000, -207.3369185715606307, 74.87906250086713555 ) ) ;
#19300 = ORIENTED_EDGE ( 'NONE', *, *, #73261, .F. ) ;
#19301 = CARTESIAN_POINT ( 'NONE',  ( 10.00000000000000000, 0.000000000000000000, 0.000000000000000000 ) ) ;
#19302 = CARTESIAN_POINT ( 'NONE',  ( 0.000000000000000000, 21.53537804866081373, 30.80686688397018358 ) ) ;
#19303 = ORIENTED_EDGE ( 'NONE', *, *, #41867, .T. ) ;
#19304 = CARTESIAN_POINT ( 'NONE',  ( 10.00000000000000000, 50.95692526931328104, 58.39081064771769292 ) ) ;
#19305 = EDGE_LOOP ( 'NONE', ( #4007, #50692, #61021, #39234 ) ) ;
#19306 = DIRECTION ( 'NONE',  ( -1.000000000000000000, 0.000000000000000000, 0.000000000000000000 ) ) ;
#19307 = EDGE_LOOP ( 'NONE', ( #60935, #44498, #885, #6833 ) ) ;
#19308 = VERTEX_POINT ( 'NONE', #53111 ) ;
#19309 = ORIENTED_EDGE ( 'NONE', *, *, #9312, .T. ) ;
#19310 = DIRECTION ( 'NONE',  ( 0.000000000000000000, 0.5877852522924684742, 0.8090169943749506709 ) ) ;
#19311 = ORIENTED_EDGE ( 'NONE', *, *, #2727, .F. ) ;
#19312 = VERTEX_POINT ( 'NONE', #12508 ) ;
#19313 = CARTESIAN_POINT ( 'NONE',  ( 96.15314808468748708, 88.00268892867053694, 79.21822916753382060 ) ) ;
#19314 = CARTESIAN_POINT ( 'NONE',  ( 95.00000000000000000, -213.0599564267049857, 88.96812500173430749 ) ) ;
#19315 = CARTESIAN_POINT ( 'NONE',  ( -10.00000000000000000, 0.000000000000000000, 0.000000000000000000 ) ) ;
#19316 = ORIENTED_EDGE ( 'NONE', *, *, #58131, .F. ) ;
#19317 = VERTEX_POINT ( 'NONE', #41100 ) ;
#19318 = EDGE_CURVE ( 'NONE', #60587, #20975, #57107, .T. ) ;
#19319 = CIRCLE ( 'NONE', #73296, 77.49899999999999523 ) ;
#19320 = ORIENTED_EDGE ( 'NONE', *, *, #55622, .T. ) ;
#19321 = CARTESIAN_POINT ( 'NONE',  ( 11.99999999999999822, 81.34940948281349904, -10.30890764327296161 ) ) ;
#19322 = CIRCLE ( 'NONE', #33721, 31.99999999999998579 ) ;
#19323 = ORIENTED_EDGE ( 'NONE', *, *, #19872, .T. ) ;
#19324 = DIRECTION ( 'NONE',  ( 1.347312414858667870E-17, 7.064000094680595780E-17, 1.000000000000000000 ) ) ;
#19325 = FACE_OUTER_BOUND ( 'NONE', #7219, .T. ) ;
#19326 = DIRECTION ( 'NONE',  ( 0.000000000000000000, 0.000000000000000000, 1.000000000000000000 ) ) ;
#19327 = LINE ( 'NONE', #71568, #73714 ) ;
#19328 = CARTESIAN_POINT ( 'NONE',  ( 1.250000000000000000, -12.36245420541525597, 0.000000000000000000 ) ) ;
#19329 = ADVANCED_FACE ( 'NONE', ( #6155 ), #35079, .T. ) ;
#19330 = DIRECTION ( 'NONE',  ( 0.000000000000000000, 0.000000000000000000, 1.000000000000000000 ) ) ;
#19331 = DIRECTION ( 'NONE',  ( 0.000000000000000000, 0.000000000000000000, 1.000000000000000000 ) ) ;
#19332 = CARTESIAN_POINT ( 'NONE',  ( -96.32499999999996021, -212.2949673200287179, 75.58020833506763836 ) ) ;
#19333 = EDGE_CURVE ( 'NONE', #6059, #35621, #60697, .T. ) ;
#19334 = DIRECTION ( 'NONE',  ( -1.000000000000000000, -0.000000000000000000, -0.000000000000000000 ) ) ;
#19336 = CARTESIAN_POINT ( 'NONE',  ( -95.00000000000002842, 86.94004357329504273, 76.26812500173430465 ) ) ;
#19335 = CARTESIAN_POINT ( 'NONE',  ( 93.67499999999998295, 92.29496732002878900, 75.36854166840096525 ) ) ;
#19337 = EDGE_LOOP ( 'NONE', ( #51866, #72938, #31540, #43952 ) ) ;
#19338 = CARTESIAN_POINT ( 'NONE',  ( 97.30629616937498838, 88.66845928578037217, 78.00114583420049996 ) ) ;
#19339 = CARTESIAN_POINT ( 'NONE',  ( 0.000000000000000000, -36.72794159290288718, 65.59268652807197952 ) ) ;
#19340 = CARTESIAN_POINT ( 'NONE',  ( -14.09999999999999964, 1.726751986797767995E-15, -1.199999999999999956 ) ) ;
#19341 = CARTESIAN_POINT ( 'NONE',  ( 92.35000000000000853, -208.4700217866474645, 77.32645833506762756 ) ) ;
#19342 = CARTESIAN_POINT ( 'NONE',  ( -3.000000000000002665, 2.549714635824789697E-15, -20.64000000000000057 ) ) ;
#19343 = AXIS2_PLACEMENT_3D ( 'NONE', #30359, #35276, #53305 ) ;
#19344 = CARTESIAN_POINT ( 'NONE',  ( 10.00000000000000000, -34.44570377933549565, -69.42325613327476219 ) ) ;
#19345 = EDGE_CURVE ( 'NONE', #21124, #53528, #63133, .T. ) ;
#19346 = ORIENTED_EDGE ( 'NONE', *, *, #12745, .T. ) ;
#19347 = DIRECTION ( 'NONE',  ( -0.000000000000000000, -0.000000000000000000, -1.000000000000000000 ) ) ;
#19348 = AXIS2_PLACEMENT_3D ( 'NONE', #52629, #1181, #24080 ) ;
#19349 = CARTESIAN_POINT ( 'NONE',  ( 2.600913415846943225E-12, -120.0000000000000000, -65.00000000000000000 ) ) ;
#19350 = ORIENTED_EDGE ( 'NONE', *, *, #57531, .F. ) ;
#19351 = AXIS2_PLACEMENT_3D ( 'NONE', #2198, #73439, #63296 ) ;
#19352 = VERTEX_POINT ( 'NONE', #12136 ) ;
#19353 = AXIS2_PLACEMENT_3D ( 'NONE', #42409, #48413, #14192 ) ;
#19354 = CARTESIAN_POINT ( 'NONE',  ( -97.64999999999996305, -209.9999999999999716, 90.00000000000000000 ) ) ;
#19355 = CARTESIAN_POINT ( 'NONE',  ( 11.99999999999999822, -41.19522573413780009, 65.64334221924896440 ) ) ;
#19356 = CARTESIAN_POINT ( 'NONE',  ( 97.65000000000000568, -208.4700217866474645, 87.90979166840097037 ) ) ;
#19357 = DIRECTION ( 'NONE',  ( -1.000000000000000000, 0.000000000000000000, 0.000000000000000000 ) ) ;
#19358 = DIRECTION ( 'NONE',  ( -0.000000000000000000, -0.000000000000000000, -1.000000000000000000 ) ) ;
#19359 =( BOUNDED_CURVE ( )  B_SPLINE_CURVE ( 2, ( #56195, #27618, #50546, #73470, #39281, #58790, #1684, #30204, #2050 ),
 .UNSPECIFIED., .F., .F. ) 
 B_SPLINE_CURVE_WITH_KNOTS ( ( 3, 2, 2, 2, 3 ),
 ( 0.2540073681283125939, 0.2540075594717653429, 0.2610633250126476734, 0.2681190905535300595, 0.2751748541904413536 ),
 .UNSPECIFIED. ) 
 CURVE ( )  GEOMETRIC_REPRESENTATION_ITEM ( )  RATIONAL_B_SPLINE_CURVE ( ( 0.9999927337532750204, 0.9999963667781091026, 1.000000000000000000, 0.8660254037844387076, 1.000000000000000000, 0.8660254037844387076, 1.000000000000000000, 0.8660254037844387076, 1.000000000000000000 ) ) 
 REPRESENTATION_ITEM ( '' )  );
#19360 = CARTESIAN_POINT ( 'NONE',  ( -96.15314808468745866, -211.9973110713294489, 75.30239583420048177 ) ) ;
#19361 = CIRCLE ( 'NONE', #4997, 31.99999999999998579 ) ;
#19362 = EDGE_CURVE ( 'NONE', #41055, #9960, #70376, .T. ) ;
#19363 = VERTEX_POINT ( 'NONE', #908 ) ;
#19364 = CARTESIAN_POINT ( 'NONE',  ( -10.00000000000000000, 0.000000000000000000, 0.000000000000000000 ) ) ;
#19365 = CYLINDRICAL_SURFACE ( 'NONE', #65474, 31.99999999999999289 ) ;
#19366 = DIRECTION ( 'NONE',  ( 1.000000000000000000, -0.000000000000000000, 0.000000000000000000 ) ) ;
#19367 = LINE ( 'NONE', #18989, #50019 ) ;
#19368 = DIRECTION ( 'NONE',  ( 0.000000000000000000, 0.5877852522924685852, 0.8090169943749508930 ) ) ;
#19369 = DIRECTION ( 'NONE',  ( 0.000000000000000000, -0.000000000000000000, 1.000000000000000000 ) ) ;
#19370 = DIRECTION ( 'NONE',  ( -1.000000000000000000, 0.000000000000000000, 0.000000000000000000 ) ) ;
#19371 = CARTESIAN_POINT ( 'NONE',  ( -97.64999999999996305, -209.9999999999999716, 76.03000000000000114 ) ) ;
#19372 = DIRECTION ( 'NONE',  ( -1.000000000000000000, 0.000000000000000000, -0.000000000000000000 ) ) ;
#19373 = EDGE_CURVE ( 'NONE', #61374, #73431, #23795, .T. ) ;
#19374 = EDGE_CURVE ( 'NONE', #5475, #20114, #57144, .T. ) ;
#19375 = CARTESIAN_POINT ( 'NONE',  ( 97.30629616937498838, 90.00000000000002842, 84.40406250086715545 ) ) ;
#19376 = CARTESIAN_POINT ( 'NONE',  ( -93.84685191531248449, -208.0026889286704943, 87.04989583420048405 ) ) ;
#19377 = CARTESIAN_POINT ( 'NONE',  ( 92.35000000007821086, 90.00001303125209517, 79.28395951162845279 ) ) ;
#19378 = EDGE_LOOP ( 'NONE', ( #43002, #38947, #66438, #2082 ) ) ;
#19379 = DIRECTION ( 'NONE',  ( -1.000000000000000000, -0.000000000000000000, -0.000000000000000000 ) ) ;
#19380 = VECTOR ( 'NONE', #68088, 1000.000000000000000 ) ;
#19381 = CARTESIAN_POINT ( 'NONE',  ( -92.34999999999999432, -209.9999999999999716, 81.42749999999999488 ) ) ;
#19382 = CARTESIAN_POINT ( 'NONE',  ( -96.15314808468751551, 88.00268892867056536, 76.41364583420048007 ) ) ;
#19383 = CIRCLE ( 'NONE', #24179, 4.750000000000000000 ) ;
#19384 = CIRCLE ( 'NONE', #38609, 32.00000000000000000 ) ;
#19385 = CARTESIAN_POINT ( 'NONE',  ( 92.69370383062501162, -208.6684592857803011, 88.31989583420046586 ) ) ;
#19386 = ORIENTED_EDGE ( 'NONE', *, *, #8056, .F. ) ;
#19387 = AXIS2_PLACEMENT_3D ( 'NONE', #42376, #71667, #49115 ) ;
#19388 = PRESENTATION_STYLE_ASSIGNMENT (( #25413 ) ) ;
#19389 = ORIENTED_EDGE ( 'NONE', *, *, #2828, .F. ) ;
#19390 = ORIENTED_EDGE ( 'NONE', *, *, #73574, .F. ) ;
#19391 = CIRCLE ( 'NONE', #70965, 15.77977592589476608 ) ;
#19392 = CARTESIAN_POINT ( 'NONE',  ( 10.00000000000000000, 74.65491531819118620, -8.830959090342659579 ) ) ;
#19394 = CARTESIAN_POINT ( 'NONE',  ( 10.00000000000000000, 33.79645857604513992, -16.45098606841138178 ) ) ;
#19393 = VECTOR ( 'NONE', #26911, 1000.000000000000000 ) ;
#19395 = CIRCLE ( 'NONE', #24203, 31.99999999999998579 ) ;
#19396 = ORIENTED_EDGE ( 'NONE', *, *, #5951, .F. ) ;
#19397 = DIRECTION ( 'NONE',  ( 0.000000000000000000, -9.787530781167598712E-16, -1.000000000000000000 ) ) ;
#19398 = CARTESIAN_POINT ( 'NONE',  ( 96.15314808468748708, -208.0026889286704943, 80.06489583420048461 ) ) ;
#19399 = CARTESIAN_POINT ( 'NONE',  ( -3.360000000000002096, 0.000000000000000000, -21.00000000000000000 ) ) ;
#19400 = CARTESIAN_POINT ( 'NONE',  ( -95.00000000000002842, 93.05995642670504253, 76.58562500173430010 ) ) ;
#19401 = CARTESIAN_POINT ( 'NONE',  ( 0.000000000000000000, -33.80338159004273280, -16.23288003029533044 ) ) ;
#19402 = FACE_OUTER_BOUND ( 'NONE', #11747, .T. ) ;
#19403 = CARTESIAN_POINT ( 'NONE',  ( 10.00000000000000000, 55.20638768913760686, 51.02545421589343988 ) ) ;
#19404 = CARTESIAN_POINT ( 'NONE',  ( 92.35000000000000853, -209.9999999999999716, 80.47499999999999432 ) ) ;
#19405 = EDGE_CURVE ( 'NONE', #36301, #20472, #2965, .T. ) ;
#19406 = VERTEX_POINT ( 'NONE', #33827 ) ;
#19407 = EDGE_LOOP ( 'NONE', ( #46223, #33024, #37291, #41105 ) ) ;
#19408 = ORIENTED_EDGE ( 'NONE', *, *, #63107, .T. ) ;
#19409 = ORIENTED_EDGE ( 'NONE', *, *, #51082, .F. ) ;
#19410 = CARTESIAN_POINT ( 'NONE',  ( 97.64999999999999147, -209.9999999999999716, 87.14249999999999829 ) ) ;
#19411 = EDGE_CURVE ( 'NONE', #23675, #8687, #4237, .T. ) ;
#19412 = CARTESIAN_POINT ( 'NONE',  ( -96.15314808468751551, 88.00268892867056536, 82.92239583420048632 ) ) ;
#19413 = DIRECTION ( 'NONE',  ( 0.000000000000000000, -0.3090169943749349057, -0.9510565162951577500 ) ) ;
#19414 = LINE ( 'NONE', #3271, #54633 ) ;
#19415 = ADVANCED_FACE ( 'NONE', ( #45123 ), #28926, .T. ) ;
#19416 = FACE_OUTER_BOUND ( 'NONE', #8458, .T. ) ;
#19417 = ORIENTED_EDGE ( 'NONE', *, *, #9838, .F. ) ;
#19418 = CARTESIAN_POINT ( 'NONE',  ( -92.34999999999999432, -209.9999999999999716, 89.12687500173430521 ) ) ;
#19419 = ORIENTED_EDGE ( 'NONE', *, *, #544, .F. ) ;
#19420 = DIRECTION ( 'NONE',  ( 1.000000000000000000, 0.000000000000000000, 0.000000000000000000 ) ) ;
#19421 = VERTEX_POINT ( 'NONE', #51485 ) ;
#19422 = CARTESIAN_POINT ( 'NONE',  ( -93.67500000000003979, 92.29496732002878900, 85.42270833506762528 ) ) ;
#19423 = CARTESIAN_POINT ( 'NONE',  ( 97.30629616937498838, 91.33154071421968467, 86.36197916753383197 ) ) ;
#19424 = DIRECTION ( 'NONE',  ( -1.000000000000000000, -0.000000000000000000, 0.000000000000000000 ) ) ;
#19425 = CARTESIAN_POINT ( 'NONE',  ( -93.14543241548912533, 88.62117599715713823, 74.79348190356850523 ) ) ;
#19426 = FACE_OUTER_BOUND ( 'NONE', #13152, .T. ) ;
#19427 = EDGE_CURVE ( 'NONE', #19829, #35960, #73665, .T. ) ;
#19428 = COLOUR_RGB ( '', 0.31764706, 0.68627451, 0.89019608) ;
#19429 = AXIS2_PLACEMENT_3D ( 'NONE', #71032, #2667, #64669 ) ;
#19430 = DIRECTION ( 'NONE',  ( -1.000000000000000000, -0.000000000000000000, -0.000000000000000000 ) ) ;
#19431 = ORIENTED_EDGE ( 'NONE', *, *, #4077, .F. ) ;
#19432 = CARTESIAN_POINT ( 'NONE',  ( 10.00000000000000000, 75.11764819372149304, 29.05362095685338986 ) ) ;
#19433 = CARTESIAN_POINT ( 'NONE',  ( -97.30629616937497417, -211.3315407142195852, 75.72572916753381378 ) ) ;
#19434 = EDGE_LOOP ( 'NONE', ( #73105, #4030, #2643, #30954 ) ) ;
#19435 = VERTEX_POINT ( 'NONE', #6024 ) ;
#19436 = DIRECTION ( 'NONE',  ( -1.000000000000000000, -0.000000000000000000, 0.000000000000000000 ) ) ;
#19437 = VECTOR ( 'NONE', #25729, 1000.000000000000000 ) ;
#19438 = CARTESIAN_POINT ( 'NONE',  ( 10.00000000000000000, -63.18004540533059554, 44.88180994100355292 ) ) ;
#19439 = EDGE_CURVE ( 'NONE', #6126, #6388, #69161, .T. ) ;
#19440 = CARTESIAN_POINT ( 'NONE',  ( 1.560000000000000053, 0.000000000000000000, 2.999999999999998668 ) ) ;
#19441 = VECTOR ( 'NONE', #34032, 1000.000000000000000 ) ;
#19442 = CARTESIAN_POINT ( 'NONE',  ( -97.30629616937497417, -211.3315407142195852, 89.21947916753381946 ) ) ;
#19443 = VERTEX_POINT ( 'NONE', #16533 ) ;
#19444 = ADVANCED_FACE ( 'NONE', ( #22937 ), #5284, .F. ) ;
#19445 = EDGE_LOOP ( 'NONE', ( #4190, #63960, #47593, #45233 ) ) ;
#19446 = EDGE_CURVE ( 'NONE', #26473, #70907, #10516, .T. ) ;
#19447 = ORIENTED_EDGE ( 'NONE', *, *, #26738, .F. ) ;
#19448 = LINE ( 'NONE', #3305, #52239 ) ;
#19449 = CIRCLE ( 'NONE', #20638, 15.50000000000000000 ) ;
#19450 = ADVANCED_FACE ( 'NONE', ( #63165 ), #10905, .T. ) ;
#19451 = EDGE_CURVE ( 'NONE', #46991, #35660, #17366, .T. ) ;
#19452 = AXIS2_PLACEMENT_3D ( 'NONE', #57728, #6946, #18232 ) ;
#19453 = CARTESIAN_POINT ( 'NONE',  ( 97.30629616937498838, 91.33154071421968467, 88.90197916753382401 ) ) ;
#19454 = DIRECTION ( 'NONE',  ( -1.000000000000000000, 0.000000000000000000, 0.000000000000000000 ) ) ;
#19455 = CARTESIAN_POINT ( 'NONE',  ( 93.84685191531248449, 91.99731107132950569, 80.64697916753381435 ) ) ;
#19456 = LINE ( 'NONE', #54053, #29264 ) ;
#19457 = PLANE ( 'NONE',  #44628 ) ;
#19458 = CARTESIAN_POINT ( 'NONE',  ( 0.000000000000000000, 73.95703589264006439, -23.16143007188350822 ) ) ;
#19459 = CARTESIAN_POINT ( 'NONE',  ( 0.000000000000000000, 22.64427369931169309, 30.00120703465213623 ) ) ;
#19460 = CYLINDRICAL_SURFACE ( 'NONE', #50809, 77.49899999999999523 ) ;
#19461 = CARTESIAN_POINT ( 'NONE',  ( 4.828573329308747830, 2.985724580418001928, -1.878862934774779836 ) ) ;
#19462 = CYLINDRICAL_SURFACE ( 'NONE', #9879, 31.99999999999999289 ) ;
#19463 = EDGE_CURVE ( 'NONE', #61855, #58186, #25743, .T. ) ;
#19464 = DIRECTION ( 'NONE',  ( 0.000000000000000000, 0.000000000000000000, 1.000000000000000000 ) ) ;
#19465 = ADVANCED_FACE ( 'NONE', ( #4913 ), #27813, .T. ) ;
#19466 = DIRECTION ( 'NONE',  ( -0.000000000000000000, -0.000000000000000000, 1.000000000000000000 ) ) ;
#19467 = ORIENTED_EDGE ( 'NONE', *, *, #33809, .T. ) ;
#19468 = CARTESIAN_POINT ( 'NONE',  ( -92.69370383062505425, 91.33154071421968467, 87.47322916753380184 ) ) ;
#19469 = DIRECTION ( 'NONE',  ( -0.9227826878668540234, -0.3853207896976547642, 0.000000000000000000 ) ) ;
#19470 = LINE ( 'NONE', #42414, #1291 ) ;
#19471 = PRODUCT_DEFINITION_SHAPE ( 'NONE', 'NONE',  #74352 ) ;
#19472 = EDGE_LOOP ( 'NONE', ( #11216, #10451, #56146, #47458 ) ) ;
#19473 = DIRECTION ( 'NONE',  ( 0.000000000000000000, 0.000000000000000000, -1.000000000000000000 ) ) ;
#19474 = CARTESIAN_POINT ( 'NONE',  ( -20.30386590532152979, -102.9045904027214959, 5.500000000000000000 ) ) ;
#19475 = CARTESIAN_POINT ( 'NONE',  ( 6.000000000000000000, 78.73519480814985627, -22.90783923731547489 ) ) ;
#19476 = CARTESIAN_POINT ( 'NONE',  ( 95.00000000000000000, -207.3369185715606307, 80.75281250086715090 ) ) ;
#19477 = VECTOR ( 'NONE', #11595, 1000.000000000000114 ) ;
#19478 = ORIENTED_EDGE ( 'NONE', *, *, #47609, .T. ) ;
#19479 = EDGE_LOOP ( 'NONE', ( #73778, #12108, #9920, #68868 ) ) ;
#19480 = AXIS2_PLACEMENT_3D ( 'NONE', #35903, #59217, #17245 ) ;
#19481 = DIRECTION ( 'NONE',  ( -1.000000000000000000, 0.000000000000000000, 0.000000000000000000 ) ) ;
#19482 = ORIENTED_EDGE ( 'NONE', *, *, #7259, .T. ) ;
#19483 = CARTESIAN_POINT ( 'NONE',  ( -1.433254160131044044E-14, -1.896421744167617418E-13, -18.00000000000031974 ) ) ;
#19484 = CIRCLE ( 'NONE', #29155, 32.00000000000000000 ) ;
#19485 = FACE_OUTER_BOUND ( 'NONE', #60642, .T. ) ;
#19486 = ORIENTED_EDGE ( 'NONE', *, *, #42475, .F. ) ;
#19487 = CARTESIAN_POINT ( 'NONE',  ( 93.84685191531249870, -208.0026889286704943, 79.53572916753381605 ) ) ;
#19488 = ORIENTED_EDGE ( 'NONE', *, *, #46860, .F. ) ;
#19489 = EDGE_CURVE ( 'NONE', #66589, #14702, #71330, .T. ) ;
#19490 = DIRECTION ( 'NONE',  ( -1.000000000000000000, -0.000000000000000000, 0.000000000000000000 ) ) ;
#19491 = ORIENTED_EDGE ( 'NONE', *, *, #6774, .F. ) ;
#19492 = VECTOR ( 'NONE', #41982, 1000.000000000000000 ) ;
#19493 = ORIENTED_EDGE ( 'NONE', *, *, #48397, .T. ) ;
#19494 = PLANE ( 'NONE',  #17772 ) ;
#19495 = AXIS2_PLACEMENT_3D ( 'NONE', #3480, #33496, #66258 ) ;
#19496 = EDGE_CURVE ( 'NONE', #36613, #62068, #8943, .T. ) ;
#19497 = DIRECTION ( 'NONE',  ( 0.000000000000000000, 0.9876883405951371042, 0.1564344650402346715 ) ) ;
#19498 = EDGE_LOOP ( 'NONE', ( #27082, #15706, #21413, #12143 ) ) ;
#19499 = DIRECTION ( 'NONE',  ( 0.000000000000000000, 0.000000000000000000, -1.000000000000000000 ) ) ;
#19500 = CARTESIAN_POINT ( 'NONE',  ( 93.67500000000001137, -212.2949673200287179, 82.56520833506762358 ) ) ;
#19501 = EDGE_CURVE ( 'NONE', #70242, #61868, #16919, .T. ) ;
#19502 = CARTESIAN_POINT ( 'NONE',  ( 92.34999999999999432, 91.52997821335252127, 86.77208333333334167 ) ) ;
#19503 = EDGE_CURVE ( 'NONE', #36972, #56117, #57592, .T. ) ;
#19504 = ORIENTED_EDGE ( 'NONE', *, *, #17175, .T. ) ;
#19505 = CARTESIAN_POINT ( 'NONE',  ( 1.433254160131044044E-14, 1.918465386552270249E-13, 18.00000000000031974 ) ) ;
#19506 = DIRECTION ( 'NONE',  ( -1.000000000000000000, 0.000000000000000000, 0.000000000000000000 ) ) ;
#19507 = ORIENTED_EDGE ( 'NONE', *, *, #42354, .F. ) ;
#19508 = VERTEX_POINT ( 'NONE', #42434 ) ;
#19509 = CARTESIAN_POINT ( 'NONE',  ( -97.30629616937501680, 90.00000000000004263, 87.26156250086715715 ) ) ;
#19510 = CARTESIAN_POINT ( 'NONE',  ( 97.30629616937498838, 91.33154071421968467, 83.02822916753379445 ) ) ;
#19511 = VERTEX_POINT ( 'NONE', #36406 ) ;
#19512 = CARTESIAN_POINT ( 'NONE',  ( 97.64999999999999147, 90.00000000000002842, 87.22187500173430408 ) ) ;
#19513 =( NAMED_UNIT ( * ) PLANE_ANGLE_UNIT ( ) SI_UNIT ( $, .RADIAN. ) );
#19514 = ORIENTED_EDGE ( 'NONE', *, *, #51883, .T. ) ;
#19515 = CARTESIAN_POINT ( 'NONE',  ( 95.00000000000000000, -206.9400435732949575, 87.38062500173430180 ) ) ;
#19516 = ORIENTED_EDGE ( 'NONE', *, *, #49318, .F. ) ;
#19517 = ORIENTED_EDGE ( 'NONE', *, *, #28659, .F. ) ;
#19518 = ADVANCED_FACE ( 'NONE', ( #57881 ), #6383, .T. ) ;
#19519 = ORIENTED_EDGE ( 'NONE', *, *, #32334, .F. ) ;
#19520 = CARTESIAN_POINT ( 'NONE',  ( 0.000000000000000000, 0.000000000000000000, -44.99999999999998579 ) ) ;
#19521 = CARTESIAN_POINT ( 'NONE',  ( 12.00000000000000000, -19.89357724624986545, 12.59942793731086219 ) ) ;
#19522 = EDGE_CURVE ( 'NONE', #57541, #69025, #24763, .T. ) ;
#19523 = CARTESIAN_POINT ( 'NONE',  ( -93.67500000000003979, 87.70503267997129626, 85.13166666666666060 ) ) ;
#19524 = ORIENTED_EDGE ( 'NONE', *, *, #54561, .T. ) ;
#19525 = CARTESIAN_POINT ( 'NONE',  ( -92.35000000002612808, 89.99999999999992895, -64.99999999999992895 ) ) ;
#19526 = DIRECTION ( 'NONE',  ( 0.000000000000000000, 0.9238795325112877377, -0.3826834323650873948 ) ) ;
#19527 = ORIENTED_EDGE ( 'NONE', *, *, #4268, .T. ) ;
#19528 = CARTESIAN_POINT ( 'NONE',  ( -8.826826895187510402, -94.96827758698185562, -2.500000000000000444 ) ) ;
#19529 = CARTESIAN_POINT ( 'NONE',  ( -97.30629616937497417, -211.3315407142195852, 82.71072916753379900 ) ) ;
#19530 = ORIENTED_EDGE ( 'NONE', *, *, #42382, .F. ) ;
#19531 = CARTESIAN_POINT ( 'NONE',  ( 1.384174031800307736, -119.4220188154534981, 2.500000000000000000 ) ) ;
#19532 = CARTESIAN_POINT ( 'NONE',  ( 11.99999999999999822, 0.000000000000000000, 0.000000000000000000 ) ) ;
#19533 = CARTESIAN_POINT ( 'NONE',  ( 10.00000000000000000, -68.26794271651239399, -31.47745569255214093 ) ) ;
#19534 = DIRECTION ( 'NONE',  ( -1.000000000000000000, 3.061616997868382648E-16, 0.000000000000000000 ) ) ;
#19535 = CARTESIAN_POINT ( 'NONE',  ( 10.00000000000000000, -22.64427369931191336, 30.00120703465197280 ) ) ;
#19536 = EDGE_CURVE ( 'NONE', #59117, #68357, #30560, .T. ) ;
#19537 = ADVANCED_FACE ( 'NONE', ( #29286 ), #13106, .T. ) ;
#19538 = AXIS2_PLACEMENT_3D ( 'NONE', #18925, #41872, #41142 ) ;
#19539 = CARTESIAN_POINT ( 'NONE',  ( -3.000000000000000000, 16.83928648764923253, 16.46020748918050458 ) ) ;
#19540 = DIRECTION ( 'NONE',  ( 0.000000000000000000, 0.000000000000000000, 1.000000000000000000 ) ) ;
#19541 = CARTESIAN_POINT ( 'NONE',  ( 10.00000000000000000, 37.16516213103277977, 4.992566952385115719 ) ) ;
#19542 = CARTESIAN_POINT ( 'NONE',  ( 92.34999999999999432, 91.52997821335252127, 83.04145833506764518 ) ) ;
#19543 = DIRECTION ( 'NONE',  ( -0.000000000000000000, 0.5877852522924696954, 0.8090169943749498938 ) ) ;
#19544 = CARTESIAN_POINT ( 'NONE',  ( -97.30629616937501680, 91.33154071421968467, 75.61989583420047722 ) ) ;
#19545 = DIRECTION ( 'NONE',  ( 1.000000000000000000, 0.000000000000000000, -0.000000000000000000 ) ) ;
#19546 = FACE_OUTER_BOUND ( 'NONE', #68857, .T. ) ;
#19547 = VECTOR ( 'NONE', #10061, 1000.000000000000114 ) ;
#19548 = CARTESIAN_POINT ( 'NONE',  ( -3.000000000000000000, -10.45096189432344147, 21.10159698893426494 ) ) ;
#19549 = UNCERTAINTY_MEASURE_WITH_UNIT (LENGTH_MEASURE( 1.000000000000000082E-05 ), #25581, 'distance_accuracy_value', 'NONE');
#19550 = DIRECTION ( 'NONE',  ( 0.000000000000000000, 0.000000000000000000, -1.000000000000000000 ) ) ;
#19551 = CIRCLE ( 'NONE', #25567, 11.59999999999999787 ) ;
#19552 = PLANE ( 'NONE',  #8880 ) ;
#19553 = CYLINDRICAL_SURFACE ( 'NONE', #9425, 35.50000000000001421 ) ;
#19554 = VECTOR ( 'NONE', #69490, 999.9999999999998863 ) ;
#19555 = DIRECTION ( 'NONE',  ( -1.000000000000000000, 3.061616997868382648E-16, 0.000000000000000000 ) ) ;
#19556 = CYLINDRICAL_SURFACE ( 'NONE', #68238, 31.99999999999998579 ) ;
#19557 = CARTESIAN_POINT ( 'NONE',  ( 92.35001423713268309, 88.47001356683512086, 75.52729223699087413 ) ) ;
#19558 = CARTESIAN_POINT ( 'NONE',  ( -93.67499999999998295, -212.2949673200287179, 87.03666666666666174 ) ) ;
#19559 = CARTESIAN_POINT ( 'NONE',  ( -11.59999999999999787, 0.000000000000000000, 53.20000000000001705 ) ) ;
#19560 = ORIENTED_EDGE ( 'NONE', *, *, #8990, .F. ) ;
#19561 = LINE ( 'NONE', #59429, #14305 ) ;
#19562 = DIRECTION ( 'NONE',  ( 0.8225049752423776450, 0.5687579148473765889, 0.000000000000000000 ) ) ;
#19563 = CARTESIAN_POINT ( 'NONE',  ( -97.64999999994218172, 89.99998877583867340, 75.47473230081648410 ) ) ;
#19564 = CARTESIAN_POINT ( 'NONE',  ( -12.40464318976452596, 10.41032311384371489, 42.00000000000001421 ) ) ;
#19565 = VERTEX_POINT ( 'NONE', #18375 ) ;
#19566 = LINE ( 'NONE', #31587, #61112 ) ;
#19567 = DIRECTION ( 'NONE',  ( 0.000000000000000000, -0.8526401643540860720, -0.5224985647159589019 ) ) ;
#19568 = VERTEX_POINT ( 'NONE', #41683 ) ;
#19569 = AXIS2_PLACEMENT_3D ( 'NONE', #70485, #53971, #25395 ) ;
#19570 =( BOUNDED_CURVE ( )  B_SPLINE_CURVE ( 2, ( #6497, #34313, #17032, #46717, #69640, #5763, #6137 ),
 .UNSPECIFIED., .F., .F. ) 
 B_SPLINE_CURVE_WITH_KNOTS ( ( 3, 2, 2, 3 ),
 ( 0.3541666666666665741, 0.3611111111111109939, 0.3680555555555554137, 0.3749999999999998335 ),
 .UNSPECIFIED. ) 
 CURVE ( )  GEOMETRIC_REPRESENTATION_ITEM ( )  RATIONAL_B_SPLINE_CURVE ( ( 1.000000000000002220, 0.8660254037844365982, 1.000000000000000000, 0.8660254037844387076, 1.000000000000000000, 0.8660254037844419273, 0.9999999999999967804 ) ) 
 REPRESENTATION_ITEM ( '' )  );
#19571 = CARTESIAN_POINT ( 'NONE',  ( 95.00000000000000000, -207.3369185715606307, 83.13406250086714522 ) ) ;
#19572 = CARTESIAN_POINT ( 'NONE',  ( 97.30629616937498838, -208.6684592857803295, 87.63197916753381378 ) ) ;
#19573 = ORIENTED_EDGE ( 'NONE', *, *, #23372, .F. ) ;
#19574 = ADVANCED_FACE ( 'NONE', ( #64261 ), #41321, .F. ) ;
#19575 = CARTESIAN_POINT ( 'NONE',  ( 95.00000000000000000, -207.3369185715606307, 88.37281250086715545 ) ) ;
#19576 = ORIENTED_EDGE ( 'NONE', *, *, #73317, .T. ) ;
#19577 = EDGE_CURVE ( 'NONE', #55579, #61669, #69520, .T. ) ;
#19578 = FACE_OUTER_BOUND ( 'NONE', #58275, .T. ) ;
#19579 = EDGE_LOOP ( 'NONE', ( #35247, #18678, #21199, #46077 ) ) ;
#19580 = CARTESIAN_POINT ( 'NONE',  ( -92.69370383062502583, 88.66845928578038638, 76.09614583420048461 ) ) ;
#19581 = AXIS2_PLACEMENT_3D ( 'NONE', #32235, #65372, #42803 ) ;
#19582 = ORIENTED_EDGE ( 'NONE', *, *, #4422, .T. ) ;
#19583 = EDGE_CURVE ( 'NONE', #12638, #15647, #63019, .T. ) ;
#19584 = ORIENTED_EDGE ( 'NONE', *, *, #46762, .T. ) ;
#19585 = DIRECTION ( 'NONE',  ( -1.000000000000000000, -0.000000000000000000, 0.000000000000000000 ) ) ;
#19586 = ORIENTED_EDGE ( 'NONE', *, *, #54065, .T. ) ;
#19587 = CARTESIAN_POINT ( 'NONE',  ( 92.34999999999999432, 89.99999348150291212, 88.17437522718662990 ) ) ;
#19588 = CARTESIAN_POINT ( 'NONE',  ( 10.00000000000000000, -72.35160999960801576, -20.41045688087902121 ) ) ;
#19589 = ADVANCED_FACE ( 'NONE', ( #46966 ), #12369, .F. ) ;
#19590 = VERTEX_POINT ( 'NONE', #69878 ) ;
#19591 = CARTESIAN_POINT ( 'NONE',  ( 94.99999999999998579, 90.00000000000002842, 90.00000000000000000 ) ) ;
#19592 = EDGE_LOOP ( 'NONE', ( #15190, #2286, #16945, #17739 ) ) ;
#19593 = CARTESIAN_POINT ( 'NONE',  ( 97.65000000000006253, -211.5299782133523934, 86.45458333333331780 ) ) ;
#19594 = EDGE_CURVE ( 'NONE', #54186, #47415, #64621, .T. ) ;
#19595 = VECTOR ( 'NONE', #2137, 1000.000000000000000 ) ;
#19596 = ORIENTED_EDGE ( 'NONE', *, *, #55280, .T. ) ;
#19597 = ORIENTED_EDGE ( 'NONE', *, *, #55538, .T. ) ;
#19598 = VECTOR ( 'NONE', #73266, 1000.000000000000000 ) ;
#19599 = ORIENTED_EDGE ( 'NONE', *, *, #51162, .T. ) ;
#19600 = CARTESIAN_POINT ( 'NONE',  ( 96.15314808468748708, -208.0026889286704943, 79.27114583420046756 ) ) ;
#19601 = AXIS2_PLACEMENT_3D ( 'NONE', #20291, #25566, #72163 ) ;
#19602 = CARTESIAN_POINT ( 'NONE',  ( 10.00000000000000000, 23.16143007188532366, -73.95703589263949596 ) ) ;
#19603 = CARTESIAN_POINT ( 'NONE',  ( 0.000000000000000000, 55.20638768913760686, 51.02545421589343988 ) ) ;
#19604 = VERTEX_POINT ( 'NONE', #48072 ) ;
#19605 = CARTESIAN_POINT ( 'NONE',  ( -0.2999999999999947153, 1.530808498934191521E-15, 12.50000000000000000 ) ) ;
#19606 = ORIENTED_EDGE ( 'NONE', *, *, #1593, .T. ) ;
#19607 = CARTESIAN_POINT ( 'NONE',  ( -92.35000000000016485, 88.47002178664749295, 80.73958333333335702 ) ) ;
#19608 = DIRECTION ( 'NONE',  ( -0.000000000000000000, -0.000000000000000000, 1.000000000000000000 ) ) ;
#19609 = CYLINDRICAL_SURFACE ( 'NONE', #4898, 2.649999999999985700 ) ;
#19610 = CARTESIAN_POINT ( 'NONE',  ( -7.499999999999969802, 76.30000000000001137, -204.9999999999999716 ) ) ;
#19611 = CARTESIAN_POINT ( 'NONE',  ( -97.30629616937497417, -208.6684592857803011, 80.69989583420048973 ) ) ;
#19612 = EDGE_CURVE ( 'NONE', #59733, #21161, #24397, .T. ) ;
#19613 = CARTESIAN_POINT ( 'NONE',  ( -95.00000000000002842, 87.33691857156074434, 78.53031250086715431 ) ) ;
#19614 = EDGE_CURVE ( 'NONE', #25706, #57093, #1513, .T. ) ;
#19615 = VERTEX_POINT ( 'NONE', #58988 ) ;
#19616 = CARTESIAN_POINT ( 'NONE',  ( 92.69370383062498320, 88.66845928578037217, 82.71072916753379900 ) ) ;
#19617 = VERTEX_POINT ( 'NONE', #70235 ) ;
#19618 = DIRECTION ( 'NONE',  ( 1.000000000000000000, 0.000000000000000000, 0.000000000000000000 ) ) ;
#19619 = CARTESIAN_POINT ( 'NONE',  ( 5.000000000000000000, 33.71516098798849015, -74.74816331893393340 ) ) ;
#19620 = DIRECTION ( 'NONE',  ( -1.000000000000000000, 0.000000000000000000, -0.000000000000000000 ) ) ;
#19621 = LINE ( 'NONE', #30896, #73954 ) ;
#19622 = LINE ( 'NONE', #42568, #62069 ) ;
#19623 = CARTESIAN_POINT ( 'NONE',  ( -97.30629616937495996, -209.9999999999999716, 82.65781250086713783 ) ) ;
#19624 = CARTESIAN_POINT ( 'NONE',  ( 97.64999999999999147, 90.00000000000002842, 87.14249999999999829 ) ) ;
#19625 = DIRECTION ( 'NONE',  ( 0.000000000000000000, -0.8090169943749508930, 0.5877852522924683631 ) ) ;
#19626 = DIRECTION ( 'NONE',  ( 0.000000000000000000, 0.9945218953682730678, -0.1045284632676570791 ) ) ;
#19627 = ORIENTED_EDGE ( 'NONE', *, *, #50517, .F. ) ;
#19628 = EDGE_CURVE ( 'NONE', #6829, #53064, #7479, .T. ) ;
#19629 = EDGE_CURVE ( 'NONE', #72554, #35320, #72568, .T. ) ;
#19630 = ORIENTED_EDGE ( 'NONE', *, *, #64868, .T. ) ;
#19631 = CARTESIAN_POINT ( 'NONE',  ( 10.00000000000000000, 5.202137450156907761, -37.22597642581151689 ) ) ;
#19632 = LINE ( 'NONE', #58764, #73486 ) ;
#19633 = CARTESIAN_POINT ( 'NONE',  ( 0.000000000000000000, 0.000000000000000000, 0.000000000000000000 ) ) ;
#19634 = CARTESIAN_POINT ( 'NONE',  ( -95.00000000000002842, 92.66308142843932671, 84.40406250086712703 ) ) ;
#19635 = CARTESIAN_POINT ( 'NONE',  ( 0.000000000000000000, 5.202137450156389953, 37.22597642581160216 ) ) ;
#19636 = CARTESIAN_POINT ( 'NONE',  ( -2.499999999999970690, 73.00000000000001421, -255.0000000000000000 ) ) ;
#19637 = CARTESIAN_POINT ( 'NONE',  ( 6.000000000000000000, 81.90746397400393164, -3.894527615416979671 ) ) ;
#19638 = EDGE_LOOP ( 'NONE', ( #23840, #17287, #5548, #29777 ) ) ;
#19639 = CARTESIAN_POINT ( 'NONE',  ( -95.00000000000002842, 87.33691857156074434, 75.19656250086714522 ) ) ;
#19640 = CIRCLE ( 'NONE', #71248, 12.50000000000000000 ) ;
#19641 = DIRECTION ( 'NONE',  ( 1.000000000000000000, -7.677074106448950501E-15, -2.598394312951952234E-14 ) ) ;
#19642 = AXIS2_PLACEMENT_3D ( 'NONE', #21239, #39303, #34019 ) ;
#19643 = DIRECTION ( 'NONE',  ( -1.000000000000000000, 0.000000000000000000, -0.000000000000000000 ) ) ;
#19644 = PLANE ( 'NONE',  #30926 ) ;
#19645 = DIRECTION ( 'NONE',  ( 0.000000000000000000, 0.000000000000000000, 1.000000000000000000 ) ) ;
#19646 = CARTESIAN_POINT ( 'NONE',  ( 97.64999999999994884, -211.5299782133524786, 82.64458333333332973 ) ) ;
#19647 = CARTESIAN_POINT ( 'NONE',  ( -97.30629616937497417, -211.3315407142195852, 81.59947916753381492 ) ) ;
#19648 = FACE_OUTER_BOUND ( 'NONE', #61909, .T. ) ;
#19649 = CONICAL_SURFACE ( 'NONE', #28078, 5.000000000000000888, 1.047197551196596299 ) ;
#19650 = CIRCLE ( 'NONE', #58098, 16.00000000000000000 ) ;
#19651 = CARTESIAN_POINT ( 'NONE',  ( -92.35000000000003695, 90.00000000000004263, 90.00000000000000000 ) ) ;
#19652 = DIRECTION ( 'NONE',  ( 0.000000000000000000, -0.9510565162951500895, -0.3090169943749583314 ) ) ;
#19653 = CARTESIAN_POINT ( 'NONE',  ( 0.000000000000000000, 0.000000000000000000, 0.000000000000000000 ) ) ;
#19654 = ORIENTED_EDGE ( 'NONE', *, *, #14105, .T. ) ;
#19655 = DIRECTION ( 'NONE',  ( -1.000000000000000000, -4.476705744456277943E-17, 0.000000000000000000 ) ) ;
#19656 = DIRECTION ( 'NONE',  ( 0.000000000000000000, 0.000000000000000000, 1.000000000000000000 ) ) ;
#19657 = DIRECTION ( 'NONE',  ( 1.000000000000000000, 0.000000000000000000, 0.000000000000000000 ) ) ;
#19658 = CIRCLE ( 'NONE', #37650, 42.00000000000000000 ) ;
#19659 = AXIS2_PLACEMENT_3D ( 'NONE', #49600, #21782, #44732 ) ;
#19660 = EDGE_CURVE ( 'NONE', #70270, #56502, #47374, .T. ) ;
#19661 = CARTESIAN_POINT ( 'NONE',  ( 10.00000000000000000, -12.93880638057259169, -76.41127070299286572 ) ) ;
#19662 = CARTESIAN_POINT ( 'NONE',  ( 92.69370383062501162, -208.6684592857803011, 89.11364583420049712 ) ) ;
#19663 = ORIENTED_EDGE ( 'NONE', *, *, #6722, .F. ) ;
#19664 = EDGE_CURVE ( 'NONE', #56468, #25977, #1791, .T. ) ;
#19665 = DIRECTION ( 'NONE',  ( -1.000000000000000000, -0.000000000000000000, -0.000000000000000000 ) ) ;
#19666 = CYLINDRICAL_SURFACE ( 'NONE', #34274, 37.49900000000000233 ) ;
#19667 = VERTEX_POINT ( 'NONE', #48433 ) ;
#19668 = EDGE_CURVE ( 'NONE', #8349, #56500, #22158, .T. ) ;
#19669 = DIRECTION ( 'NONE',  ( -1.000000000000000000, -0.000000000000000000, -0.000000000000000000 ) ) ;
#19670 = VERTEX_POINT ( 'NONE', #54090 ) ;
#19671 = EDGE_CURVE ( 'NONE', #14488, #15472, #35356, .T. ) ;
#19672 = CARTESIAN_POINT ( 'NONE',  ( 10.00000000000000000, 0.000000000000000000, 37.49900000000000233 ) ) ;
#19673 = VERTEX_POINT ( 'NONE', #26234 ) ;
#19674 = EDGE_CURVE ( 'NONE', #8287, #54048, #13757, .T. ) ;
#19675 = VERTEX_POINT ( 'NONE', #60833 ) ;
#19676 = ORIENTED_EDGE ( 'NONE', *, *, #21569, .F. ) ;
#19677 = DIRECTION ( 'NONE',  ( -1.000000000000000000, 0.000000000000000000, 0.000000000000000000 ) ) ;
#19678 = VERTEX_POINT ( 'NONE', #9315 ) ;
#19679 = AXIS2_PLACEMENT_3D ( 'NONE', #726, #41279, #63852 ) ;
#19680 = ORIENTED_EDGE ( 'NONE', *, *, #68235, .F. ) ;
#19681 = CARTESIAN_POINT ( 'NONE',  ( 97.30629616937498838, 90.00000000000002842, 79.95906250086714806 ) ) ;
#19682 = DIRECTION ( 'NONE',  ( 0.000000000000000000, 0.8910065241883690090, -0.4539904997395446395 ) ) ;
#19683 = EDGE_CURVE ( 'NONE', #2618, #32855, #23387, .T. ) ;
#19684 = FACE_OUTER_BOUND ( 'NONE', #39852, .T. ) ;
#19685 = VERTEX_POINT ( 'NONE', #42801 ) ;
#19686 = AXIS2_PLACEMENT_3D ( 'NONE', #71144, #24927, #70397 ) ;
#19687 = EDGE_LOOP ( 'NONE', ( #10613, #18059, #48429, #73756 ) ) ;
#19688 = ORIENTED_EDGE ( 'NONE', *, *, #22702, .T. ) ;
#19689 = CARTESIAN_POINT ( 'NONE',  ( -92.34999999999999432, -209.9999999999999716, 90.00000000000000000 ) ) ;
#19690 = ORIENTED_EDGE ( 'NONE', *, *, #33634, .F. ) ;
#19691 = DIRECTION ( 'NONE',  ( 0.000000000000000000, 0.000000000000000000, -1.000000000000000000 ) ) ;
#19692 = CARTESIAN_POINT ( 'NONE',  ( 0.000000000000000000, -132.5000000000000000, 40.00000000000000711 ) ) ;
#19693 = PLANE ( 'NONE',  #7532 ) ;
#19694 = CARTESIAN_POINT ( 'NONE',  ( 0.000000000000000000, 0.000000000000000000, 0.000000000000000000 ) ) ;
#19695 = CARTESIAN_POINT ( 'NONE',  ( 0.000000000000000000, -39.04073710021332744, -15.48615015657624028 ) ) ;
#19696 = DIRECTION ( 'NONE',  ( 0.8774505977381983346, 0.4796670183876293736, 0.000000000000000000 ) ) ;
#19697 = CARTESIAN_POINT ( 'NONE',  ( -94.99999999999997158, -209.9999999999999716, 90.00000000000000000 ) ) ;
#19698 = CARTESIAN_POINT ( 'NONE',  ( -93.09170853947338742, -211.8387288276635729, 74.44346887015069569 ) ) ;
#19699 = EDGE_CURVE ( 'NONE', #43669, #1173, #72099, .T. ) ;
#19700 = FACE_OUTER_BOUND ( 'NONE', #30121, .T. ) ;
#19701 = EDGE_CURVE ( 'NONE', #72850, #39929, #32914, .T. ) ;
#19703 = CARTESIAN_POINT ( 'NONE',  ( -97.65000000000001990, 90.00000000000004263, 74.83937500173429669 ) ) ;
#19702 = CARTESIAN_POINT ( 'NONE',  ( 97.64999999999999147, 90.00000000000002842, 77.06187500173429328 ) ) ;
#19704 = AXIS2_PLACEMENT_3D ( 'NONE', #38279, #67223, #20981 ) ;
#19705 = ORIENTED_EDGE ( 'NONE', *, *, #51579, .F. ) ;
#19706 = CARTESIAN_POINT ( 'NONE',  ( 94.99999999999998579, 92.66308142843935514, 75.67281250086716682 ) ) ;
#19707 = AXIS2_PLACEMENT_3D ( 'NONE', #61380, #10596, #4245 ) ;
#19708 = CARTESIAN_POINT ( 'NONE',  ( 11.99999999999999822, 0.000000000000000000, 0.000000000000000000 ) ) ;
#19709 = DIRECTION ( 'NONE',  ( -0.000000000000000000, -0.000000000000000000, 1.000000000000000000 ) ) ;
#19710 = CARTESIAN_POINT ( 'NONE',  ( 93.67500000000001137, -207.7050326799711968, 77.27354166840096639 ) ) ;
#19711 = LINE ( 'NONE', #47924, #13434 ) ;
#19712 = CARTESIAN_POINT ( 'NONE',  ( 10.00000000000000000, 0.000000000000000000, 0.000000000000000000 ) ) ;
#19713 = EDGE_LOOP ( 'NONE', ( #45893, #58178, #43286, #25168 ) ) ;
#19715 = CYLINDRICAL_SURFACE ( 'NONE', #30185, 16.00000000000000000 ) ;
#19714 = VECTOR ( 'NONE', #14843, 1000.000000000000000 ) ;
#19716 = VECTOR ( 'NONE', #50919, 1000.000000000000000 ) ;
#19717 = CARTESIAN_POINT ( 'NONE',  ( 7.103376864691351012E-17, -120.0000000000000000, -85.59999999999999432 ) ) ;
#19718 = ORIENTED_EDGE ( 'NONE', *, *, #54636, .T. ) ;
#19719 = ORIENTED_EDGE ( 'NONE', *, *, #67114, .F. ) ;
#19720 = DIRECTION ( 'NONE',  ( 0.3090169943749573878, -0.9510565162951503115, 0.000000000000000000 ) ) ;
#19721 = CARTESIAN_POINT ( 'NONE',  ( 11.99999999999999822, -59.03342792756297541, 46.54456581323783126 ) ) ;
#19722 = DIRECTION ( 'NONE',  ( -1.000000000000000000, 0.000000000000000000, 0.000000000000000000 ) ) ;
#19723 = AXIS2_PLACEMENT_3D ( 'NONE', #19122, #52225, #47694 ) ;
#19724 = LINE ( 'NONE', #8463, #3971 ) ;
#19725 = CARTESIAN_POINT ( 'NONE',  ( 0.000000000000000000, 0.000000000000000000, 0.000000000000000000 ) ) ;
#19726 = ORIENTED_EDGE ( 'NONE', *, *, #36903, .T. ) ;
#19727 = VECTOR ( 'NONE', #14049, 1000.000000000000000 ) ;
#19728 = CARTESIAN_POINT ( 'NONE',  ( -92.35000000000003695, 90.00000000000004263, 90.00000000000000000 ) ) ;
#19729 = DIRECTION ( 'NONE',  ( -1.000000000000000000, 0.000000000000000000, 0.000000000000000000 ) ) ;
#19730 = DIRECTION ( 'NONE',  ( 0.9730327541852497042, -0.2306669878475623159, 0.000000000000000000 ) ) ;
#19731 = CARTESIAN_POINT ( 'NONE',  ( -3.961125083139900749, -143.2122702051246677, 5.500000000000000000 ) ) ;
#19732 = DIRECTION ( 'NONE',  ( -1.000000000000000000, 0.000000000000000000, 0.000000000000000000 ) ) ;
#19733 = DIRECTION ( 'NONE',  ( 0.000000000000000000, -0.000000000000000000, -1.000000000000000000 ) ) ;
#19734 = UNCERTAINTY_MEASURE_WITH_UNIT (LENGTH_MEASURE( 1.000000000000000082E-05 ), #49739, 'distance_accuracy_value', 'NONE');
#19735 = DIRECTION ( 'NONE',  ( 1.000000000000000000, 0.000000000000000000, 0.000000000000000000 ) ) ;
#19736 = CARTESIAN_POINT ( 'NONE',  ( 15.00000000000000000, -20.55727247249748402, -16.78983467731284307 ) ) ;
#19737 = CARTESIAN_POINT ( 'NONE',  ( -3.000000000000000000, -10.45096189432344147, 21.10159698893426494 ) ) ;
#19738 = ADVANCED_FACE ( 'NONE', ( #65732 ), #13836, .T. ) ;
#19739 = CIRCLE ( 'NONE', #71345, 82.00000000000000000 ) ;
#19740 = CARTESIAN_POINT ( 'NONE',  ( 94.99999999999998579, 87.33691857156068750, 82.97531250086714749 ) ) ;
#19741 = CARTESIAN_POINT ( 'NONE',  ( -92.69370383062498320, -209.9999999999999716, 87.57906250086715261 ) ) ;
#19742 = CARTESIAN_POINT ( 'NONE',  ( 0.000000000000000000, 0.000000000000000000, 37.49900000000000233 ) ) ;
#19743 = ORIENTED_EDGE ( 'NONE', *, *, #72795, .T. ) ;
#19744 = DIRECTION ( 'NONE',  ( -0.000000000000000000, -0.000000000000000000, 1.000000000000000000 ) ) ;
#19745 = CARTESIAN_POINT ( 'NONE',  ( -94.99999999999997158, -206.9400435732949575, 80.31624999999998238 ) ) ;
#19746 = DIRECTION ( 'NONE',  ( 0.000000000000000000, -0.7071067811865536790, 0.7071067811865412445 ) ) ;
#19747 = VECTOR ( 'NONE', #40976, 1000.000000000000000 ) ;
#19748 = EDGE_CURVE ( 'NONE', #5237, #27457, #53381, .T. ) ;
#19749 = CARTESIAN_POINT ( 'NONE',  ( 93.84685191531251292, -211.9973110713294489, 84.03364583420047040 ) ) ;
#19750 = EDGE_LOOP ( 'NONE', ( #71760, #42692, #11730, #59676 ) ) ;
#19751 = EDGE_CURVE ( 'NONE', #15472, #37783, #72824, .T. ) ;
#19752 = DIRECTION ( 'NONE',  ( 1.000000000000000000, 0.000000000000000000, -0.000000000000000000 ) ) ;
#19753 = ORIENTED_EDGE ( 'NONE', *, *, #49069, .T. ) ;
#19754 = CIRCLE ( 'NONE', #55781, 16.00000000000000355 ) ;
#19755 = AXIS2_PLACEMENT_3D ( 'NONE', #19603, #66231, #42189 ) ;
#19756 = ORIENTED_EDGE ( 'NONE', *, *, #66552, .T. ) ;
#19757 = ADVANCED_FACE ( 'NONE', ( #32234, #43561 ), #55187, .T. ) ;
#19758 = EDGE_CURVE ( 'NONE', #17434, #73771, #49538, .T. ) ;
#19759 = CARTESIAN_POINT ( 'NONE',  ( 11.99999999999999822, 21.60688246758586573, 79.10210256391376049 ) ) ;
#19760 = CIRCLE ( 'NONE', #46235, 31.99999999999998934 ) ;
#19761 = VERTEX_POINT ( 'NONE', #60110 ) ;
#19762 = CARTESIAN_POINT ( 'NONE',  ( -3.000000000000000000, 9.615535125378775305, 24.73947219025917121 ) ) ;
#19763 = CARTESIAN_POINT ( 'NONE',  ( 97.30629616937498838, -211.3315407142195852, 78.00114583420049996 ) ) ;
#19764 = CARTESIAN_POINT ( 'NONE',  ( 10.00000000000000000, 55.20638768913831029, -51.02545421589267960 ) ) ;
#19765 = DIRECTION ( 'NONE',  ( 0.000000000000000000, 0.000000000000000000, 1.000000000000000000 ) ) ;
#19766 = CYLINDRICAL_SURFACE ( 'NONE', #52059, 31.99999999999999289 ) ;
#19767 = CYLINDRICAL_SURFACE ( 'NONE', #38724, 42.00000000000000000 ) ;
#19768 = ADVANCED_FACE ( 'NONE', ( #8589 ), #25500, .F. ) ;
#19769 = CARTESIAN_POINT ( 'NONE',  ( -92.35000000010070664, 90.00002309722640348, 83.41187580057902551 ) ) ;
#19770 = CARTESIAN_POINT ( 'NONE',  ( 96.32499999999998863, -207.7050326799711968, 81.53333333333333144 ) ) ;
#19771 = CIRCLE ( 'NONE', #61826, 37.49900000000000944 ) ;
#19772 = VERTEX_POINT ( 'NONE', #38264 ) ;
#19773 = ORIENTED_EDGE ( 'NONE', *, *, #68582, .F. ) ;
#19774 = ORIENTED_EDGE ( 'NONE', *, *, #17563, .F. ) ;
#19775 = ORIENTED_EDGE ( 'NONE', *, *, #26337, .T. ) ;
#19776 = LINE ( 'NONE', #25796, #16593 ) ;
#19777 = FILL_AREA_STYLE ('',( #48360 ) ) ;
#19778 = CARTESIAN_POINT ( 'NONE',  ( -97.30629616937501680, 90.00000000000004263, 83.45156250086715488 ) ) ;
#19779 = LINE ( 'NONE', #32163, #48264 ) ;
#19780 = DIRECTION ( 'NONE',  ( 1.000000000000000000, 0.000000000000000000, 0.000000000000000000 ) ) ;
#19781 = CARTESIAN_POINT ( 'NONE',  ( 97.64999999999997726, 91.52997821335252127, 75.13041666666666174 ) ) ;
#19782 = VERTEX_POINT ( 'NONE', #61206 ) ;
#19783 = CARTESIAN_POINT ( 'NONE',  ( -92.34999999999999432, -211.5299782133524502, 84.62895833506763665 ) ) ;
#19785 = ORIENTED_EDGE ( 'NONE', *, *, #27570, .T. ) ;
#19784 = ADVANCED_FACE ( 'NONE', ( #2621 ), #9696, .T. ) ;
#19786 = EDGE_CURVE ( 'NONE', #56288, #2618, #48544, .T. ) ;
#19787 = CARTESIAN_POINT ( 'NONE',  ( 8.700667342345820288, -98.11853780484867116, 5.500000000000000000 ) ) ;
#19788 = ORIENTED_EDGE ( 'NONE', *, *, #62696, .F. ) ;
#19789 = CARTESIAN_POINT ( 'NONE',  ( -92.35000000000005116, 91.52997821335253548, 85.36979166840096411 ) ) ;
#19790 =( BOUNDED_CURVE ( )  B_SPLINE_CURVE ( 2, ( #59520, #19646, #60270, #41848, #37700, #60632, #13275 ),
 .UNSPECIFIED., .F., .F. ) 
 B_SPLINE_CURVE_WITH_KNOTS ( ( 3, 2, 2, 3 ),
 ( 0.4791666666666668517, 0.4861111111111112160, 0.4930555555555556357, 0.5000000000000000000 ),
 .UNSPECIFIED. ) 
 CURVE ( )  GEOMETRIC_REPRESENTATION_ITEM ( )  RATIONAL_B_SPLINE_CURVE ( ( 0.9999999999999967804, 0.8660254037844419273, 1.000000000000000000, 0.8660254037844387076, 1.000000000000000000, 0.8660254037844387076, 1.000000000000000000 ) ) 
 REPRESENTATION_ITEM ( '' )  );
#19792 = ADVANCED_FACE ( 'NONE', ( #72313 ), #56524, .T. ) ;
#19791 = ORIENTED_EDGE ( 'NONE', *, *, #23211, .T. ) ;
#19793 = CARTESIAN_POINT ( 'NONE',  ( 92.69370383062498320, 88.66845928578037217, 86.04447916753382231 ) ) ;
#19794 = CARTESIAN_POINT ( 'NONE',  ( -7.670864526094549163, -97.73662565058241114, 5.500000000000000000 ) ) ;
#19795 = CARTESIAN_POINT ( 'NONE',  ( -92.91683521822002945, 88.99941091287938377, 74.79348190356857629 ) ) ;
#19796 = CARTESIAN_POINT ( 'NONE',  ( 92.35000000019411459, -210.0000198427945861, 86.27002759516706476 ) ) ;
#19797 = CYLINDRICAL_SURFACE ( 'NONE', #72083, 2.649999999999985700 ) ;
#19798 = ORIENTED_EDGE ( 'NONE', *, *, #58943, .T. ) ;
#19799 = DIRECTION ( 'NONE',  ( 0.000000000000000000, -0.2334453638559126354, 0.9723699203976748917 ) ) ;
#19800 = CARTESIAN_POINT ( 'NONE',  ( 11.99999999999999822, 28.89263327155746097, 71.91182617369197771 ) ) ;
#19801 = AXIS2_PLACEMENT_3D ( 'NONE', #31060, #19780, #25799 ) ;
#19802 = ORIENTED_EDGE ( 'NONE', *, *, #43564, .T. ) ;
#19803 = EDGE_LOOP ( 'NONE', ( #20859, #65932, #52840, #35180 ) ) ;
#19804 = DIRECTION ( 'NONE',  ( 0.000000000000000000, 0.000000000000000000, 1.000000000000000000 ) ) ;
#19805 = CARTESIAN_POINT ( 'NONE',  ( 0.000000000000000000, 0.000000000000000000, 40.80000000000001847 ) ) ;
#19806 = CARTESIAN_POINT ( 'NONE',  ( 1.560000000000000053, 1.732050807568878747, 7.017607234860990640E-28 ) ) ;
#19807 = CARTESIAN_POINT ( 'NONE',  ( -96.15314808468747287, -208.0026889286704943, 85.25072916753381946 ) ) ;
#19808 = EDGE_LOOP ( 'NONE', ( #22587, #72818, #20330, #53340 ) ) ;
#19809 = AXIS2_PLACEMENT_3D ( 'NONE', #46581, #34935, #11611 ) ;
#19810 = CARTESIAN_POINT ( 'NONE',  ( 10.00000000000000000, 0.000000000000000000, 0.000000000000000000 ) ) ;
#19811 = AXIS2_PLACEMENT_3D ( 'NONE', #49649, #72577, #21076 ) ;
#19812 = VERTEX_POINT ( 'NONE', #5028 ) ;
#19813 = ORIENTED_EDGE ( 'NONE', *, *, #47957, .T. ) ;
#19814 = DIRECTION ( 'NONE',  ( 1.000000000000000000, 0.000000000000000000, 0.000000000000000000 ) ) ;
#19815 = AXIS2_PLACEMENT_3D ( 'NONE', #67570, #26960, #16065 ) ;
#19816 = CARTESIAN_POINT ( 'NONE',  ( 92.69370383062498320, 90.00000000000002842, 88.53156250086716739 ) ) ;
#19817 = DIRECTION ( 'NONE',  ( 0.000000000000000000, 0.000000000000000000, -1.000000000000000000 ) ) ;
#19818 = CARTESIAN_POINT ( 'NONE',  ( 92.69370383062498320, 91.33154071421968467, 81.96989583420047154 ) ) ;
#19819 = DIRECTION ( 'NONE',  ( 1.000000000000000000, -0.000000000000000000, 0.000000000000000000 ) ) ;
#19820 = CARTESIAN_POINT ( 'NONE',  ( 11.99999999999999822, -71.27951684758005513, -30.41916302227188851 ) ) ;
#19821 = VECTOR ( 'NONE', #54049, 1000.000000000000000 ) ;
#19822 = LINE ( 'NONE', #3311, #46872 ) ;
#19823 = DIRECTION ( 'NONE',  ( 1.000000000000000000, 0.000000000000000000, 0.000000000000000000 ) ) ;
#19824 = LINE ( 'NONE', #42403, #29899 ) ;
#19825 = EDGE_CURVE ( 'NONE', #35387, #20380, #42652, .T. ) ;
#19826 = DIRECTION ( 'NONE',  ( 1.000000000000000000, -0.000000000000000000, -0.000000000000000000 ) ) ;
#19827 = AXIS2_PLACEMENT_3D ( 'NONE', #3654, #43865, #15657 ) ;
#19828 = LINE ( 'NONE', #65714, #26536 ) ;
#19829 = VERTEX_POINT ( 'NONE', #55770 ) ;
#19830 = CARTESIAN_POINT ( 'NONE',  ( -96.15314808468752972, 91.99731107132950569, 86.36197916753381776 ) ) ;
#19831 = DIRECTION ( 'NONE',  ( 0.000000000000000000, -1.000000000000000000, -1.040834085586084257E-14 ) ) ;
#19832 = EDGE_CURVE ( 'NONE', #11576, #51303, #22199, .T. ) ;
#19833 = CIRCLE ( 'NONE', #49832, 77.49899999999999523 ) ;
#19834 = ADVANCED_FACE ( 'NONE', ( #67793 ), #27933, .T. ) ;
#19835 = DIRECTION ( 'NONE',  ( 0.000000000000000000, 0.000000000000000000, 1.000000000000000000 ) ) ;
#19836 = VECTOR ( 'NONE', #32221, 1000.000000000000000 ) ;
#19837 = ORIENTED_EDGE ( 'NONE', *, *, #51335, .T. ) ;
#19838 = CARTESIAN_POINT ( 'NONE',  ( -10.00000000000000000, 0.000000000000000000, 0.000000000000000000 ) ) ;
#19839 = DIRECTION ( 'NONE',  ( -0.000000000000000000, -0.000000000000000000, 1.000000000000000000 ) ) ;
#19840 = CARTESIAN_POINT ( 'NONE',  ( 10.00000000000000000, -33.80338159004296017, 16.23288003029484727 ) ) ;
#19841 = EDGE_CURVE ( 'NONE', #51781, #64620, #73817, .T. ) ;
#19842 = CIRCLE ( 'NONE', #4261, 77.49899999999998101 ) ;
#19843 = CARTESIAN_POINT ( 'NONE',  ( 92.69370383062501162, -209.9999999999999716, 83.45156250086715488 ) ) ;
#19844 = ORIENTED_EDGE ( 'NONE', *, *, #26552, .T. ) ;
#19845 = VERTEX_POINT ( 'NONE', #62156 ) ;
#19846 = CARTESIAN_POINT ( 'NONE',  ( 5.999999999999999112, -51.29473840253269401, 63.97538442413407012 ) ) ;
#19847 = ORIENTED_EDGE ( 'NONE', *, *, #63123, .F. ) ;
#19848 = ADVANCED_FACE ( 'NONE', ( #67041 ), #16283, .F. ) ;
#19849 = DIRECTION ( 'NONE',  ( 0.000000000000000000, 0.2334453638559058908, -0.9723699203976764460 ) ) ;
#19850 = CARTESIAN_POINT ( 'NONE',  ( 0.000000000000000000, 28.89263327155850192, -71.91182617369156560 ) ) ;
#19851 = AXIS2_PLACEMENT_3D ( 'NONE', #56114, #67014, #44093 ) ;
#19853 = ORIENTED_EDGE ( 'NONE', *, *, #14537, .F. ) ;
#19852 = ADVANCED_FACE ( 'NONE', ( #21928 ), #44870, .T. ) ;
#19854 = AXIS2_PLACEMENT_3D ( 'NONE', #27668, #16013, #22403 ) ;
#19855 = CARTESIAN_POINT ( 'NONE',  ( 11.99999999999999822, 0.000000000000000000, 0.000000000000000000 ) ) ;
#19856 = CARTESIAN_POINT ( 'NONE',  ( 92.69370383062501162, -211.3315407142195852, 76.51947916753381662 ) ) ;
#19857 = VERTEX_POINT ( 'NONE', #55022 ) ;
#19858 = FACE_OUTER_BOUND ( 'NONE', #53173, .T. ) ;
#19859 = VERTEX_POINT ( 'NONE', #43763 ) ;
#19860 = EDGE_CURVE ( 'NONE', #72633, #3278, #55600, .T. ) ;
#19861 = AXIS2_PLACEMENT_3D ( 'NONE', #1715, #45711, #17117 ) ;
#19862 = ORIENTED_EDGE ( 'NONE', *, *, #50475, .F. ) ;
#19863 = CARTESIAN_POINT ( 'NONE',  ( 10.00000000000000000, 8.966570791701860443, -81.50828551894217355 ) ) ;
#19864 =( LENGTH_UNIT ( ) NAMED_UNIT ( * ) SI_UNIT ( .MILLI., .METRE. ) );
#19865 = CARTESIAN_POINT ( 'NONE',  ( 10.00000000000000000, -31.52238457039580055, -27.75498641678775869 ) ) ;
#19866 = ORIENTED_EDGE ( 'NONE', *, *, #13725, .T. ) ;
#19867 = CARTESIAN_POINT ( 'NONE',  ( -17.26469406256017791, -140.1601175325492648, 5.500000000000000000 ) ) ;
#19868 = CARTESIAN_POINT ( 'NONE',  ( 96.32499999999998863, -207.7050326799711968, 84.78770833506763438 ) ) ;
#19869 = CARTESIAN_POINT ( 'NONE',  ( 97.64999999999997726, 88.47002178664753558, 86.45458333333333201 ) ) ;
#19870 = ORIENTED_EDGE ( 'NONE', *, *, #67297, .T. ) ;
#19871 = CARTESIAN_POINT ( 'NONE',  ( 10.00000000000000178, 0.000000000000000000, 21.00000000000000000 ) ) ;
#19872 = EDGE_CURVE ( 'NONE', #72308, #67235, #42597, .T. ) ;
#19873 = FACE_OUTER_BOUND ( 'NONE', #35042, .T. ) ;
#19874 = VERTEX_POINT ( 'NONE', #9900 ) ;
#19875 = ORIENTED_EDGE ( 'NONE', *, *, #41968, .T. ) ;
#19876 = CARTESIAN_POINT ( 'NONE',  ( -92.69370383062505425, 91.33154071421968467, 86.36197916753383197 ) ) ;
#19877 = CARTESIAN_POINT ( 'NONE',  ( 92.69370383062498320, 90.00000000000002842, 82.65781250086713783 ) ) ;
#19878 = ORIENTED_EDGE ( 'NONE', *, *, #35542, .F. ) ;
#19879 = AXIS2_PLACEMENT_3D ( 'NONE', #26834, #72330, #65596 ) ;
#19880 = CARTESIAN_POINT ( 'NONE',  ( 94.99999999999998579, 93.05995642670504253, 84.20562500173429044 ) ) ;
#19881 = DIRECTION ( 'NONE',  ( 0.000000000000000000, 0.3826834323650841752, 0.9238795325112891810 ) ) ;
#19882 = EDGE_LOOP ( 'NONE', ( #25597, #17919 ) ) ;
#19883 = CARTESIAN_POINT ( 'NONE',  ( 97.64997150697853101, -208.4700053361938217, 87.27479280632981329 ) ) ;
#19884 = EDGE_LOOP ( 'NONE', ( #51714, #23664, #38298, #16293 ) ) ;
#19885 = EDGE_LOOP ( 'NONE', ( #66743, #35843, #68236, #61852 ) ) ;
#19886 = AXIS2_PLACEMENT_3D ( 'NONE', #10607, #4995, #51573 ) ;
#19887 = ORIENTED_EDGE ( 'NONE', *, *, #54736, .F. ) ;
#19888 = CARTESIAN_POINT ( 'NONE',  ( -3.000000000000000000, 14.60985201121729737, -18.46759930825687945 ) ) ;
#19889 = DIRECTION ( 'NONE',  ( 0.000000000000000000, 0.000000000000000000, -1.000000000000000000 ) ) ;
#19890 = CARTESIAN_POINT ( 'NONE',  ( -93.67500000000003979, 87.70503267997129626, 83.22666666666665947 ) ) ;
#19891 = ORIENTED_EDGE ( 'NONE', *, *, #52870, .T. ) ;
#19892 = CARTESIAN_POINT ( 'NONE',  ( 0.000000000000000000, 0.000000000000000000, 0.000000000000000000 ) ) ;
#19893 = DIRECTION ( 'NONE',  ( -1.000000000000000000, -0.000000000000000000, 0.000000000000000000 ) ) ;
#19894 = ORIENTED_EDGE ( 'NONE', *, *, #17311, .F. ) ;
#19895 = CARTESIAN_POINT ( 'NONE',  ( -10.00000000000000000, 0.000000000000000000, 0.000000000000000000 ) ) ;
#19896 = CARTESIAN_POINT ( 'NONE',  ( -94.99999999999997158, -207.3369185715606307, 78.05406250086714692 ) ) ;
#19897 = ORIENTED_EDGE ( 'NONE', *, *, #13058, .F. ) ;
#19898 = CARTESIAN_POINT ( 'NONE',  ( 10.00000000000000000, 25.88420570971438650, -27.13269053701069566 ) ) ;
#19899 = CARTESIAN_POINT ( 'NONE',  ( -3.000000000000000000, -0.9646360437372163421, -23.52805723605591126 ) ) ;
#19900 = DIRECTION ( 'NONE',  ( 0.000000000000000000, 0.000000000000000000, 1.000000000000000000 ) ) ;
#19901 = CARTESIAN_POINT ( 'NONE',  ( 0.000000000000000000, -74.74816331893454446, 33.71516098798714722 ) ) ;
#19902 = DIRECTION ( 'NONE',  ( 0.000000000000000000, -0.9781476007338041345, -0.2079116908177664480 ) ) ;
#19903 = DIRECTION ( 'NONE',  ( 0.000000000000000000, 0.000000000000000000, 1.000000000000000000 ) ) ;
#19904 = CYLINDRICAL_SURFACE ( 'NONE', #54070, 77.49899999999999523 ) ;
#19905 = LINE ( 'NONE', #55613, #69989 ) ;
#19906 = DIRECTION ( 'NONE',  ( 0.000000000000000000, -1.000000000000000000, 0.000000000000000000 ) ) ;
#19907 = CARTESIAN_POINT ( 'NONE',  ( 0.000000000000000000, -20.55727247249748046, 16.78983467731285018 ) ) ;
#19908 = CARTESIAN_POINT ( 'NONE',  ( -97.30629616937501680, 90.00000000000004263, 89.16656250086715829 ) ) ;
#19909 = CARTESIAN_POINT ( 'NONE',  ( 0.000000000000000000, 39.78640506895604290, 66.50666863322015843 ) ) ;
#19910 = DIRECTION ( 'NONE',  ( -1.000000000000000000, 0.000000000000000000, 0.000000000000000000 ) ) ;
#19911 = DIRECTION ( 'NONE',  ( 0.000000000000000000, -0.6691306063588662312, 0.7431448254773870277 ) ) ;
#19912 = DIRECTION ( 'NONE',  ( 1.000000000000000000, 0.000000000000000000, 0.000000000000000000 ) ) ;
#19913 = EDGE_CURVE ( 'NONE', #59706, #48451, #50104, .T. ) ;
#19915 = CARTESIAN_POINT ( 'NONE',  ( 10.00000000000000000, 14.66109333815460225, 73.73191006444577056 ) ) ;
#19914 = AXIS2_PLACEMENT_3D ( 'NONE', #50103, #21542, #38847 ) ;
#19916 = CARTESIAN_POINT ( 'NONE',  ( 0.000000000000000000, 78.73519480814955784, 22.90783923731657268 ) ) ;
#19917 = CARTESIAN_POINT ( 'NONE',  ( -8.637688417678548447, 13.69818742750669749, -55.00000000000000000 ) ) ;
#19918 = ADVANCED_FACE ( 'NONE', ( #55396 ), #3917, .F. ) ;
#19919 = CARTESIAN_POINT ( 'NONE',  ( 95.00000000000000000, -213.0599564267049857, 78.72875000000001933 ) ) ;
#19920 = AXIS2_PLACEMENT_3D ( 'NONE', #32417, #55362, #15881 ) ;
#19921 = CARTESIAN_POINT ( 'NONE',  ( 0.000000000000000000, 21.32104025579158701, -30.84782396557194772 ) ) ;
#19922 = CARTESIAN_POINT ( 'NONE',  ( -94.99999999999997158, -206.9400435732949575, 86.66624999999999091 ) ) ;
#19923 = AXIS2_PLACEMENT_3D ( 'NONE', #26668, #55621, #71046 ) ;
#19924 = EDGE_CURVE ( 'NONE', #16380, #58612, #16181, .T. ) ;
#19925 = DIRECTION ( 'NONE',  ( -0.8225049752423776450, -0.5687579148473765889, 0.000000000000000000 ) ) ;
#19926 = PRODUCT_DEFINITION_SHAPE ( 'NONE', 'NONE',  #74350 ) ;
#19927 = AXIS2_PLACEMENT_3D ( 'NONE', #62571, #15937, #45651 ) ;
#19928 = CIRCLE ( 'NONE', #39166, 16.00000000000000000 ) ;
#19929 = ADVANCED_FACE ( 'NONE', ( #890 ), #35061, .T. ) ;
#19930 = VERTEX_POINT ( 'NONE', #62923 ) ;
#19931 = DIRECTION ( 'NONE',  ( -1.000000000000000000, 0.000000000000000000, -0.000000000000000000 ) ) ;
#19932 = LINE ( 'NONE', #59806, #69469 ) ;
#19933 = CARTESIAN_POINT ( 'NONE',  ( 92.35001469785311201, -208.4700133008379908, 81.77145774807790701 ) ) ;
#19934 = LINE ( 'NONE', #47412, #52227 ) ;
#19935 = AXIS2_PLACEMENT_3D ( 'NONE', #7195, #63619, #29732 ) ;
#19936 = VERTEX_POINT ( 'NONE', #17397 ) ;
#19937 = CARTESIAN_POINT ( 'NONE',  ( 11.99999999999999822, 14.67089635893819377, -73.72996012237423713 ) ) ;
#19938 = FACE_OUTER_BOUND ( 'NONE', #12680, .T. ) ;
#19939 = EDGE_LOOP ( 'NONE', ( #37186, #60655, #56872 ) ) ;
#19940 = CARTESIAN_POINT ( 'NONE',  ( 93.84685191531249870, -208.0026889286704943, 80.64697916753381435 ) ) ;
#19941 = CARTESIAN_POINT ( 'NONE',  ( 95.00000000000000000, -207.3369185715606307, 88.37281250086715545 ) ) ;
#19942 = ORIENTED_EDGE ( 'NONE', *, *, #6400, .F. ) ;
#19943 = CARTESIAN_POINT ( 'NONE',  ( 97.30629616937498838, -208.6684592857803011, 86.99697916753382287 ) ) ;
#19944 = VERTEX_POINT ( 'NONE', #52340 ) ;
#19945 = DIRECTION ( 'NONE',  ( 0.000000000000000000, -0.9238795325112821866, -0.3826834323651006065 ) ) ;
#19946 = ORIENTED_EDGE ( 'NONE', *, *, #60446, .T. ) ;
#19947 = EDGE_CURVE ( 'NONE', #1126, #18290, #23053, .T. ) ;
#19948 = EDGE_CURVE ( 'NONE', #32439, #40132, #19570, .T. ) ;
#19949 = CARTESIAN_POINT ( 'NONE',  ( -93.84685191531252713, 88.00268892867056536, 76.04322916753382344 ) ) ;
#19950 = CLOSED_SHELL ( 'NONE', ( #42893, #36755, #68081, #63577, #73857, #60437, #50519, #56280, #54351, #70120, #22173, #5020, #18725, #28532, #65307, #22440, #35457, #25376, #30889, #72228, #68185, #32933, #43433, #61318, #31044, #39748, #18511 ) ) ;
#19951 = VERTEX_POINT ( 'NONE', #33947 ) ;
#19952 = ORIENTED_EDGE ( 'NONE', *, *, #58375, .F. ) ;
#19953 = CARTESIAN_POINT ( 'NONE',  ( 0.000000000000000000, 70.52718814184294160, -26.02418014898236720 ) ) ;
#19954 = ORIENTED_EDGE ( 'NONE', *, *, #57680, .F. ) ;
#19955 = LINE ( 'NONE', #49633, #7681 ) ;
#19956 = SURFACE_STYLE_USAGE ( .BOTH. , #3081 ) ;
#19957 = ORIENTED_EDGE ( 'NONE', *, *, #63694, .T. ) ;
#19958 = CARTESIAN_POINT ( 'NONE',  ( 2.750000000000000000, 5.817072295949927426E-16, -4.750000000000000000 ) ) ;
#19959 = ADVANCED_FACE ( 'NONE', ( #51609 ), #18138, .T. ) ;
#19960 = ORIENTED_EDGE ( 'NONE', *, *, #26993, .T. ) ;
#19961 = CARTESIAN_POINT ( 'NONE',  ( 92.35000000000000853, -209.9999999999999716, 86.18999999999999773 ) ) ;
#19962 = AXIS2_PLACEMENT_3D ( 'NONE', #68470, #817, #24091 ) ;
#19963 = VERTEX_POINT ( 'NONE', #51233 ) ;
#19964 = EDGE_LOOP ( 'NONE', ( #17606, #5381, #25613, #23865 ) ) ;
#19965 = ORIENTED_EDGE ( 'NONE', *, *, #69130, .F. ) ;
#19966 = CARTESIAN_POINT ( 'NONE',  ( 92.69370383062501162, -208.6684592857803011, 78.79489583420047438 ) ) ;
#19967 = DIRECTION ( 'NONE',  ( -0.9227826878668545785, -0.3853207896976533209, 0.000000000000000000 ) ) ;
#19968 = ITEM_DEFINED_TRANSFORMATION ( 'NONE', 'NONE', #2841,  #43395 ) ;
#19969 = ORIENTED_EDGE ( 'NONE', *, *, #40057, .F. ) ;
#19970 = DIRECTION ( 'NONE',  ( 0.000000000000000000, 0.8910065241883657894, 0.4539904997395509678 ) ) ;
#19971 = VERTEX_POINT ( 'NONE', #162 ) ;
#19972 = AXIS2_PLACEMENT_3D ( 'NONE', #25267, #70357, #47816 ) ;
#19973 = DIRECTION ( 'NONE',  ( -1.000000000000000000, 0.000000000000000000, 0.000000000000000000 ) ) ;
#19974 = CARTESIAN_POINT ( 'NONE',  ( 1.560000000000000053, -1.732050807568877859, -1.752539433813135784E-17 ) ) ;
#19975 = ORIENTED_EDGE ( 'NONE', *, *, #73518, .F. ) ;
#19976 = CARTESIAN_POINT ( 'NONE',  ( -94.99999999999997158, -206.9400435732949575, 88.65062500173428361 ) ) ;
#19977 = CARTESIAN_POINT ( 'NONE',  ( 0.000000000000000000, 0.000000000000000000, 0.000000000000000000 ) ) ;
#19978 = CARTESIAN_POINT ( 'NONE',  ( -97.30629616937497417, -208.6684592857803011, 81.33489583420048064 ) ) ;
#19979 = CARTESIAN_POINT ( 'NONE',  ( -95.00000000000002842, 92.66308142843932671, 79.48281250086715488 ) ) ;
#19980 = ORIENTED_EDGE ( 'NONE', *, *, #15523, .F. ) ;
#19981 = AXIS2_PLACEMENT_3D ( 'NONE', #31934, #65431, #37595 ) ;
#19982 = CARTESIAN_POINT ( 'NONE',  ( 97.30629616937498838, 91.33154071421968467, 79.85322916753379729 ) ) ;
#19983 = ORIENTED_EDGE ( 'NONE', *, *, #58677, .T. ) ;
#19984 = FACE_OUTER_BOUND ( 'NONE', #27276, .T. ) ;
#19985 = FACE_OUTER_BOUND ( 'NONE', #28500, .T. ) ;
#19986 = DIRECTION ( 'NONE',  ( -1.000000000000000000, 0.000000000000000000, -0.000000000000000000 ) ) ;
#19987 = FACE_BOUND ( 'NONE', #24950, .T. ) ;
#19988 = CARTESIAN_POINT ( 'NONE',  ( -11.59517495878806947, -96.12423995607481686, -5.500000000000000000 ) ) ;
#19989 = CARTESIAN_POINT ( 'NONE',  ( -97.30629616937495996, -209.9999999999999716, 81.38781250086714181 ) ) ;
#19990 = CARTESIAN_POINT ( 'NONE',  ( -94.99999999999997158, -213.0599564267049857, 89.52374999999999261 ) ) ;
#19991 = DIRECTION ( 'NONE',  ( 1.000000000000000000, -0.000000000000000000, -0.000000000000000000 ) ) ;
#19992 = LINE ( 'NONE', #72237, #13231 ) ;
#19993 = ORIENTED_EDGE ( 'NONE', *, *, #54809, .T. ) ;
#19994 = AXIS2_PLACEMENT_3D ( 'NONE', #57140, #33069, #21803 ) ;
#19995 = EDGE_LOOP ( 'NONE', ( #34649, #30436, #14690, #10513 ) ) ;
#19996 = LINE ( 'NONE', #71127, #48061 ) ;
#19997 = CARTESIAN_POINT ( 'NONE',  ( -96.32500000000001705, 87.70503267997129626, 75.50083333333331836 ) ) ;
#19998 = CARTESIAN_POINT ( 'NONE',  ( -97.64997399466426486, 88.47000677245993927, 84.41729270697882725 ) ) ;
#19999 = CARTESIAN_POINT ( 'NONE',  ( -92.69370383062502583, 88.66845928578038638, 83.55739583420047722 ) ) ;
#20000 = CARTESIAN_POINT ( 'NONE',  ( 10.00000000000000000, 0.000000000000000000, 0.000000000000000000 ) ) ;
#20001 = CARTESIAN_POINT ( 'NONE',  ( 0.000000000000000000, 22.64427369931212297, -30.00120703465181293 ) ) ;
#20002 = LINE ( 'NONE', #59140, #30051 ) ;
#20003 = VERTEX_POINT ( 'NONE', #57258 ) ;
#20004 = FACE_OUTER_BOUND ( 'NONE', #34511, .T. ) ;
#20005 = EDGE_CURVE ( 'NONE', #53485, #68824, #26863, .T. ) ;
#20006 = FACE_OUTER_BOUND ( 'NONE', #54380, .T. ) ;
#20007 = AXIS2_PLACEMENT_3D ( 'NONE', #5586, #34881, #41260 ) ;
#20008 = CARTESIAN_POINT ( 'NONE',  ( -97.64999999960637922, 90.00002930319634231, 82.45844277051273252 ) ) ;
#20009 = EDGE_CURVE ( 'NONE', #65417, #51113, #29397, .T. ) ;
#20010 = CYLINDRICAL_SURFACE ( 'NONE', #57398, 2.649999999999999467 ) ;
#20011 = CARTESIAN_POINT ( 'NONE',  ( 11.99999999999999822, 67.80270845531889279, 46.11716303203210288 ) ) ;
#20012 = CARTESIAN_POINT ( 'NONE',  ( 92.34999999999999432, 90.00000000000002842, 86.18999999999999773 ) ) ;
#20013 = CARTESIAN_POINT ( 'NONE',  ( -93.84685191531247028, -211.9973110713294489, 83.66322916753382799 ) ) ;
#20014 = EDGE_CURVE ( 'NONE', #58552, #68894, #30456, .T. ) ;
#20015 = CARTESIAN_POINT ( 'NONE',  ( 11.99999999999999822, 34.44570377933693806, -69.42325613327405165 ) ) ;
#20016 =( BOUNDED_CURVE ( )  B_SPLINE_CURVE ( 2, ( #14274, #25558, #37227, #39452, #62012, #10121, #44724 ),
 .UNSPECIFIED., .F., .F. ) 
 B_SPLINE_CURVE_WITH_KNOTS ( ( 3, 2, 2, 3 ),
 ( 0.1905056698837213069, 0.1975614351447063655, 0.2046172006855887515, 0.2116728463006668226 ),
 .UNSPECIFIED. ) 
 CURVE ( )  GEOMETRIC_REPRESENTATION_ITEM ( )  RATIONAL_B_SPLINE_CURVE ( ( 1.000000000000000000, 0.8660254037844387076, 1.000000000000000000, 0.8660254037844387076, 1.000000000000000000, 0.8660276809308541379, 0.9999954457845777744 ) ) 
 REPRESENTATION_ITEM ( '' )  );
#20017 = EDGE_CURVE ( 'NONE', #45142, #39027, #70061, .T. ) ;
#20018 = CIRCLE ( 'NONE', #40476, 32.00000000000000000 ) ;
#20019 = CARTESIAN_POINT ( 'NONE',  ( 93.84685191531248449, 88.00268892867053694, 75.30239583420048177 ) ) ;
#20020 = DIRECTION ( 'NONE',  ( 0.000000000000000000, 0.000000000000000000, 1.000000000000000000 ) ) ;
#20021 = DIRECTION ( 'NONE',  ( -1.000000000000000000, 0.000000000000000000, 0.000000000000000000 ) ) ;
#20022 = CIRCLE ( 'NONE', #24815, 82.00000000000000000 ) ;
#20023 = ORIENTED_EDGE ( 'NONE', *, *, #59501, .T. ) ;
#20024 = FACE_OUTER_BOUND ( 'NONE', #25869, .T. ) ;
#20025 = CARTESIAN_POINT ( 'NONE',  ( -97.65000000000001990, 90.00000000000004263, 78.57000000000000739 ) ) ;
#20026 = CARTESIAN_POINT ( 'NONE',  ( 8.000000000000007105, 22.90000000000021885, 2.510511456526457458E-13 ) ) ;
#20027 = VECTOR ( 'NONE', #13615, 1000.000000000000000 ) ;
#20028 = LINE ( 'NONE', #19661, #20496 ) ;
#20030 = EDGE_CURVE ( 'NONE', #27941, #39489, #15824, .T. ) ;
#20029 = CARTESIAN_POINT ( 'NONE',  ( 96.15314808468750130, -211.9973110713294489, 88.74322916753382628 ) ) ;
#20031 = ORIENTED_EDGE ( 'NONE', *, *, #53988, .T. ) ;
#20032 = ADVANCED_FACE ( 'NONE', ( #17761 ), #63650, .F. ) ;
#20033 = CARTESIAN_POINT ( 'NONE',  ( 92.35000000000002274, -208.4700217866474645, 87.40708333333333258 ) ) ;
#20034 = AXIS2_PLACEMENT_3D ( 'NONE', #72882, #43974, #21386 ) ;
#20035 = DIRECTION ( 'NONE',  ( -1.000000000000000000, 0.000000000000000000, 0.000000000000000000 ) ) ;
#20036 = EDGE_LOOP ( 'NONE', ( #32274, #30662, #45050 ) ) ;
#20037 = DIRECTION ( 'NONE',  ( -1.000000000000000000, 0.000000000000000000, 0.000000000000000000 ) ) ;
#20038 = VECTOR ( 'NONE', #57863, 1000.000000000000000 ) ;
#20039 = ORIENTED_EDGE ( 'NONE', *, *, #10496, .T. ) ;
#20040 = CARTESIAN_POINT ( 'NONE',  ( -92.35000000000003695, 90.00000000000004263, 84.60249999999999204 ) ) ;
#20041 = EDGE_CURVE ( 'NONE', #60073, #23222, #62542, .T. ) ;
#20042 = EDGE_CURVE ( 'NONE', #62534, #64128, #23289, .T. ) ;
#20043 = AXIS2_PLACEMENT_3D ( 'NONE', #24674, #52135, #6648 ) ;
#20044 = ORIENTED_EDGE ( 'NONE', *, *, #14004, .T. ) ;
#20045 = ORIENTED_EDGE ( 'NONE', *, *, #10343, .T. ) ;
#20046 = EDGE_LOOP ( 'NONE', ( #39010, #28819, #47071, #51243 ) ) ;
#20047 = ORIENTED_EDGE ( 'NONE', *, *, #19860, .F. ) ;
#20048 = CARTESIAN_POINT ( 'NONE',  ( -23.50000000000000355, -120.0000000000000000, -64.00000000000000000 ) ) ;
#20049 = AXIS2_PLACEMENT_3D ( 'NONE', #53607, #26426, #2149 ) ;
#20050 = VERTEX_POINT ( 'NONE', #52720 ) ;
#20051 = ORIENTED_EDGE ( 'NONE', *, *, #51102, .T. ) ;
#20052 = CARTESIAN_POINT ( 'NONE',  ( 92.69370383062498320, 91.33154071421968467, 78.95364583420048632 ) ) ;
#20053 = LINE ( 'NONE', #3174, #69594 ) ;
#20054 = DIRECTION ( 'NONE',  ( 0.000000000000000000, 0.000000000000000000, 1.000000000000000000 ) ) ;
#20055 = ORIENTED_EDGE ( 'NONE', *, *, #54491, .T. ) ;
#20056 = VERTEX_POINT ( 'NONE', #56893 ) ;
#20057 = ORIENTED_EDGE ( 'NONE', *, *, #69758, .T. ) ;
#20058 = CARTESIAN_POINT ( 'NONE',  ( -23.50000000000000355, -120.0000000000000000, -80.00000000000000000 ) ) ;
#20059 = VERTEX_POINT ( 'NONE', #5402 ) ;
#20060 = CARTESIAN_POINT ( 'NONE',  ( 0.000000000000000000, 0.000000000000000000, 99.99999999999997158 ) ) ;
#20061 = CARTESIAN_POINT ( 'NONE',  ( 11.99999999999999822, -41.76937507738831812, 62.50329211542423025 ) ) ;
#20062 = FACE_OUTER_BOUND ( 'NONE', #47871, .T. ) ;
#20063 = DIRECTION ( 'NONE',  ( -1.000000000000000000, -0.000000000000000000, -0.000000000000000000 ) ) ;
#20064 = CARTESIAN_POINT ( 'NONE',  ( 23.11608002360578240, -124.4885236261218182, -2.500000000000000000 ) ) ;
#20065 = PLANE ( 'NONE',  #27557 ) ;
#20066 = PLANE ( 'NONE',  #25064 ) ;
#20067 = CARTESIAN_POINT ( 'NONE',  ( -92.34999999999999432, -208.4700217866474645, 74.57479166840096241 ) ) ;
#20068 = CARTESIAN_POINT ( 'NONE',  ( -92.69370383062502583, 88.66845928578038638, 87.52614583420049144 ) ) ;
#20069 = ORIENTED_EDGE ( 'NONE', *, *, #57236, .T. ) ;
#20070 =( REPRESENTATION_RELATIONSHIP ('NONE','NONE', #31117, #30982 ) REPRESENTATION_RELATIONSHIP_WITH_TRANSFORMATION ( #30510 )SHAPE_REPRESENTATION_RELATIONSHIP( ) );
#20072 = CARTESIAN_POINT ( 'NONE',  ( -92.69370383062504004, 90.00000000000004263, 88.69031250086715090 ) ) ;
#20071 = CARTESIAN_POINT ( 'NONE',  ( 94.99999999999998579, 86.94004357329500010, 74.99812500173430863 ) ) ;
#20073 = VERTEX_POINT ( 'NONE', #28294 ) ;
#20074 = CARTESIAN_POINT ( 'NONE',  ( 92.69370383062498320, 90.00000000000002842, 77.10156250086714635 ) ) ;
#20075 = AXIS2_PLACEMENT_3D ( 'NONE', #39491, #33837, #27821 ) ;
#20076 = FACE_OUTER_BOUND ( 'NONE', #5604, .T. ) ;
#20077 = LINE ( 'NONE', #26464, #52290 ) ;
#20078 = CARTESIAN_POINT ( 'NONE',  ( 0.000000000000000000, -77.19088730480518734, -6.903761155838607166 ) ) ;
#20079 = PLANE ( 'NONE',  #7435 ) ;
#20080 = AXIS2_PLACEMENT_3D ( 'NONE', #33097, #57171, #40612 ) ;
#20081 = CARTESIAN_POINT ( 'NONE',  ( -93.67500000000003979, 92.29496732002878900, 89.15333333333333599 ) ) ;
#20082 = VERTEX_POINT ( 'NONE', #22678 ) ;
#20083 = CARTESIAN_POINT ( 'NONE',  ( -92.35000000000000853, -211.5299782133524218, 87.72458333333332803 ) ) ;
#20084 = DIRECTION ( 'NONE',  ( 0.000000000000000000, 0.000000000000000000, 1.000000000000000000 ) ) ;
#20085 = ORIENTED_EDGE ( 'NONE', *, *, #23524, .T. ) ;
#20086 = AXIS2_PLACEMENT_3D ( 'NONE', #26737, #60961, #14723 ) ;
#20087 = VERTEX_POINT ( 'NONE', #45625 ) ;
#20088 = ADVANCED_FACE ( 'NONE', ( #68547 ), #59475, .T. ) ;
#20089 = FACE_OUTER_BOUND ( 'NONE', #15287, .T. ) ;
#20090 = CYLINDRICAL_SURFACE ( 'NONE', #17783, 82.00000000000000000 ) ;
#20091 = CARTESIAN_POINT ( 'NONE',  ( -95.00000000000002842, 93.05995642670504253, 86.11062500173430578 ) ) ;
#20092 = EDGE_CURVE ( 'NONE', #65477, #21000, #60449, .T. ) ;
#20093 = CARTESIAN_POINT ( 'NONE',  ( 0.000000000000000000, 17.80606268964540106, 33.00180498840052934 ) ) ;
#20094 = DIRECTION ( 'NONE',  ( 1.000000000000000000, -7.571541139944061634E-15, -2.603472992745718826E-14 ) ) ;
#20095 = CARTESIAN_POINT ( 'NONE',  ( -97.30629616937495996, -209.9999999999999716, 75.83156250086716454 ) ) ;
#20096 = ORIENTED_EDGE ( 'NONE', *, *, #49978, .T. ) ;
#20097 = EDGE_CURVE ( 'NONE', #55952, #17105, #65314, .T. ) ;
#20098 = FACE_OUTER_BOUND ( 'NONE', #41114, .T. ) ;
#20099 = CARTESIAN_POINT ( 'NONE',  ( -21.33958957442910886, -129.9559990355020034, -5.500000000000000000 ) ) ;
#20100 = VECTOR ( 'NONE', #42805, 1000.000000000000000 ) ;
#20101 = LINE ( 'NONE', #20491, #15402 ) ;
#20102 = EDGE_CURVE ( 'NONE', #33622, #42810, #54209, .T. ) ;
#20103 = FACE_OUTER_BOUND ( 'NONE', #22552, .T. ) ;
#20104 = LINE ( 'NONE', #54699, #32901 ) ;
#20105 = CARTESIAN_POINT ( 'NONE',  ( -0.0004442498525516064278, 0.001194404164626844313, -80.00000000000001421 ) ) ;
#20106 = CARTESIAN_POINT ( 'NONE',  ( 10.00000000000000000, -14.67089635893658794, -73.72996012237454977 ) ) ;
#20107 = PLANE ( 'NONE',  #10036 ) ;
#20108 = CIRCLE ( 'NONE', #58533, 12.49999999999999645 ) ;
#20109 = LINE ( 'NONE', #44814, #71857 ) ;
#20110 = EDGE_CURVE ( 'NONE', #12130, #54409, #17271, .T. ) ;
#20111 = CARTESIAN_POINT ( 'NONE',  ( 93.84685191531248449, 91.99731107132950569, 83.98072916753382344 ) ) ;
#20112 = CARTESIAN_POINT ( 'NONE',  ( -93.84685191531248449, -208.0026889286704943, 81.96989583420048575 ) ) ;
#20113 = FACE_OUTER_BOUND ( 'NONE', #66292, .T. ) ;
#20114 = VERTEX_POINT ( 'NONE', #19605 ) ;
#20115 = CARTESIAN_POINT ( 'NONE',  ( -92.34999999999999432, -209.9999999999999716, 81.42749999999999488 ) ) ;
#20116 = CARTESIAN_POINT ( 'NONE',  ( -96.32499999999996021, -207.7050326799711968, 79.09916666666666174 ) ) ;
#20117 = CARTESIAN_POINT ( 'NONE',  ( -10.00000000000000000, 0.000000000000000000, 0.000000000000000000 ) ) ;
#20119 = ADVANCED_FACE ( 'NONE', ( #42926 ), #53093, .T. ) ;
#20118 = CARTESIAN_POINT ( 'NONE',  ( 93.84685191531249870, -208.0026889286704943, 83.82197916753381151 ) ) ;
#20120 = VERTEX_POINT ( 'NONE', #1633 ) ;
#20121 = ADVANCED_FACE ( 'NONE', ( #15352 ), #36162, .F. ) ;
#20122 = CARTESIAN_POINT ( 'NONE',  ( 97.08316478178004161, 88.99941091287935535, 74.79348190356853365 ) ) ;
#20123 = ORIENTED_EDGE ( 'NONE', *, *, #19405, .T. ) ;
#20124 = AXIS2_PLACEMENT_3D ( 'NONE', #21335, #46151, #52507 ) ;
#20125 = ORIENTED_EDGE ( 'NONE', *, *, #39907, .T. ) ;
#20126 = AXIS2_PLACEMENT_3D ( 'NONE', #10777, #29161, #51738 ) ;
#20127 = CARTESIAN_POINT ( 'NONE',  ( 11.99999999999999822, 34.44570377933598593, 69.42325613327452061 ) ) ;
#20128 = AXIS2_PLACEMENT_3D ( 'NONE', #12782, #52645, #19167 ) ;
#20129 = CIRCLE ( 'NONE', #16547, 16.00000000000000000 ) ;
#20130 = ORIENTED_EDGE ( 'NONE', *, *, #45584, .F. ) ;
#20131 = FACE_OUTER_BOUND ( 'NONE', #49692, .T. ) ;
#20132 = CARTESIAN_POINT ( 'NONE',  ( 95.00000000000000000, -207.3369185715606307, 77.57781250086715374 ) ) ;
#20133 = CARTESIAN_POINT ( 'NONE',  ( 0.000000000000000000, -77.49459641780886443, 0.8261519478428549501 ) ) ;
#20134 = DIRECTION ( 'NONE',  ( 1.000000000000000000, 0.000000000000000000, 0.000000000000000000 ) ) ;
#20135 = CARTESIAN_POINT ( 'NONE',  ( 0.000000000000000000, 9.188173127307290855, 40.98264845739752360 ) ) ;
#20136 = CARTESIAN_POINT ( 'NONE',  ( 96.32499999999998863, 87.70503267997126784, 76.87666666666666515 ) ) ;
#20137 = DIRECTION ( 'NONE',  ( 1.000000000000000000, 0.000000000000000000, 0.000000000000000000 ) ) ;
#20138 = CARTESIAN_POINT ( 'NONE',  ( 96.32499999999998863, -207.7050326799711968, 80.89833333333332632 ) ) ;
#20139 = ORIENTED_EDGE ( 'NONE', *, *, #47435, .T. ) ;
#20140 = ORIENTED_EDGE ( 'NONE', *, *, #16571, .F. ) ;
#20141 = ORIENTED_EDGE ( 'NONE', *, *, #49978, .F. ) ;
#20142 = ORIENTED_EDGE ( 'NONE', *, *, #51109, .F. ) ;
#20143 = LINE ( 'NONE', #60398, #18998 ) ;
#20144 = CIRCLE ( 'NONE', #60995, 31.99999999999998934 ) ;
#20145 =( NAMED_UNIT ( * ) PLANE_ANGLE_UNIT ( ) SI_UNIT ( $, .RADIAN. ) );
#20146 = CARTESIAN_POINT ( 'NONE',  ( -93.84685191531252713, 88.00268892867056536, 85.56822916753381492 ) ) ;
#20147 = CARTESIAN_POINT ( 'NONE',  ( -11.59999999999999787, 0.000000000000000000, -43.79999999999998295 ) ) ;
#20148 = AXIS2_PLACEMENT_3D ( 'NONE', #63836, #35248, #58179 ) ;
#20149 = CARTESIAN_POINT ( 'NONE',  ( 10.00000000000000000, 0.000000000000000000, 0.000000000000000000 ) ) ;
#20150 = CARTESIAN_POINT ( 'NONE',  ( 97.64999999999997726, 88.47002178664753558, 76.29458333333333542 ) ) ;
#20151 = AXIS2_PLACEMENT_3D ( 'NONE', #58143, #1419, #69786 ) ;
#20152 = CARTESIAN_POINT ( 'NONE',  ( -2.500000000000011990, -62.44997998398397954, -269.9999999999999432 ) ) ;
#20153 = AXIS2_PLACEMENT_3D ( 'NONE', #24557, #8001, #70392 ) ;
#20154 = ORIENTED_EDGE ( 'NONE', *, *, #30107, .T. ) ;
#20155 = CARTESIAN_POINT ( 'NONE',  ( -94.99999999999997158, -213.0599564267049857, 87.06312500173430635 ) ) ;
#20156 = EDGE_CURVE ( 'NONE', #40784, #45539, #25642, .T. ) ;
#20157 = ORIENTED_EDGE ( 'NONE', *, *, #16964, .F. ) ;
#20158 = DIRECTION ( 'NONE',  ( 0.000000000000000000, 0.000000000000000000, -1.000000000000000000 ) ) ;
#20159 = ORIENTED_EDGE ( 'NONE', *, *, #14453, .F. ) ;
#20160 = CARTESIAN_POINT ( 'NONE',  ( -97.65000000000001990, 88.47002178664754979, 87.59229166840096070 ) ) ;
#20161 = CIRCLE ( 'NONE', #17750, 19.21700905503013601 ) ;
#20162 = VERTEX_POINT ( 'NONE', #9722 ) ;
#20163 = CARTESIAN_POINT ( 'NONE',  ( 93.84685191531248449, 88.00268892867053694, 85.46239583420047836 ) ) ;
#20164 = DIRECTION ( 'NONE',  ( 0.000000000000000000, 0.000000000000000000, 1.000000000000000000 ) ) ;
#20165 = DIRECTION ( 'NONE',  ( -1.000000000000000000, 0.000000000000000000, 0.000000000000000000 ) ) ;
#20166 = CARTESIAN_POINT ( 'NONE',  ( 11.99999999999999822, -71.91182617369167929, -28.89263327155821059 ) ) ;
#20167 = CARTESIAN_POINT ( 'NONE',  ( 10.00000000000000000, 21.53537804866081373, 30.80686688397018358 ) ) ;
#20168 = ORIENTED_EDGE ( 'NONE', *, *, #26603, .T. ) ;
#20169 = CYLINDRICAL_SURFACE ( 'NONE', #57939, 31.99999999999998579 ) ;
#20170 = DIRECTION ( 'NONE',  ( 0.000000000000000000, 0.000000000000000000, 1.000000000000000000 ) ) ;
#20171 = ORIENTED_EDGE ( 'NONE', *, *, #34446, .F. ) ;
#20172 = ORIENTED_EDGE ( 'NONE', *, *, #54847, .T. ) ;
#20173 = EDGE_CURVE ( 'NONE', #14992, #44417, #38295, .T. ) ;
#20174 = CARTESIAN_POINT ( 'NONE',  ( 10.00000000000000000, -25.88420570971381807, -27.13269053701123212 ) ) ;
#20175 = EDGE_CURVE ( 'NONE', #68980, #4178, #1696, .T. ) ;
#20176 = LINE ( 'NONE', #43140, #66059 ) ;
#20177 = CARTESIAN_POINT ( 'NONE',  ( -97.64999999999996305, -209.9999999999999716, 83.01499999999998636 ) ) ;
#20178 = CARTESIAN_POINT ( 'NONE',  ( -96.15314808468745866, -211.9973110713294489, 84.82739583420048746 ) ) ;
#20179 = ORIENTED_EDGE ( 'NONE', *, *, #49642, .T. ) ;
#20180 = AXIS2_PLACEMENT_3D ( 'NONE', #3997, #72389, #67878 ) ;
#20181 = LINE ( 'NONE', #43145, #52486 ) ;
#20182 = ORIENTED_EDGE ( 'NONE', *, *, #62309, .F. ) ;
#20183 = AXIS2_PLACEMENT_3D ( 'NONE', #6269, #63408, #51366 ) ;
#20184 = EDGE_CURVE ( 'NONE', #55652, #29642, #1993, .T. ) ;
#20185 = CARTESIAN_POINT ( 'NONE',  ( -10.00000000000000000, 0.000000000000000000, 0.000000000000000000 ) ) ;
#20186 = CARTESIAN_POINT ( 'NONE',  ( 93.84685191531248449, 91.99731107132950569, 89.69572916753382685 ) ) ;
#20187 = VECTOR ( 'NONE', #39256, 1000.000000000000000 ) ;
#20188 = CARTESIAN_POINT ( 'NONE',  ( 0.000000000000000000, 74.18225833017888249, 34.94270380257665209 ) ) ;
#20189 = CARTESIAN_POINT ( 'NONE',  ( 97.30629616937498838, 90.00000000000002842, 76.62531250086713897 ) ) ;
#20190 = AXIS2_PLACEMENT_3D ( 'NONE', #46660, #41033, #58310 ) ;
#20191 = FACE_OUTER_BOUND ( 'NONE', #24407, .T. ) ;
#20192 = DIRECTION ( 'NONE',  ( 0.000000000000000000, -0.2334453638558922628, -0.9723699203976798877 ) ) ;
#20193 = CYLINDRICAL_SURFACE ( 'NONE', #2582, 3.000000000000000888 ) ;
#20194 = CARTESIAN_POINT ( 'NONE',  ( 93.98225765065670601, 92.19538700400579501, 74.85985921673514554 ) ) ;
#20195 = DIRECTION ( 'NONE',  ( 0.000000000000000000, -0.9238795325112906243, 0.3826834323650805114 ) ) ;
#20196 = CYLINDRICAL_SURFACE ( 'NONE', #29787, 15.77977592589476608 ) ;
#20197 = ADVANCED_FACE ( 'NONE', ( #55587 ), #59849, .T. ) ;
#20198 = DIRECTION ( 'NONE',  ( -1.000000000000000000, -0.000000000000000000, -0.000000000000000000 ) ) ;
#20199 = CARTESIAN_POINT ( 'NONE',  ( 0.000000000000000000, 64.81221759200343513, 50.23322058963371006 ) ) ;
#20200 = VECTOR ( 'NONE', #572, 1000.000000000000000 ) ;
#20201 = VERTEX_POINT ( 'NONE', #36527 ) ;
#20202 = CARTESIAN_POINT ( 'NONE',  ( -93.84685191531254134, 91.99731107132950569, 83.71614583420047495 ) ) ;
#20203 = CARTESIAN_POINT ( 'NONE',  ( -90.00000000000002842, 95.00000000000002842, 90.00000000000000000 ) ) ;
#20204 = AXIS2_PLACEMENT_3D ( 'NONE', #20912, #60778, #42740 ) ;
#20205 = CIRCLE ( 'NONE', #30998, 77.49900000000000944 ) ;
#20207 = EDGE_CURVE ( 'NONE', #56328, #51709, #7959, .T. ) ;
#20206 = CARTESIAN_POINT ( 'NONE',  ( 92.35000000039364920, -209.9999706968037287, 82.45844277051352833 ) ) ;
#20208 = EDGE_CURVE ( 'NONE', #68971, #6723, #41803, .T. ) ;
#20209 = VERTEX_POINT ( 'NONE', #2373 ) ;
#20210 = DIRECTION ( 'NONE',  ( -1.000000000000000000, -0.000000000000000000, -0.000000000000000000 ) ) ;
#20211 = EDGE_CURVE ( 'NONE', #11722, #60065, #62915, .T. ) ;
#20212 = CARTESIAN_POINT ( 'NONE',  ( 94.99999999999998579, 93.05995642670504253, 85.39624999999998067 ) ) ;
#20213 = CARTESIAN_POINT ( 'NONE',  ( 96.82636346428385821, 88.24022384386941553, 74.93163452119478052 ) ) ;
#20214 = CARTESIAN_POINT ( 'NONE',  ( 93.84685191531251292, -211.9973110713294489, 80.38239583420048007 ) ) ;
#20215 = ORIENTED_EDGE ( 'NONE', *, *, #72615, .T. ) ;
#20216 = ORIENTED_EDGE ( 'NONE', *, *, #32001, .T. ) ;
#20217 = LINE ( 'NONE', #19846, #66807 ) ;
#20218 = CARTESIAN_POINT ( 'NONE',  ( 10.00000000000000000, 0.000000000000000000, 0.000000000000000000 ) ) ;
#20219 =( BOUNDED_CURVE ( )  B_SPLINE_CURVE ( 2, ( #14711, #4196, #9814, #3459, #60596, #72581, #44784 ),
 .UNSPECIFIED., .F., .F. ) 
 B_SPLINE_CURVE_WITH_KNOTS ( ( 3, 2, 2, 3 ),
 ( 0.3541666666666665741, 0.3611111111111109939, 0.3680555555555554137, 0.3749999999999998335 ),
 .UNSPECIFIED. ) 
 CURVE ( )  GEOMETRIC_REPRESENTATION_ITEM ( )  RATIONAL_B_SPLINE_CURVE ( ( 1.000000000000002220, 0.8660254037844365982, 1.000000000000000000, 0.8660254037844387076, 1.000000000000000000, 0.8660254037844419273, 0.9999999999999967804 ) ) 
 REPRESENTATION_ITEM ( '' )  );
#20220 = DIRECTION ( 'NONE',  ( -1.000000000000000000, 0.000000000000000000, 0.000000000000000000 ) ) ;
#20221 = CIRCLE ( 'NONE', #53893, 1.000000000000000000 ) ;
#20222 = VERTEX_POINT ( 'NONE', #51425 ) ;
#20223 = DIRECTION ( 'NONE',  ( 0.000000000000000000, 0.000000000000000000, 1.000000000000000000 ) ) ;
#20224 = CARTESIAN_POINT ( 'NONE',  ( 97.30629616937498838, -208.6684592857803011, 76.83697916753382628 ) ) ;
#20225 = CIRCLE ( 'NONE', #1084, 15.99999999999999645 ) ;
#20226 = AXIS2_PLACEMENT_3D ( 'NONE', #19737, #43067, #14477 ) ;
#20227 = ORIENTED_EDGE ( 'NONE', *, *, #9436, .F. ) ;
#20228 = FACE_BOUND ( 'NONE', #11954, .T. ) ;
#20229 = ORIENTED_EDGE ( 'NONE', *, *, #7905, .T. ) ;
#20230 = ORIENTED_EDGE ( 'NONE', *, *, #21925, .T. ) ;
#20231 = DIRECTION ( 'NONE',  ( -1.000000000000000000, -0.000000000000000000, -0.000000000000000000 ) ) ;
#20232 = AXIS2_PLACEMENT_3D ( 'NONE', #71410, #19182, #25202 ) ;
#20233 = DIRECTION ( 'NONE',  ( -0.000000000000000000, -0.000000000000000000, -1.000000000000000000 ) ) ;
#20234 = EDGE_LOOP ( 'NONE', ( #13127, #36802, #48068, #39684 ) ) ;
#20235 = DIRECTION ( 'NONE',  ( 1.000000000000000000, 0.000000000000000000, 0.000000000000000000 ) ) ;
#20236 = CARTESIAN_POINT ( 'NONE',  ( 92.35000000000000853, -209.9999999999999716, 84.36437500173430237 ) ) ;
#20237 = CARTESIAN_POINT ( 'NONE',  ( 96.32499999999997442, 92.29496732002878900, 84.07333333333333769 ) ) ;
#20238 = EDGE_LOOP ( 'NONE', ( #68129, #37578, #2152, #53624 ) ) ;
#20239 = CARTESIAN_POINT ( 'NONE',  ( -89.99999999999998579, -124.0000000000000142, -40.00000000000002132 ) ) ;
#20240 = LINE ( 'NONE', #31897, #28474 ) ;
#20241 = EDGE_LOOP ( 'NONE', ( #26191, #25286, #61665, #42842 ) ) ;
#20242 = ORIENTED_EDGE ( 'NONE', *, *, #15627, .F. ) ;
#20243 = CARTESIAN_POINT ( 'NONE',  ( -93.84685191531254134, 91.99731107132950569, 87.68489583420048916 ) ) ;
#20244 = CARTESIAN_POINT ( 'NONE',  ( 96.15314808468748708, 91.99731107132950569, 81.81114583420047381 ) ) ;
#20245 = EDGE_LOOP ( 'NONE', ( #68135, #5492, #21895, #3823 ) ) ;
#20246 = CIRCLE ( 'NONE', #20308, 37.49900000000000944 ) ;
#20247 = CARTESIAN_POINT ( 'NONE',  ( 97.64999999999999147, 90.00000000000002842, 82.77687500173431090 ) ) ;
#20248 = CIRCLE ( 'NONE', #22699, 31.99999999999998579 ) ;
#20249 = ADVANCED_FACE ( 'NONE', ( #67986 ), #5222, .F. ) ;
#20250 = DIRECTION ( 'NONE',  ( -1.000000000000000000, 0.000000000000000000, 0.000000000000000000 ) ) ;
#20251 = VERTEX_POINT ( 'NONE', #17221 ) ;
#20252 = FACE_BOUND ( 'NONE', #31636, .T. ) ;
#20253 = ORIENTED_EDGE ( 'NONE', *, *, #7508, .T. ) ;
#20254 = CIRCLE ( 'NONE', #38303, 31.99999999999999289 ) ;
#20255 = EDGE_LOOP ( 'NONE', ( #14831, #49366 ) ) ;
#20256 = ORIENTED_EDGE ( 'NONE', *, *, #31215, .F. ) ;
#20257 = LINE ( 'NONE', #39336, #56566 ) ;
#20258 = EDGE_CURVE ( 'NONE', #47563, #24844, #10066, .T. ) ;
#20259 = DIRECTION ( 'NONE',  ( -1.000000000000000000, -0.000000000000000000, 0.000000000000000000 ) ) ;
#20260 = AXIS2_PLACEMENT_3D ( 'NONE', #4919, #10910, #15805 ) ;
#20261 = VECTOR ( 'NONE', #11696, 1000.000000000000000 ) ;
#20262 = CARTESIAN_POINT ( 'NONE',  ( -97.65000000000001990, 90.00000000000004263, 84.28499999999999659 ) ) ;
#20263 = EDGE_CURVE ( 'NONE', #9063, #56318, #59292, .T. ) ;
#20264 = EDGE_LOOP ( 'NONE', ( #39956, #14822, #25955, #60799 ) ) ;
#20265 = CARTESIAN_POINT ( 'NONE',  ( -92.34999999999999432, -208.4700217866474645, 80.92479166840097093 ) ) ;
#20266 = STYLED_ITEM ( 'NONE', ( #19388 ), #37031 ) ;
#20267 = CARTESIAN_POINT ( 'NONE',  ( 96.32499999999998863, 87.70503267997126784, 89.02104166840096866 ) ) ;
#20268 = ORIENTED_EDGE ( 'NONE', *, *, #59491, .T. ) ;
#20269 = CARTESIAN_POINT ( 'NONE',  ( -0.0004442498525516064278, 0.001194404164626844313, -80.00000000000000000 ) ) ;
#20270 = CARTESIAN_POINT ( 'NONE',  ( -93.84685191531247028, -211.9973110713294489, 77.78947916753381264 ) ) ;
#20271 = ORIENTED_EDGE ( 'NONE', *, *, #46421, .T. ) ;
#20272 = CARTESIAN_POINT ( 'NONE',  ( 10.00000000000000000, 22.48208911017551515, -35.47612816024499693 ) ) ;
#20273 = CARTESIAN_POINT ( 'NONE',  ( 11.99999999999999822, -31.46837873495025306, 68.27212725128265447 ) ) ;
#20274 = FACE_OUTER_BOUND ( 'NONE', #52240, .T. ) ;
#20275 = CARTESIAN_POINT ( 'NONE',  ( 10.00000000000000000, 76.41127070299273782, 12.93880638057342836 ) ) ;
#20276 = ADVANCED_FACE ( 'NONE', ( #11210 ), #39045, .F. ) ;
#20277 = DIRECTION ( 'NONE',  ( -1.000000000000000000, 0.000000000000000000, 0.000000000000000000 ) ) ;
#20278 = DIRECTION ( 'NONE',  ( -0.000000000000000000, -0.000000000000000000, 1.000000000000000000 ) ) ;
#20279 = CARTESIAN_POINT ( 'NONE',  ( 97.30629616937498838, 90.00000000000002842, 87.42031250086714067 ) ) ;
#20280 = DIRECTION ( 'NONE',  ( 1.000000000000000000, 0.000000000000000000, 0.000000000000000000 ) ) ;
#20281 = LINE ( 'NONE', #38703, #27983 ) ;
#20282 = DIRECTION ( 'NONE',  ( 1.000000000000000000, 0.000000000000000000, 0.000000000000000000 ) ) ;
#20283 = CIRCLE ( 'NONE', #58717, 37.49900000000000233 ) ;
#20284 = CARTESIAN_POINT ( 'NONE',  ( -92.69370383062502583, 91.33154071421968467, 76.04322916753380923 ) ) ;
#20285 = DIRECTION ( 'NONE',  ( -1.000000000000000000, 0.000000000000000000, 0.000000000000000000 ) ) ;
#20286 = DIRECTION ( 'NONE',  ( 0.000000000000000000, 0.000000000000000000, 1.000000000000000000 ) ) ;
#20287 = EDGE_CURVE ( 'NONE', #18187, #15802, #22120, .T. ) ;
#20288 = DIRECTION ( 'NONE',  ( 0.000000000000000000, -0.7431448254773870277, -0.6691306063588662312 ) ) ;
#20289 = AXIS2_PLACEMENT_3D ( 'NONE', #54221, #59861, #25635 ) ;
#20290 = ADVANCED_FACE ( 'NONE', ( #51058 ), #62362, .F. ) ;
#20291 = CARTESIAN_POINT ( 'NONE',  ( 0.000000000000000000, -68.27212725128298132, 31.46837873494953541 ) ) ;
#20292 = ADVANCED_FACE ( 'NONE', ( #5963 ), #55958, .T. ) ;
#20293 = VECTOR ( 'NONE', #73490, 1000.000000000000000 ) ;
#20294 = VECTOR ( 'NONE', #9021, 1000.000000000000000 ) ;
#20295 = UNCERTAINTY_MEASURE_WITH_UNIT (LENGTH_MEASURE( 1.000000000000000082E-05 ), #44678, 'distance_accuracy_value', 'NONE');
#20296 = LINE ( 'NONE', #33422, #4069 ) ;
#20297 = PLANE ( 'NONE',  #62254 ) ;
#20299 = VECTOR ( 'NONE', #72159, 1000.000000000000000 ) ;
#20298 = CARTESIAN_POINT ( 'NONE',  ( -3.000000000000002665, 0.000000000000000000, 20.64000000000000057 ) ) ;
#20300 = CARTESIAN_POINT ( 'NONE',  ( 93.67499999999999716, 87.70503267997126784, 75.58020833506763836 ) ) ;
#20301 = CARTESIAN_POINT ( 'NONE',  ( -97.64999999999994884, -208.4700217866474645, 88.04208333333332348 ) ) ;
#20302 = CARTESIAN_POINT ( 'NONE',  ( -93.62329079302944024, 87.70919997534043944, 75.00000000000000000 ) ) ;
#20303 = EDGE_CURVE ( 'NONE', #35138, #33465, #35249, .T. ) ;
#20304 = ADVANCED_FACE ( 'NONE', ( #5591 ), #73982, .T. ) ;
#20305 = ORIENTED_EDGE ( 'NONE', *, *, #44761, .T. ) ;
#20306 = LINE ( 'NONE', #21039, #67116 ) ;
#20307 = LINE ( 'NONE', #3055, #68300 ) ;
#20309 = PRESENTATION_STYLE_ASSIGNMENT (( #7922 ) ) ;
#20308 = AXIS2_PLACEMENT_3D ( 'NONE', #21097, #13619, #2761 ) ;
#20310 = CARTESIAN_POINT ( 'NONE',  ( -96.32500000000001705, 92.29496732002878900, 84.81416666666666515 ) ) ;
#20311 = CIRCLE ( 'NONE', #52677, 31.99999999999999289 ) ;
#20312 = AXIS2_PLACEMENT_3D ( 'NONE', #47416, #42516, #8677 ) ;
#20313 = AXIS2_PLACEMENT_3D ( 'NONE', #11200, #27747, #34126 ) ;
#20314 = ORIENTED_EDGE ( 'NONE', *, *, #18815, .T. ) ;
#20315 = AXIS2_PLACEMENT_3D ( 'NONE', #34570, #69167, #62809 ) ;
#20316 = ORIENTED_EDGE ( 'NONE', *, *, #66871, .T. ) ;
#20317 = CIRCLE ( 'NONE', #8299, 42.00000000000000000 ) ;
#20318 = DIRECTION ( 'NONE',  ( 0.000000000000000000, 0.000000000000000000, 1.000000000000000000 ) ) ;
#20319 = DIRECTION ( 'NONE',  ( -1.000000000000000000, 0.000000000000000000, 0.000000000000000000 ) ) ;
#20320 = ORIENTED_EDGE ( 'NONE', *, *, #17223, .F. ) ;
#20321 = AXIS2_PLACEMENT_3D ( 'NONE', #51024, #57045, #22457 ) ;
#20322 = CARTESIAN_POINT ( 'NONE',  ( 93.84685191531249870, -208.0026889286704943, 81.28197916753380525 ) ) ;
#20323 = CARTESIAN_POINT ( 'NONE',  ( 97.30629616937498838, -208.6684592857803295, 83.82197916753382572 ) ) ;
#20324 = ORIENTED_EDGE ( 'NONE', *, *, #26540, .T. ) ;
#20325 = CARTESIAN_POINT ( 'NONE',  ( 97.30629616937498838, -208.6684592857803011, 85.72697916753381264 ) ) ;
#20326 = ORIENTED_EDGE ( 'NONE', *, *, #24507, .F. ) ;
#20327 = FACE_BOUND ( 'NONE', #36709, .T. ) ;
#20328 = EDGE_LOOP ( 'NONE', ( #49283, #40959, #25066, #73306 ) ) ;
#20329 = CARTESIAN_POINT ( 'NONE',  ( -93.84685191531252713, 88.00268892867056536, 78.58322916753382970 ) ) ;
#20330 = ORIENTED_EDGE ( 'NONE', *, *, #6247, .F. ) ;
#20331 = ORIENTED_EDGE ( 'NONE', *, *, #53638, .F. ) ;
#20332 = CARTESIAN_POINT ( 'NONE',  ( 0.000000000000000000, -25.88420570971419821, 27.13269053701087330 ) ) ;
#20333 = VERTEX_POINT ( 'NONE', #61603 ) ;
#20334 = CARTESIAN_POINT ( 'NONE',  ( -2.500000000000015543, -73.00000000000001421, -204.9999999999999716 ) ) ;
#20335 = CARTESIAN_POINT ( 'NONE',  ( 15.00000000000000000, 23.59884966291538078, 12.14883922797231008 ) ) ;
#20336 = ORIENTED_EDGE ( 'NONE', *, *, #21047, .T. ) ;
#20337 = CARTESIAN_POINT ( 'NONE',  ( 0.000000000000000000, 49.70050353004975818, -59.46389618801909904 ) ) ;
#20338 = ORIENTED_EDGE ( 'NONE', *, *, #62316, .T. ) ;
#20339 = DIRECTION ( 'NONE',  ( 0.000000000000000000, -0.7071067811865389130, -0.7071067811865562325 ) ) ;
#20340 = CIRCLE ( 'NONE', #50346, 37.49900000000000944 ) ;
#20341 = EDGE_LOOP ( 'NONE', ( #4915, #11263, #59812, #64820 ) ) ;
#20342 = AXIS2_PLACEMENT_3D ( 'NONE', #65353, #1493, #24379 ) ;
#20343 = EDGE_CURVE ( 'NONE', #67844, #10235, #34024, .T. ) ;
#20344 = CONICAL_SURFACE ( 'NONE', #51581, 12.85999999999999943, 0.7853981633974482790 ) ;
#20345 = ORIENTED_EDGE ( 'NONE', *, *, #43825, .F. ) ;
#20346 = ORIENTED_EDGE ( 'NONE', *, *, #55522, .F. ) ;
#20347 = CARTESIAN_POINT ( 'NONE',  ( 95.00000000000000000, -212.6630814284392557, 79.00656250086713328 ) ) ;
#20348 = DIRECTION ( 'NONE',  ( -0.000000000000000000, -0.000000000000000000, -1.000000000000000000 ) ) ;
#20349 = CONTEXT_DEPENDENT_SHAPE_REPRESENTATION ( #34016, #57245 ) ;
#20350 = CARTESIAN_POINT ( 'NONE',  ( 0.000000000000000000, 40.98264845739749518, 9.188173127307448951 ) ) ;
#20352 = ADVANCED_FACE ( 'NONE', ( #38673 ), #73239, .T. ) ;
#20351 = ORIENTED_EDGE ( 'NONE', *, *, #32810, .F. ) ;
#20353 = ORIENTED_EDGE ( 'NONE', *, *, #28244, .T. ) ;
#20354 = DIRECTION ( 'NONE',  ( 0.000000000000000000, -6.982962677686266711E-15, 1.000000000000000000 ) ) ;
#20355 = B_SPLINE_CURVE_WITH_KNOTS ( 'NONE', 3,
 ( #44421, #67342, #15086, #45163, #73339, #27478, #33114, #56062, #60959, #4579, #39523, #33872, #55691, #16206, #10561, #72588, #4208, #27099, #50031, #32375 ),
 .UNSPECIFIED., .F., .F.,
 ( 4, 2, 2, 2, 2, 2, 2, 2, 2, 4 ),
 ( 2.781148944256651962E-07, 0.0008372784139787452749, 0.001674278713063064939, 0.002511279012147384603, 0.003348279311231704483, 0.003766779460773864857, 0.004185279610316025231, 0.005022279909400345112, 0.005859280208484664992, 0.006696280507568985740 ),
 .UNSPECIFIED. ) ;
#20356 = EDGE_CURVE ( 'NONE', #36497, #45028, #50853, .T. ) ;
#20357 = VECTOR ( 'NONE', #57933, 1000.000000000000000 ) ;
#20358 = ORIENTED_EDGE ( 'NONE', *, *, #66728, .T. ) ;
#20359 = DIRECTION ( 'NONE',  ( 1.000000000000000000, 0.000000000000000000, 0.000000000000000000 ) ) ;
#20360 = EDGE_CURVE ( 'NONE', #3632, #12392, #50304, .T. ) ;
#20361 = CARTESIAN_POINT ( 'NONE',  ( -92.35000000002563070, -209.9999999999999716, -74.99999999999356248 ) ) ;
#20362 = CARTESIAN_POINT ( 'NONE',  ( -96.15314808468751551, 88.00268892867056536, 80.38239583420048007 ) ) ;
#20363 = ORIENTED_EDGE ( 'NONE', *, *, #47308, .T. ) ;
#20364 = CARTESIAN_POINT ( 'NONE',  ( 97.30629616937498838, 90.00000000000002842, 76.62531250086713897 ) ) ;
#20365 = ORIENTED_EDGE ( 'NONE', *, *, #9533, .F. ) ;
#20366 = DIRECTION ( 'NONE',  ( 0.9227826878668540234, 0.3853207896976547087, 0.000000000000000000 ) ) ;
#20367 = CARTESIAN_POINT ( 'NONE',  ( -94.99999999999997158, -212.6630814284392557, 87.89656250086713385 ) ) ;
#20368 = FACE_OUTER_BOUND ( 'NONE', #73986, .T. ) ;
#20369 = CARTESIAN_POINT ( 'NONE',  ( 10.00000000000000000, -41.76937507738745836, -62.50329211542482710 ) ) ;
#20370 = DIRECTION ( 'NONE',  ( -1.000000000000000000, 0.000000000000000000, -0.000000000000000000 ) ) ;
#20371 = CARTESIAN_POINT ( 'NONE',  ( -97.30629616937497417, -211.3315407142195852, 82.07572916753382231 ) ) ;
#20372 = CIRCLE ( 'NONE', #28737, 4.750000000000000000 ) ;
#20373 = ADVANCED_FACE ( 'NONE', ( #40156 ), #27371, .F. ) ;
#20374 = DIRECTION ( 'NONE',  ( 0.000000000000000000, -0.9510565162951543083, 0.3090169943749448977 ) ) ;
#20375 = CARTESIAN_POINT ( 'NONE',  ( -3.000000000000000000, -14.54903810567676636, 22.19967320028755964 ) ) ;
#20376 = CARTESIAN_POINT ( 'NONE',  ( 15.00000000000000000, -0.9646360437375368635, -23.52805723605589705 ) ) ;
#20377 = VERTEX_POINT ( 'NONE', #4856 ) ;
#20378 = AXIS2_PLACEMENT_3D ( 'NONE', #4750, #73881, #72753 ) ;
#20379 = CIRCLE ( 'NONE', #17964, 31.99999999999998579 ) ;
#20380 = VERTEX_POINT ( 'NONE', #44696 ) ;
#20381 = DIRECTION ( 'NONE',  ( -0.000000000000000000, 0.4067366430758000417, -0.9135454576426009776 ) ) ;
#20382 = CIRCLE ( 'NONE', #38416, 31.99999999999999289 ) ;
#20383 = AXIS2_PLACEMENT_3D ( 'NONE', #72810, #25855, #49525 ) ;
#20384 = DIRECTION ( 'NONE',  ( -1.000000000000000000, -0.000000000000000000, -0.000000000000000000 ) ) ;
#20385 = DIRECTION ( 'NONE',  ( 1.000000000000000000, 0.000000000000000000, 0.000000000000000000 ) ) ;
#20386 = CARTESIAN_POINT ( 'NONE',  ( -96.15314808468752972, 91.99731107132950569, 86.36197916753381776 ) ) ;
#20387 = CARTESIAN_POINT ( 'NONE',  ( -95.67252605959615153, -207.6887180216938020, 74.85222950654856788 ) ) ;
#20388 = LINE ( 'NONE', #42581, #12186 ) ;
#20389 = ADVANCED_FACE ( 'NONE', ( #16104 ), #58543, .T. ) ;
#20390 = CARTESIAN_POINT ( 'NONE',  ( 0.000000000000000000, 0.000000000000000000, 0.000000000000000000 ) ) ;
#20391 = ORIENTED_EDGE ( 'NONE', *, *, #12478, .F. ) ;
#20392 = EDGE_CURVE ( 'NONE', #54097, #65643, #40088, .T. ) ;
#20393 = DIRECTION ( 'NONE',  ( 1.000000000000000000, -3.061616997868382648E-16, -0.000000000000000000 ) ) ;
#20394 = EDGE_CURVE ( 'NONE', #60472, #64608, #17589, .T. ) ;
#20396 = ADVANCED_FACE ( 'NONE', ( #30703 ), #29225, .T. ) ;
#20395 = CARTESIAN_POINT ( 'NONE',  ( 0.000000000000000000, -22.67460108101782978, 6.353146135317912169 ) ) ;
#20397 = DIRECTION ( 'NONE',  ( -1.000000000000000000, 0.000000000000000000, -0.000000000000000000 ) ) ;
#20398 = CARTESIAN_POINT ( 'NONE',  ( 0.000000000000000000, 71.27951684758068041, -30.41916302227036439 ) ) ;
#20399 = CARTESIAN_POINT ( 'NONE',  ( -2.991272306860052410, 4.046490820311134939, -0.5592653008974223239 ) ) ;
#20400 = CARTESIAN_POINT ( 'NONE',  ( 50.00005079999999680, 2.571758278209441661E-15, -21.00000000000000000 ) ) ;
#20401 = DIRECTION ( 'NONE',  ( -1.000000000000000000, -0.000000000000000000, -0.000000000000000000 ) ) ;
#20402 = CARTESIAN_POINT ( 'NONE',  ( -92.69370383062498320, -209.9999999999999716, 83.76906250086716454 ) ) ;
#20403 = EDGE_CURVE ( 'NONE', #30983, #9893, #18444, .T. ) ;
#20404 = AXIS2_PLACEMENT_3D ( 'NONE', #14052, #43767, #9542 ) ;
#20405 = LINE ( 'NONE', #44077, #68317 ) ;
#20406 = VECTOR ( 'NONE', #60999, 1000.000000000000000 ) ;
#20407 = CARTESIAN_POINT ( 'NONE',  ( -93.33921851433959205, -211.6002521295065435, 74.80065602173004891 ) ) ;
#20408 = CARTESIAN_POINT ( 'NONE',  ( -92.34999999999998010, 88.47002178664760663, 88.99458333333333826 ) ) ;
#20409 = ORIENTED_EDGE ( 'NONE', *, *, #14926, .F. ) ;
#20410 = EDGE_CURVE ( 'NONE', #23771, #2356, #69820, .T. ) ;
#20411 = CARTESIAN_POINT ( 'NONE',  ( -92.34999999999999432, -211.5299782133524218, 82.08895833506764461 ) ) ;
#20412 = LINE ( 'NONE', #71152, #13066 ) ;
#20413 = AXIS2_PLACEMENT_3D ( 'NONE', #70027, #5799, #58022 ) ;
#20414 = DIRECTION ( 'NONE',  ( 0.000000000000000000, -0.2079116908177532363, 0.9781476007338069101 ) ) ;
#20415 = AXIS2_PLACEMENT_3D ( 'NONE', #3006, #25899, #19881 ) ;
#20416 = DIRECTION ( 'NONE',  ( 0.000000000000000000, 0.000000000000000000, 1.000000000000000000 ) ) ;
#20417 = ORIENTED_EDGE ( 'NONE', *, *, #47358, .T. ) ;
#20418 = CARTESIAN_POINT ( 'NONE',  ( 10.00000000000000000, -14.67089635893764665, 73.72996012237435082 ) ) ;
#20419 = CARTESIAN_POINT ( 'NONE',  ( -21.33958957442910886, -129.9559990355020034, 5.500000000000000000 ) ) ;
#20420 = ORIENTED_EDGE ( 'NONE', *, *, #69088, .F. ) ;
#20421 = CARTESIAN_POINT ( 'NONE',  ( -12.50000000000000000, -132.5000000000000000, 2.500000000000000000 ) ) ;
#20422 = VERTEX_POINT ( 'NONE', #53281 ) ;
#20423 = AXIS2_PLACEMENT_3D ( 'NONE', #39344, #34427, #5145 ) ;
#20424 = ORIENTED_EDGE ( 'NONE', *, *, #26121, .F. ) ;
#20425 = FACE_BOUND ( 'NONE', #4201, .T. ) ;
#20426 = AXIS2_PLACEMENT_3D ( 'NONE', #71322, #14191, #43166 ) ;
#20427 = CIRCLE ( 'NONE', #62475, 37.49900000000000233 ) ;
#20428 = ORIENTED_EDGE ( 'NONE', *, *, #35255, .T. ) ;
#20429 = ORIENTED_EDGE ( 'NONE', *, *, #45150, .F. ) ;
#20430 = AXIS2_PLACEMENT_3D ( 'NONE', #25978, #48907, #54200 ) ;
#20431 = ORIENTED_EDGE ( 'NONE', *, *, #65130, .F. ) ;
#20432 = CIRCLE ( 'NONE', #61281, 31.99999999999998579 ) ;
#20433 = EDGE_LOOP ( 'NONE', ( #20624, #15650, #58807, #70244 ) ) ;
#20434 = CYLINDRICAL_SURFACE ( 'NONE', #67150, 2.649999999999999467 ) ;
#20435 = VERTEX_POINT ( 'NONE', #64563 ) ;
#20436 = VERTEX_POINT ( 'NONE', #13044 ) ;
#20437 = CARTESIAN_POINT ( 'NONE',  ( 92.69370383062498320, 90.00000000000002842, 75.19656250086714522 ) ) ;
#20438 = CARTESIAN_POINT ( 'NONE',  ( 6.000000000000000000, 22.90783923731740401, -78.73519480814930205 ) ) ;
#20439 = CARTESIAN_POINT ( 'NONE',  ( -7.469491406282117829, 4.756046723998917258, -64.01812422950395387 ) ) ;
#20440 = VERTEX_POINT ( 'NONE', #64204 ) ;
#20441 = VERTEX_POINT ( 'NONE', #52916 ) ;
#20442 = EDGE_CURVE ( 'NONE', #31367, #31252, #63838, .T. ) ;
#20443 = ORIENTED_EDGE ( 'NONE', *, *, #43801, .T. ) ;
#20444 = PLANE ( 'NONE',  #73087 ) ;
#20445 = ORIENTED_EDGE ( 'NONE', *, *, #56090, .F. ) ;
#20446 = CARTESIAN_POINT ( 'NONE',  ( 92.69370383062501162, -211.3315407142195852, 89.06072916753379332 ) ) ;
#20447 = CARTESIAN_POINT ( 'NONE',  ( 4.553649124439118623E-15, 4.011548038196366406E-15, 52.00000000000002132 ) ) ;
#20448 = DIRECTION ( 'NONE',  ( -1.000000000000000000, 0.000000000000000000, 0.000000000000000000 ) ) ;
#20449 = EDGE_CURVE ( 'NONE', #6916, #39794, #7041, .T. ) ;
#20450 = CARTESIAN_POINT ( 'NONE',  ( -97.51367041768835975, 89.99999999999990052, 74.91808492278043730 ) ) ;
#20451 = DIRECTION ( 'NONE',  ( 0.000000000000000000, 0.000000000000000000, 1.000000000000000000 ) ) ;
#20452 = DIRECTION ( 'NONE',  ( 0.000000000000000000, 0.000000000000000000, 1.000000000000000000 ) ) ;
#20453 = DIRECTION ( 'NONE',  ( -0.000000000000000000, -0.000000000000000000, 1.000000000000000000 ) ) ;
#20454 = EDGE_CURVE ( 'NONE', #68894, #58552, #33824, .T. ) ;
#20455 = CARTESIAN_POINT ( 'NONE',  ( 0.000000000000000000, -24.73286445877757345, 73.44644590900053061 ) ) ;
#20456 = EDGE_CURVE ( 'NONE', #71442, #49949, #6679, .T. ) ;
#20457 = CARTESIAN_POINT ( 'NONE',  ( -96.32499999999996021, -212.2949673200287179, 77.48520833506763950 ) ) ;
#20458 = CARTESIAN_POINT ( 'NONE',  ( -92.69370383062502583, 88.66845928578038638, 88.16114583420048234 ) ) ;
#20459 = ORIENTED_EDGE ( 'NONE', *, *, #64946, .F. ) ;
#20461 = CARTESIAN_POINT ( 'NONE',  ( -92.69370383062502583, 88.66845928578038638, 87.36739583420047950 ) ) ;
#20460 = CARTESIAN_POINT ( 'NONE',  ( 97.30629616937498838, 88.66845928578037217, 88.63739583420047552 ) ) ;
#20462 = ORIENTED_EDGE ( 'NONE', *, *, #64847, .T. ) ;
#20463 = CARTESIAN_POINT ( 'NONE',  ( 92.69370383062498320, 90.00000000000002842, 76.46656250086715545 ) ) ;
#20464 = CARTESIAN_POINT ( 'NONE',  ( 11.99999999999999822, -81.34940948281328588, -10.30890764327469356 ) ) ;
#20465 = CARTESIAN_POINT ( 'NONE',  ( 95.00000000000000000, -209.9999999999999716, 90.00000000000000000 ) ) ;
#20466 = CARTESIAN_POINT ( 'NONE',  ( -97.64999999999996305, -209.9999999999999716, 86.82500000000000284 ) ) ;
#20467 = CARTESIAN_POINT ( 'NONE',  ( 11.99999999999999822, -75.54627589209931671, -17.28742895386162814 ) ) ;
#20468 = DIRECTION ( 'NONE',  ( 0.000000000000000000, 0.000000000000000000, -1.000000000000000000 ) ) ;
#20469 = VECTOR ( 'NONE', #45470, 1000.000000000000000 ) ;
#20470 = DIRECTION ( 'NONE',  ( -1.000000000000000000, -0.000000000000000000, 0.000000000000000000 ) ) ;
#20471 = DIRECTION ( 'NONE',  ( -1.000000000000000000, -0.000000000000000000, 0.000000000000000000 ) ) ;
#20472 = VERTEX_POINT ( 'NONE', #41266 ) ;
#20473 = ORIENTED_EDGE ( 'NONE', *, *, #67246, .T. ) ;
#20474 = CIRCLE ( 'NONE', #22903, 0.5999999999999998668 ) ;
#20475 = ADVANCED_FACE ( 'NONE', ( #35610 ), #23602, .T. ) ;
#20476 = FACE_OUTER_BOUND ( 'NONE', #54763, .T. ) ;
#20477 = LINE ( 'NONE', #25741, #3419 ) ;
#20478 = PLANE ( 'NONE',  #65132 ) ;
#20479 = CARTESIAN_POINT ( 'NONE',  ( 10.00000000000000000, -2.946379043146863719, 75.11764819372146462 ) ) ;
#20480 = DIRECTION ( 'NONE',  ( -0.000000000000000000, -0.000000000000000000, -1.000000000000000000 ) ) ;
#20481 = CARTESIAN_POINT ( 'NONE',  ( -92.69370383062498320, -208.6684592857803011, 74.93197916753381094 ) ) ;
#20482 =( BOUNDED_CURVE ( )  B_SPLINE_CURVE ( 2, ( #25530, #13868, #8622, #19515, #14620, #19883, #48098 ),
 .UNSPECIFIED., .F., .F. ) 
 B_SPLINE_CURVE_WITH_KNOTS ( ( 3, 2, 2, 3 ),
 ( 0.1270039290051390157, 0.1340595452767650575, 0.1411153108176474713, 0.1481709449575358828 ),
 .UNSPECIFIED. ) 
 CURVE ( )  GEOMETRIC_REPRESENTATION_ITEM ( )  RATIONAL_B_SPLINE_CURVE ( ( 0.9999943314824852880, 0.8660282381031578769, 1.000000000000000000, 0.8660254037844387076, 1.000000000000000000, 0.8660278988213007123, 0.9999950100192072089 ) ) 
 REPRESENTATION_ITEM ( '' )  );
#20483 = ORIENTED_EDGE ( 'NONE', *, *, #54273, .F. ) ;
#20484 = CARTESIAN_POINT ( 'NONE',  ( -92.69370383062504004, 90.00000000000004263, 82.34031250086714238 ) ) ;
#20485 = CIRCLE ( 'NONE', #62518, 31.99999999999998934 ) ;
#20486 = DIRECTION ( 'NONE',  ( 1.000000000000000000, 1.427937372958405461E-15, 7.962523111839130290E-16 ) ) ;
#20487 = AXIS2_PLACEMENT_3D ( 'NONE', #4567, #16196, #3827 ) ;
#20488 = EDGE_CURVE ( 'NONE', #18578, #52314, #1819, .T. ) ;
#20489 = EDGE_CURVE ( 'NONE', #41023, #61214, #21802, .T. ) ;
#20490 = VECTOR ( 'NONE', #18414, 1000.000000000000000 ) ;
#20491 = CARTESIAN_POINT ( 'NONE',  ( 5.000000000000000000, 16.65560815589464028, -38.55633173626993226 ) ) ;
#20492 = DIRECTION ( 'NONE',  ( -1.000000000000000000, 0.000000000000000000, 0.000000000000000000 ) ) ;
#20493 = CARTESIAN_POINT ( 'NONE',  ( 10.00000000000000000, 23.16143007188426850, 73.95703589263983702 ) ) ;
#20494 = CARTESIAN_POINT ( 'NONE',  ( -97.64999999999996305, -209.9999999999999716, 87.45999999999999375 ) ) ;
#20495 = DIRECTION ( 'NONE',  ( -1.000000000000000000, 0.000000000000000000, 0.000000000000000000 ) ) ;
#20496 = VECTOR ( 'NONE', #54264, 1000.000000000000000 ) ;
#20497 = CARTESIAN_POINT ( 'NONE',  ( -97.64999999993855795, 90.00001182123732235, 81.82400613091868991 ) ) ;
#20498 = CARTESIAN_POINT ( 'NONE',  ( 0.000000000000000000, 0.000000000000000000, 0.000000000000000000 ) ) ;
#20499 = CARTESIAN_POINT ( 'NONE',  ( 94.99999999999998579, 92.66308142843932671, 79.48281250086715488 ) ) ;
#20500 = CARTESIAN_POINT ( 'NONE',  ( -93.84685191531248449, -208.0026889286704943, 84.50989583420049200 ) ) ;
#20501 = CYLINDRICAL_SURFACE ( 'NONE', #14627, 77.49899999999999523 ) ;
#20502 = VERTEX_POINT ( 'NONE', #52529 ) ;
#20503 = CARTESIAN_POINT ( 'NONE',  ( -92.34999999999993747, -211.5299782133523934, 81.37458333333333371 ) ) ;
#20504 = CARTESIAN_POINT ( 'NONE',  ( -96.32499999999996021, -207.7050326799711968, 77.19416666666666060 ) ) ;
#20505 = DIRECTION ( 'NONE',  ( 0.000000000000000000, 0.000000000000000000, 1.000000000000000000 ) ) ;
#20506 = CARTESIAN_POINT ( 'NONE',  ( 96.15314808468748708, -208.0026889286704943, 82.44614583420046472 ) ) ;
#20507 = ORIENTED_EDGE ( 'NONE', *, *, #38353, .T. ) ;
#20508 = CARTESIAN_POINT ( 'NONE',  ( 97.30629616937500259, 90.00000000000002842, 74.79348190356851944 ) ) ;
#20509 = ORIENTED_EDGE ( 'NONE', *, *, #50735, .F. ) ;
#20510 = CARTESIAN_POINT ( 'NONE',  ( 15.00000000000000000, -13.04903810567675393, -19.60159698893424718 ) ) ;
#20511 = VERTEX_POINT ( 'NONE', #12312 ) ;
#20512 = VECTOR ( 'NONE', #64505, 1000.000000000000000 ) ;
#20513 = AXIS2_PLACEMENT_3D ( 'NONE', #1370, #30253, #23155 ) ;
#20515 = AXIS2_PLACEMENT_3D ( 'NONE', #73451, #44902, #67075 ) ;
#20514 = CARTESIAN_POINT ( 'NONE',  ( -94.99999999999997158, -209.9999999999999716, 90.00000000000000000 ) ) ;
#20516 = ORIENTED_EDGE ( 'NONE', *, *, #35004, .T. ) ;
#20517 = CARTESIAN_POINT ( 'NONE',  ( 97.30629616937498838, -211.3315407142195852, 78.63614583420046245 ) ) ;
#20518 = FACE_OUTER_BOUND ( 'NONE', #64196, .T. ) ;
#20519 = CARTESIAN_POINT ( 'NONE',  ( -92.35000000000400178, 89.99999541993113894, 76.42687486206344261 ) ) ;
#20520 = CARTESIAN_POINT ( 'NONE',  ( -97.51895106303135208, 89.82936612246383845, 74.92125785461006160 ) ) ;
#20521 = CARTESIAN_POINT ( 'NONE',  ( 5.000000000000000000, 21.60688246758696707, -79.10210256391346206 ) ) ;
#20522 = CARTESIAN_POINT ( 'NONE',  ( 0.000000000000000000, -68.27212725128254078, -31.46837873495049465 ) ) ;
#20523 = CARTESIAN_POINT ( 'NONE',  ( 95.00000000000000000, -213.0599564267049857, 79.99874999999998693 ) ) ;
#20524 = ADVANCED_FACE ( 'NONE', ( #41625 ), #36351, .T. ) ;
#20525 = AXIS2_PLACEMENT_3D ( 'NONE', #64313, #65785, #48124 ) ;
#20526 = ORIENTED_EDGE ( 'NONE', *, *, #7732, .F. ) ;
#20527 = EDGE_LOOP ( 'NONE', ( #22232, #50764, #19785, #43190 ) ) ;
#20528 = ORIENTED_EDGE ( 'NONE', *, *, #46698, .T. ) ;
#20529 = ORIENTED_EDGE ( 'NONE', *, *, #41767, .T. ) ;
#20530 = DIRECTION ( 'NONE',  ( -0.000000000000000000, -0.000000000000000000, 1.000000000000000000 ) ) ;
#20531 = AXIS2_PLACEMENT_3D ( 'NONE', #63382, #29883, #52837 ) ;
#20532 = AXIS2_PLACEMENT_3D ( 'NONE', #5974, #40528, #11950 ) ;
#20533 = CARTESIAN_POINT ( 'NONE',  ( -95.00000000000002842, 92.66308142843932671, 83.29281250086717137 ) ) ;
#20534 = ADVANCED_FACE ( 'NONE', ( #58180 ), #6325, .T. ) ;
#20535 = CARTESIAN_POINT ( 'NONE',  ( -96.32500000000001705, 87.70503267997129626, 81.93020833506763267 ) ) ;
#20536 = VECTOR ( 'NONE', #6359, 1000.000000000000114 ) ;
#20537 = DIRECTION ( 'NONE',  ( -0.000000000000000000, -0.000000000000000000, -1.000000000000000000 ) ) ;
#20538 = DIRECTION ( 'NONE',  ( -2.603472992746261562E-14, -2.546204323184492723E-14, 1.000000000000000000 ) ) ;
#20539 = LINE ( 'NONE', #9627, #28412 ) ;
#20541 = EDGE_LOOP ( 'NONE', ( #45021, #49319, #33171, #13226 ) ) ;
#20540 = ADVANCED_FACE ( 'NONE', ( #23977 ), #69460, .F. ) ;
#20542 = CARTESIAN_POINT ( 'NONE',  ( -97.64999999999994884, -208.4700217866474645, 84.94645833506763211 ) ) ;
#20543 = ORIENTED_EDGE ( 'NONE', *, *, #50845, .T. ) ;
#20544 = CARTESIAN_POINT ( 'NONE',  ( -0.9774260708577104939, -118.8621782758236378, 2.500000000000000000 ) ) ;
#20545 = ORIENTED_EDGE ( 'NONE', *, *, #5311, .F. ) ;
#20546 = CARTESIAN_POINT ( 'NONE',  ( -93.67500000000003979, 92.29496732002878900, 82.24770833506762813 ) ) ;
#20547 = EDGE_CURVE ( 'NONE', #4586, #22671, #14906, .T. ) ;
#20548 = ORIENTED_EDGE ( 'NONE', *, *, #65995, .T. ) ;
#20549 = CARTESIAN_POINT ( 'NONE',  ( 92.69370383062498320, 88.66845928578037217, 87.31447916753381833 ) ) ;
#20550 = DIRECTION ( 'NONE',  ( -1.000000000000000000, 0.000000000000000000, 0.000000000000000000 ) ) ;
#20551 = DIRECTION ( 'NONE',  ( -1.000000000000000000, -0.000000000000000000, 0.000000000000000000 ) ) ;
#20552 = LINE ( 'NONE', #43506, #30176 ) ;
#20553 = DIRECTION ( 'NONE',  ( -0.000000000000000000, -0.000000000000000000, 1.000000000000000000 ) ) ;
#20554 = LINE ( 'NONE', #60783, #42103 ) ;
#20555 = ORIENTED_EDGE ( 'NONE', *, *, #52004, .T. ) ;
#20556 = DIRECTION ( 'NONE',  ( 0.000000000000000000, 0.3826834323650907810, -0.9238795325112864054 ) ) ;
#20557 = FACE_OUTER_BOUND ( 'NONE', #10144, .T. ) ;
#20558 = VERTEX_POINT ( 'NONE', #2921 ) ;
#20559 = EDGE_LOOP ( 'NONE', ( #36156, #6187, #12609, #61203 ) ) ;
#20560 = CYLINDRICAL_SURFACE ( 'NONE', #13343, 77.49899999999999523 ) ;
#20561 = EDGE_CURVE ( 'NONE', #44780, #11375, #48220, .T. ) ;
#20562 = EDGE_CURVE ( 'NONE', #66356, #17407, #59691, .T. ) ;
#20563 = LINE ( 'NONE', #54042, #32379 ) ;
#20564 = LINE ( 'NONE', #38600, #70130 ) ;
#20565 = CARTESIAN_POINT ( 'NONE',  ( -92.69370383062498320, -211.3315407142195852, 84.35114583420049428 ) ) ;
#20566 = ORIENTED_EDGE ( 'NONE', *, *, #68576, .T. ) ;
#20567 = DIRECTION ( 'NONE',  ( 0.000000000000000000, 0.000000000000000000, 1.000000000000000000 ) ) ;
#20568 = ORIENTED_EDGE ( 'NONE', *, *, #3990, .T. ) ;
#20569 = AXIS2_PLACEMENT_3D ( 'NONE', #35920, #18992, #29530 ) ;
#20570 = AXIS2_PLACEMENT_3D ( 'NONE', #49399, #47921, #72325 ) ;
#20571 = LINE ( 'NONE', #14177, #7813 ) ;
#20572 = CIRCLE ( 'NONE', #21747, 16.00000000000000355 ) ;
#20573 = EDGE_CURVE ( 'NONE', #32327, #3906, #61153, .T. ) ;
#20574 = EDGE_CURVE ( 'NONE', #6723, #5282, #44640, .T. ) ;
#20575 = DIRECTION ( 'NONE',  ( 0.000000000000000000, 0.000000000000000000, 1.000000000000000000 ) ) ;
#20576 = AXIS2_PLACEMENT_3D ( 'NONE', #71134, #24912, #8372 ) ;
#20577 = CARTESIAN_POINT ( 'NONE',  ( 0.000000000000000000, 0.000000000000000000, -40.00000000000000000 ) ) ;
#20578 = CARTESIAN_POINT ( 'NONE',  ( 92.69370383062498320, 90.00000000000002842, 78.84781250086714977 ) ) ;
#20579 = DIRECTION ( 'NONE',  ( -1.000000000000000000, -0.000000000000000000, -0.000000000000000000 ) ) ;
#20580 = CARTESIAN_POINT ( 'NONE',  ( 92.35001072511518316, 91.52998440550067016, 86.85145790673759336 ) ) ;
#20581 = CARTESIAN_POINT ( 'NONE',  ( 11.99999999999999822, -26.01480285779785362, -70.53064760720343429 ) ) ;
#20582 = DIRECTION ( 'NONE',  ( -1.000000000000000000, 0.000000000000000000, 0.000000000000000000 ) ) ;
#20583 = CARTESIAN_POINT ( 'NONE',  ( -11.99999999999999645, 0.000000000000000000, 0.000000000000000000 ) ) ;
#20584 = FACE_OUTER_BOUND ( 'NONE', #66943, .T. ) ;
#20585 = AXIS2_PLACEMENT_3D ( 'NONE', #59293, #350, #23241 ) ;
#20586 = CARTESIAN_POINT ( 'NONE',  ( -2.499999999999965361, 90.00000000000000000, -310.0000000000000000 ) ) ;
#20587 = LINE ( 'NONE', #66818, #67333 ) ;
#20588 = ORIENTED_EDGE ( 'NONE', *, *, #68412, .F. ) ;
#20589 = CARTESIAN_POINT ( 'NONE',  ( -92.69370383062505425, 88.66845928578038638, 83.55739583420047722 ) ) ;
#20590 = AXIS2_PLACEMENT_3D ( 'NONE', #48578, #19259, #42946 ) ;
#20591 = DIRECTION ( 'NONE',  ( 0.000000000000000000, 0.2079116908177641720, 0.9781476007338045786 ) ) ;
#20592 = AXIS2_PLACEMENT_3D ( 'NONE', #25019, #37050, #23920 ) ;
#20593 = CARTESIAN_POINT ( 'NONE',  ( 4.999999999999999112, 3.925862922256769583, -41.81611651403857621 ) ) ;
#20594 = VERTEX_POINT ( 'NONE', #20915 ) ;
#20595 = AXIS2_PLACEMENT_3D ( 'NONE', #60905, #61649, #54887 ) ;
#20596 = LINE ( 'NONE', #43547, #18638 ) ;
#20597 = CARTESIAN_POINT ( 'NONE',  ( -90.00000000000002842, 85.00000000000002842, -80.00000000000000000 ) ) ;
#20598 = CARTESIAN_POINT ( 'NONE',  ( 96.74471819418077700, 88.31889241252949319, 74.86350982016037392 ) ) ;
#20599 = ADVANCED_FACE ( 'NONE', ( #37106 ), #31448, .F. ) ;
#20600 = CARTESIAN_POINT ( 'NONE',  ( 10.00000000000000000, 0.000000000000000000, 0.000000000000000000 ) ) ;
#20601 = CARTESIAN_POINT ( 'NONE',  ( 95.00000000000000000, -212.6630814284392557, 79.16531250086715943 ) ) ;
#20602 = VERTEX_POINT ( 'NONE', #26553 ) ;
#20603 = ADVANCED_FACE ( 'NONE', ( #49485 ), #9638, .T. ) ;
#20604 = ORIENTED_EDGE ( 'NONE', *, *, #28534, .F. ) ;
#20605 = EDGE_CURVE ( 'NONE', #73443, #73391, #20552, .T. ) ;
#20606 = DIRECTION ( 'NONE',  ( 0.8660254037844382635, -0.5000000000000006661, 0.000000000000000000 ) ) ;
#20607 = DIRECTION ( 'NONE',  ( -1.000000000000000000, -0.000000000000000000, -0.000000000000000000 ) ) ;
#20608 = CARTESIAN_POINT ( 'NONE',  ( 11.99999999999999822, -28.89263327155693517, -71.91182617369219088 ) ) ;
#20609 = FILL_AREA_STYLE ('',( #55561 ) ) ;
#20610 = CARTESIAN_POINT ( 'NONE',  ( 97.30629616937498838, -209.9999999999999716, 76.78406250086715090 ) ) ;
#20611 = EDGE_CURVE ( 'NONE', #42748, #50561, #59667, .T. ) ;
#20612 = CIRCLE ( 'NONE', #62673, 31.99999999999999289 ) ;
#20613 = ORIENTED_EDGE ( 'NONE', *, *, #8430, .F. ) ;
#20614 = DIRECTION ( 'NONE',  ( -1.000000000000000000, -0.000000000000000000, 0.000000000000000000 ) ) ;
#20615 = ORIENTED_EDGE ( 'NONE', *, *, #57542, .T. ) ;
#20616 = ORIENTED_EDGE ( 'NONE', *, *, #54166, .T. ) ;
#20617 = PLANE ( 'NONE',  #44181 ) ;
#20618 = VECTOR ( 'NONE', #59791, 1000.000000000000114 ) ;
#20619 = FACE_OUTER_BOUND ( 'NONE', #69649, .T. ) ;
#20620 = VERTEX_POINT ( 'NONE', #66781 ) ;
#20621 = PLANE ( 'NONE',  #35379 ) ;
#20622 = CARTESIAN_POINT ( 'NONE',  ( 92.35000000000002274, -211.5299782133524502, 79.97229166840095615 ) ) ;
#20623 = CARTESIAN_POINT ( 'NONE',  ( 97.64999999999997726, 91.52997821335252127, 86.56041666666665435 ) ) ;
#20624 = ORIENTED_EDGE ( 'NONE', *, *, #36515, .T. ) ;
#20625 = DIRECTION ( 'NONE',  ( 0.000000000000000000, 0.000000000000000000, 1.000000000000000000 ) ) ;
#20626 = CIRCLE ( 'NONE', #1465, 42.00000000000000000 ) ;
#20627 = CARTESIAN_POINT ( 'NONE',  ( -97.64999999954989107, -210.0000310946949753, 88.81037122969127040 ) ) ;
#20628 = ORIENTED_EDGE ( 'NONE', *, *, #46294, .T. ) ;
#20629 = CARTESIAN_POINT ( 'NONE',  ( 92.34999999999999432, 90.00000000000002842, 84.36437500173430237 ) ) ;
#20630 = AXIS2_PLACEMENT_3D ( 'NONE', #41528, #64466, #25714 ) ;
#20631 = CARTESIAN_POINT ( 'NONE',  ( -95.00000000000002842, 87.33691857156074434, 85.51531250086715374 ) ) ;
#20632 = EDGE_CURVE ( 'NONE', #29346, #6316, #51814, .T. ) ;
#20633 = CARTESIAN_POINT ( 'NONE',  ( 93.84685191531248449, 88.00268892867053694, 80.85864583420047325 ) ) ;
#20634 = VERTEX_POINT ( 'NONE', #43128 ) ;
#20635 = DIRECTION ( 'NONE',  ( 1.000000000000000000, 0.000000000000000000, 0.000000000000000000 ) ) ;
#20636 = ORIENTED_EDGE ( 'NONE', *, *, #18471, .F. ) ;
#20637 = DIRECTION ( 'NONE',  ( -1.000000000000000000, 0.000000000000000000, 0.000000000000000000 ) ) ;
#20638 = AXIS2_PLACEMENT_3D ( 'NONE', #21852, #4583, #16211 ) ;
#20639 = ORIENTED_EDGE ( 'NONE', *, *, #53546, .F. ) ;
#20640 = EDGE_LOOP ( 'NONE', ( #61510, #69476, #67920, #56511 ) ) ;
#20641 = ORIENTED_EDGE ( 'NONE', *, *, #40402, .T. ) ;
#20642 = AXIS2_PLACEMENT_3D ( 'NONE', #5450, #51282, #33238 ) ;
#20643 = DIRECTION ( 'NONE',  ( -1.000000000000000000, -0.000000000000000000, 0.000000000000000000 ) ) ;
#20644 = EDGE_CURVE ( 'NONE', #13867, #10228, #31406, .T. ) ;
#20645 = VERTEX_POINT ( 'NONE', #38207 ) ;
#20646 = EDGE_CURVE ( 'NONE', #68795, #43361, #48012, .T. ) ;
#20647 = CARTESIAN_POINT ( 'NONE',  ( 10.00000000000000000, 0.000000000000000000, 0.000000000000000000 ) ) ;
#20648 = DIRECTION ( 'NONE',  ( -0.6862798483830533369, -0.7273375899149812085, 0.000000000000000000 ) ) ;
#20649 = VERTEX_POINT ( 'NONE', #65315 ) ;
#20650 = DIRECTION ( 'NONE',  ( -1.000000000000000000, 0.000000000000000000, 0.000000000000000000 ) ) ;
#20651 = CARTESIAN_POINT ( 'NONE',  ( -92.69370383062498320, -208.6684592857803011, 79.21822916753380639 ) ) ;
#20652 = ORIENTED_EDGE ( 'NONE', *, *, #61454, .T. ) ;
#20653 = EDGE_CURVE ( 'NONE', #45134, #23125, #54028, .T. ) ;
#20654 = DIRECTION ( 'NONE',  ( -1.000000000000000000, 0.000000000000000000, 0.000000000000000000 ) ) ;
#20655 = CARTESIAN_POINT ( 'NONE',  ( 0.000000000000000000, 31.46837873494978055, 68.27212725128286763 ) ) ;
#20656 = CARTESIAN_POINT ( 'NONE',  ( -92.35000000000003695, 90.00000000000004263, 90.00000000000000000 ) ) ;
#20657 = DIRECTION ( 'NONE',  ( 0.000000000000000000, 0.000000000000000000, 1.000000000000000000 ) ) ;
#20658 = CARTESIAN_POINT ( 'NONE',  ( 95.00000000000000000, -206.9400435732949575, 83.57062500173429953 ) ) ;
#20659 = DIRECTION ( 'NONE',  ( 1.000000000000000000, 0.000000000000000000, 0.000000000000000000 ) ) ;
#20660 = CARTESIAN_POINT ( 'NONE',  ( 97.64999999999999147, 90.00000000000002842, 77.61749999999999261 ) ) ;
#20661 = CARTESIAN_POINT ( 'NONE',  ( -94.99999999999997158, -209.9999999999999716, 90.00000000000000000 ) ) ;
#20662 = LINE ( 'NONE', #21020, #30170 ) ;
#20663 = LINE ( 'NONE', #3037, #24392 ) ;
#20664 = DIRECTION ( 'NONE',  ( 0.000000000000000000, -0.9945218953682730678, 0.1045284632676570929 ) ) ;
#20665 = FACE_OUTER_BOUND ( 'NONE', #70811, .T. ) ;
#20666 = CARTESIAN_POINT ( 'NONE',  ( -93.67500000000003979, 87.70503267997129626, 87.75104166840095843 ) ) ;
#20667 = CARTESIAN_POINT ( 'NONE',  ( 15.00000000000000000, 23.49999999999999645, -1.500000000000003997 ) ) ;
#20668 = CARTESIAN_POINT ( 'NONE',  ( 24.95699195200416654, -110.9640411295978595, -5.500000000000000000 ) ) ;
#20669 = VECTOR ( 'NONE', #16876, 1000.000000000000000 ) ;
#20670 = DIRECTION ( 'NONE',  ( 0.000000000000000000, -0.5877852522924708056, 0.8090169943749490056 ) ) ;
#20671 = DIRECTION ( 'NONE',  ( 0.000000000000000000, 0.000000000000000000, -1.000000000000000000 ) ) ;
#20672 = AXIS2_PLACEMENT_3D ( 'NONE', #23274, #40936, #34537 ) ;
#20673 = FACE_OUTER_BOUND ( 'NONE', #4348, .T. ) ;
#20674 = CARTESIAN_POINT ( 'NONE',  ( -97.64999999999996305, -209.9999999999999716, 88.09499999999999886 ) ) ;
#20675 = AXIS2_PLACEMENT_3D ( 'NONE', #28506, #16879, #5242 ) ;
#20676 = DIRECTION ( 'NONE',  ( -1.000000000000000000, 0.000000000000000000, -0.000000000000000000 ) ) ;
#20677 = AXIS2_PLACEMENT_3D ( 'NONE', #9643, #66430, #55510 ) ;
#20678 =( BOUNDED_CURVE ( )  B_SPLINE_CURVE ( 2, ( #73104, #59346, #67485, #55084, #60744, #54720, #15974 ),
 .UNSPECIFIED., .F., .F. ) 
 B_SPLINE_CURVE_WITH_KNOTS ( ( 3, 2, 2, 3 ),
 ( 0.8890265259402125864, 0.8960822236964605114, 0.9031379892373780915, 0.9101937466136234001 ),
 .UNSPECIFIED. ) 
 CURVE ( )  GEOMETRIC_REPRESENTATION_ITEM ( )  RATIONAL_B_SPLINE_CURVE ( ( 0.9999974258394913607, 0.8660266908770580807, 1.000000000000000000, 0.8660254037844387076, 1.000000000000000000, 0.8660254037844387076, 1.000000000000000000 ) ) 
 REPRESENTATION_ITEM ( '' )  );
#20679 = DIRECTION ( 'NONE',  ( -1.000000000000000000, 0.000000000000000000, 0.000000000000000000 ) ) ;
#20680 = LINE ( 'NONE', #38343, #32252 ) ;
#20681 = DIRECTION ( 'NONE',  ( 1.000000000000000000, 1.427937372958405461E-15, 7.962523111839130290E-16 ) ) ;
#20682 = CARTESIAN_POINT ( 'NONE',  ( -92.35000000000003695, 90.00000000000004263, 76.34749999999999659 ) ) ;
#20683 = VECTOR ( 'NONE', #5931, 999.9999999999998863 ) ;
#20684 = AXIS2_PLACEMENT_3D ( 'NONE', #67516, #28391, #56240 ) ;
#20685 = ORIENTED_EDGE ( 'NONE', *, *, #66868, .T. ) ;
#20686 = EDGE_CURVE ( 'NONE', #73599, #10620, #2566, .T. ) ;
#20687 = ORIENTED_EDGE ( 'NONE', *, *, #67763, .F. ) ;
#20689 = ADVANCED_FACE ( 'NONE', ( #55873 ), #5132, .F. ) ;
#20688 = DIRECTION ( 'NONE',  ( -0.000000000000000000, 0.9781476007338042455, 0.2079116908177664758 ) ) ;
#20690 = DIRECTION ( 'NONE',  ( 1.000000000000000000, -0.000000000000000000, -0.000000000000000000 ) ) ;
#20691 = ORIENTED_EDGE ( 'NONE', *, *, #23360, .T. ) ;
#20692 = CARTESIAN_POINT ( 'NONE',  ( 97.30629616937498838, -211.3315407142195852, 82.92239583420045790 ) ) ;
#20693 = CARTESIAN_POINT ( 'NONE',  ( 92.69370383062501162, -209.9999999999999716, 84.08656250086716000 ) ) ;
#20694 = ORIENTED_EDGE ( 'NONE', *, *, #44984, .T. ) ;
#20695 = CARTESIAN_POINT ( 'NONE',  ( 92.69370383062501162, -209.9999999999999716, 87.89656250086714806 ) ) ;
#20696 = EDGE_CURVE ( 'NONE', #40781, #67331, #49392, .T. ) ;
#20697 = EDGE_CURVE ( 'NONE', #23233, #48188, #51336, .T. ) ;
#20698 = VERTEX_POINT ( 'NONE', #61895 ) ;
#20699 = DIRECTION ( 'NONE',  ( -1.000000000000000000, 0.000000000000000000, -0.000000000000000000 ) ) ;
#20700 = ORIENTED_EDGE ( 'NONE', *, *, #51004, .F. ) ;
#20701 = CARTESIAN_POINT ( 'NONE',  ( -93.84685191531252713, 88.00268892867056536, 77.31322916753381946 ) ) ;
#20702 = ORIENTED_EDGE ( 'NONE', *, *, #60967, .T. ) ;
#20703 = ORIENTED_EDGE ( 'NONE', *, *, #66728, .F. ) ;
#20704 = CARTESIAN_POINT ( 'NONE',  ( -8.452893869119503023, -12.51233732111638375, 0.000000000000000000 ) ) ;
#20705 = VERTEX_POINT ( 'NONE', #45730 ) ;
#20706 = CARTESIAN_POINT ( 'NONE',  ( 11.99999999999999822, 8.830959090342393125, 74.65491531819122883 ) ) ;
#20707 = CARTESIAN_POINT ( 'NONE',  ( -0.4966694826856976608, -121.4153866697721611, -2.500000000000000000 ) ) ;
#20708 = ORIENTED_EDGE ( 'NONE', *, *, #16555, .F. ) ;
#20709 = CARTESIAN_POINT ( 'NONE',  ( -95.00000000000002842, 90.00000000000004263, 90.00000000000000000 ) ) ;
#20710 = ORIENTED_EDGE ( 'NONE', *, *, #57574, .T. ) ;
#20711 = CARTESIAN_POINT ( 'NONE',  ( 93.67500000000001137, -212.2949673200287179, 81.29520833506762756 ) ) ;
#20712 = ADVANCED_FACE ( 'NONE', ( #63028 ), #61519, .T. ) ;
#20713 = ORIENTED_EDGE ( 'NONE', *, *, #12207, .F. ) ;
#20714 = VERTEX_POINT ( 'NONE', #21267 ) ;
#20715 = EDGE_LOOP ( 'NONE', ( #59163, #5941, #43105, #22645 ) ) ;
#20716 = CARTESIAN_POINT ( 'NONE',  ( 92.69370383062501162, -209.9999999999999716, 77.57781250086713953 ) ) ;
#20717 = CARTESIAN_POINT ( 'NONE',  ( 92.34999999999999432, 90.00000000000002842, 89.44437500173430067 ) ) ;
#20718 = ORIENTED_EDGE ( 'NONE', *, *, #37002, .T. ) ;
#20719 = VECTOR ( 'NONE', #50928, 1000.000000000000000 ) ;
#20720 = EDGE_LOOP ( 'NONE', ( #56536, #41689, #23190, #24956 ) ) ;
#20721 = EDGE_LOOP ( 'NONE', ( #61146, #57412 ) ) ;
#20722 = DIRECTION ( 'NONE',  ( -1.000000000000000000, 0.000000000000000000, -0.000000000000000000 ) ) ;
#20723 = CARTESIAN_POINT ( 'NONE',  ( 0.000000000000000000, -62.20884554313985149, -46.21855187248698371 ) ) ;
#20724 = CARTESIAN_POINT ( 'NONE',  ( -92.69370383062502583, 91.33154071421968467, 78.10697916753383652 ) ) ;
#20725 = CIRCLE ( 'NONE', #20576, 77.49899999999999523 ) ;
#20726 = EDGE_CURVE ( 'NONE', #66942, #13012, #10376, .T. ) ;
#20727 = EDGE_CURVE ( 'NONE', #68066, #11414, #47041, .T. ) ;
#20728 = VERTEX_POINT ( 'NONE', #15655 ) ;
#20729 = ADVANCED_FACE ( 'NONE', ( #40068 ), #38587, .F. ) ;
#20730 = CARTESIAN_POINT ( 'NONE',  ( 97.30629616937498838, 91.33154071421968467, 76.04322916753380923 ) ) ;
#20731 = AXIS2_PLACEMENT_3D ( 'NONE', #16395, #22795, #11849 ) ;
#20732 = ORIENTED_EDGE ( 'NONE', *, *, #4015, .T. ) ;
#20733 = CARTESIAN_POINT ( 'NONE',  ( 11.99999999999999822, 12.93880638057315657, 76.41127070299278046 ) ) ;
#20734 = DIRECTION ( 'NONE',  ( -1.000000000000000000, 0.000000000000000000, 0.000000000000000000 ) ) ;
#20735 = DIRECTION ( 'NONE',  ( 0.000000000000000000, 0.000000000000000000, 1.000000000000000000 ) ) ;
#20736 = DIRECTION ( 'NONE',  ( 0.000000000000000000, 0.000000000000000000, -1.000000000000000000 ) ) ;
#20737 = DIRECTION ( 'NONE',  ( -1.000000000000000000, 0.000000000000000000, 0.000000000000000000 ) ) ;
#20738 = CARTESIAN_POINT ( 'NONE',  ( -92.69370383062498320, -211.3315407142195852, 80.38239583420049428 ) ) ;
#20739 = CARTESIAN_POINT ( 'NONE',  ( 10.00000000000000000, 33.79645857604513992, 16.45098606841138178 ) ) ;
#20740 = DIRECTION ( 'NONE',  ( 0.000000000000000000, -0.8910065241883626808, -0.4539904997395568520 ) ) ;
#20741 = VECTOR ( 'NONE', #41737, 1000.000000000000000 ) ;
#20742 = LINE ( 'NONE', #48213, #43262 ) ;
#20743 = VERTEX_POINT ( 'NONE', #73895 ) ;
#20744 = VECTOR ( 'NONE', #69212, 1000.000000000000000 ) ;
#20745 = EDGE_LOOP ( 'NONE', ( #10007, #21443, #17654, #4238 ) ) ;
#20746 = FACE_OUTER_BOUND ( 'NONE', #25820, .T. ) ;
#20747 = FACE_OUTER_BOUND ( 'NONE', #33669, .T. ) ;
#20748 = DIRECTION ( 'NONE',  ( -1.000000000000000000, -0.000000000000000000, 0.000000000000000000 ) ) ;
#20749 = CARTESIAN_POINT ( 'NONE',  ( -92.69370383062502583, 91.33154071421968467, 86.20322916753382003 ) ) ;
#20750 = LINE ( 'NONE', #60620, #17829 ) ;
#20751 = LINE ( 'NONE', #54601, #13375 ) ;
#20752 = ORIENTED_EDGE ( 'NONE', *, *, #25952, .T. ) ;
#20753 = LINE ( 'NONE', #10213, #13751 ) ;
#20754 = DIRECTION ( 'NONE',  ( -1.000000000000000000, 0.000000000000000000, 0.000000000000000000 ) ) ;
#20755 = DIRECTION ( 'NONE',  ( 0.000000000000000000, 0.000000000000000000, 1.000000000000000000 ) ) ;
#20756 = DIRECTION ( 'NONE',  ( 0.000000000000000000, 0.000000000000000000, 1.000000000000000000 ) ) ;
#20757 = FACE_OUTER_BOUND ( 'NONE', #44749, .T. ) ;
#20758 = CARTESIAN_POINT ( 'NONE',  ( 0.000000000000000000, 0.000000000000000000, 0.000000000000000000 ) ) ;
#20759 = CARTESIAN_POINT ( 'NONE',  ( -92.69370383062498320, -208.6684592857803011, 83.18697916753382060 ) ) ;
#20760 = CARTESIAN_POINT ( 'NONE',  ( 93.67499999999999716, 87.70503267997126784, 76.21520833506762926 ) ) ;
#20761 = ADVANCED_FACE ( 'NONE', ( #4021 ), #44609, .T. ) ;
#20762 = DIRECTION ( 'NONE',  ( 0.000000000000000000, 0.8910065241883656784, 0.4539904997395511344 ) ) ;
#20763 = EDGE_CURVE ( 'NONE', #12172, #45600, #68619, .T. ) ;
#20764 = CARTESIAN_POINT ( 'NONE',  ( -92.34999999999999432, -209.9999999999999716, 78.88750000000000284 ) ) ;
#20765 = CARTESIAN_POINT ( 'NONE',  ( 11.59999999999999964, -0.8299999999999999600, 0.000000000000000000 ) ) ;
#20766 = ORIENTED_EDGE ( 'NONE', *, *, #4589, .F. ) ;
#20767 = AXIS2_PLACEMENT_3D ( 'NONE', #62154, #3914, #4284 ) ;
#20768 = CARTESIAN_POINT ( 'NONE',  ( 0.000000000000000000, 0.000000000000000000, 0.000000000000000000 ) ) ;
#20769 = DIRECTION ( 'NONE',  ( 0.000000000000000000, 0.000000000000000000, 1.000000000000000000 ) ) ;
#20770 = LINE ( 'NONE', #32042, #35394 ) ;
#20771 = ADVANCED_FACE ( 'NONE', ( #32923 ), #45351, .T. ) ;
#20772 = VECTOR ( 'NONE', #49353, 1000.000000000000114 ) ;
#20773 = ADVANCED_FACE ( 'NONE', ( #72766 ), #5503, .T. ) ;
#20774 = LINE ( 'NONE', #45205, #765 ) ;
#20775 = ORIENTED_EDGE ( 'NONE', *, *, #28622, .F. ) ;
#20776 = CARTESIAN_POINT ( 'NONE',  ( 6.000000000000000000, 80.28980883073781172, -16.65972982744850128 ) ) ;
#20777 = CARTESIAN_POINT ( 'NONE',  ( 4.999999999999999112, -41.81611651403864727, 3.925862922256025289 ) ) ;
#20778 = ORIENTED_EDGE ( 'NONE', *, *, #25873, .F. ) ;
#20779 = AXIS2_PLACEMENT_3D ( 'NONE', #4737, #67497, #15622 ) ;
#20780 = LINE ( 'NONE', #65927, #28012 ) ;
#20781 = CARTESIAN_POINT ( 'NONE',  ( -99.99999999999997158, -204.9999999999999716, 90.00000000000000000 ) ) ;
#20782 = AXIS2_PLACEMENT_3D ( 'NONE', #43354, #66274, #59146 ) ;
#20783 = ORIENTED_EDGE ( 'NONE', *, *, #23113, .T. ) ;
#20784 = FACE_OUTER_BOUND ( 'NONE', #36547, .T. ) ;
#20785 = ADVANCED_FACE ( 'NONE', ( #28401 ), #22030, .T. ) ;
#20786 = VERTEX_POINT ( 'NONE', #44975 ) ;
#20787 = AXIS2_PLACEMENT_3D ( 'NONE', #4502, #74010, #67639 ) ;
#20788 = CARTESIAN_POINT ( 'NONE',  ( 0.000000000000000000, -10.41901085202107247, 40.68715046381925049 ) ) ;
#20789 = AXIS2_PLACEMENT_3D ( 'NONE', #73636, #22154, #45094 ) ;
#20790 = ORIENTED_EDGE ( 'NONE', *, *, #36098, .T. ) ;
#20791 = ORIENTED_EDGE ( 'NONE', *, *, #52201, .F. ) ;
#20792 = ORIENTED_EDGE ( 'NONE', *, *, #68531, .T. ) ;
#20793 = ORIENTED_EDGE ( 'NONE', *, *, #40594, .F. ) ;
#20794 = FACE_OUTER_BOUND ( 'NONE', #24136, .T. ) ;
#20795 = ORIENTED_EDGE ( 'NONE', *, *, #69620, .T. ) ;
#20796 = EDGE_CURVE ( 'NONE', #15499, #65637, #67901, .T. ) ;
#20797 = VERTEX_POINT ( 'NONE', #39331 ) ;
#20798 = CARTESIAN_POINT ( 'NONE',  ( 97.30629616937498838, 90.00000000000002842, 76.14906250086716000 ) ) ;
#20799 = FACE_OUTER_BOUND ( 'NONE', #28028, .T. ) ;
#20800 = ADVANCED_FACE ( 'NONE', ( #62268 ), #68652, .F. ) ;
#20801 = CYLINDRICAL_SURFACE ( 'NONE', #40507, 31.99999999999999289 ) ;
#20802 = ORIENTED_EDGE ( 'NONE', *, *, #53580, .F. ) ;
#20803 = ORIENTED_EDGE ( 'NONE', *, *, #50154, .T. ) ;
#20804 = ORIENTED_EDGE ( 'NONE', *, *, #49134, .F. ) ;
#20805 = CARTESIAN_POINT ( 'NONE',  ( 93.84685191531248449, 91.99731107132950569, 86.99697916753380866 ) ) ;
#20807 = ORIENTED_EDGE ( 'NONE', *, *, #21925, .F. ) ;
#20806 = EDGE_CURVE ( 'NONE', #45028, #62825, #23157, .T. ) ;
#20808 = CARTESIAN_POINT ( 'NONE',  ( 97.30629616937498838, -211.3315407142195852, 88.63739583420047552 ) ) ;
#20809 = DIRECTION ( 'NONE',  ( -1.908195823574487804E-17, -1.387778780781445676E-17, 1.000000000000000000 ) ) ;
#20810 = DIRECTION ( 'NONE',  ( 0.000000000000000000, 0.000000000000000000, 1.000000000000000000 ) ) ;
#20811 = DIRECTION ( 'NONE',  ( 1.000000000000000000, -5.236901059551556403E-15, -2.618450529775778123E-14 ) ) ;
#20812 = DIRECTION ( 'NONE',  ( 1.000000000000000000, 0.000000000000000000, 0.000000000000000000 ) ) ;
#20813 = CARTESIAN_POINT ( 'NONE',  ( -97.64999999999996305, -209.9999999999999716, 81.74500000000000455 ) ) ;
#20814 = CARTESIAN_POINT ( 'NONE',  ( -97.64999999999990621, -208.4700217866474361, 82.96208333333332519 ) ) ;
#20815 = DIRECTION ( 'NONE',  ( -1.000000000000000000, 0.000000000000000000, 0.000000000000000000 ) ) ;
#20816 = CARTESIAN_POINT ( 'NONE',  ( -92.34999999999999432, -211.5299782133524502, 75.10395833506764518 ) ) ;
#20817 = CARTESIAN_POINT ( 'NONE',  ( -97.30629616937501680, 91.33154071421968467, 89.11364583420049712 ) ) ;
#20818 = EDGE_CURVE ( 'NONE', #68659, #57100, #71002, .T. ) ;
#20819 = VERTEX_POINT ( 'NONE', #29506 ) ;
#20821 = CARTESIAN_POINT ( 'NONE',  ( -92.69370383062504004, 90.00000000000004263, 86.78531250086714977 ) ) ;
#20820 = CARTESIAN_POINT ( 'NONE',  ( 92.69370383062498320, 90.00000000000002842, 87.10281250086714522 ) ) ;
#20822 = ORIENTED_EDGE ( 'NONE', *, *, #12449, .T. ) ;
#20823 = CARTESIAN_POINT ( 'NONE',  ( 97.30629616937498838, 90.00000000000002842, 74.87906250086714977 ) ) ;
#20824 = DIRECTION ( 'NONE',  ( 1.000000000000000000, 0.000000000000000000, 0.000000000000000000 ) ) ;
#20825 = CARTESIAN_POINT ( 'NONE',  ( 12.13205353604972991, -140.1820037904669789, 5.500000000000000000 ) ) ;
#20826 = DIRECTION ( 'NONE',  ( 0.000000000000000000, -0.7071067811865389130, -0.7071067811865562325 ) ) ;
#20827 = DIRECTION ( 'NONE',  ( -0.000000000000000000, -1.000000000000000000, -1.445602896647339656E-16 ) ) ;
#20828 = ADVANCED_FACE ( 'NONE', ( #12227 ), #625, .F. ) ;
#20829 = DIRECTION ( 'NONE',  ( 1.000000000000000000, 0.000000000000000000, 0.000000000000000000 ) ) ;
#20830 = AXIS2_PLACEMENT_3D ( 'NONE', #54661, #43021, #53183 ) ;
#20831 = DIRECTION ( 'NONE',  ( -1.000000000000000000, 0.000000000000000000, 0.000000000000000000 ) ) ;
#20832 = PLANE ( 'NONE',  #31207 ) ;
#20833 = ORIENTED_EDGE ( 'NONE', *, *, #32761, .F. ) ;
#20834 = AXIS2_PLACEMENT_3D ( 'NONE', #67498, #43838, #68245 ) ;
#20835 = ORIENTED_EDGE ( 'NONE', *, *, #15091, .T. ) ;
#20836 = CARTESIAN_POINT ( 'NONE',  ( -95.00000000000002842, 86.94004357329504273, 81.90374999999998806 ) ) ;
#20837 = CARTESIAN_POINT ( 'NONE',  ( 10.00000000000000000, 63.18004540533092239, -44.88180994100307686 ) ) ;
#20838 = CARTESIAN_POINT ( 'NONE',  ( 93.67500000000001137, -212.2949673200287179, 75.58020833506763836 ) ) ;
#20839 = CARTESIAN_POINT ( 'NONE',  ( 100.0000000000000000, -214.9999999999999716, 90.00000000000000000 ) ) ;
#20840 = CARTESIAN_POINT ( 'NONE',  ( 2.600913415846943225E-12, -120.0000000000000000, -65.00000000000000000 ) ) ;
#20841 = CARTESIAN_POINT ( 'NONE',  ( 23.11608002360578240, -124.4885236261218182, -5.500000000000000000 ) ) ;
#20842 = CARTESIAN_POINT ( 'NONE',  ( -93.84685191531248449, -208.0026889286704943, 75.61989583420049144 ) ) ;
#20843 = AXIS2_PLACEMENT_3D ( 'NONE', #13907, #60182, #30462 ) ;
#20844 = ORIENTED_EDGE ( 'NONE', *, *, #21305, .T. ) ;
#20845 = CARTESIAN_POINT ( 'NONE',  ( -92.69370383062502583, 88.66845928578038638, 81.65239583420049030 ) ) ;
#20846 = CARTESIAN_POINT ( 'NONE',  ( -25.50183398199384754, -112.6408924756582053, 5.500000000000000000 ) ) ;
#20847 = CIRCLE ( 'NONE', #6475, 62.50000000000000000 ) ;
#20848 = AXIS2_PLACEMENT_3D ( 'NONE', #66985, #16230, #9473 ) ;
#20849 = CARTESIAN_POINT ( 'NONE',  ( 11.99999999999999822, 73.44644590900094272, -24.73286445877629802 ) ) ;
#20850 = LINE ( 'NONE', #49425, #23691 ) ;
#20851 = FACE_OUTER_BOUND ( 'NONE', #38153, .T. ) ;
#20852 = DIRECTION ( 'NONE',  ( 0.000000000000000000, 0.3090169943749410120, 0.9510565162951557516 ) ) ;
#20853 = DIRECTION ( 'NONE',  ( -1.000000000000000000, -0.000000000000000000, -0.000000000000000000 ) ) ;
#20854 = DIRECTION ( 'NONE',  ( -1.000000000000000000, 0.000000000000000000, 0.000000000000000000 ) ) ;
#20855 = CARTESIAN_POINT ( 'NONE',  ( 93.84685191531248449, 91.99731107132950569, 78.90072916753382515 ) ) ;
#20856 = AXIS2_PLACEMENT_3D ( 'NONE', #72851, #13233, #65492 ) ;
#20857 = CARTESIAN_POINT ( 'NONE',  ( -96.15314808468745866, -211.9973110713294489, 84.82739583420048746 ) ) ;
#20858 = CARTESIAN_POINT ( 'NONE',  ( -3.000000000000000000, -0.9646360437372163421, -23.52805723605591126 ) ) ;
#20859 = ORIENTED_EDGE ( 'NONE', *, *, #43161, .T. ) ;
#20860 = CARTESIAN_POINT ( 'NONE',  ( 97.65000000002596892, 89.99999999999992895, -64.99999999999992895 ) ) ;
#20861 = CARTESIAN_POINT ( 'NONE',  ( -92.34999999999999432, -211.5299782133524502, 76.29458333333333542 ) ) ;
#20862 = ADVANCED_FACE ( 'NONE', ( #47188 ), #7341, .T. ) ;
#20863 = LINE ( 'NONE', #4337, #17359 ) ;
#20864 = EDGE_CURVE ( 'NONE', #74311, #73251, #22001, .T. ) ;
#20865 = EDGE_CURVE ( 'NONE', #52132, #48511, #65273, .T. ) ;
#20866 = EDGE_CURVE ( 'NONE', #66496, #35486, #34414, .T. ) ;
#20867 = CARTESIAN_POINT ( 'NONE',  ( 92.69370383062501162, -211.3315407142195852, 83.34572916753380412 ) ) ;
#20868 = ORIENTED_EDGE ( 'NONE', *, *, #37964, .T. ) ;
#20869 = CIRCLE ( 'NONE', #41278, 31.99999999999998579 ) ;
#20870 = LINE ( 'NONE', #55828, #50265 ) ;
#20871 = ORIENTED_EDGE ( 'NONE', *, *, #18747, .F. ) ;
#20872 = DIRECTION ( 'NONE',  ( 1.000000000000000000, -0.000000000000000000, -0.000000000000000000 ) ) ;
#20873 = ORIENTED_EDGE ( 'NONE', *, *, #15217, .T. ) ;
#20874 = DIRECTION ( 'NONE',  ( -1.000000000000000000, 0.000000000000000000, 0.000000000000000000 ) ) ;
#20875 = AXIS2_PLACEMENT_3D ( 'NONE', #8318, #26704, #60577 ) ;
#20876 = EDGE_CURVE ( 'NONE', #51690, #26546, #52081, .T. ) ;
#20877 = EDGE_CURVE ( 'NONE', #61574, #24509, #35163, .T. ) ;
#20878 = CARTESIAN_POINT ( 'NONE',  ( 93.84685191531249870, -208.0026889286704943, 76.99572916753382401 ) ) ;
#20879 = CARTESIAN_POINT ( 'NONE',  ( 10.00000000000000000, -74.65491531819111515, -8.830959090343204920 ) ) ;
#20880 = DIRECTION ( 'NONE',  ( -1.000000000000000000, 0.000000000000000000, -0.000000000000000000 ) ) ;
#20881 = AXIS2_PLACEMENT_3D ( 'NONE', #70619, #47343, #30038 ) ;
#20882 =( BOUNDED_CURVE ( )  B_SPLINE_CURVE ( 2, ( #50597, #61522, #10006, #45732, #22032, #32925, #55875 ),
 .UNSPECIFIED., .F., .F. ) 
 B_SPLINE_CURVE_WITH_KNOTS ( ( 3, 2, 2, 3 ),
 ( 0.1250000000000002220, 0.1319444444444446418, 0.1388888888888890338, 0.1458333333333334536 ),
 .UNSPECIFIED. ) 
 CURVE ( )  GEOMETRIC_REPRESENTATION_ITEM ( )  RATIONAL_B_SPLINE_CURVE ( ( 0.9999999999999956701, 0.8660254037844430375, 1.000000000000000000, 0.8660254037844387076, 1.000000000000000000, 0.8660254037844365982, 1.000000000000002220 ) ) 
 REPRESENTATION_ITEM ( '' )  );
#20883 = CARTESIAN_POINT ( 'NONE',  ( 95.00000000000000000, -213.0599564267049857, 83.80875000000000341 ) ) ;
#20884 = CARTESIAN_POINT ( 'NONE',  ( 97.30629616937498838, 90.00000000000002842, 85.67406250086715147 ) ) ;
#20885 = AXIS2_PLACEMENT_3D ( 'NONE', #33240, #17085, #51284 ) ;
#20886 = CARTESIAN_POINT ( 'NONE',  ( 97.65000000000000568, 88.47002178664752137, 75.10395833506764518 ) ) ;
#20887 = CARTESIAN_POINT ( 'NONE',  ( 92.35000000000002274, -211.5299782133524502, 81.79791666666666572 ) ) ;
#20888 = EDGE_LOOP ( 'NONE', ( #41636, #44612, #10351, #67715 ) ) ;
#20889 = EDGE_LOOP ( 'NONE', ( #51992, #61101 ) ) ;
#20890 = ORIENTED_EDGE ( 'NONE', *, *, #46293, .T. ) ;
#20891 = AXIS2_PLACEMENT_3D ( 'NONE', #5808, #64420, #7276 ) ;
#20892 = ORIENTED_EDGE ( 'NONE', *, *, #29930, .T. ) ;
#20893 = CARTESIAN_POINT ( 'NONE',  ( 95.00000000000000000, -206.9400435732949575, 89.20624999999999716 ) ) ;
#20894 = EDGE_CURVE ( 'NONE', #33655, #55964, #33884, .T. ) ;
#20896 = ADVANCED_FACE ( 'NONE', ( #58842 ), #35529, .T. ) ;
#20895 = VECTOR ( 'NONE', #467, 1000.000000000000000 ) ;
#20897 = FILL_AREA_STYLE ('',( #14512 ) ) ;
#20898 = CARTESIAN_POINT ( 'NONE',  ( -92.69370383062502583, 91.33154071421968467, 85.72697916753381264 ) ) ;
#20899 = CARTESIAN_POINT ( 'NONE',  ( 2.499999999999982681, -79.99999999999998579, -310.0000000000000000 ) ) ;
#20900 = CYLINDRICAL_SURFACE ( 'NONE', #5455, 32.50000000000000000 ) ;
#20901 = CARTESIAN_POINT ( 'NONE',  ( -94.99999999999997158, -213.0599564267049857, 88.33312500173431658 ) ) ;
#20902 = CARTESIAN_POINT ( 'NONE',  ( 10.00000000000000000, -16.45098606841149902, 33.79645857604508308 ) ) ;
#20903 = EDGE_LOOP ( 'NONE', ( #58911, #46520, #34391, #53379 ) ) ;
#20904 = CARTESIAN_POINT ( 'NONE',  ( -97.64999999999996305, -209.9999999999999716, 87.53937500173429953 ) ) ;
#20905 = ORIENTED_EDGE ( 'NONE', *, *, #50739, .T. ) ;
#20906 = LINE ( 'NONE', #61142, #44650 ) ;
#20907 = ADVANCED_FACE ( 'NONE', ( #29880 ), #6600, .F. ) ;
#20908 = VERTEX_POINT ( 'NONE', #1372 ) ;
#20909 = CARTESIAN_POINT ( 'NONE',  ( -97.65000000000001990, 88.47002178664754979, 83.14729166840096752 ) ) ;
#20910 = ORIENTED_EDGE ( 'NONE', *, *, #70875, .T. ) ;
#20911 = CARTESIAN_POINT ( 'NONE',  ( 94.99999999999998579, 92.66308142843935514, 85.83281250086714920 ) ) ;
#20912 = CARTESIAN_POINT ( 'NONE',  ( 0.000000000000000000, -5.202137450156129717, -37.22597642581163768 ) ) ;
#20913 = LINE ( 'NONE', #14531, #21040 ) ;
#20914 = CIRCLE ( 'NONE', #65362, 37.49900000000000233 ) ;
#20915 = CARTESIAN_POINT ( 'NONE',  ( 10.00000000000000000, -6.736453364083817341, 36.88895765772630142 ) ) ;
#20916 = CARTESIAN_POINT ( 'NONE',  ( -100.0000000000000142, 95.00000000000002842, -90.00000000000000000 ) ) ;
#20917 = CARTESIAN_POINT ( 'NONE',  ( 10.00000000000000000, 0.000000000000000000, 0.000000000000000000 ) ) ;
#20918 = VERTEX_POINT ( 'NONE', #53196 ) ;
#20919 = DIRECTION ( 'NONE',  ( -1.000000000000000000, -0.000000000000000000, 0.000000000000000000 ) ) ;
#20920 = LINE ( 'NONE', #72048, #49138 ) ;
#20921 = ORIENTED_EDGE ( 'NONE', *, *, #22240, .T. ) ;
#20922 = EDGE_LOOP ( 'NONE', ( #23646, #11933, #71927, #64521 ) ) ;
#20923 = CARTESIAN_POINT ( 'NONE',  ( 11.99999999999999822, -41.76937507738745836, -62.50329211542482710 ) ) ;
#20924 = AXIS2_PLACEMENT_3D ( 'NONE', #35997, #17973, #64217 ) ;
#20925 = DIRECTION ( 'NONE',  ( 0.000000000000000000, 0.9876883405951371042, 0.1564344650402347547 ) ) ;
#20926 = DIRECTION ( 'NONE',  ( 0.000000000000000000, 0.000000000000000000, 1.000000000000000000 ) ) ;
#20927 = CARTESIAN_POINT ( 'NONE',  ( -96.15314808468745866, -211.9973110713294489, 86.09739583420049769 ) ) ;
#20928 = ORIENTED_EDGE ( 'NONE', *, *, #63241, .F. ) ;
#20929 = DIRECTION ( 'NONE',  ( 0.000000000000000000, 0.000000000000000000, -1.000000000000000000 ) ) ;
#20930 = EDGE_LOOP ( 'NONE', ( #46676, #58718, #11364, #6973 ) ) ;
#20931 = DIRECTION ( 'NONE',  ( -0.000000000000000000, -0.000000000000000000, 1.000000000000000000 ) ) ;
#20932 = AXIS2_PLACEMENT_3D ( 'NONE', #65018, #13497, #63912 ) ;
#20933 = FACE_OUTER_BOUND ( 'NONE', #36508, .T. ) ;
#20934 = CARTESIAN_POINT ( 'NONE',  ( 97.64999999999999147, -210.0000058630886031, 82.77687479895030265 ) ) ;
#20935 = CARTESIAN_POINT ( 'NONE',  ( 92.69370383062498320, 90.00000000000002842, 76.94281250086713442 ) ) ;
#20936 = DIRECTION ( 'NONE',  ( 0.000000000000000000, 1.000000000000000000, 3.469446951953614978E-15 ) ) ;
#20937 = CYLINDRICAL_SURFACE ( 'NONE', #25242, 77.49899999999999523 ) ;
#20938 = CARTESIAN_POINT ( 'NONE',  ( 10.00000000000000000, -49.70050353004933896, 59.46389618801946852 ) ) ;
#20939 = CARTESIAN_POINT ( 'NONE',  ( -32.50000000000000000, -120.0000000000000000, 2.500000000000000000 ) ) ;
#20940 = CYLINDRICAL_SURFACE ( 'NONE', #23195, 16.00000000000000000 ) ;
#20941 = CARTESIAN_POINT ( 'NONE',  ( -94.99999999999997158, -213.0599564267049857, 86.98374999999998636 ) ) ;
#20942 = VECTOR ( 'NONE', #17357, 1000.000000000000000 ) ;
#20943 = CARTESIAN_POINT ( 'NONE',  ( -92.93550210798944988, -208.9360650323627624, 74.79348190356850523 ) ) ;
#20944 = CARTESIAN_POINT ( 'NONE',  ( 11.99999999999999822, -74.65491531819124305, 8.830959090342128448 ) ) ;
#20945 = EDGE_LOOP ( 'NONE', ( #59905, #26063, #23758, #54024 ) ) ;
#20946 = AXIS2_PLACEMENT_3D ( 'NONE', #28715, #51656, #201 ) ;
#20947 = CARTESIAN_POINT ( 'NONE',  ( -95.00000000000002842, 87.33691857156074434, 82.18156250086715886 ) ) ;
#20948 = CARTESIAN_POINT ( 'NONE',  ( -10.00000000000000000, 0.000000000000000000, 0.000000000000000000 ) ) ;
#20949 = EDGE_CURVE ( 'NONE', #63525, #24130, #1734, .T. ) ;
#20950 = CIRCLE ( 'NONE', #42595, 2.500000000000000000 ) ;
#20951 = EDGE_CURVE ( 'NONE', #70455, #35173, #70958, .T. ) ;
#20952 = LINE ( 'NONE', #38248, #13822 ) ;
#20953 = AXIS2_PLACEMENT_3D ( 'NONE', #27434, #44752, #33443 ) ;
#20954 = ORIENTED_EDGE ( 'NONE', *, *, #44137, .T. ) ;
#20955 = EDGE_CURVE ( 'NONE', #6931, #21000, #19711, .T. ) ;
#20956 = DIRECTION ( 'NONE',  ( 1.000000000000000000, 0.000000000000000000, 0.000000000000000000 ) ) ;
#20957 = FACE_OUTER_BOUND ( 'NONE', #65990, .T. ) ;
#20958 = DIRECTION ( 'NONE',  ( 0.000000000000000000, 0.000000000000000000, 1.000000000000000000 ) ) ;
#20959 = AXIS2_PLACEMENT_3D ( 'NONE', #4476, #19973, #27372 ) ;
#20960 = ADVANCED_FACE ( 'NONE', ( #13700 ), #60333, .T. ) ;
#20961 = DIRECTION ( 'NONE',  ( -1.000000000000000000, 0.000000000000000000, 0.000000000000000000 ) ) ;
#20962 = CARTESIAN_POINT ( 'NONE',  ( 97.30629616937498838, -209.9999999999999716, 78.68906250086715204 ) ) ;
#20963 = ORIENTED_EDGE ( 'NONE', *, *, #60939, .T. ) ;
#20964 = ORIENTED_EDGE ( 'NONE', *, *, #21115, .T. ) ;
#20965 = EDGE_CURVE ( 'NONE', #10184, #16367, #70843, .T. ) ;
#20966 = ADVANCED_FACE ( 'NONE', ( #30616 ), #36636, .T. ) ;
#20967 = CYLINDRICAL_SURFACE ( 'NONE', #18863, 77.49899999999999523 ) ;
#20968 = DIRECTION ( 'NONE',  ( 0.000000000000000000, 0.000000000000000000, 1.000000000000000000 ) ) ;
#20969 = CARTESIAN_POINT ( 'NONE',  ( -3.000000000000000000, 18.84667830672579925, 18.68964196561269020 ) ) ;
#20970 = CARTESIAN_POINT ( 'NONE',  ( 15.00000000000000000, 0.000000000000000000, 0.000000000000000000 ) ) ;
#20971 = LINE ( 'NONE', #49174, #59718 ) ;
#20972 = CARTESIAN_POINT ( 'NONE',  ( 92.69370383062501162, -211.3315407142195852, 75.88447916753382572 ) ) ;
#20973 = ORIENTED_EDGE ( 'NONE', *, *, #19671, .F. ) ;
#20974 = CARTESIAN_POINT ( 'NONE',  ( -93.67499999999998295, -207.7050326799711968, 87.88333333333332575 ) ) ;
#20975 = VERTEX_POINT ( 'NONE', #13336 ) ;
#20976 = VERTEX_POINT ( 'NONE', #19342 ) ;
#20977 = DIRECTION ( 'NONE',  ( 0.000000000000000000, 0.6691306063588579045, -0.7431448254773945772 ) ) ;
#20978 = EDGE_CURVE ( 'NONE', #64618, #46085, #8812, .T. ) ;
#20979 = EDGE_CURVE ( 'NONE', #47807, #7440, #37012, .T. ) ;
#20980 = AXIS2_PLACEMENT_3D ( 'NONE', #23585, #23963, #69442 ) ;
#20981 = DIRECTION ( 'NONE',  ( 0.000000000000000000, -0.7604059656000228262, -0.6494480483301932061 ) ) ;
#20982 = ORIENTED_EDGE ( 'NONE', *, *, #17265, .F. ) ;
#20983 = CARTESIAN_POINT ( 'NONE',  ( 10.00000000000000000, 36.73666225445988687, -65.58780272294035285 ) ) ;
#20984 = CARTESIAN_POINT ( 'NONE',  ( 96.32499999999998863, -207.7050326799711968, 80.34270833506762699 ) ) ;
#20985 = CARTESIAN_POINT ( 'NONE',  ( 92.34999999999999432, 90.00000000000002842, 86.18999999999999773 ) ) ;
#20986 = ORIENTED_EDGE ( 'NONE', *, *, #51546, .T. ) ;
#20987 = FACE_OUTER_BOUND ( 'NONE', #61742, .T. ) ;
#20988 = CARTESIAN_POINT ( 'NONE',  ( -92.98549755320793508, -211.1324117838502161, 74.79348190356850523 ) ) ;
#20989 = ORIENTED_EDGE ( 'NONE', *, *, #15039, .F. ) ;
#20990 = DIRECTION ( 'NONE',  ( 1.000000000000000000, -0.000000000000000000, 0.000000000000000000 ) ) ;
#20991 = CARTESIAN_POINT ( 'NONE',  ( -93.84685191531254134, 91.99731107132950569, 85.14489583420048291 ) ) ;
#20992 = AXIS2_PLACEMENT_3D ( 'NONE', #16158, #66556, #61287 ) ;
#20993 = CARTESIAN_POINT ( 'NONE',  ( 93.84685191531248449, 88.00268892867053694, 83.39864583420047950 ) ) ;
#20994 = CIRCLE ( 'NONE', #35389, 82.00000000000000000 ) ;
#20995 = ORIENTED_EDGE ( 'NONE', *, *, #27237, .F. ) ;
#20996 = DIRECTION ( 'NONE',  ( -0.9435911131814398445, 0.3311129884571295534, 0.000000000000000000 ) ) ;
#20997 = ORIENTED_EDGE ( 'NONE', *, *, #58852, .T. ) ;
#20998 = CARTESIAN_POINT ( 'NONE',  ( 17.82587367876289974, -104.6869915565625320, -2.500000000000000000 ) ) ;
#20999 = AXIS2_PLACEMENT_3D ( 'NONE', #27522, #28257, #10230 ) ;
#21000 = VERTEX_POINT ( 'NONE', #59581 ) ;
#21001 = ORIENTED_EDGE ( 'NONE', *, *, #68235, .T. ) ;
#21003 = CARTESIAN_POINT ( 'NONE',  ( 93.67499999999998295, 92.29496732002878900, 79.09916666666666174 ) ) ;
#21002 = CIRCLE ( 'NONE', #6633, 12.75000000000265388 ) ;
#21004 = ORIENTED_EDGE ( 'NONE', *, *, #34235, .F. ) ;
#21005 = LINE ( 'NONE', #66873, #22747 ) ;
#21006 = CARTESIAN_POINT ( 'NONE',  ( 96.32499999999998863, 87.70503267997126784, 88.38604166840097776 ) ) ;
#21007 = ORIENTED_EDGE ( 'NONE', *, *, #40670, .T. ) ;
#21008 = DIRECTION ( 'NONE',  ( -1.000000000000000000, -0.000000000000000000, 0.000000000000000000 ) ) ;
#21009 = CARTESIAN_POINT ( 'NONE',  ( -93.84685191531248449, -208.0026889286704943, 78.00114583420048575 ) ) ;
#21010 = EDGE_LOOP ( 'NONE', ( #73136, #2178, #63344, #70888 ) ) ;
#21011 = CARTESIAN_POINT ( 'NONE',  ( 11.99999999999999822, -81.90746397400386059, -3.894527615418766242 ) ) ;
#21012 = CARTESIAN_POINT ( 'NONE',  ( 0.000000000000000000, 8.688484142253939169, 21.88630264137371029 ) ) ;
#21013 = CARTESIAN_POINT ( 'NONE',  ( -93.67499999999998295, -207.7050326799711968, 89.23270833506762756 ) ) ;
#21014 = DIRECTION ( 'NONE',  ( -1.000000000000000000, 0.000000000000000000, 0.000000000000000000 ) ) ;
#21015 = VECTOR ( 'NONE', #15950, 1000.000000000000000 ) ;
#21016 = DIRECTION ( 'NONE',  ( 0.000000000000000000, 0.000000000000000000, 1.000000000000000000 ) ) ;
#21017 = CARTESIAN_POINT ( 'NONE',  ( 96.15314808468748708, 88.00268892867053694, 86.67947916753381321 ) ) ;
#21018 = ADVANCED_FACE ( 'NONE', ( #71204 ), #20079, .F. ) ;
#21019 = DIRECTION ( 'NONE',  ( 0.000000000000000000, 0.2334453638558990629, 0.9723699203976782224 ) ) ;
#21020 = CARTESIAN_POINT ( 'NONE',  ( 17.50000000000000355, 2.143131898507868643E-15, 20.00000000000000000 ) ) ;
#21021 =( BOUNDED_CURVE ( )  B_SPLINE_CURVE ( 2, ( #22716, #17068, #55804, #5063, #16320, #67452, #27962 ),
 .UNSPECIFIED., .F., .F. ) 
 B_SPLINE_CURVE_WITH_KNOTS ( ( 3, 2, 2, 3 ),
 ( 0.6666666666666667407, 0.6736111111111112715, 0.6805555555555555802, 0.6875000000000000000 ),
 .UNSPECIFIED. ) 
 CURVE ( )  GEOMETRIC_REPRESENTATION_ITEM ( )  RATIONAL_B_SPLINE_CURVE ( ( 0.9999999999999978906, 0.8660254037844408170, 1.000000000000000000, 0.8660254037844387076, 1.000000000000000000, 0.8660254037844387076, 1.000000000000000000 ) ) 
 REPRESENTATION_ITEM ( '' )  );
#21022 = CARTESIAN_POINT ( 'NONE',  ( -97.65000000000001990, 90.00000000000004263, 88.80937500173430976 ) ) ;
#21023 = EDGE_CURVE ( 'NONE', #58797, #30533, #36271, .T. ) ;
#21024 = DIRECTION ( 'NONE',  ( 0.000000000000000000, -0.8910065241883722287, 0.4539904997395383113 ) ) ;
#21025 = LINE ( 'NONE', #27030, #66453 ) ;
#21026 = CARTESIAN_POINT ( 'NONE',  ( 94.99999999999998579, 86.94004357329502852, 77.45874999999999488 ) ) ;
#21027 = ADVANCED_FACE ( 'NONE', ( #31361 ), #60698, .T. ) ;
#21028 = CARTESIAN_POINT ( 'NONE',  ( 96.32499999999998863, -207.7050326799711968, 75.18333333333332291 ) ) ;
#21029 = LINE ( 'NONE', #31939, #44848 ) ;
#21030 = EDGE_CURVE ( 'NONE', #30236, #41798, #9177, .T. ) ;
#21031 = CARTESIAN_POINT ( 'NONE',  ( 94.99999999999998579, 90.00000000000002842, 90.00000000000000000 ) ) ;
#21032 = VECTOR ( 'NONE', #48651, 1000.000000000000000 ) ;
#21033 = DIRECTION ( 'NONE',  ( 0.000000000000000000, 0.000000000000000000, 1.000000000000000000 ) ) ;
#21034 = EDGE_CURVE ( 'NONE', #21161, #30764, #27253, .T. ) ;
#21035 = CARTESIAN_POINT ( 'NONE',  ( -94.99999999999997158, -213.0599564267049857, 84.44375000000000853 ) ) ;
#21036 = DIRECTION ( 'NONE',  ( -0.000000000000000000, -0.000000000000000000, 1.000000000000000000 ) ) ;
#21037 = CIRCLE ( 'NONE', #46286, 16.00000000000000000 ) ;
#21038 = EDGE_CURVE ( 'NONE', #73511, #39300, #55039, .T. ) ;
#21039 = CARTESIAN_POINT ( 'NONE',  ( 23.49955575015362186, 0.001194404164453295421, -49.00000000000061107 ) ) ;
#21040 = VECTOR ( 'NONE', #32182, 1000.000000000000000 ) ;
#21041 = CARTESIAN_POINT ( 'NONE',  ( -100.0000000000000142, 95.00000000000002842, 90.00000000000000000 ) ) ;
#21042 = DIRECTION ( 'NONE',  ( 1.000000000000000000, -0.000000000000000000, 0.000000000000000000 ) ) ;
#21043 = VECTOR ( 'NONE', #19473, 1000.000000000000000 ) ;
#21044 = EDGE_LOOP ( 'NONE', ( #6442, #33576, #55751, #47285 ) ) ;
#21045 = AXIS2_PLACEMENT_3D ( 'NONE', #5154, #38606, #67921 ) ;
#21046 = ORIENTED_EDGE ( 'NONE', *, *, #1925, .T. ) ;
#21047 = EDGE_CURVE ( 'NONE', #3438, #48900, #49402, .T. ) ;
#21048 = CARTESIAN_POINT ( 'NONE',  ( 0.000000000000000000, 81.50828551894240093, -8.966570791699803422 ) ) ;
#21049 = EDGE_CURVE ( 'NONE', #8256, #56438, #74181, .T. ) ;
#21050 = CARTESIAN_POINT ( 'NONE',  ( 6.377742925735834234, -145.7647898336708181, 5.500000000000000000 ) ) ;
#21051 = ORIENTED_EDGE ( 'NONE', *, *, #43208, .T. ) ;
#21052 =( REPRESENTATION_RELATIONSHIP ('NONE','NONE', #31117, #23018 ) REPRESENTATION_RELATIONSHIP_WITH_TRANSFORMATION ( #44404 )SHAPE_REPRESENTATION_RELATIONSHIP( ) );
#21053 = CARTESIAN_POINT ( 'NONE',  ( 96.15314808468750130, -211.9973110713294489, 82.23447916753380582 ) ) ;
#21054 = CARTESIAN_POINT ( 'NONE',  ( 95.00000000000000000, -207.3369185715606307, 85.19781250086714408 ) ) ;
#21055 = EDGE_LOOP ( 'NONE', ( #13443, #10931, #9721, #63458 ) ) ;
#21056 = VECTOR ( 'NONE', #30165, 1000.000000000000000 ) ;
#21057 = CARTESIAN_POINT ( 'NONE',  ( 95.00000000000000000, -212.6630814284392557, 84.88031250086714863 ) ) ;
#21058 = EDGE_LOOP ( 'NONE', ( #49823, #55739, #22135, #22123 ) ) ;
#21059 = DIRECTION ( 'NONE',  ( 0.000000000000000000, 0.000000000000000000, 1.000000000000000000 ) ) ;
#21060 = ORIENTED_EDGE ( 'NONE', *, *, #15076, .F. ) ;
#21061 = CARTESIAN_POINT ( 'NONE',  ( -97.30629616937501680, 90.00000000000004263, 76.46656250086715545 ) ) ;
#21062 = EDGE_LOOP ( 'NONE', ( #59086, #7464, #64654, #33012 ) ) ;
#21063 = EDGE_LOOP ( 'NONE', ( #23247, #53271, #47821, #30020 ) ) ;
#21064 = CARTESIAN_POINT ( 'NONE',  ( 10.00000000000000000, 0.000000000000000000, 0.000000000000000000 ) ) ;
#21065 = ORIENTED_EDGE ( 'NONE', *, *, #57804, .F. ) ;
#21066 = CYLINDRICAL_SURFACE ( 'NONE', #20875, 37.49900000000000233 ) ;
#21067 = LINE ( 'NONE', #39496, #64480 ) ;
#21068 = VERTEX_POINT ( 'NONE', #44134 ) ;
#21069 = CARTESIAN_POINT ( 'NONE',  ( -2.500000000000000000, 16.00000000000000000, -10.00000000000000178 ) ) ;
#21070 = ORIENTED_EDGE ( 'NONE', *, *, #10625, .T. ) ;
#21071 = DIRECTION ( 'NONE',  ( -1.000000000000000000, 0.000000000000000000, -0.000000000000000000 ) ) ;
#21072 = EDGE_LOOP ( 'NONE', ( #18748, #51518, #15989, #51428 ) ) ;
#21073 = VERTEX_POINT ( 'NONE', #27191 ) ;
#21074 = ORIENTED_EDGE ( 'NONE', *, *, #7381, .F. ) ;
#21075 = CARTESIAN_POINT ( 'NONE',  ( 93.84685191531251292, -211.9973110713294489, 75.14364583420046984 ) ) ;
#21076 = DIRECTION ( 'NONE',  ( -3.061616997868382648E-16, -1.000000000000000000, 0.000000000000000000 ) ) ;
#21077 = ORIENTED_EDGE ( 'NONE', *, *, #14785, .F. ) ;
#21078 = ORIENTED_EDGE ( 'NONE', *, *, #62869, .T. ) ;
#21079 = ORIENTED_EDGE ( 'NONE', *, *, #69762, .T. ) ;
#21080 = FACE_OUTER_BOUND ( 'NONE', #37360, .T. ) ;
#21081 = FACE_BOUND ( 'NONE', #70491, .T. ) ;
#21082 = CARTESIAN_POINT ( 'NONE',  ( -95.00000000000002842, 93.05995642670501411, 89.84125000000000227 ) ) ;
#21083 = EDGE_CURVE ( 'NONE', #10069, #10617, #32633, .T. ) ;
#21084 = EDGE_LOOP ( 'NONE', ( #59670, #40579, #38566, #50188 ) ) ;
#21085 = CARTESIAN_POINT ( 'NONE',  ( 97.30629616937498838, 90.00000000000002842, 77.26031250086714408 ) ) ;
#21086 = ORIENTED_EDGE ( 'NONE', *, *, #14243, .F. ) ;
#21087 = SURFACE_STYLE_USAGE ( .BOTH. , #4952 ) ;
#21088 = CARTESIAN_POINT ( 'NONE',  ( -97.30629616937497417, -211.3315407142195852, 89.06072916753379332 ) ) ;
#21089 = FACE_OUTER_BOUND ( 'NONE', #3886, .T. ) ;
#21090 = VECTOR ( 'NONE', #7697, 1000.000000000000000 ) ;
#21091 = CARTESIAN_POINT ( 'NONE',  ( 10.00000000000000000, 62.50884508063487033, -41.76106447765422303 ) ) ;
#21092 = CARTESIAN_POINT ( 'NONE',  ( 10.00000000000000000, 26.02418014898310261, 70.52718814184268581 ) ) ;
#21093 = CARTESIAN_POINT ( 'NONE',  ( -96.15314808468745866, -211.9973110713294489, 79.58864583420047722 ) ) ;
#21094 = DIRECTION ( 'NONE',  ( 0.000000000000000000, 0.000000000000000000, 1.000000000000000000 ) ) ;
#21095 = DIRECTION ( 'NONE',  ( 0.000000000000000000, 0.000000000000000000, -1.000000000000000000 ) ) ;
#21096 = CIRCLE ( 'NONE', #67922, 31.99999999999999289 ) ;
#21097 = CARTESIAN_POINT ( 'NONE',  ( 0.000000000000000000, 0.000000000000000000, 0.000000000000000000 ) ) ;
#21098 = EDGE_LOOP ( 'NONE', ( #55732, #12826, #2898, #10515 ) ) ;
#21099 = CIRCLE ( 'NONE', #71542, 31.99999999999998579 ) ;
#21100 = EDGE_LOOP ( 'NONE', ( #72123, #61727, #10533, #26807 ) ) ;
#21101 = DIRECTION ( 'NONE',  ( 0.000000000000000000, 0.3826834323650841752, 0.9238795325112891810 ) ) ;
#21102 = EDGE_CURVE ( 'NONE', #38008, #46917, #50509, .T. ) ;
#21103 = AXIS2_PLACEMENT_3D ( 'NONE', #51269, #62580, #17793 ) ;
#21104 = DIRECTION ( 'NONE',  ( 0.000000000000000000, 0.000000000000000000, 1.000000000000000000 ) ) ;
#21105 = EDGE_CURVE ( 'NONE', #46694, #67190, #42266, .T. ) ;
#21106 = CARTESIAN_POINT ( 'NONE',  ( 97.65000000000000568, 88.47002178664752137, 80.18395833506764347 ) ) ;
#21107 = CARTESIAN_POINT ( 'NONE',  ( -92.69370383062502583, 91.33154071421968467, 83.02822916753379445 ) ) ;
#21108 = DIRECTION ( 'NONE',  ( -1.000000000000000000, 0.000000000000000000, 0.000000000000000000 ) ) ;
#21109 = LINE ( 'NONE', #56466, #24182 ) ;
#21110 = CIRCLE ( 'NONE', #19927, 77.49900000000000944 ) ;
#21111 = AXIS2_PLACEMENT_3D ( 'NONE', #48933, #71860, #54952 ) ;
#21112 =( BOUNDED_CURVE ( )  B_SPLINE_CURVE ( 2, ( #38256, #1594, #61199, #19204, #53059, #9686, #66470, #32609, #60466 ),
 .UNSPECIFIED., .F., .F. ) 
 B_SPLINE_CURVE_WITH_KNOTS ( ( 3, 2, 2, 2, 3 ),
 ( 0.4021785743327794815, 0.4021786358302962827, 0.4092344013711782802, 0.4162901669120601666, 0.4233457466685775494 ),
 .UNSPECIFIED. ) 
 CURVE ( )  GEOMETRIC_REPRESENTATION_ITEM ( )  RATIONAL_B_SPLINE_CURVE ( ( 0.9999976645955351851, 0.9999988322875899005, 1.000000000000000000, 0.8660254037844387076, 1.000000000000000000, 0.8660254037844387076, 1.000000000000000000, 0.8660289314505841274, 0.9999929448534821130 ) ) 
 REPRESENTATION_ITEM ( '' )  );
#21113 = ORIENTED_EDGE ( 'NONE', *, *, #29756, .T. ) ;
#21114 = FACE_OUTER_BOUND ( 'NONE', #27095, .T. ) ;
#21115 = EDGE_CURVE ( 'NONE', #45794, #52450, #68115, .T. ) ;
#21116 = EDGE_CURVE ( 'NONE', #2269, #39726, #16304, .T. ) ;
#21117 = CARTESIAN_POINT ( 'NONE',  ( 5.000000000000000000, -59.75363087400113926, 56.15606465354937882 ) ) ;
#21118 = CARTESIAN_POINT ( 'NONE',  ( 15.00000000000000000, 8.688484142253932063, -21.88630264137371029 ) ) ;
#21119 = DIRECTION ( 'NONE',  ( 0.000000000000000000, 0.7071067811865439090, 0.7071067811865512365 ) ) ;
#21120 = AXIS2_PLACEMENT_3D ( 'NONE', #36491, #41049, #63978 ) ;
#21121 = CARTESIAN_POINT ( 'NONE',  ( 96.32499999999998863, -207.7050326799711968, 88.59770833506763665 ) ) ;
#21122 = CARTESIAN_POINT ( 'NONE',  ( -92.69370383062498320, -208.6684592857803011, 81.91697916753381037 ) ) ;
#21123 = DIRECTION ( 'NONE',  ( 0.000000000000000000, 0.000000000000000000, 1.000000000000000000 ) ) ;
#21124 = VERTEX_POINT ( 'NONE', #3935 ) ;
#21125 = ADVANCED_FACE ( 'NONE', ( #28313 ), #21562, .T. ) ;
#21126 = DIRECTION ( 'NONE',  ( 1.000000000000000000, 0.000000000000000000, -0.000000000000000000 ) ) ;
#21127 = CARTESIAN_POINT ( 'NONE',  ( 10.00000000000000000, -71.21200624218823805, 40.65526001592589722 ) ) ;
#21128 = DIRECTION ( 'NONE',  ( 0.000000000000000000, 1.000000000000000000, 0.000000000000000000 ) ) ;
#21129 = ORIENTED_EDGE ( 'NONE', *, *, #68945, .T. ) ;
#21130 = DIRECTION ( 'NONE',  ( 1.000000000000000000, 0.000000000000000000, 0.000000000000000000 ) ) ;
#21131 = CARTESIAN_POINT ( 'NONE',  ( 0.000000000000000000, -77.32052557432837148, -5.256550761633681290 ) ) ;
#21132 = ADVANCED_BREP_SHAPE_REPRESENTATION ( '', ( #37419, #43395 ), #41132 ) ;
#21133 = FACE_OUTER_BOUND ( 'NONE', #1917, .T. ) ;
#21134 = CARTESIAN_POINT ( 'NONE',  ( 0.000000000000000000, -120.0000000000000000, 40.00000000000000711 ) ) ;
#21135 = ORIENTED_EDGE ( 'NONE', *, *, #35801, .F. ) ;
#21136 = EDGE_CURVE ( 'NONE', #21245, #6700, #32530, .T. ) ;
#21137 = DIRECTION ( 'NONE',  ( -1.000000000000000000, 0.000000000000000000, -0.000000000000000000 ) ) ;
#21138 = DIRECTION ( 'NONE',  ( 0.4796670183876304283, -0.8774505977381978905, 0.000000000000000000 ) ) ;
#21139 = EDGE_LOOP ( 'NONE', ( #10921, #10624, #46326, #65349 ) ) ;
#21140 = CARTESIAN_POINT ( 'NONE',  ( 0.000000000000000000, -20.55727247249726020, -16.78983467731313084 ) ) ;
#21141 = FACE_OUTER_BOUND ( 'NONE', #57607, .T. ) ;
#21142 = EDGE_CURVE ( 'NONE', #73989, #15264, #9841, .T. ) ;
#21143 = ORIENTED_EDGE ( 'NONE', *, *, #66112, .T. ) ;
#21144 = CYLINDRICAL_SURFACE ( 'NONE', #16223, 82.00000000000000000 ) ;
#21145 = ORIENTED_EDGE ( 'NONE', *, *, #46412, .F. ) ;
#21146 = DIRECTION ( 'NONE',  ( 0.000000000000000000, 0.000000000000000000, 1.000000000000000000 ) ) ;
#21147 = EDGE_LOOP ( 'NONE', ( #31466, #33559 ) ) ;
#21148 = AXIS2_PLACEMENT_3D ( 'NONE', #58739, #12122, #52343 ) ;
#21149 = EDGE_LOOP ( 'NONE', ( #3751, #36654, #62994, #66078 ) ) ;
#21150 = VECTOR ( 'NONE', #60174, 1000.000000000000114 ) ;
#21151 = VERTEX_POINT ( 'NONE', #2670 ) ;
#21152 = FACE_OUTER_BOUND ( 'NONE', #5581, .T. ) ;
#21153 = VERTEX_POINT ( 'NONE', #2298 ) ;
#21154 = PRODUCT_DEFINITION_SHAPE ( 'NONE', 'NONE',  #40301 ) ;
#21155 = AXIS2_PLACEMENT_3D ( 'NONE', #38043, #20385, #60256 ) ;
#21156 = AXIS2_PLACEMENT_3D ( 'NONE', #95, #34246, #56068 ) ;
#21157 = VERTEX_POINT ( 'NONE', #65424 ) ;
#21158 = CARTESIAN_POINT ( 'NONE',  ( 93.84685191531248449, 91.99731107132950569, 76.99572916753382401 ) ) ;
#21159 = CARTESIAN_POINT ( 'NONE',  ( 10.00000000000000000, -32.34446384429951138, -26.79245525562750530 ) ) ;
#21160 = PLANE ( 'NONE',  #947 ) ;
#21161 = VERTEX_POINT ( 'NONE', #41730 ) ;
#21162 = VERTEX_POINT ( 'NONE', #25550 ) ;
#21163 = ORIENTED_EDGE ( 'NONE', *, *, #8942, .T. ) ;
#21164 = CARTESIAN_POINT ( 'NONE',  ( 92.69370383062498320, 91.33154071421968467, 87.68489583420047495 ) ) ;
#21165 = VERTEX_POINT ( 'NONE', #12783 ) ;
#21166 = CARTESIAN_POINT ( 'NONE',  ( 97.30629616937498838, -211.3315407142195852, 84.82739583420045903 ) ) ;
#21167 = DIRECTION ( 'NONE',  ( -1.000000000000000000, 0.000000000000000000, -0.000000000000000000 ) ) ;
#21168 = DIRECTION ( 'NONE',  ( 0.000000000000000000, 0.000000000000000000, 1.000000000000000000 ) ) ;
#21169 = DIRECTION ( 'NONE',  ( -1.000000000000000000, 0.000000000000000000, 0.000000000000000000 ) ) ;
#21170 = LINE ( 'NONE', #67796, #67221 ) ;
#21171 = DIRECTION ( 'NONE',  ( 0.000000000000000000, 0.000000000000000000, 1.000000000000000000 ) ) ;
#21172 = CARTESIAN_POINT ( 'NONE',  ( -97.30629616937495996, -209.9999999999999716, 88.37281250086715545 ) ) ;
#21173 = CARTESIAN_POINT ( 'NONE',  ( -93.84685191531252713, 88.00268892867056536, 88.74322916753382628 ) ) ;
#21174 = VERTEX_POINT ( 'NONE', #8261 ) ;
#21176 = CARTESIAN_POINT ( 'NONE',  ( -97.30629616937501680, 88.66845928578038638, 89.06072916753379332 ) ) ;
#21175 = CARTESIAN_POINT ( 'NONE',  ( 97.30629616937498838, 88.66845928578037217, 88.00239583420047040 ) ) ;
#21177 = ORIENTED_EDGE ( 'NONE', *, *, #50081, .T. ) ;
#21178 = CARTESIAN_POINT ( 'NONE',  ( 92.35000000019411459, -210.0000198431783929, 84.36502760998391182 ) ) ;
#21179 = DIRECTION ( 'NONE',  ( -1.000000000000000000, 0.000000000000000000, -0.000000000000000000 ) ) ;
#21180 = CARTESIAN_POINT ( 'NONE',  ( 4.999999999999999112, 3.925862922256769583, -41.81611651403857621 ) ) ;
#21181 = CARTESIAN_POINT ( 'NONE',  ( 2.750000000000000000, 0.000000000000000000, 0.000000000000000000 ) ) ;
#21182 = CARTESIAN_POINT ( 'NONE',  ( -94.99999999999997158, -207.3369185715606307, 88.84906250086713442 ) ) ;
#21183 = CARTESIAN_POINT ( 'NONE',  ( -95.00000000000002842, 93.05995642670504253, 89.20624999999999716 ) ) ;
#21184 = ADVANCED_FACE ( 'NONE', ( #14268 ), #36458, .F. ) ;
#21185 = CARTESIAN_POINT ( 'NONE',  ( -3.000000000000000000, -19.89357724625003598, 12.59942793731059574 ) ) ;
#21186 = DIRECTION ( 'NONE',  ( -0.9918136447140100120, 0.1276937514489704939, 0.000000000000000000 ) ) ;
#21187 = VERTEX_POINT ( 'NONE', #7160 ) ;
#21188 = ORIENTED_EDGE ( 'NONE', *, *, #55423, .F. ) ;
#21189 = ADVANCED_FACE ( 'NONE', ( #53390 ), #1559, .F. ) ;
#21190 = CARTESIAN_POINT ( 'NONE',  ( -92.35000000000005116, 88.47002178664754979, 82.00958333333332462 ) ) ;
#21191 = ADVANCED_FACE ( 'NONE', ( #70288 ), #65056, .T. ) ;
#21192 = DIRECTION ( 'NONE',  ( 1.000000000000000000, 0.000000000000000000, 0.000000000000000000 ) ) ;
#21193 = DIRECTION ( 'NONE',  ( 0.000000000000000000, -0.3090169943749549453, 0.9510565162951511997 ) ) ;
#21194 = CARTESIAN_POINT ( 'NONE',  ( 11.99999999999999822, 0.000000000000000000, 0.000000000000000000 ) ) ;
#21195 = DIRECTION ( 'NONE',  ( 0.000000000000000000, 0.000000000000000000, 1.000000000000000000 ) ) ;
#21196 = DIRECTION ( 'NONE',  ( 0.000000000000000000, 1.000000000000000000, 3.469446951953614189E-15 ) ) ;
#21197 = CARTESIAN_POINT ( 'NONE',  ( 10.00000000000000000, 41.91543099594818500, 2.663952781846293139 ) ) ;
#21198 = AXIS2_PLACEMENT_3D ( 'NONE', #4957, #61345, #5327 ) ;
#21199 = ORIENTED_EDGE ( 'NONE', *, *, #9734, .T. ) ;
#21200 = CARTESIAN_POINT ( 'NONE',  ( -92.69370383062502583, 91.33154071421968467, 81.12322916753382174 ) ) ;
#21201 = AXIS2_PLACEMENT_3D ( 'NONE', #66219, #48175, #48902 ) ;
#21202 = EDGE_CURVE ( 'NONE', #24336, #14991, #30807, .T. ) ;
#21203 = DIRECTION ( 'NONE',  ( 1.000000000000000000, 0.000000000000000000, 0.000000000000000000 ) ) ;
#21204 = DIRECTION ( 'NONE',  ( 0.000000000000000000, 0.000000000000000000, 1.000000000000000000 ) ) ;
#21205 = AXIS2_PLACEMENT_3D ( 'NONE', #7470, #58231, #1134 ) ;
#21206 = FACE_OUTER_BOUND ( 'NONE', #9045, .T. ) ;
#21207 = FACE_OUTER_BOUND ( 'NONE', #970, .T. ) ;
#21208 = CARTESIAN_POINT ( 'NONE',  ( -96.32499999999996021, -207.7050326799711968, 87.35416666666665719 ) ) ;
#21209 = CIRCLE ( 'NONE', #22461, 37.49900000000000233 ) ;
#21210 = FACE_OUTER_BOUND ( 'NONE', #4373, .T. ) ;
#21211 = VECTOR ( 'NONE', #49961, 999.9999999999998863 ) ;
#21212 = EDGE_CURVE ( 'NONE', #39181, #68344, #24814, .T. ) ;
#21213 = EDGE_CURVE ( 'NONE', #60043, #9438, #30440, .T. ) ;
#21214 = AXIS2_PLACEMENT_3D ( 'NONE', #17267, #68030, #11253 ) ;
#21215 = CARTESIAN_POINT ( 'NONE',  ( 93.84685191531248449, 91.99731107132950569, 79.53572916753381605 ) ) ;
#21216 = CARTESIAN_POINT ( 'NONE',  ( -97.30629616937495996, -209.9999999999999716, 82.81656250086714977 ) ) ;
#21217 = FACE_BOUND ( 'NONE', #50736, .T. ) ;
#21218 = ORIENTED_EDGE ( 'NONE', *, *, #60127, .F. ) ;
#21219 = FACE_OUTER_BOUND ( 'NONE', #4278, .T. ) ;
#21220 = CARTESIAN_POINT ( 'NONE',  ( -92.34999999999999432, -211.5299782133524502, 79.46958333333333258 ) ) ;
#21221 = CARTESIAN_POINT ( 'NONE',  ( 92.34999999999995168, -208.4700217866474929, 78.51708333333334622 ) ) ;
#21222 = EDGE_CURVE ( 'NONE', #14321, #68714, #20626, .T. ) ;
#21223 = CIRCLE ( 'NONE', #50039, 31.99999999999999289 ) ;
#21224 = CARTESIAN_POINT ( 'NONE',  ( -92.69370383062505425, 88.66845928578038638, 79.27114583420048177 ) ) ;
#21225 = CARTESIAN_POINT ( 'NONE',  ( 96.15314808468748708, -208.0026889286704943, 84.98614583420047097 ) ) ;
#21226 = VERTEX_POINT ( 'NONE', #19168 ) ;
#21227 = CIRCLE ( 'NONE', #34445, 16.00000000000000000 ) ;
#21228 = ADVANCED_FACE ( 'NONE', ( #13530 ), #64672, .T. ) ;
#21229 = DIRECTION ( 'NONE',  ( 0.000000000000000000, 0.000000000000000000, 1.000000000000000000 ) ) ;
#21230 = VERTEX_POINT ( 'NONE', #71401 ) ;
#21231 = FACE_OUTER_BOUND ( 'NONE', #41668, .T. ) ;
#21232 = VERTEX_POINT ( 'NONE', #18791 ) ;
#21233 = DIRECTION ( 'NONE',  ( -0.000000000000000000, -0.000000000000000000, 1.000000000000000000 ) ) ;
#21234 = ORIENTED_EDGE ( 'NONE', *, *, #41073, .T. ) ;
#21235 = VERTEX_POINT ( 'NONE', #20275 ) ;
#21236 = CARTESIAN_POINT ( 'NONE',  ( 11.99999999999999822, -20.40083707022935400, 72.35432306680478121 ) ) ;
#21237 = CARTESIAN_POINT ( 'NONE',  ( 5.000000000000000000, -22.48208911017525580, 35.47612816024516036 ) ) ;
#21238 = CARTESIAN_POINT ( 'NONE',  ( 10.00000000000000000, 81.34940948281335693, 10.30890764327412690 ) ) ;
#21239 = CARTESIAN_POINT ( 'NONE',  ( 11.99999999999999822, 55.19960302592066625, 51.03279382321107249 ) ) ;
#21240 = CARTESIAN_POINT ( 'NONE',  ( 92.69370383062498320, 91.33154071421968467, 87.20864583420049598 ) ) ;
#21241 = CIRCLE ( 'NONE', #8063, 16.00000000000000000 ) ;
#21242 = CARTESIAN_POINT ( 'NONE',  ( 93.67499999999999716, 87.70503267997126784, 80.66020833506763665 ) ) ;
#21243 = CARTESIAN_POINT ( 'NONE',  ( 93.67500000000001137, -207.7050326799711968, 77.19416666666666060 ) ) ;
#21244 = AXIS2_PLACEMENT_3D ( 'NONE', #25171, #65034, #54473 ) ;
#21245 = VERTEX_POINT ( 'NONE', #25189 ) ;
#21246 = ORIENTED_EDGE ( 'NONE', *, *, #3032, .T. ) ;
#21247 = VERTEX_POINT ( 'NONE', #48117 ) ;
#21248 = ORIENTED_EDGE ( 'NONE', *, *, #60456, .F. ) ;
#21249 = FACE_OUTER_BOUND ( 'NONE', #19434, .T. ) ;
#21250 = LINE ( 'NONE', #66410, #13438 ) ;
#21251 = AXIS2_PLACEMENT_3D ( 'NONE', #15586, #55811, #60353 ) ;
#21252 = DIRECTION ( 'NONE',  ( -0.000000000000000000, -0.000000000000000000, 1.000000000000000000 ) ) ;
#21253 = CARTESIAN_POINT ( 'NONE',  ( -96.32499999999996021, -212.2949673200287179, 88.28020833506764120 ) ) ;
#21254 = CARTESIAN_POINT ( 'NONE',  ( 5.000000000000000000, 2.886751345948125991, -6.000000000000000000 ) ) ;
#21255 = VERTEX_POINT ( 'NONE', #19901 ) ;
#21256 = CARTESIAN_POINT ( 'NONE',  ( -97.64999999999994884, -208.4700217866474645, 86.21645833506764234 ) ) ;
#21257 = ORIENTED_EDGE ( 'NONE', *, *, #66224, .T. ) ;
#21258 = DIRECTION ( 'NONE',  ( 0.000000000000000000, 0.000000000000000000, -1.000000000000000000 ) ) ;
#21259 = AXIS2_PLACEMENT_3D ( 'NONE', #74115, #39927, #23008 ) ;
#21260 = EDGE_LOOP ( 'NONE', ( #27713, #58341, #598, #38242 ) ) ;
#21261 = CARTESIAN_POINT ( 'NONE',  ( -95.00000000000002842, 86.94004357329504273, 84.52312500173428589 ) ) ;
#21262 = VERTEX_POINT ( 'NONE', #31550 ) ;
#21263 = CARTESIAN_POINT ( 'NONE',  ( 94.99999999999998579, 92.66308142843935514, 82.02281250086714692 ) ) ;
#21264 = CARTESIAN_POINT ( 'NONE',  ( 0.000000000000000000, 37.01155633439059756, 6.555932627142549762 ) ) ;
#21265 = FACE_OUTER_BOUND ( 'NONE', #7581, .T. ) ;
#21266 = EDGE_CURVE ( 'NONE', #50963, #57918, #43462, .T. ) ;
#21267 = CARTESIAN_POINT ( 'NONE',  ( -89.99999999999998579, -204.9999999999999716, -80.00000000000000000 ) ) ;
#21268 = CARTESIAN_POINT ( 'NONE',  ( -3.759344165985237129, 0.000000000000000000, 0.000000000000000000 ) ) ;
#21269 = DIRECTION ( 'NONE',  ( 1.000000000000000000, 0.000000000000000000, 0.000000000000000000 ) ) ;
#21270 = ORIENTED_EDGE ( 'NONE', *, *, #14105, .F. ) ;
#21271 = DIRECTION ( 'NONE',  ( 1.000000000000000000, 0.000000000000000000, 0.000000000000000000 ) ) ;
#21272 = DIRECTION ( 'NONE',  ( -1.000000000000000000, 0.000000000000000000, 0.000000000000000000 ) ) ;
#21273 = ORIENTED_EDGE ( 'NONE', *, *, #65110, .F. ) ;
#21274 = ADVANCED_FACE ( 'NONE', ( #13157 ), #53027, .F. ) ;
#21275 = AXIS2_PLACEMENT_3D ( 'NONE', #68892, #57239, #11721 ) ;
#21276 = ORIENTED_EDGE ( 'NONE', *, *, #19489, .T. ) ;
#21277 = EDGE_CURVE ( 'NONE', #20050, #32222, #11029, .T. ) ;
#21278 = EDGE_CURVE ( 'NONE', #15874, #52714, #13887, .T. ) ;
#21279 = AXIS2_PLACEMENT_3D ( 'NONE', #30410, #53355, #24782 ) ;
#21280 = DIRECTION ( 'NONE',  ( 0.000000000000000000, 0.000000000000000000, 1.000000000000000000 ) ) ;
#21281 = DIRECTION ( 'NONE',  ( -1.000000000000000000, 0.000000000000000000, 0.000000000000000000 ) ) ;
#21282 = DIRECTION ( 'NONE',  ( 1.000000000000000000, 0.000000000000000000, 0.000000000000000000 ) ) ;
#21283 = ADVANCED_FACE ( 'NONE', ( #48848 ), #71767, .T. ) ;
#21284 = CARTESIAN_POINT ( 'NONE',  ( -93.84685191531248449, -208.0026889286704943, 83.23989583420049598 ) ) ;
#21285 = ORIENTED_EDGE ( 'NONE', *, *, #72815, .T. ) ;
#21286 = DIRECTION ( 'NONE',  ( -0.000000000000000000, -0.000000000000000000, 1.000000000000000000 ) ) ;
#21287 = ORIENTED_EDGE ( 'NONE', *, *, #14883, .F. ) ;
#21288 = EDGE_CURVE ( 'NONE', #8336, #39875, #37494, .T. ) ;
#21289 = CARTESIAN_POINT ( 'NONE',  ( 11.99999999999999822, 30.41916302227114599, 71.27951684758035356 ) ) ;
#21290 = CARTESIAN_POINT ( 'NONE',  ( -4.653126046682595884, -146.1313684676804314, 5.500000000000000000 ) ) ;
#21291 = CARTESIAN_POINT ( 'NONE',  ( 92.35000000000000853, -209.9999999999999716, 83.09437500173430635 ) ) ;
#21292 = CARTESIAN_POINT ( 'NONE',  ( 94.99999999999998579, 87.33691857156068750, 79.64156250086713840 ) ) ;
#21293 = CARTESIAN_POINT ( 'NONE',  ( 0.000000000000000000, 0.000000000000000000, 0.000000000000000000 ) ) ;
#21294 = DIRECTION ( 'NONE',  ( 0.000000000000000000, 0.000000000000000000, 1.000000000000000000 ) ) ;
#21295 = CARTESIAN_POINT ( 'NONE',  ( 0.000000000000000000, -46.53671651293907274, -59.03961581697448935 ) ) ;
#21296 = CARTESIAN_POINT ( 'NONE',  ( 94.32747394040349320, 92.31128197830615534, 74.85222950654856788 ) ) ;
#21297 = PLANE ( 'NONE',  #56843 ) ;
#21298 = DIRECTION ( 'NONE',  ( -1.000000000000000000, 0.000000000000000000, -0.000000000000000000 ) ) ;
#21299 = AXIS2_PLACEMENT_3D ( 'NONE', #60431, #61911, #60797 ) ;
#21300 = LINE ( 'NONE', #26950, #15601 ) ;
#21301 = EDGE_CURVE ( 'NONE', #50464, #26778, #3850, .T. ) ;
#21302 = DIRECTION ( 'NONE',  ( -0.9997280174009349762, 0.02332147558787671729, 0.000000000000000000 ) ) ;
#21303 = ORIENTED_EDGE ( 'NONE', *, *, #54341, .F. ) ;
#21304 = CARTESIAN_POINT ( 'NONE',  ( -97.30629616937501680, 88.66845928578038638, 82.71072916753378479 ) ) ;
#21305 = EDGE_CURVE ( 'NONE', #5518, #37933, #47098, .T. ) ;
#21306 = EDGE_CURVE ( 'NONE', #17551, #49698, #45873, .T. ) ;
#21307 = CYLINDRICAL_SURFACE ( 'NONE', #2364, 32.00000000000000000 ) ;
#21308 = VECTOR ( 'NONE', #8079, 1000.000000000000000 ) ;
#21309 = AXIS2_PLACEMENT_3D ( 'NONE', #39923, #16233, #28245 ) ;
#21310 = FACE_OUTER_BOUND ( 'NONE', #2407, .T. ) ;
#21311 = EDGE_CURVE ( 'NONE', #67063, #26486, #56710, .T. ) ;
#21312 = VERTEX_POINT ( 'NONE', #37949 ) ;
#21313 =( BOUNDED_CURVE ( )  B_SPLINE_CURVE ( 2, ( #31401, #21221, #38156, #43458, #38536, #61474, #27230 ),
 .UNSPECIFIED., .F., .F. ) 
 B_SPLINE_CURVE_WITH_KNOTS ( ( 3, 2, 2, 3 ),
 ( 0.7499999999999996669, 0.7569444444444439757, 0.7638888888888883955, 0.7708333333333328152 ),
 .UNSPECIFIED. ) 
 CURVE ( )  GEOMETRIC_REPRESENTATION_ITEM ( )  RATIONAL_B_SPLINE_CURVE ( ( 1.000000000000006439, 0.8660254037844322683, 1.000000000000000000, 0.8660254037844387076, 1.000000000000000000, 0.8660254037844493658, 0.9999999999999893419 ) ) 
 REPRESENTATION_ITEM ( '' )  );
#21314 = CARTESIAN_POINT ( 'NONE',  ( 94.99999999999998579, 90.00000000000002842, 90.00000000000000000 ) ) ;
#21315 = CARTESIAN_POINT ( 'NONE',  ( 0.000000000000000000, -68.27212725128298132, 31.46837873494953541 ) ) ;
#21316 = DIRECTION ( 'NONE',  ( -1.000000000000000000, 0.000000000000000000, 0.000000000000000000 ) ) ;
#21317 = CYLINDRICAL_SURFACE ( 'NONE', #52341, 2.649999999999985700 ) ;
#21318 = CARTESIAN_POINT ( 'NONE',  ( 93.84685191531249870, -208.0026889286704943, 80.17072916753382117 ) ) ;
#21319 = AXIS2_PLACEMENT_3D ( 'NONE', #19403, #65290, #13762 ) ;
#21320 = VECTOR ( 'NONE', #33332, 1000.000000000000000 ) ;
#21321 = EDGE_LOOP ( 'NONE', ( #59720, #31697, #65949, #44990 ) ) ;
#21322 = VERTEX_POINT ( 'NONE', #55977 ) ;
#21323 = VECTOR ( 'NONE', #36565, 1000.000000000000000 ) ;
#21324 = CARTESIAN_POINT ( 'NONE',  ( 11.99999999999999822, 73.95703589264006439, -23.16143007188350822 ) ) ;
#21325 = DIRECTION ( 'NONE',  ( -1.000000000000000000, 0.000000000000000000, 0.000000000000000000 ) ) ;
#21326 = AXIS2_PLACEMENT_3D ( 'NONE', #15498, #38436, #32775 ) ;
#21327 = CARTESIAN_POINT ( 'NONE',  ( -23.30023580412278505, -123.4057321492263384, 5.500000000000000000 ) ) ;
#21328 = DIRECTION ( 'NONE',  ( -1.000000000000000000, -0.000000000000000000, 0.000000000000000000 ) ) ;
#21329 = DIRECTION ( 'NONE',  ( 1.000000000000000000, -0.000000000000000000, -0.000000000000000000 ) ) ;
#21330 = CARTESIAN_POINT ( 'NONE',  ( 93.84685191531251292, -211.9973110713294489, 76.57239583420049200 ) ) ;
#21331 = ORIENTED_EDGE ( 'NONE', *, *, #19701, .F. ) ;
#21332 = DIRECTION ( 'NONE',  ( 0.000000000000000000, 0.9876883405951371042, 0.1564344650402347547 ) ) ;
#21333 = EDGE_LOOP ( 'NONE', ( #66923, #71925, #21618, #18096 ) ) ;
#21334 = ORIENTED_EDGE ( 'NONE', *, *, #2521, .T. ) ;
#21335 = CARTESIAN_POINT ( 'NONE',  ( 0.000000000000000000, -68.26794271651286294, 31.47745569255117104 ) ) ;
#21336 = CARTESIAN_POINT ( 'NONE',  ( -97.65000000000001990, 91.52997821335253548, 89.39145833506763950 ) ) ;
#21337 = ORIENTED_EDGE ( 'NONE', *, *, #1750, .F. ) ;
#21338 = SPHERICAL_SURFACE ( 'NONE', #50994, 5.315148208181397216 ) ;
#21339 = CARTESIAN_POINT ( 'NONE',  ( 95.00000000000000000, -206.9400435732949575, 79.76062500173429726 ) ) ;
#21340 = CARTESIAN_POINT ( 'NONE',  ( 96.32499999999998863, 87.70503267997126784, 82.59166666666665435 ) ) ;
#21341 = ORIENTED_EDGE ( 'NONE', *, *, #69362, .F. ) ;
#21342 = DIRECTION ( 'NONE',  ( -1.000000000000000000, 0.000000000000000000, 0.000000000000000000 ) ) ;
#21343 = ORIENTED_EDGE ( 'NONE', *, *, #20102, .F. ) ;
#21344 = CARTESIAN_POINT ( 'NONE',  ( -97.64996030324587650, -211.5300011322840987, 88.86229325377448163 ) ) ;
#21345 = EDGE_LOOP ( 'NONE', ( #68643, #4860, #3806, #238 ) ) ;
#21346 = DIRECTION ( 'NONE',  ( -1.000000000000000000, -0.000000000000000000, -0.000000000000000000 ) ) ;
#21347 = CARTESIAN_POINT ( 'NONE',  ( -92.69370383062505425, 91.33154071421968467, 85.72697916753381264 ) ) ;
#21348 = AXIS2_PLACEMENT_3D ( 'NONE', #64630, #64272, #30037 ) ;
#21349 = CARTESIAN_POINT ( 'NONE',  ( 93.84685191531248449, 91.99731107132950569, 78.10697916753380809 ) ) ;
#21350 = VERTEX_POINT ( 'NONE', #33035 ) ;
#21351 = AXIS2_PLACEMENT_3D ( 'NONE', #72798, #61182, #60810 ) ;
#21352 = CARTESIAN_POINT ( 'NONE',  ( 15.00000000000000000, 0.000000000000000000, 0.000000000000000000 ) ) ;
#21353 = DIRECTION ( 'NONE',  ( 0.000000000000000000, 0.000000000000000000, 1.000000000000000000 ) ) ;
#21354 = ORIENTED_EDGE ( 'NONE', *, *, #17233, .T. ) ;
#21355 = CARTESIAN_POINT ( 'NONE',  ( 0.000000000000000000, 76.66974797899835892, 11.30684508768368346 ) ) ;
#21356 = CARTESIAN_POINT ( 'NONE',  ( -97.30629616937497417, -211.3315407142195852, 79.53572916753380184 ) ) ;
#21357 = EDGE_LOOP ( 'NONE', ( #69985, #31134, #29014, #44287 ) ) ;
#21358 = AXIS2_PLACEMENT_3D ( 'NONE', #67446, #26846, #49771 ) ;
#21359 = ADVANCED_FACE ( 'NONE', ( #31925 ), #55232, .F. ) ;
#21360 = VERTEX_POINT ( 'NONE', #73257 ) ;
#21361 = AXIS2_PLACEMENT_3D ( 'NONE', #53132, #29812, #18540 ) ;
#21362 = CARTESIAN_POINT ( 'NONE',  ( 0.000000000000000000, -31.46837873494930093, -68.27212725128309501 ) ) ;
#21363 = ADVANCED_FACE ( 'NONE', ( #50332 ), #49584, .T. ) ;
#21364 = EDGE_CURVE ( 'NONE', #72371, #43291, #14640, .T. ) ;
#21365 = ORIENTED_EDGE ( 'NONE', *, *, #52973, .F. ) ;
#21366 = DIRECTION ( 'NONE',  ( 1.000000000000000000, -0.000000000000000000, -0.000000000000000000 ) ) ;
#21367 = CARTESIAN_POINT ( 'NONE',  ( 96.32499999999997442, 92.29496732002878900, 89.23270833506762756 ) ) ;
#21368 = EDGE_LOOP ( 'NONE', ( #54998, #67816, #39334, #74040 ) ) ;
#21369 = CARTESIAN_POINT ( 'NONE',  ( -94.99999999999997158, -212.6630814284392557, 78.37156250086714238 ) ) ;
#21370 = VERTEX_POINT ( 'NONE', #60521 ) ;
#21371 = CARTESIAN_POINT ( 'NONE',  ( 92.34999999999999432, 90.00000000000002842, 88.80937500173430976 ) ) ;
#21372 = FACE_OUTER_BOUND ( 'NONE', #47191, .T. ) ;
#21373 = DIRECTION ( 'NONE',  ( -0.000000000000000000, -0.000000000000000000, 1.000000000000000000 ) ) ;
#21374 = CARTESIAN_POINT ( 'NONE',  ( 5.000000000000000000, 16.65560815589464028, -38.55633173626993226 ) ) ;
#21375 = CARTESIAN_POINT ( 'NONE',  ( 100.0000000000260201, 95.00000000000001421, -75.00000000000000000 ) ) ;
#21376 = VECTOR ( 'NONE', #22198, 1000.000000000000114 ) ;
#21377 = CYLINDRICAL_SURFACE ( 'NONE', #73316, 12.50000000000000000 ) ;
#21379 = AXIS2_PLACEMENT_3D ( 'NONE', #53280, #58542, #23976 ) ;
#21378 = CARTESIAN_POINT ( 'NONE',  ( 92.69370383062498320, 90.00000000000002842, 88.37281250086715545 ) ) ;
#21380 = CARTESIAN_POINT ( 'NONE',  ( -10.90093335751250692, 0.000000000000000000, 0.000000000000000000 ) ) ;
#21381 = CARTESIAN_POINT ( 'NONE',  ( 92.35000000052950497, 90.00003365185392568, 81.18829462297337329 ) ) ;
#21382 = AXIS2_PLACEMENT_3D ( 'NONE', #21990, #44937, #39292 ) ;
#21383 = CARTESIAN_POINT ( 'NONE',  ( -97.65000000000001990, 90.00000000000004263, 86.82500000000000284 ) ) ;
#21384 = EDGE_CURVE ( 'NONE', #30754, #33832, #32681, .T. ) ;
#21385 = AXIS2_PLACEMENT_3D ( 'NONE', #73729, #33893, #56837 ) ;
#21386 = DIRECTION ( 'NONE',  ( 0.000000000000000000, 0.07845909572784529051, -0.9969173337331279638 ) ) ;
#21387 = EDGE_CURVE ( 'NONE', #48269, #31307, #72909, .T. ) ;
#21388 = DIRECTION ( 'NONE',  ( -1.000000000000000000, 0.000000000000000000, -0.000000000000000000 ) ) ;
#21389 = CARTESIAN_POINT ( 'NONE',  ( 0.000000000000000000, 0.000000000000000000, 0.000000000000000000 ) ) ;
#21390 = AXIS2_PLACEMENT_3D ( 'NONE', #31407, #71624, #52214 ) ;
#21391 = DIRECTION ( 'NONE',  ( -0.9227826878668540234, -0.3853207896976546531, 0.000000000000000000 ) ) ;
#21392 = CARTESIAN_POINT ( 'NONE',  ( 5.999999999999999112, -44.99326035066101781, 68.55367621811126355 ) ) ;
#21393 = DIRECTION ( 'NONE',  ( 0.000000000000000000, -0.4999999999999921174, 0.8660254037844431485 ) ) ;
#21394 = ADVANCED_FACE ( 'NONE', ( #9743 ), #26283, .F. ) ;
#21395 = EDGE_CURVE ( 'NONE', #46506, #73838, #11136, .T. ) ;
#21396 = LINE ( 'NONE', #26673, #10692 ) ;
#21397 = CARTESIAN_POINT ( 'NONE',  ( -92.34999999999999432, -211.5299782133524502, 85.81958333333331268 ) ) ;
#21398 = DIRECTION ( 'NONE',  ( -0.000000000000000000, -0.000000000000000000, 1.000000000000000000 ) ) ;
#21399 = VECTOR ( 'NONE', #59646, 1000.000000000000000 ) ;
#21400 = DIRECTION ( 'NONE',  ( -1.000000000000000000, -0.000000000000000000, 0.000000000000000000 ) ) ;
#21401 = CARTESIAN_POINT ( 'NONE',  ( -2.499999999999970690, 73.00000000000001421, -204.9999999999999716 ) ) ;
#21402 = DIRECTION ( 'NONE',  ( 0.5687579148473765889, -0.8225049752423776450, 0.000000000000000000 ) ) ;
#21403 = VECTOR ( 'NONE', #71139, 1000.000000000000000 ) ;
#21404 = AXIS2_PLACEMENT_3D ( 'NONE', #49054, #50803, #33897 ) ;
#21405 = DIRECTION ( 'NONE',  ( -0.000000000000000000, 0.000000000000000000, 1.000000000000000000 ) ) ;
#21406 = CARTESIAN_POINT ( 'NONE',  ( 92.69370383062501162, -211.3315407142195852, 89.21947916753381946 ) ) ;
#21407 = CIRCLE ( 'NONE', #49066, 3.299999999999983391 ) ;
#21408 = VECTOR ( 'NONE', #33715, 1000.000000000000000 ) ;
#21409 = ORIENTED_EDGE ( 'NONE', *, *, #58148, .F. ) ;
#21410 = ORIENTED_EDGE ( 'NONE', *, *, #72194, .T. ) ;
#21411 = CARTESIAN_POINT ( 'NONE',  ( 0.000000000000000000, -23.29833615347104825, -3.418703333116803744 ) ) ;
#21412 = CARTESIAN_POINT ( 'NONE',  ( 0.000000000000000000, -37.58145647212453611, -0.6853352020794456489 ) ) ;
#21413 = ORIENTED_EDGE ( 'NONE', *, *, #24894, .F. ) ;
#21414 = CARTESIAN_POINT ( 'NONE',  ( 96.15314808468750130, -211.9973110713294489, 79.05947916753380866 ) ) ;
#21415 = CARTESIAN_POINT ( 'NONE',  ( 97.30629616937498838, -211.3315407142195852, 86.25614583420048120 ) ) ;
#21416 = ORIENTED_EDGE ( 'NONE', *, *, #33009, .T. ) ;
#21417 = B_SPLINE_CURVE_WITH_KNOTS ( 'NONE', 3,
 ( #59702, #8182, #20943, #43898, #31849, #66816 ),
 .UNSPECIFIED., .F., .F.,
 ( 4, 2, 4 ),
 ( 0.000000000000000000, 0.0008269033587275169102, 0.001653806717455033820 ),
 .UNSPECIFIED. ) ;
#21418 = CARTESIAN_POINT ( 'NONE',  ( 92.69370383062501162, -211.3315407142195852, 87.94947916753382344 ) ) ;
#21419 = AXIS2_PLACEMENT_3D ( 'NONE', #11066, #22726, #44916 ) ;
#21420 = VERTEX_POINT ( 'NONE', #32289 ) ;
#21421 = DIRECTION ( 'NONE',  ( -1.000000000000000000, 0.000000000000000000, 0.000000000000000000 ) ) ;
#21422 = ORIENTED_EDGE ( 'NONE', *, *, #19082, .F. ) ;
#21423 = DIRECTION ( 'NONE',  ( -1.000000000000000000, 0.000000000000000000, -0.000000000000000000 ) ) ;
#21424 = CIRCLE ( 'NONE', #56290, 31.99999999999998934 ) ;
#21425 = ORIENTED_EDGE ( 'NONE', *, *, #44669, .T. ) ;
#21426 = DIRECTION ( 'NONE',  ( -1.000000000000000000, 0.000000000000000000, 0.000000000000000000 ) ) ;
#21427 = AXIS2_PLACEMENT_3D ( 'NONE', #61670, #33449, #4171 ) ;
#21428 = EDGE_LOOP ( 'NONE', ( #33909, #33256, #7433, #29850 ) ) ;
#21429 = DIRECTION ( 'NONE',  ( -1.000000000000000000, -0.000000000000000000, -0.000000000000000000 ) ) ;
#21430 = CARTESIAN_POINT ( 'NONE',  ( 96.32499999999998863, -212.2949673200287179, 89.02104166840096866 ) ) ;
#21431 = CIRCLE ( 'NONE', #63500, 77.49899999999999523 ) ;
#21432 = VERTEX_POINT ( 'NONE', #49953 ) ;
#21433 = DIRECTION ( 'NONE',  ( -1.000000000000000000, -0.000000000000000000, 0.000000000000000000 ) ) ;
#21434 = ORIENTED_EDGE ( 'NONE', *, *, #51945, .F. ) ;
#21435 = LINE ( 'NONE', #61684, #61225 ) ;
#21436 = ORIENTED_EDGE ( 'NONE', *, *, #54640, .F. ) ;
#21437 = EDGE_CURVE ( 'NONE', #16575, #60507, #72869, .T. ) ;
#21438 = ORIENTED_EDGE ( 'NONE', *, *, #36388, .T. ) ;
#21439 = EDGE_LOOP ( 'NONE', ( #12753, #17200, #66925, #57313 ) ) ;
#21440 = CARTESIAN_POINT ( 'NONE',  ( 92.69370383062501162, -208.6684592857803011, 76.25489583420049655 ) ) ;
#21441 = CONTEXT_DEPENDENT_SHAPE_REPRESENTATION ( #54666, #24870 ) ;
#21442 = LINE ( 'NONE', #73322, #49807 ) ;
#21443 = ORIENTED_EDGE ( 'NONE', *, *, #6703, .F. ) ;
#21444 = ORIENTED_EDGE ( 'NONE', *, *, #73940, .F. ) ;
#21445 = EDGE_CURVE ( 'NONE', #57978, #58272, #340, .T. ) ;
#21446 = ORIENTED_EDGE ( 'NONE', *, *, #64264, .F. ) ;
#21447 = PLANE ( 'NONE',  #20487 ) ;
#21448 =( BOUNDED_CURVE ( )  B_SPLINE_CURVE ( 2, ( #28438, #69050, #35194, #22068, #5168, #28067, #45011, #67938, #16427, #73932, #34084, #57029, #51010, #22443, #45387, #16804, #62690, #11161, #5540, #51371, #22822, #74308, #45760, #11517, #68685, #17170, #40104, #63058, #34450, #42327, #18633, #41572, #65260, #69772, #35562, #53974, #64513, #29539, #31022, #7369, #25018, #47222, #19741, #41211, #29911, #47959, #70877, #52477, #2134, #13733, #12991, #58492, #19376, #1767, #24654, #24295, #71236, #36670, #59616, #8099, #47585, #35928, #25400, #2518, #48327, #42690, #65628, #1402, #14099, #37049, #1028, #58877, #52863, #46861, #6628, #59242, #30287, #70489, #53231, #23919, #18274, #41954, #19002, #70132, #64149, #12624, #64892, #6988, #13366, #36299, #53595, #7734, #30649, #60363, #20857, #31393, #60730, #59995, #21594, #44549, #20500, #8480, #44170, #43073, #25762, #32127, #71985, #67468, #38531, #27224, #66005, #73092, #49431, #55818, #67093, #15960, #43451, #72710, #9208, #54345, #14851, #49060, #9586, #26125, #32506, #31762, #4331, #72360, #2869, #50158, #61467, #37798, #21216, #48691, #55072, #61090, #43813, #66371, #55446, #3603, #3965, #26864, #26503, #66731, #8848, #15594, #15220, #71615, #20112, #38151, #49790, #14479, #9947, #32869, #37431, #54705, #3234, #27612, #29083, #27976, #50914, #16334, #50541, #68216, #34740, #73836, #63325, #5814, #51659, #46390, #62592, #11071, #45670, #51281, #69317, #33994, #34361, #57682, #38900, #67842, #22348, #68595, #68960, #39276, #73464, #10320, #17082, #11787, #10693, #33237, #21973, #39647, #56577, #74215, #40017, #61837, #45297, #22732, #62206, #28721, #33620, #16711, #6185, #207, #23099, #52019, #568, #56189, #4710, #44922, #23461, #5076, #56941, #5449, #28345, #62971, #11427, #57304, #46030, #17445, #40374, #59526, #69688, #17809, #30564, #8012, #36578, #36211, #1679, #64802, #47862, #63697, #12538, #29819, #7644, #24930, #47500, #40758, #18910, #64426, #65171, #30929, #35473, #41855, #70785, #47137, #53509, #59153, #52774, #24568, #13279, #70401, #42240, #19289, #2044, #23828, #53877, #2423, #18185, #13645, #58404, #46769, #29446, #12170, #25312, #48242, #64063, #35108, #6544, #18549, #6904, #30199, #58038, #52389, #1317, #937, #41129, #24210, #70045, #41484, #12902, #35835, #58784, #7281, #53139, #20407, #27132 ),
 .UNSPECIFIED., .F., .F. ) 
 B_SPLINE_CURVE_WITH_KNOTS ( ( 3, 2, 2, 2, 2, 2, 2, 2, 2, 2, 2, 2, 2, 2, 2, 2, 2, 2, 2, 2, 2, 2, 2, 2, 2, 2, 2, 2, 2, 2, 2, 2, 2, 2, 2, 2, 2, 2, 2, 2, 2, 2, 2, 2, 2, 2, 2, 2, 2, 2, 2, 2, 2, 2, 2, 2, 2, 2, 2, 2, 2, 2, 2, 2, 2, 2, 2, 2, 2, 2, 2, 2, 2, 2, 2, 2, 2, 2, 2, 2, 2, 2, 2, 2, 2, 2, 2, 2, 2, 2, 2, 2, 2, 2, 2, 2, 2, 2, 2, 2, 2, 2, 2, 2, 2, 2, 2, 2, 2, 2, 2, 2, 2, 2, 2, 2, 2, 2, 2, 2, 2, 2, 2, 2, 2, 2, 2, 2, 2, 2, 2, 2, 2, 2, 2, 2, 2, 2, 2, 2, 2, 2, 2, 3 ),
 ( 0.000000000000000000, 0.007055764916269566256, 0.01411152983253913251, 0.02116729474880869877, 0.02822305966507826502, 0.03527882458134783822, 0.04233458949761739754, 0.04939035441388697073, 0.05644611933015653005, 0.06350188424642609630, 0.07055764916269567644, 0.07761341407896524269, 0.08466917899523479507, 0.09172494391150436133, 0.09878070882777394146, 0.1058364737440435077, 0.1128922386603130601, 0.1199480035765826264, 0.1270037684928521926, 0.1340595334091217727, 0.1411152983253913529, 0.1481710632416609053, 0.1552268281579304854, 0.1622825930742000100, 0.1693383579904695901, 0.1763941229067391703, 0.1834498878230087227, 0.1905056527392783028, 0.1975614176555478829, 0.2046171825718174353, 0.2116729474880870154, 0.2187287124043565678, 0.2257844773206261202, 0.2328402422368957003, 0.2398960071531652527, 0.2469517720694348328, 0.2540075369857043852, 0.2610633019019739653, 0.2681190668182435455, 0.2751748317345130701, 0.2822305966507827057, 0.2892863615670522304, 0.2963421264833218105, 0.3033978913995913906, 0.3104536563158609708, 0.3175094212321304954, 0.3245651861484000200, 0.3316209510646696557, 0.3386767159809391803, 0.3457324808972087604, 0.3527882458134783406, 0.3598440107297479207, 0.3668997756460174453, 0.3739555405622870810, 0.3810113054785566056, 0.3880670703948261302, 0.3951228353110957658, 0.4021786002273652905, 0.4092343651436348706, 0.4162901300599044507, 0.4233458949761740309, 0.4304016598924435555, 0.4374574248087131356, 0.4445131897249827158, 0.4515689546412522404, 0.4586247195575218205, 0.4656804844737914006, 0.4727362493900609808, 0.4797920143063305054, 0.4868477792226001410, 0.4939035441388696657, 0.5009593090551393013, 0.5080150739714087704, 0.5150708388876783506, 0.5221266038039479307, 0.5291823687202175108, 0.5362381336364870910, 0.5432938985527566711, 0.5503496634690261402, 0.5574054283852958314, 0.5644611933015654115, 0.5715169582178348806, 0.5785727231341044607, 0.5856284880503740409, 0.5926842529666436210, 0.5997400178829132011, 0.6067957827991827813, 0.6138515477154522504, 0.6209073126317219415, 0.6279630775479914107, 0.6350188424642609908, 0.6420746073805305709, 0.6491303722968000400, 0.6561861372130697312, 0.6632419021293393113, 0.6702976670456087804, 0.6773534319618783606, 0.6844091968781480517, 0.6914649617944175208, 0.6985207267106871010, 0.7055764916269566811, 0.7126322565432261502, 0.7196880214594958414, 0.7267437863757654215, 0.7337995512920348906, 0.7408553162083044707, 0.7479110811245741619, 0.7549668460408436310, 0.7620226109571132111, 0.7690783758733827913, 0.7761341407896522604, 0.7831899057059219516, 0.7902456706221915317, 0.7973014355384610008, 0.8043572004547305809, 0.8114129653710002721, 0.8184687302872697412, 0.8255244952035393213, 0.8325802601198089015, 0.8396360250360783706, 0.8466917899523480617, 0.8537475548686176419, 0.8608033197848871110, 0.8678590847011566911, 0.8749148496174262712, 0.8819706145336958514, 0.8890263794499654315, 0.8960821443662349006, 0.9031379092825044808, 0.9101936741987741719, 0.9172494391150436410, 0.9243052040313132212, 0.9313609689475828013, 0.9384167338638523814, 0.9454724987801219616, 0.9525282636963915417, 0.9595840286126610108, 0.9666397935289305909, 0.9736955584452002821, 0.9807513233614697512, 0.9878070882777393313, 0.9948628531940089115, 0.9999999123559573100, 1.000000000000000000 ),
 .UNSPECIFIED. ) 
 CURVE ( )  GEOMETRIC_REPRESENTATION_ITEM ( )  RATIONAL_B_SPLINE_CURVE ( ( 1.000000000000000000, 0.8660254037844387076, 1.000000000000000000, 0.8660254037844387076, 1.000000000000000000, 0.8660254037844387076, 1.000000000000000000, 0.8660254037844387076, 1.000000000000000000, 0.8660254037844387076, 1.000000000000000000, 0.8660254037844387076, 1.000000000000000000, 0.8660254037844387076, 1.000000000000000000, 0.8660254037844387076, 1.000000000000000000, 0.8660254037844387076, 1.000000000000000000, 0.8660254037844387076, 1.000000000000000000, 0.8660254037844387076, 1.000000000000000000, 0.8660254037844387076, 1.000000000000000000, 0.8660254037844387076, 1.000000000000000000, 0.8660254037844387076, 1.000000000000000000, 0.8660254037844387076, 1.000000000000000000, 0.8660254037844387076, 1.000000000000000000, 0.8660254037844387076, 1.000000000000000000, 0.8660254037844387076, 1.000000000000000000, 0.8660254037844387076, 1.000000000000000000, 0.8660254037844387076, 1.000000000000000000, 0.8660254037844387076, 1.000000000000000000, 0.8660254037844387076, 1.000000000000000000, 0.8660254037844387076, 1.000000000000000000, 0.8660254037844387076, 1.000000000000000000, 0.8660254037844387076, 1.000000000000000000, 0.8660254037844387076, 1.000000000000000000, 0.8660254037844387076, 1.000000000000000000, 0.8660254037844387076, 1.000000000000000000, 0.8660254037844387076, 1.000000000000000000, 0.8660254037844387076, 1.000000000000000000, 0.8660254037844387076, 1.000000000000000000, 0.8660254037844387076, 1.000000000000000000, 0.8660254037844387076, 1.000000000000000000, 0.8660254037844387076, 1.000000000000000000, 0.8660254037844387076, 1.000000000000000000, 0.8660254037844387076, 1.000000000000000000, 0.8660254037844387076, 1.000000000000000000, 0.8660254037844387076, 1.000000000000000000, 0.8660254037844387076, 1.000000000000000000, 0.8660254037844387076, 1.000000000000000000, 0.8660254037844387076, 1.000000000000000000, 0.8660254037844387076, 1.000000000000000000, 0.8660254037844387076, 1.000000000000000000, 0.8660254037844387076, 1.000000000000000000, 0.8660254037844387076, 1.000000000000000000, 0.8660254037844387076, 1.000000000000000000, 0.8660254037844387076, 1.000000000000000000, 0.8660254037844387076, 1.000000000000000000, 0.8660254037844387076, 1.000000000000000000, 0.8660254037844387076, 1.000000000000000000, 0.8660254037844387076, 1.000000000000000000, 0.8660254037844387076, 1.000000000000000000, 0.8660254037844387076, 1.000000000000000000, 0.8660254037844387076, 1.000000000000000000, 0.8660254037844387076, 1.000000000000000000, 0.8660254037844387076, 1.000000000000000000, 0.8660254037844387076, 1.000000000000000000, 0.8660254037844387076, 1.000000000000000000, 0.8660254037844387076, 1.000000000000000000, 0.8660254037844387076, 1.000000000000000000, 0.8660254037844387076, 1.000000000000000000, 0.8660254037844387076, 1.000000000000000000, 0.8660254037844387076, 1.000000000000000000, 0.8660254037844387076, 1.000000000000000000, 0.8660254037844387076, 1.000000000000000000, 0.8660254037844387076, 1.000000000000000000, 0.8660254037844387076, 1.000000000000000000, 0.8660254037844387076, 1.000000000000000000, 0.8660254037844387076, 1.000000000000000000, 0.8660254037844387076, 1.000000000000000000, 0.8660254037844387076, 1.000000000000000000, 0.8660254037844387076, 1.000000000000000000, 0.8660254037844387076, 1.000000000000000000, 0.8660254037844387076, 1.000000000000000000, 0.8660254037844387076, 1.000000000000000000, 0.8660254037844387076, 1.000000000000000000, 0.8660254037844387076, 1.000000000000000000, 0.8660254037844387076, 1.000000000000000000, 0.8660254037844387076, 1.000000000000000000, 0.8660254037844387076, 1.000000000000000000, 0.8660254037844387076, 1.000000000000000000, 0.8660254037844387076, 1.000000000000000000, 0.8660254037844387076, 1.000000000000000000, 0.8660254037844387076, 1.000000000000000000, 0.8660254037844387076, 1.000000000000000000, 0.8660254037844387076, 1.000000000000000000, 0.8660254037844387076, 1.000000000000000000, 0.8660254037844387076, 1.000000000000000000, 0.8660254037844387076, 1.000000000000000000, 0.8660254037844387076, 1.000000000000000000, 0.8660254037844387076, 1.000000000000000000, 0.8660254037844387076, 1.000000000000000000, 0.8660254037844387076, 1.000000000000000000, 0.8660254037844387076, 1.000000000000000000, 0.8660254037844387076, 1.000000000000000000, 0.8660254037844387076, 1.000000000000000000, 0.8660254037844387076, 1.000000000000000000, 0.8660254037844387076, 1.000000000000000000, 0.8660254037844387076, 1.000000000000000000, 0.8660254037844387076, 1.000000000000000000, 0.8660254037844387076, 1.000000000000000000, 0.8660254037844387076, 1.000000000000000000, 0.8660254037844387076, 1.000000000000000000, 0.8660254037844387076, 1.000000000000000000, 0.8660254037844387076, 1.000000000000000000, 0.8660254037844387076, 1.000000000000000000, 0.8660254037844387076, 1.000000000000000000, 0.8660254037844387076, 1.000000000000000000, 0.8660254037844387076, 1.000000000000000000, 0.8660254037844387076, 1.000000000000000000, 0.8660254037844387076, 1.000000000000000000, 0.8660254037844387076, 1.000000000000000000, 0.8660254037844387076, 1.000000000000000000, 0.8660254037844387076, 1.000000000000000000, 0.8660254037844387076, 1.000000000000000000, 0.8660254037844387076, 1.000000000000000000, 0.8660254037844387076, 1.000000000000000000, 0.8660254037844387076, 1.000000000000000000, 0.8660254037844387076, 1.000000000000000000, 0.8660254037844387076, 1.000000000000000000, 0.8660254037844387076, 1.000000000000000000, 0.8660254037844387076, 1.000000000000000000, 0.8660254037844387076, 1.000000000000000000, 0.8660254037844387076, 1.000000000000000000, 0.8660254037844387076, 1.000000000000000000, 0.8660254037844387076, 1.000000000000000000, 0.8660254037844387076, 1.000000000000000000, 0.8660254037844387076, 1.000000000000000000, 0.8660254037844387076, 1.000000000000000000, 0.8660254037844387076, 1.000000000000000000, 0.8660254037844387076, 1.000000000000000000, 0.8660254037844387076, 1.000000000000000000, 0.8660254037844387076, 1.000000000000000000, 0.8660254037844387076, 1.000000000000000000, 0.8660254037844387076, 1.000000000000000000, 0.8660254037844387076, 1.000000000000000000, 0.8660254037844387076, 1.000000000000000000, 0.8660254037844387076, 1.000000000000000000, 0.8660254037844387076, 1.000000000000000000, 0.8660254037844387076, 1.000000000000000000, 0.8660254037844387076, 1.000000000000000000, 0.9024577157650887083, 0.9469497795711399046, 0.9469497795711399046, 0.9469497795711399046 ) ) 
 REPRESENTATION_ITEM ( '' )  );
#21449 = CARTESIAN_POINT ( 'NONE',  ( 10.00000000000000000, -35.91791733033525702, 68.67312586194982771 ) ) ;
#21450 = EDGE_CURVE ( 'NONE', #15852, #19406, #51823, .T. ) ;
#21452 = CARTESIAN_POINT ( 'NONE',  ( -96.32500000000001705, 87.70503267997129626, 89.47083333333333144 ) ) ;
#21451 = AXIS2_PLACEMENT_3D ( 'NONE', #17036, #21548, #56897 ) ;
#21453 = EDGE_LOOP ( 'NONE', ( #12005, #40661, #13442, #48156 ) ) ;
#21454 = CARTESIAN_POINT ( 'NONE',  ( 92.69370383062498320, 90.00000000000002842, 78.84781250086714977 ) ) ;
#21455 = ORIENTED_EDGE ( 'NONE', *, *, #12119, .T. ) ;
#21456 = FACE_OUTER_BOUND ( 'NONE', #25020, .T. ) ;
#21458 = ORIENTED_EDGE ( 'NONE', *, *, #51684, .F. ) ;
#21457 = EDGE_CURVE ( 'NONE', #55964, #57897, #42324, .T. ) ;
#21459 = AXIS2_PLACEMENT_3D ( 'NONE', #64836, #31342, #36246 ) ;
#21460 = CARTESIAN_POINT ( 'NONE',  ( 0.000000000000000000, 0.000000000000000000, 125.0000000000000000 ) ) ;
#21461 = PLANE ( 'NONE',  #6780 ) ;
#21462 = CARTESIAN_POINT ( 'NONE',  ( 0.000000000000000000, 9.615535125378775305, 24.73947219025917121 ) ) ;
#21463 = CARTESIAN_POINT ( 'NONE',  ( -94.99999999999997158, -212.6630814284392557, 78.37156250086714238 ) ) ;
#21464 = CIRCLE ( 'NONE', #14285, 13.90444123027096879 ) ;
#21465 = AXIS2_PLACEMENT_3D ( 'NONE', #37966, #61276, #68026 ) ;
#21466 = LINE ( 'NONE', #3842, #59070 ) ;
#21467 = DIRECTION ( 'NONE',  ( -1.000000000000000000, -0.000000000000000000, 0.000000000000000000 ) ) ;
#21468 = CARTESIAN_POINT ( 'NONE',  ( -97.64999999999999147, -208.4700217866474929, 84.23208333333334963 ) ) ;
#21469 = ORIENTED_EDGE ( 'NONE', *, *, #32399, .F. ) ;
#21470 = AXIS2_PLACEMENT_3D ( 'NONE', #13898, #65433, #36108 ) ;
#21471 = EDGE_LOOP ( 'NONE', ( #6289, #60911, #7303, #30891 ) ) ;
#21472 = DIRECTION ( 'NONE',  ( 1.000000000000000000, 0.000000000000000000, 0.000000000000000000 ) ) ;
#21473 = VECTOR ( 'NONE', #62879, 1000.000000000000000 ) ;
#21474 = CARTESIAN_POINT ( 'NONE',  ( -92.34999999999990905, -211.5299782133524502, 88.99458333333333826 ) ) ;
#21475 = EDGE_CURVE ( 'NONE', #22889, #58924, #67535, .T. ) ;
#21476 = LINE ( 'NONE', #56830, #15151 ) ;
#21477 = ADVANCED_FACE ( 'NONE', ( #30265 ), #11229, .F. ) ;
#21478 = CARTESIAN_POINT ( 'NONE',  ( -96.15314808468751551, 88.00268892867056536, 81.49364583420047836 ) ) ;
#21479 = FACE_OUTER_BOUND ( 'NONE', #41775, .T. ) ;
#21480 = DIRECTION ( 'NONE',  ( -1.000000000000000000, -0.000000000000000000, 0.000000000000000000 ) ) ;
#21481 = ORIENTED_EDGE ( 'NONE', *, *, #73088, .F. ) ;
#21482 = CARTESIAN_POINT ( 'NONE',  ( -20.63750000000000284, -2.946905753441389499E-14, -1.643265707204933640E-14 ) ) ;
#21483 = CIRCLE ( 'NONE', #40721, 31.99999999999998579 ) ;
#21484 = DIRECTION ( 'NONE',  ( 0.000000000000000000, -0.1564344650402380854, 0.9876883405951365491 ) ) ;
#21486 = CARTESIAN_POINT ( 'NONE',  ( 0.000000000000000000, 27.13269053701132094, -25.88420570971372570 ) ) ;
#21485 = CIRCLE ( 'NONE', #43150, 42.00000000000000000 ) ;
#21487 = AXIS2_PLACEMENT_3D ( 'NONE', #24781, #42086, #65024 ) ;
#21488 = CARTESIAN_POINT ( 'NONE',  ( 10.00000000000000000, 17.80606268964540462, 33.00180498840053644 ) ) ;
#21489 = FACE_OUTER_BOUND ( 'NONE', #39511, .T. ) ;
#21490 = CARTESIAN_POINT ( 'NONE',  ( -97.30629616937497417, -208.6684592857803011, 78.95364583420048632 ) ) ;
#21491 = AXIS2_PLACEMENT_3D ( 'NONE', #12375, #28190, #51124 ) ;
#21492 = VECTOR ( 'NONE', #19931, 1000.000000000000000 ) ;
#21493 = FACE_OUTER_BOUND ( 'NONE', #8493, .T. ) ;
#21494 = AXIS2_PLACEMENT_3D ( 'NONE', #74322, #34101, #4435 ) ;
#21495 = VERTEX_POINT ( 'NONE', #7712 ) ;
#21496 = DIRECTION ( 'NONE',  ( -1.000000000000000000, -0.000000000000000000, 0.000000000000000000 ) ) ;
#21497 = CARTESIAN_POINT ( 'NONE',  ( 92.35000000039373447, 90.00002930740642171, 76.74344264317738862 ) ) ;
#21498 = DIRECTION ( 'NONE',  ( 0.000000000000000000, -0.6494480483301739993, -0.7604059656000390355 ) ) ;
#21499 = VERTEX_POINT ( 'NONE', #39812 ) ;
#21500 = DIRECTION ( 'NONE',  ( -1.000000000000000000, -0.000000000000000000, -0.000000000000000000 ) ) ;
#21501 = CARTESIAN_POINT ( 'NONE',  ( 11.99999999999999822, 0.000000000000000000, 0.000000000000000000 ) ) ;
#21502 = FACE_OUTER_BOUND ( 'NONE', #14715, .T. ) ;
#21503 = ORIENTED_EDGE ( 'NONE', *, *, #54481, .F. ) ;
#21504 = AXIS2_PLACEMENT_3D ( 'NONE', #60950, #49295, #71105 ) ;
#21505 = CARTESIAN_POINT ( 'NONE',  ( -97.64999999993855795, 90.00001182178863246, 76.10900611559313234 ) ) ;
#21506 = CARTESIAN_POINT ( 'NONE',  ( 0.000000000000000000, -9.188173127307592836, 40.98264845739746676 ) ) ;
#21507 = ORIENTED_EDGE ( 'NONE', *, *, #18737, .F. ) ;
#21508 = CONICAL_SURFACE ( 'NONE', #20289, 2.445500000000000007, 0.7853981633974678189 ) ;
#21509 = CARTESIAN_POINT ( 'NONE',  ( 23.49916127795269460, -121.5130826919798039, 5.500000000000000000 ) ) ;
#21510 = CARTESIAN_POINT ( 'NONE',  ( -95.00000000000002842, 93.05995642670504253, 77.77624999999999034 ) ) ;
#21511 = ORIENTED_EDGE ( 'NONE', *, *, #38387, .T. ) ;
#21512 = AXIS2_PLACEMENT_3D ( 'NONE', #12190, #41149, #29110 ) ;
#21513 = EDGE_CURVE ( 'NONE', #18038, #53602, #27916, .T. ) ;
#21514 = AXIS2_PLACEMENT_3D ( 'NONE', #60092, #13461, #48052 ) ;
#21515 = CARTESIAN_POINT ( 'NONE',  ( -3.000000000000000000, -0.9646360437375307573, 23.52805723605590060 ) ) ;
#21516 = AXIS2_PLACEMENT_3D ( 'NONE', #13612, #65504, #64761 ) ;
#21517 = VERTEX_POINT ( 'NONE', #34521 ) ;
#21518 = CARTESIAN_POINT ( 'NONE',  ( -92.35000000000003695, 90.00000000000004263, 76.98250000000000171 ) ) ;
#21519 = CARTESIAN_POINT ( 'NONE',  ( 0.000000000000000000, 62.50884508063487033, -41.76106447765422303 ) ) ;
#21520 = ORIENTED_EDGE ( 'NONE', *, *, #68681, .T. ) ;
#21521 = EDGE_LOOP ( 'NONE', ( #13503, #69731, #49130, #29633 ) ) ;
#21522 = VECTOR ( 'NONE', #62031, 1000.000000000000000 ) ;
#21523 = ADVANCED_FACE ( 'NONE', ( #45084 ), #68006, .T. ) ;
#21524 = ORIENTED_EDGE ( 'NONE', *, *, #39635, .T. ) ;
#21525 = CARTESIAN_POINT ( 'NONE',  ( 0.000000000000000000, 66.50666863322000211, 39.78640506895628448 ) ) ;
#21526 = EDGE_CURVE ( 'NONE', #9779, #15045, #11082, .T. ) ;
#21527 = ORIENTED_EDGE ( 'NONE', *, *, #2266, .F. ) ;
#21528 = ORIENTED_EDGE ( 'NONE', *, *, #45538, .F. ) ;
#21529 = CARTESIAN_POINT ( 'NONE',  ( 92.69370383062498320, 90.00000000000002842, 77.10156250086714635 ) ) ;
#21530 = DIRECTION ( 'NONE',  ( -1.000000000000000000, 0.000000000000000000, 0.000000000000000000 ) ) ;
#21531 = DIRECTION ( 'NONE',  ( 0.000000000000000000, 0.5877852522924684742, 0.8090169943749506709 ) ) ;
#21532 = EDGE_LOOP ( 'NONE', ( #29760, #11813, #18571, #24869 ) ) ;
#21533 = EDGE_CURVE ( 'NONE', #55639, #37724, #40538, .T. ) ;
#21534 = VERTEX_POINT ( 'NONE', #53207 ) ;
#21535 = ORIENTED_EDGE ( 'NONE', *, *, #28786, .T. ) ;
#21536 = CARTESIAN_POINT ( 'NONE',  ( 8.452893869119503023, -12.51233732111638375, 0.000000000000000000 ) ) ;
#21537 = ORIENTED_EDGE ( 'NONE', *, *, #60997, .F. ) ;
#21538 = CARTESIAN_POINT ( 'NONE',  ( 97.30629616937498838, -209.9999999999999716, 86.15031250086714465 ) ) ;
#21539 = AXIS2_PLACEMENT_3D ( 'NONE', #56983, #62252, #45336 ) ;
#21540 = VECTOR ( 'NONE', #9269, 1000.000000000000114 ) ;
#21541 = APPLICATION_PROTOCOL_DEFINITION ( 'draft international standard', 'automotive_design', 1998, #43164 ) ;
#21542 = DIRECTION ( 'NONE',  ( -0.000000000000000000, -0.000000000000000000, 1.000000000000000000 ) ) ;
#21543 = CARTESIAN_POINT ( 'NONE',  ( -94.99999999999997158, -209.9999999999999716, 90.00000000000000000 ) ) ;
#21544 = DIRECTION ( 'NONE',  ( -1.000000000000000000, 0.000000000000000000, 0.000000000000000000 ) ) ;
#21545 = DIRECTION ( 'NONE',  ( -1.000000000000000000, 0.000000000000000000, 0.000000000000000000 ) ) ;
#21546 = CYLINDRICAL_SURFACE ( 'NONE', #54035, 2.649999999999999467 ) ;
#21547 = AXIS2_PLACEMENT_3D ( 'NONE', #38093, #2459, #32071 ) ;
#21548 = DIRECTION ( 'NONE',  ( -1.000000000000000000, -0.000000000000000000, -0.000000000000000000 ) ) ;
#21549 = VECTOR ( 'NONE', #40952, 1000.000000000000000 ) ;
#21550 = CARTESIAN_POINT ( 'NONE',  ( -93.84685191531248449, -208.0026889286704943, 88.16114583420046813 ) ) ;
#21551 = CARTESIAN_POINT ( 'NONE',  ( -97.30629616937501680, 88.66845928578038638, 84.13947916753383538 ) ) ;
#21552 = ORIENTED_EDGE ( 'NONE', *, *, #46181, .T. ) ;
#21554 = CARTESIAN_POINT ( 'NONE',  ( -97.30629616937501680, 88.66845928578038638, 86.52072916753381548 ) ) ;
#21553 = CARTESIAN_POINT ( 'NONE',  ( 93.84685191531248449, 88.00268892867053694, 86.57364583420047666 ) ) ;
#21555 =( BOUNDED_CURVE ( )  B_SPLINE_CURVE ( 2, ( #56341, #40521, #22499, #45814, #50684, #45440, #57086 ),
 .UNSPECIFIED., .F., .F. ) 
 B_SPLINE_CURVE_WITH_KNOTS ( ( 3, 2, 2, 3 ),
 ( 0.02116741234826875415, 0.02822306216352945749, 0.03527882770441185395, 0.04233441017594429673 ),
 .UNSPECIFIED. ) 
 CURVE ( )  GEOMETRIC_REPRESENTATION_ITEM ( )  RATIONAL_B_SPLINE_CURVE ( ( 0.9999956052850527133, 0.8660276011779528549, 1.000000000000000000, 0.8660254037844387076, 1.000000000000000000, 0.8660288798979939306, 0.9999930479532725958 ) ) 
 REPRESENTATION_ITEM ( '' )  );
#21556 = ORIENTED_EDGE ( 'NONE', *, *, #19439, .F. ) ;
#21557 = LINE ( 'NONE', #32466, #61086 ) ;
#21558 = ADVANCED_FACE ( 'NONE', ( #24632 ), #51079, .T. ) ;
#21559 = CYLINDRICAL_SURFACE ( 'NONE', #49323, 31.99999999999998579 ) ;
#21560 = LINE ( 'NONE', #28311, #61951 ) ;
#21561 = CYLINDRICAL_SURFACE ( 'NONE', #60027, 37.49900000000000233 ) ;
#21562 = CYLINDRICAL_SURFACE ( 'NONE', #67480, 82.00000000000000000 ) ;
#21563 = CYLINDRICAL_SURFACE ( 'NONE', #54675, 2.649999999999985700 ) ;
#21564 = CARTESIAN_POINT ( 'NONE',  ( 0.000000000000000000, 0.000000000000000000, -25.03750572909317285 ) ) ;
#21565 = LINE ( 'NONE', #62565, #7062 ) ;
#21566 = ORIENTED_EDGE ( 'NONE', *, *, #34356, .T. ) ;
#21567 = ORIENTED_EDGE ( 'NONE', *, *, #30377, .F. ) ;
#21568 = CARTESIAN_POINT ( 'NONE',  ( -97.65000000000001990, 90.00000000000004263, 83.01499999999998636 ) ) ;
#21569 = EDGE_CURVE ( 'NONE', #73113, #51687, #53100, .T. ) ;
#21570 = CARTESIAN_POINT ( 'NONE',  ( 0.000000000000000000, 59.75363087400153006, -56.15606465354896670 ) ) ;
#21571 = EDGE_CURVE ( 'NONE', #43311, #36423, #34965, .T. ) ;
#21572 = CARTESIAN_POINT ( 'NONE',  ( -96.32500000000001705, 87.70503267997129626, 78.67583333333332973 ) ) ;
#21573 = CARTESIAN_POINT ( 'NONE',  ( 10.00000000000000000, 0.000000000000000000, 0.000000000000000000 ) ) ;
#21574 = DIRECTION ( 'NONE',  ( -1.000000000000000000, -0.000000000000000000, 0.000000000000000000 ) ) ;
#21575 = CARTESIAN_POINT ( 'NONE',  ( 93.67499999999998295, 92.29496732002878900, 87.43354166840096298 ) ) ;
#21576 = LINE ( 'NONE', #15576, #61363 ) ;
#21577 = DIRECTION ( 'NONE',  ( 0.000000000000000000, 0.000000000000000000, 1.000000000000000000 ) ) ;
#21578 = CIRCLE ( 'NONE', #16766, 31.99999999999998579 ) ;
#21579 = ADVANCED_FACE ( 'NONE', ( #5986 ), #2115, .F. ) ;
#21580 = VERTEX_POINT ( 'NONE', #18978 ) ;
#21581 = CARTESIAN_POINT ( 'NONE',  ( -92.69370383062502583, 91.33154071421968467, 82.39322916753381776 ) ) ;
#21583 = CARTESIAN_POINT ( 'NONE',  ( 15.00000000000000000, 0.000000000000000000, 0.000000000000000000 ) ) ;
#21582 = VECTOR ( 'NONE', #11768, 1000.000000000000114 ) ;
#21584 = CARTESIAN_POINT ( 'NONE',  ( -95.00000000000002842, 86.94004357329504273, 85.71374999999999034 ) ) ;
#21585 = DIRECTION ( 'NONE',  ( -1.000000000000000000, 0.000000000000000000, 0.000000000000000000 ) ) ;
#21586 = DIRECTION ( 'NONE',  ( 0.000000000000000000, 0.000000000000000000, 1.000000000000000000 ) ) ;
#21587 = AXIS2_PLACEMENT_3D ( 'NONE', #55917, #27717, #4432 ) ;
#21588 = DIRECTION ( 'NONE',  ( -3.069126149805119941E-16, -1.000000000000000000, 0.000000000000000000 ) ) ;
#21589 = CARTESIAN_POINT ( 'NONE',  ( -94.99999999999997158, -212.6630814284392557, 89.32531250086715602 ) ) ;
#21590 = PRESENTATION_STYLE_ASSIGNMENT (( #45667 ) ) ;
#21591 = DIRECTION ( 'NONE',  ( -1.000000000000000000, -1.427937372958405461E-15, -7.962523111839130290E-16 ) ) ;
#21592 = CIRCLE ( 'NONE', #34091, 77.49899999999999523 ) ;
#21593 = CARTESIAN_POINT ( 'NONE',  ( 92.69370383062498320, 91.33154071421968467, 82.12864583420048348 ) ) ;
#21594 = CARTESIAN_POINT ( 'NONE',  ( -96.15314808468747287, -208.0026889286704943, 84.61572916753381435 ) ) ;
#21595 = CARTESIAN_POINT ( 'NONE',  ( 11.99999999999999822, 55.20638768913831029, -51.02545421589267960 ) ) ;
#21596 = AXIS2_PLACEMENT_3D ( 'NONE', #47651, #42024, #66793 ) ;
#21597 = ORIENTED_EDGE ( 'NONE', *, *, #46965, .T. ) ;
#21598 = CARTESIAN_POINT ( 'NONE',  ( -92.35000000045957336, 90.00004935162611730, 87.22187670868784437 ) ) ;
#21599 = CARTESIAN_POINT ( 'NONE',  ( -92.34999999999999432, -211.5299782133524502, 77.56458333333333144 ) ) ;
#21600 = DIRECTION ( 'NONE',  ( -1.000000000000000000, -0.000000000000000000, -0.000000000000000000 ) ) ;
#21601 = VECTOR ( 'NONE', #38239, 1000.000000000000000 ) ;
#21602 = AXIS2_PLACEMENT_3D ( 'NONE', #69276, #56896, #52723 ) ;
#21603 = AXIS2_PLACEMENT_3D ( 'NONE', #47193, #69746, #40821 ) ;
#21604 = CIRCLE ( 'NONE', #64884, 82.00000000000000000 ) ;
#21605 = AXIS2_PLACEMENT_3D ( 'NONE', #72274, #73754, #67006 ) ;
#21606 = CARTESIAN_POINT ( 'NONE',  ( -93.84685191531252713, 88.00268892867056536, 79.85322916753381151 ) ) ;
#21607 = CARTESIAN_POINT ( 'NONE',  ( 97.30629616937498838, -209.9999999999999716, 80.43531250086714124 ) ) ;
#21608 = ORIENTED_EDGE ( 'NONE', *, *, #72222, .F. ) ;
#21609 = CARTESIAN_POINT ( 'NONE',  ( 0.000000000000000000, 35.47612816024523852, 22.48208911017513145 ) ) ;
#21610 = ORIENTED_EDGE ( 'NONE', *, *, #53378, .T. ) ;
#21611 = CARTESIAN_POINT ( 'NONE',  ( 92.35000000052950497, 90.00003365185392568, 81.18829462297337329 ) ) ;
#21612 = ORIENTED_EDGE ( 'NONE', *, *, #19463, .T. ) ;
#21613 = EDGE_CURVE ( 'NONE', #8165, #30236, #17093, .T. ) ;
#21614 = CARTESIAN_POINT ( 'NONE',  ( 97.64999999999999147, -209.9999999999999716, 90.00000000000000000 ) ) ;
#21615 = VERTEX_POINT ( 'NONE', #64867 ) ;
#21616 = ORIENTED_EDGE ( 'NONE', *, *, #42890, .F. ) ;
#21617 = EDGE_CURVE ( 'NONE', #46834, #48739, #6636, .T. ) ;
#21618 = ORIENTED_EDGE ( 'NONE', *, *, #36425, .F. ) ;
#21619 = CARTESIAN_POINT ( 'NONE',  ( 96.15314808468748708, -208.0026889286704943, 75.61989583420049144 ) ) ;
#21620 = EDGE_CURVE ( 'NONE', #46914, #15732, #50724, .T. ) ;
#21621 = VERTEX_POINT ( 'NONE', #43793 ) ;
#21622 = DIRECTION ( 'NONE',  ( -1.000000000000000000, 0.000000000000000000, 0.000000000000000000 ) ) ;
#21623 = DIRECTION ( 'NONE',  ( -1.000000000000000000, 0.000000000000000000, 0.000000000000000000 ) ) ;
#21624 = CARTESIAN_POINT ( 'NONE',  ( 94.99999999999998579, 87.33691857156068750, 87.42031250086715488 ) ) ;
#21625 = AXIS2_PLACEMENT_3D ( 'NONE', #11718, #34663, #27538 ) ;
#21626 = CARTESIAN_POINT ( 'NONE',  ( 5.000000000000002665, 34.94270380257741948, -74.18225833017852722 ) ) ;
#21627 = CARTESIAN_POINT ( 'NONE',  ( 92.35000000000000853, -209.9999999999999716, 76.66499999999999204 ) ) ;
#21628 = ORIENTED_EDGE ( 'NONE', *, *, #38643, .F. ) ;
#21629 = EDGE_CURVE ( 'NONE', #9811, #18134, #43050, .T. ) ;
#21630 = ORIENTED_EDGE ( 'NONE', *, *, #68496, .F. ) ;
#21631 = AXIS2_PLACEMENT_3D ( 'NONE', #20390, #25656, #19271 ) ;
#21632 = ORIENTED_EDGE ( 'NONE', *, *, #2033, .F. ) ;
#21633 = ORIENTED_EDGE ( 'NONE', *, *, #72326, .T. ) ;
#21634 = FACE_OUTER_BOUND ( 'NONE', #34240, .T. ) ;
#21635 = AXIS2_PLACEMENT_3D ( 'NONE', #46850, #18625, #65254 ) ;
#21636 = DIRECTION ( 'NONE',  ( -1.000000000000000000, 0.000000000000000000, -0.000000000000000000 ) ) ;
#21637 = DIRECTION ( 'NONE',  ( -1.000000000000000000, 0.000000000000000000, -0.000000000000000000 ) ) ;
#21638 = AXIS2_PLACEMENT_3D ( 'NONE', #42125, #70291, #36462 ) ;
#21639 = CARTESIAN_POINT ( 'NONE',  ( -8.452893869119503023, -12.51233732111638375, -1.199999999999999956 ) ) ;
#21640 = FACE_OUTER_BOUND ( 'NONE', #6906, .T. ) ;
#21641 = LINE ( 'NONE', #34783, #57299 ) ;
#21642 = VERTEX_POINT ( 'NONE', #55427 ) ;
#21643 = CARTESIAN_POINT ( 'NONE',  ( -97.64999999999994884, -211.5299782133524502, 81.24229166840098060 ) ) ;
#21644 = ORIENTED_EDGE ( 'NONE', *, *, #39108, .F. ) ;
#21645 = CARTESIAN_POINT ( 'NONE',  ( 10.00000000000000000, 0.000000000000000000, 0.000000000000000000 ) ) ;
#21646 = ORIENTED_EDGE ( 'NONE', *, *, #49219, .F. ) ;
#21648 = CARTESIAN_POINT ( 'NONE',  ( -92.35000000000005116, 91.52997821335253548, 83.46479166840096298 ) ) ;
#21647 = CARTESIAN_POINT ( 'NONE',  ( 94.99999999999998579, 93.05995642670504253, 81.03062500173430749 ) ) ;
#21649 = EDGE_LOOP ( 'NONE', ( #30424, #45563, #40231, #31968 ) ) ;
#21650 = CARTESIAN_POINT ( 'NONE',  ( 94.99999999999998579, 92.66308142843935514, 83.29281250086717137 ) ) ;
#21651 = EDGE_CURVE ( 'NONE', #5520, #2120, #31656, .T. ) ;
#21652 = CARTESIAN_POINT ( 'NONE',  ( 11.99999999999999822, -44.88180994100329713, -63.18004540533077318 ) ) ;
#21653 = CARTESIAN_POINT ( 'NONE',  ( -93.67499999999998295, -212.2949673200287179, 82.67104166840096013 ) ) ;
#21654 = DIRECTION ( 'NONE',  ( 1.000000000000000000, 0.000000000000000000, -0.000000000000000000 ) ) ;
#21655 = AXIS2_PLACEMENT_3D ( 'NONE', #11856, #58110, #48586 ) ;
#21656 = FACE_OUTER_BOUND ( 'NONE', #69415, .T. ) ;
#21657 = DIRECTION ( 'NONE',  ( 1.000000000000000000, 0.000000000000000000, 0.000000000000000000 ) ) ;
#21658 = ORIENTED_EDGE ( 'NONE', *, *, #62312, .T. ) ;
#21659 = CARTESIAN_POINT ( 'NONE',  ( 97.65000000000004832, -208.4700217866475214, 77.67041666666666799 ) ) ;
#21660 = DIRECTION ( 'NONE',  ( 0.000000000000000000, 0.000000000000000000, 1.000000000000000000 ) ) ;
#21661 = AXIS2_PLACEMENT_3D ( 'NONE', #8242, #48471, #54124 ) ;
#21662 = DIRECTION ( 'NONE',  ( 1.000000000000000000, 1.427937372958405461E-15, 7.962523111839130290E-16 ) ) ;
#21663 = VERTEX_POINT ( 'NONE', #37414 ) ;
#21664 = ORIENTED_EDGE ( 'NONE', *, *, #34449, .F. ) ;
#21665 = AXIS2_PLACEMENT_3D ( 'NONE', #30358, #8920, #36746 ) ;
#21666 = EDGE_CURVE ( 'NONE', #33478, #59348, #70855, .T. ) ;
#21667 = CARTESIAN_POINT ( 'NONE',  ( 0.000000000000000000, 39.78640506895698081, -66.50666863321957578 ) ) ;
#21668 = EDGE_CURVE ( 'NONE', #15499, #56357, #68728, .T. ) ;
#21669 = LINE ( 'NONE', #33304, #5462 ) ;
#21670 = CARTESIAN_POINT ( 'NONE',  ( -97.65000000000001990, 90.00000000000004263, 90.00000000000000000 ) ) ;
#21671 = CARTESIAN_POINT ( 'NONE',  ( -97.30629616937495996, -209.9999999999999716, 80.91156250086716284 ) ) ;
#21672 = ORIENTED_EDGE ( 'NONE', *, *, #34194, .T. ) ;
#21673 = FACE_BOUND ( 'NONE', #25864, .T. ) ;
#21674 = ORIENTED_EDGE ( 'NONE', *, *, #64527, .F. ) ;
#21675 = DIRECTION ( 'NONE',  ( -1.000000000000000000, 0.000000000000000000, 0.000000000000000000 ) ) ;
#21676 = FACE_BOUND ( 'NONE', #61839, .T. ) ;
#21677 = CARTESIAN_POINT ( 'NONE',  ( -94.99999999999997158, -213.0599564267049857, 76.26812500173430465 ) ) ;
#21678 = CARTESIAN_POINT ( 'NONE',  ( 96.15314808468748708, 91.99731107132950569, 77.36614583420046642 ) ) ;
#21679 = DIRECTION ( 'NONE',  ( -1.000000000000000000, 0.000000000000000000, -0.000000000000000000 ) ) ;
#21680 = DIRECTION ( 'NONE',  ( -1.000000000000000000, 0.000000000000000000, 0.000000000000000000 ) ) ;
#21681 = DIRECTION ( 'NONE',  ( 1.000000000000000000, -0.000000000000000000, -0.000000000000000000 ) ) ;
#21682 = CARTESIAN_POINT ( 'NONE',  ( 0.4966694826857007139, -118.5846133302278247, -2.500000000000000000 ) ) ;
#21683 = CARTESIAN_POINT ( 'NONE',  ( 10.00000000000000000, 0.000000000000000000, 0.000000000000000000 ) ) ;
#21684 = DIRECTION ( 'NONE',  ( -0.3311129884571280546, -0.9435911131814402886, 0.000000000000000000 ) ) ;
#21685 = CARTESIAN_POINT ( 'NONE',  ( 92.34999999999995168, -211.5299782133524218, 83.06791666666666174 ) ) ;
#21686 = CARTESIAN_POINT ( 'NONE',  ( 92.69370383062498320, 90.00000000000002842, 89.16656250086715829 ) ) ;
#21687 = DIRECTION ( 'NONE',  ( -1.000000000000000000, 0.000000000000000000, -0.000000000000000000 ) ) ;
#21688 = CARTESIAN_POINT ( 'NONE',  ( 0.000000000000000000, 37.58145647212453611, 0.6853352020791767529 ) ) ;
#21689 = EDGE_LOOP ( 'NONE', ( #65947, #8074, #11473, #48353 ) ) ;
#21690 = AXIS2_PLACEMENT_3D ( 'NONE', #22435, #45380, #56278 ) ;
#21691 = CARTESIAN_POINT ( 'NONE',  ( -92.69370383062505425, 91.33154071421968467, 82.39322916753381776 ) ) ;
#21692 = VECTOR ( 'NONE', #20094, 1000.000000000000000 ) ;
#21693 = DIRECTION ( 'NONE',  ( 0.000000000000000000, 0.000000000000000000, 1.000000000000000000 ) ) ;
#21694 = CARTESIAN_POINT ( 'NONE',  ( 3.429551818649054340, -146.3199197248623875, 5.500000000000000000 ) ) ;
#21695 = EDGE_CURVE ( 'NONE', #10267, #46506, #13479, .T. ) ;
#21696 = EDGE_LOOP ( 'NONE', ( #15878, #48183, #25469, #74244 ) ) ;
#21697 = CARTESIAN_POINT ( 'NONE',  ( 10.00000000000000000, 0.000000000000000000, 0.000000000000000000 ) ) ;
#21698 = CARTESIAN_POINT ( 'NONE',  ( 10.00000000000000178, 2.571758278209441661E-15, -21.00000000000000000 ) ) ;
#21699 = CARTESIAN_POINT ( 'NONE',  ( 10.00000000000000000, 37.01155633439059756, 6.555932627142549762 ) ) ;
#21700 = ADVANCED_FACE ( 'NONE', ( #25383 ), #20478, .F. ) ;
#21701 = VECTOR ( 'NONE', #66169, 1000.000000000000114 ) ;
#21702 = AXIS2_PLACEMENT_3D ( 'NONE', #19154, #1914, #58641 ) ;
#21703 = CARTESIAN_POINT ( 'NONE',  ( 0.000000000000000000, 0.000000000000000000, 0.000000000000000000 ) ) ;
#21704 = CARTESIAN_POINT ( 'NONE',  ( 95.00000000000000000, -207.3369185715606307, 78.84781250086714977 ) ) ;
#21705 = EDGE_CURVE ( 'NONE', #59850, #48671, #1570, .T. ) ;
#21706 = CIRCLE ( 'NONE', #39716, 16.00000000000000000 ) ;
#21707 = ORIENTED_EDGE ( 'NONE', *, *, #2239, .F. ) ;
#21708 = CIRCLE ( 'NONE', #48127, 82.00000000000000000 ) ;
#21709 = EDGE_CURVE ( 'NONE', #6766, #44013, #42309, .T. ) ;
#21710 = ORIENTED_EDGE ( 'NONE', *, *, #69910, .F. ) ;
#21711 = CARTESIAN_POINT ( 'NONE',  ( 5.000000000000002665, 74.18225833017937987, -34.94270380257560049 ) ) ;
#21712 = CARTESIAN_POINT ( 'NONE',  ( -10.00000000000000000, 0.000000000000000000, 0.000000000000000000 ) ) ;
#21713 = CARTESIAN_POINT ( 'NONE',  ( 0.000000000000000000, 39.47590169984846398, 71.87247863392427405 ) ) ;
#21714 = LINE ( 'NONE', #43921, #11046 ) ;
#21715 = CARTESIAN_POINT ( 'NONE',  ( 97.64999999999324132, -209.9999940177821713, 82.14187520865721126 ) ) ;
#21716 = CARTESIAN_POINT ( 'NONE',  ( 97.64999999999999147, -209.9999999999999716, 87.14249999999999829 ) ) ;
#21717 = ADVANCED_FACE ( 'NONE', ( #13711 ), #51913, .T. ) ;
#21718 = ORIENTED_EDGE ( 'NONE', *, *, #45073, .T. ) ;
#21719 = DIRECTION ( 'NONE',  ( -1.000000000000000000, 0.000000000000000000, 0.000000000000000000 ) ) ;
#21720 = ORIENTED_EDGE ( 'NONE', *, *, #2328, .T. ) ;
#21721 = VERTEX_POINT ( 'NONE', #8080 ) ;
#21722 = DIRECTION ( 'NONE',  ( -0.9827303690289279636, -0.1850432970638682117, 0.000000000000000000 ) ) ;
#21723 = DIRECTION ( 'NONE',  ( -1.000000000000000000, -0.000000000000000000, 0.000000000000000000 ) ) ;
#21724 = ORIENTED_EDGE ( 'NONE', *, *, #26062, .T. ) ;
#21725 = CARTESIAN_POINT ( 'NONE',  ( 92.35001943615621656, -208.4700105651774606, 78.59645755884378104 ) ) ;
#21726 = CARTESIAN_POINT ( 'NONE',  ( 92.35000000000002274, -208.4700217866474645, 81.13645833506764404 ) ) ;
#21727 = CARTESIAN_POINT ( 'NONE',  ( 96.32499999999998863, 87.70503267997126784, 81.95666666666666345 ) ) ;
#21728 = ORIENTED_EDGE ( 'NONE', *, *, #7880, .T. ) ;
#21729 = CARTESIAN_POINT ( 'NONE',  ( 10.00000000000000000, -10.96151621346461447, -35.95386929396268272 ) ) ;
#21730 = ORIENTED_EDGE ( 'NONE', *, *, #9397, .F. ) ;
#21731 = CARTESIAN_POINT ( 'NONE',  ( 0.000000000000000000, 6.762365576493643893, -25.66652317338391853 ) ) ;
#21732 = EDGE_CURVE ( 'NONE', #50224, #14612, #60433, .T. ) ;
#21733 = VERTEX_POINT ( 'NONE', #43435 ) ;
#21734 = CARTESIAN_POINT ( 'NONE',  ( 50.00005079999999680, 0.000000000000000000, 0.000000000000000000 ) ) ;
#21735 = CARTESIAN_POINT ( 'NONE',  ( -92.69370383062504004, 90.00000000000004263, 85.67406250086715147 ) ) ;
#21736 = CARTESIAN_POINT ( 'NONE',  ( 97.30629616937498838, 91.33154071421968467, 79.21822916753380639 ) ) ;
#21737 = ADVANCED_FACE ( 'NONE', ( #59978 ), #66352, .T. ) ;
#21738 = EDGE_LOOP ( 'NONE', ( #14032, #42267, #53511, #15944 ) ) ;
#21739 = EDGE_CURVE ( 'NONE', #53358, #52748, #30284, .T. ) ;
#21740 = CYLINDRICAL_SURFACE ( 'NONE', #22586, 23.50000000000489919 ) ;
#21741 = DIRECTION ( 'NONE',  ( -0.000000000000000000, -0.000000000000000000, 1.000000000000000000 ) ) ;
#21742 = DIRECTION ( 'NONE',  ( -1.000000000000000000, -0.000000000000000000, -0.000000000000000000 ) ) ;
#21743 = CIRCLE ( 'NONE', #26517, 42.00000000000000000 ) ;
#21744 = CARTESIAN_POINT ( 'NONE',  ( 12.00000000000000000, -19.89357724625003598, -12.59942793731059041 ) ) ;
#21745 = ORIENTED_EDGE ( 'NONE', *, *, #39498, .T. ) ;
#21746 = PLANE ( 'NONE',  #15249 ) ;
#21747 = AXIS2_PLACEMENT_3D ( 'NONE', #3392, #72155, #66534 ) ;
#21748 = EDGE_CURVE ( 'NONE', #3018, #31113, #48305, .T. ) ;
#21749 = ADVANCED_FACE ( 'NONE', ( #54323 ), #72690, .T. ) ;
#21750 = CARTESIAN_POINT ( 'NONE',  ( -93.84685191531248449, -208.0026889286704943, 81.81114583420047381 ) ) ;
#21751 = VERTEX_POINT ( 'NONE', #33221 ) ;
#21752 = ORIENTED_EDGE ( 'NONE', *, *, #17546, .T. ) ;
#21753 = FACE_OUTER_BOUND ( 'NONE', #26107, .T. ) ;
#21754 = VERTEX_POINT ( 'NONE', #56922 ) ;
#21755 = EDGE_CURVE ( 'NONE', #4487, #63285, #45925, .T. ) ;
#21756 = FACE_OUTER_BOUND ( 'NONE', #40870, .T. ) ;
#21757 = DIRECTION ( 'NONE',  ( -1.000000000000000000, -0.000000000000000000, -0.000000000000000000 ) ) ;
#21758 = ORIENTED_EDGE ( 'NONE', *, *, #43886, .F. ) ;
#21759 = CARTESIAN_POINT ( 'NONE',  ( -92.69370383062498320, -211.3315407142195852, 75.93739583420047268 ) ) ;
#21760 = ORIENTED_EDGE ( 'NONE', *, *, #22870, .T. ) ;
#21761 = DIRECTION ( 'NONE',  ( 0.000000000000000000, 0.7604059656000276002, 0.6494480483301875440 ) ) ;
#21762 = CARTESIAN_POINT ( 'NONE',  ( 0.000000000000000000, 0.000000000000000000, -40.00000000000000000 ) ) ;
#21763 = FACE_OUTER_BOUND ( 'NONE', #29032, .T. ) ;
#21764 = CARTESIAN_POINT ( 'NONE',  ( 10.00000000000000000, 65.59268652807210742, 36.72794159290264560 ) ) ;
#21765 = ADVANCED_FACE ( 'NONE', ( #45274 ), #35117, .F. ) ;
#21766 = DIRECTION ( 'NONE',  ( 1.000000000000000000, -0.000000000000000000, 0.000000000000000000 ) ) ;
#21767 = VECTOR ( 'NONE', #17053, 1000.000000000000000 ) ;
#21768 = DIRECTION ( 'NONE',  ( 0.000000000000000000, 0.000000000000000000, 1.000000000000000000 ) ) ;
#21769 = CARTESIAN_POINT ( 'NONE',  ( 93.84685191531248449, 91.99731107132950569, 88.26697916753380468 ) ) ;
#21770 = FACE_OUTER_BOUND ( 'NONE', #37210, .T. ) ;
#21771 = CIRCLE ( 'NONE', #50579, 82.00000000000000000 ) ;
#21772 = CARTESIAN_POINT ( 'NONE',  ( 0.000000000000000000, 17.67226234102874116, -33.17418723428288274 ) ) ;
#21773 = DIRECTION ( 'NONE',  ( 0.000000000000000000, 0.000000000000000000, 1.000000000000000000 ) ) ;
#21774 = CARTESIAN_POINT ( 'NONE',  ( 10.00000000000000000, -41.81611651403859042, -3.925862922256606602 ) ) ;
#21775 = CARTESIAN_POINT ( 'NONE',  ( 97.64999999999999147, -209.9999999999999716, 78.25249999999999773 ) ) ;
#21776 = CARTESIAN_POINT ( 'NONE',  ( 95.00000000000000000, -209.9999999999999716, 90.00000000000000000 ) ) ;
#21777 = CARTESIAN_POINT ( 'NONE',  ( 11.99999999999999822, 0.000000000000000000, 0.000000000000000000 ) ) ;
#21778 =( BOUNDED_CURVE ( )  B_SPLINE_CURVE ( 2, ( #47748, #47025, #24822, #19542, #7896, #36105, #42492, #18798, #53032, #54146, #65430 ),
 .UNSPECIFIED., .F., .F. ) 
 B_SPLINE_CURVE_WITH_KNOTS ( ( 3, 2, 2, 2, 2, 3 ),
 ( 0.4233457466685775494, 0.4233459324529421086, 0.4304016979938243836, 0.4374574635347067142, 0.4445132290755889337, 0.4445132602971398339 ),
 .UNSPECIFIED. ) 
 CURVE ( )  GEOMETRIC_REPRESENTATION_ITEM ( )  RATIONAL_B_SPLINE_CURVE ( ( 0.9999929448534821130, 0.9999964723338545802, 1.000000000000000000, 0.8660254037844387076, 1.000000000000000000, 0.8660254037844387076, 1.000000000000000000, 0.8660254037844387076, 1.000000000000000000, 0.9999994071664300987, 0.9999988143381067784 ) ) 
 REPRESENTATION_ITEM ( '' )  );
#21779 = DIRECTION ( 'NONE',  ( 0.8225049752423776450, 0.5687579148473764779, 0.000000000000000000 ) ) ;
#21780 = CARTESIAN_POINT ( 'NONE',  ( 0.000000000000000000, 77.32052557432849937, -5.256550761632002633 ) ) ;
#21781 = CARTESIAN_POINT ( 'NONE',  ( 92.35000000000002274, -208.4700217866474361, 84.86708333333332632 ) ) ;
#21782 = DIRECTION ( 'NONE',  ( -1.000000000000000000, 0.000000000000000000, 0.000000000000000000 ) ) ;
#21783 = CYLINDRICAL_SURFACE ( 'NONE', #14286, 37.49900000000000233 ) ;
#21784 = CARTESIAN_POINT ( 'NONE',  ( -93.67499999999998295, -212.2949673200287179, 84.49666666666666970 ) ) ;
#21785 = CYLINDRICAL_SURFACE ( 'NONE', #44603, 77.49899999999999523 ) ;
#21786 = PRODUCT_DEFINITION_SHAPE ( 'NONE', 'NONE',  #33419 ) ;
#21787 = CARTESIAN_POINT ( 'NONE',  ( -95.00000000000002842, 93.05995642670504253, 77.14124999999999943 ) ) ;
#21788 = CARTESIAN_POINT ( 'NONE',  ( 10.00000000000000000, 39.78640506895604290, 66.50666863322015843 ) ) ;
#21789 = SURFACE_STYLE_FILL_AREA ( #22171 ) ;
#21790 = DIRECTION ( 'NONE',  ( 1.000000000000000000, 0.000000000000000000, 0.000000000000000000 ) ) ;
#21791 =( GEOMETRIC_REPRESENTATION_CONTEXT ( 3 ) GLOBAL_UNCERTAINTY_ASSIGNED_CONTEXT ( ( #55031 ) ) GLOBAL_UNIT_ASSIGNED_CONTEXT ( ( #38147, #3228, #15590 ) ) REPRESENTATION_CONTEXT ( 'NONE', 'WORKASPACE' ) );
#21792 = VECTOR ( 'NONE', #18425, 1000.000000000000000 ) ;
#21793 = EDGE_CURVE ( 'NONE', #49620, #27381, #68196, .T. ) ;
#21794 = CIRCLE ( 'NONE', #12185, 31.99999999999999645 ) ;
#21795 = CARTESIAN_POINT ( 'NONE',  ( 92.69370383062501162, -209.9999999999999716, 89.16656250086715829 ) ) ;
#21796 = ADVANCED_FACE ( 'NONE', ( #67448, #34343, #32850, #16692, #27201, #38880, #45653 ), #61820, .F. ) ;
#21797 = CIRCLE ( 'NONE', #48215, 3.299999999999997158 ) ;
#21798 = EDGE_LOOP ( 'NONE', ( #73584, #20710, #50204, #70895 ) ) ;
#21799 = EDGE_CURVE ( 'NONE', #45134, #27007, #5429, .T. ) ;
#21800 = ORIENTED_EDGE ( 'NONE', *, *, #66707, .F. ) ;
#21801 = ADVANCED_FACE ( 'NONE', ( #39996 ), #56167, .T. ) ;
#21802 = CIRCLE ( 'NONE', #65025, 0.2999999999999999334 ) ;
#21803 = DIRECTION ( 'NONE',  ( 0.000000000000000000, 0.000000000000000000, 1.000000000000000000 ) ) ;
#21804 = ORIENTED_EDGE ( 'NONE', *, *, #12984, .T. ) ;
#21805 = DIRECTION ( 'NONE',  ( 0.000000000000000000, 0.000000000000000000, -1.000000000000000000 ) ) ;
#21806 = CARTESIAN_POINT ( 'NONE',  ( 92.69370383062501162, -208.6684592857803295, 76.88989583420047325 ) ) ;
#21807 = ORIENTED_EDGE ( 'NONE', *, *, #64934, .F. ) ;
#21808 = CARTESIAN_POINT ( 'NONE',  ( 97.30629616937498838, -211.3315407142195852, 83.08114583420048405 ) ) ;
#21809 = ORIENTED_EDGE ( 'NONE', *, *, #1808, .F. ) ;
#21810 = DIRECTION ( 'NONE',  ( -1.000000000000000000, -0.000000000000000000, 0.000000000000000000 ) ) ;
#21811 = EDGE_LOOP ( 'NONE', ( #39774, #43846, #9617, #65122 ) ) ;
#21812 = AXIS2_PLACEMENT_3D ( 'NONE', #10197, #26378, #44798 ) ;
#21813 = CARTESIAN_POINT ( 'NONE',  ( -92.69370383062502583, 91.33154071421968467, 75.56697916753383026 ) ) ;
#21814 = CIRCLE ( 'NONE', #71065, 82.00000000000000000 ) ;
#21815 = ORIENTED_EDGE ( 'NONE', *, *, #57917, .F. ) ;
#21816 = CARTESIAN_POINT ( 'NONE',  ( 5.000000000000002665, 29.01471420065674423, -76.69515212745984911 ) ) ;
#21817 = AXIS2_PLACEMENT_3D ( 'NONE', #56942, #46031, #73837 ) ;
#21818 = VERTEX_POINT ( 'NONE', #22713 ) ;
#21819 = CARTESIAN_POINT ( 'NONE',  ( 97.64999999999999147, 90.00000000000002842, 85.87249999999998806 ) ) ;
#21820 = DIRECTION ( 'NONE',  ( 0.000000000000000000, 0.000000000000000000, 1.000000000000000000 ) ) ;
#21821 = EDGE_CURVE ( 'NONE', #35409, #63658, #31501, .T. ) ;
#21822 = ORIENTED_EDGE ( 'NONE', *, *, #60595, .F. ) ;
#21823 = DIRECTION ( 'NONE',  ( 0.000000000000000000, -0.4539904997395541320, 0.8910065241883640130 ) ) ;
#21824 = ORIENTED_EDGE ( 'NONE', *, *, #27940, .F. ) ;
#21825 = DIRECTION ( 'NONE',  ( -1.000000000000000000, 0.000000000000000000, 0.000000000000000000 ) ) ;
#21826 = ORIENTED_EDGE ( 'NONE', *, *, #66540, .T. ) ;
#21827 = VERTEX_POINT ( 'NONE', #61448 ) ;
#21828 = ORIENTED_EDGE ( 'NONE', *, *, #25985, .T. ) ;
#21829 = CARTESIAN_POINT ( 'NONE',  ( 97.30629616937498838, -209.9999999999999716, 75.35531250086714294 ) ) ;
#21830 = ADVANCED_FACE ( 'NONE', ( #50522 ), #22331, .T. ) ;
#21831 = EDGE_CURVE ( 'NONE', #2794, #65091, #39361, .T. ) ;
#21832 = CONTEXT_DEPENDENT_SHAPE_REPRESENTATION ( #64783, #13463 ) ;
#21833 = LINE ( 'NONE', #60944, #58198 ) ;
#21834 = ORIENTED_EDGE ( 'NONE', *, *, #62697, .F. ) ;
#21835 = ORIENTED_EDGE ( 'NONE', *, *, #63676, .F. ) ;
#21836 = VERTEX_POINT ( 'NONE', #11410 ) ;
#21837 = FACE_OUTER_BOUND ( 'NONE', #66867, .T. ) ;
#21838 = DIRECTION ( 'NONE',  ( -1.000000000000000000, 0.000000000000000000, -0.000000000000000000 ) ) ;
#21839 = CARTESIAN_POINT ( 'NONE',  ( -92.69370383062502583, 91.33154071421968467, 74.93197916753381094 ) ) ;
#21840 = ORIENTED_EDGE ( 'NONE', *, *, #20449, .T. ) ;
#21841 = CARTESIAN_POINT ( 'NONE',  ( 92.69370383062498320, 90.00000000000002842, 76.30781250086714351 ) ) ;
#21842 = ORIENTED_EDGE ( 'NONE', *, *, #39386, .T. ) ;
#21843 = CARTESIAN_POINT ( 'NONE',  ( 97.64999999999999147, 90.00000000000002842, 78.33187500173430351 ) ) ;
#21844 = CARTESIAN_POINT ( 'NONE',  ( -92.69370383062498320, -209.9999999999999716, 88.05531250086713158 ) ) ;
#21845 = ORIENTED_EDGE ( 'NONE', *, *, #49527, .T. ) ;
#21846 = PLANE ( 'NONE',  #41027 ) ;
#21847 = DIRECTION ( 'NONE',  ( 0.000000000000000000, -0.9510565162951500895, -0.3090169943749583314 ) ) ;
#21848 = CARTESIAN_POINT ( 'NONE',  ( 11.99999999999999822, 0.000000000000000000, 0.000000000000000000 ) ) ;
#21849 = CARTESIAN_POINT ( 'NONE',  ( -96.15314808468745866, -211.9973110713294489, 78.31864583420048120 ) ) ;
#21850 = MECHANICAL_DESIGN_GEOMETRIC_PRESENTATION_REPRESENTATION (  '', ( #35052 ), #31397 ) ;
#21851 = VECTOR ( 'NONE', #34518, 1000.000000000000000 ) ;
#21852 = CARTESIAN_POINT ( 'NONE',  ( 0.000000000000000000, 0.000000000000000000, 0.000000000000000000 ) ) ;
#21853 = FACE_OUTER_BOUND ( 'NONE', #61028, .T. ) ;
#21854 = CARTESIAN_POINT ( 'NONE',  ( 10.00000000000000000, -29.81001611430991360, -22.74946021919165418 ) ) ;
#21855 = ORIENTED_EDGE ( 'NONE', *, *, #5278, .T. ) ;
#21856 = AXIS2_PLACEMENT_3D ( 'NONE', #45097, #37960, #33414 ) ;
#21857 = VERTEX_POINT ( 'NONE', #21954 ) ;
#21858 = CARTESIAN_POINT ( 'NONE',  ( 11.99999999999999822, -64.81221759200306565, -50.23322058963420034 ) ) ;
#21859 = CARTESIAN_POINT ( 'NONE',  ( -96.32499999999996021, -212.2949673200287179, 88.83583333333334053 ) ) ;
#21860 = CARTESIAN_POINT ( 'NONE',  ( -0.9515373497862389396, -96.47140937769621871, 5.500000000000000000 ) ) ;
#21861 = AXIS2_PLACEMENT_3D ( 'NONE', #15372, #37585, #55608 ) ;
#21862 = CARTESIAN_POINT ( 'NONE',  ( -97.30629616937501680, 88.66845928578038638, 80.80572916753382628 ) ) ;
#21863 = DIRECTION ( 'NONE',  ( -1.000000000000000000, 0.000000000000000000, 0.000000000000000000 ) ) ;
#21864 = DIRECTION ( 'NONE',  ( 0.000000000000000000, 0.000000000000000000, 1.000000000000000000 ) ) ;
#21865 = CIRCLE ( 'NONE', #30227, 16.00000000000000355 ) ;
#21866 = VERTEX_POINT ( 'NONE', #44900 ) ;
#21867 = CARTESIAN_POINT ( 'NONE',  ( -3.000000000000000000, -10.45096189432344147, 21.10159698893426494 ) ) ;
#21868 = AXIS2_PLACEMENT_3D ( 'NONE', #12282, #58518, #6296 ) ;
#21869 = LINE ( 'NONE', #66631, #6435 ) ;
#21870 = CARTESIAN_POINT ( 'NONE',  ( -24.50849501662245800, -109.8101191361138831, -5.500000000000000000 ) ) ;
#21871 = VECTOR ( 'NONE', #58447, 1000.000000000000000 ) ;
#21872 = CARTESIAN_POINT ( 'NONE',  ( 10.00000000000000000, 55.19960302592066625, 51.03279382321107249 ) ) ;
#21873 = CARTESIAN_POINT ( 'NONE',  ( 15.69955575015255533, 0.001194404164511398249, -70.60000000000039222 ) ) ;
#21874 = CYLINDRICAL_SURFACE ( 'NONE', #46027, 2.649999999999985700 ) ;
#21875 = CARTESIAN_POINT ( 'NONE',  ( -97.30629616937497417, -208.6684592857803011, 80.85864583420048746 ) ) ;
#21876 = DIRECTION ( 'NONE',  ( 0.000000000000000000, -0.9969173337331271867, -0.07845909572785568498 ) ) ;
#21877 = VERTEX_POINT ( 'NONE', #67822 ) ;
#21878 = CARTESIAN_POINT ( 'NONE',  ( 0.000000000000000000, -81.34940948281344220, 10.30890764327355846 ) ) ;
#21879 = CARTESIAN_POINT ( 'NONE',  ( 8.000000000000007105, 1.142349898368116708E-14, 6.370018489481387452E-15 ) ) ;
#21880 = DIRECTION ( 'NONE',  ( 0.000000000000000000, 0.000000000000000000, -1.000000000000000000 ) ) ;
#21881 = VERTEX_POINT ( 'NONE', #16318 ) ;
#21882 = LINE ( 'NONE', #45581, #43777 ) ;
#21883 = CARTESIAN_POINT ( 'NONE',  ( 0.000000000000000000, -31.47745569255189224, 68.26794271651249346 ) ) ;
#21884 = EDGE_CURVE ( 'NONE', #70651, #47514, #24417, .T. ) ;
#21885 = UNCERTAINTY_MEASURE_WITH_UNIT (LENGTH_MEASURE( 1.000000000000000082E-05 ), #65167, 'distance_accuracy_value', 'NONE');
#21886 = DIRECTION ( 'NONE',  ( -1.000000000000000000, 0.000000000000000000, 0.000000000000000000 ) ) ;
#21887 = ORIENTED_EDGE ( 'NONE', *, *, #49989, .T. ) ;
#21888 = EDGE_CURVE ( 'NONE', #13854, #64948, #190, .T. ) ;
#21889 = CARTESIAN_POINT ( 'NONE',  ( 0.000000000000000000, 77.49459641780886443, 0.8261519478433866359 ) ) ;
#21890 = DIRECTION ( 'NONE',  ( -1.000000000000000000, 0.000000000000000000, 0.000000000000000000 ) ) ;
#21891 = ORIENTED_EDGE ( 'NONE', *, *, #73389, .F. ) ;
#21892 = EDGE_CURVE ( 'NONE', #24265, #19617, #53123, .T. ) ;
#21893 = CARTESIAN_POINT ( 'NONE',  ( 93.84685191531251292, -211.9973110713294489, 88.47864583420047779 ) ) ;
#21894 = CARTESIAN_POINT ( 'NONE',  ( -97.64999999969889188, -209.9999754409357422, 87.53856274002470172 ) ) ;
#21895 = ORIENTED_EDGE ( 'NONE', *, *, #70274, .T. ) ;
#21896 = CARTESIAN_POINT ( 'NONE',  ( -10.00000000000000000, 0.000000000000000000, 0.000000000000000000 ) ) ;
#21897 = STYLED_ITEM ( 'NONE', ( #72835 ), #47128 ) ;
#21898 = ORIENTED_EDGE ( 'NONE', *, *, #29375, .T. ) ;
#21899 = CARTESIAN_POINT ( 'NONE',  ( -7.499999999999992895, 2.289750019674042456E-15, 0.000000000000000000 ) ) ;
#21900 = ORIENTED_EDGE ( 'NONE', *, *, #28793, .T. ) ;
#21901 = CYLINDRICAL_SURFACE ( 'NONE', #34669, 2.649999999999985700 ) ;
#21902 = CIRCLE ( 'NONE', #8707, 31.99999999999998579 ) ;
#21903 = ORIENTED_EDGE ( 'NONE', *, *, #13046, .T. ) ;
#21904 = VERTEX_POINT ( 'NONE', #18528 ) ;
#21905 = ORIENTED_EDGE ( 'NONE', *, *, #25273, .F. ) ;
#21906 = DIRECTION ( 'NONE',  ( -0.2079116908177587875, 1.197885328332318196E-16, -0.9781476007338056888 ) ) ;
#21907 = EDGE_CURVE ( 'NONE', #7440, #41355, #52985, .T. ) ;
#21908 = AXIS2_PLACEMENT_3D ( 'NONE', #30628, #369, #22898 ) ;
#21909 = ADVANCED_FACE ( 'NONE', ( #52372 ), #58387, .F. ) ;
#21910 = ORIENTED_EDGE ( 'NONE', *, *, #55555, .F. ) ;
#21911 = AXIS2_PLACEMENT_3D ( 'NONE', #16865, #46173, #39795 ) ;
#21912 = VERTEX_POINT ( 'NONE', #58770 ) ;
#21913 = CARTESIAN_POINT ( 'NONE',  ( 97.30629616937498838, 91.33154071421968467, 75.56697916753383026 ) ) ;
#21914 = DIRECTION ( 'NONE',  ( -1.000000000000000000, 0.000000000000000000, 0.000000000000000000 ) ) ;
#21915 = FACE_OUTER_BOUND ( 'NONE', #31687, .T. ) ;
#21916 = ORIENTED_EDGE ( 'NONE', *, *, #69707, .T. ) ;
#21917 = EDGE_LOOP ( 'NONE', ( #11030, #24788, #12591, #13743 ) ) ;
#21918 = ORIENTED_EDGE ( 'NONE', *, *, #36572, .T. ) ;
#21919 = CARTESIAN_POINT ( 'NONE',  ( 94.99999999999998579, 87.33691857156068750, 87.26156250086714294 ) ) ;
#21920 = CIRCLE ( 'NONE', #24391, 31.99999999999999645 ) ;
#21921 = ORIENTED_EDGE ( 'NONE', *, *, #13160, .F. ) ;
#21922 = CARTESIAN_POINT ( 'NONE',  ( 95.00000000000000000, -207.3369185715606307, 84.40406250086712703 ) ) ;
#21923 = EDGE_CURVE ( 'NONE', #18767, #58541, #29802, .T. ) ;
#21925 = EDGE_CURVE ( 'NONE', #73949, #33726, #47918, .T. ) ;
#21924 = AXIS2_PLACEMENT_3D ( 'NONE', #3848, #15101, #27112 ) ;
#21926 = DIRECTION ( 'NONE',  ( -5.551115123125782702E-17, 0.000000000000000000, -1.000000000000000000 ) ) ;
#21927 = DIRECTION ( 'NONE',  ( 0.2306669878475637314, 0.9730327541852493711, -0.000000000000000000 ) ) ;
#21928 = FACE_OUTER_BOUND ( 'NONE', #29749, .T. ) ;
#21929 = DIRECTION ( 'NONE',  ( 0.000000000000000000, 0.000000000000000000, 1.000000000000000000 ) ) ;
#21930 = DIRECTION ( 'NONE',  ( -1.000000000000000000, 0.000000000000000000, 0.000000000000000000 ) ) ;
#21931 = DIRECTION ( 'NONE',  ( 0.000000000000000000, 0.000000000000000000, 1.000000000000000000 ) ) ;
#21932 = FACE_OUTER_BOUND ( 'NONE', #47356, .T. ) ;
#21933 = CARTESIAN_POINT ( 'NONE',  ( -92.69370383062498320, -211.3315407142195852, 89.27239583420048064 ) ) ;
#21934 = CARTESIAN_POINT ( 'NONE',  ( -97.30629616937501680, 91.33154071421968467, 85.30364583420048064 ) ) ;
#21935 = ORIENTED_EDGE ( 'NONE', *, *, #38816, .T. ) ;
#21937 = CARTESIAN_POINT ( 'NONE',  ( -95.00000000000002842, 87.33691857156074434, 85.35656250086714181 ) ) ;
#21936 = CARTESIAN_POINT ( 'NONE',  ( 94.99999999999998579, 92.66308142843935514, 86.30906250086715659 ) ) ;
#21938 = ORIENTED_EDGE ( 'NONE', *, *, #57746, .T. ) ;
#21939 = DIRECTION ( 'NONE',  ( -1.000000000000000000, 0.000000000000000000, 0.000000000000000000 ) ) ;
#21940 = CARTESIAN_POINT ( 'NONE',  ( -97.64999999999996305, -209.9999999999999716, 80.55437500173430010 ) ) ;
#21941 = PLANE ( 'NONE',  #37962 ) ;
#21942 = DIRECTION ( 'NONE',  ( 0.000000000000000000, 0.000000000000000000, 1.000000000000000000 ) ) ;
#21943 = DIRECTION ( 'NONE',  ( 0.000000000000000000, 0.000000000000000000, 1.000000000000000000 ) ) ;
#21944 = CARTESIAN_POINT ( 'NONE',  ( 10.00000000000000000, 37.58145647212453611, 16.68533520207917675 ) ) ;
#21945 = CARTESIAN_POINT ( 'NONE',  ( 11.99999999999999822, 0.000000000000000000, 0.000000000000000000 ) ) ;
#21946 = DIRECTION ( 'NONE',  ( 0.000000000000000000, -0.8526401643540860720, -0.5224985647159590130 ) ) ;
#21947 = LINE ( 'NONE', #56159, #18013 ) ;
#21948 = ORIENTED_EDGE ( 'NONE', *, *, #26501, .T. ) ;
#21949 = EDGE_LOOP ( 'NONE', ( #16478, #69515, #581, #27750 ) ) ;
#21950 = CARTESIAN_POINT ( 'NONE',  ( -97.65000000000001990, 91.52997821335253548, 82.32708333333332007 ) ) ;
#21951 = CARTESIAN_POINT ( 'NONE',  ( -1.474095553543409487, -120.2775649455957989, -2.500000000000000000 ) ) ;
#21952 = CARTESIAN_POINT ( 'NONE',  ( 96.32499999999998863, -207.7050326799711968, 75.81833333333332803 ) ) ;
#21953 = CARTESIAN_POINT ( 'NONE',  ( 4.755015822784811164, -4.336808689942017736E-16, 0.000000000000000000 ) ) ;
#21954 = CARTESIAN_POINT ( 'NONE',  ( 0.000000000000000000, -2.543863470247813119, -81.96053171279905314 ) ) ;
#21955 = DIRECTION ( 'NONE',  ( 0.000000000000000000, 0.000000000000000000, -1.000000000000000000 ) ) ;
#21956 = LINE ( 'NONE', #33977, #48155 ) ;
#21957 = CARTESIAN_POINT ( 'NONE',  ( 10.00000000000000000, 5.202137450156907761, -37.22597642581151689 ) ) ;
#21958 = ORIENTED_EDGE ( 'NONE', *, *, #54155, .F. ) ;
#21959 = CARTESIAN_POINT ( 'NONE',  ( -95.00000000000002842, 92.66308142843932671, 80.59406250086715318 ) ) ;
#21960 = DIRECTION ( 'NONE',  ( 0.000000000000000000, 0.000000000000000000, 1.000000000000000000 ) ) ;
#21961 = DIRECTION ( 'NONE',  ( -1.000000000000000000, 0.000000000000000000, -0.000000000000000000 ) ) ;
#21962 = AXIS2_PLACEMENT_3D ( 'NONE', #11442, #17459, #4724 ) ;
#21963 = DIRECTION ( 'NONE',  ( 0.000000000000000000, 0.000000000000000000, 1.000000000000000000 ) ) ;
#21964 = CYLINDRICAL_SURFACE ( 'NONE', #69314, 31.99999999999998579 ) ;
#21965 = LINE ( 'NONE', #50536, #22083 ) ;
#21966 = CARTESIAN_POINT ( 'NONE',  ( -92.69370383062498320, -211.3315407142195852, 88.16114583420048234 ) ) ;
#21967 = ADVANCED_FACE ( 'NONE', ( #35813 ), #11765, .T. ) ;
#21968 = EDGE_CURVE ( 'NONE', #185, #72505, #68614, .T. ) ;
#21969 = ADVANCED_FACE ( 'NONE', ( #41469 ), #29428, .T. ) ;
#21970 = AXIS2_PLACEMENT_3D ( 'NONE', #11490, #5507, #28405 ) ;
#21971 = CARTESIAN_POINT ( 'NONE',  ( 94.99999999999998579, 87.33691857156068750, 81.70531250086715147 ) ) ;
#21972 = EDGE_CURVE ( 'NONE', #41089, #33185, #21797, .T. ) ;
#21973 = CARTESIAN_POINT ( 'NONE',  ( -96.15314808468745866, -211.9973110713294489, 79.74739583420048916 ) ) ;
#21974 = DIRECTION ( 'NONE',  ( -1.000000000000000000, -0.000000000000000000, 0.000000000000000000 ) ) ;
#21975 = VERTEX_POINT ( 'NONE', #34718 ) ;
#21976 = LINE ( 'NONE', #68219, #8871 ) ;
#21977 = DIRECTION ( 'NONE',  ( 0.000000000000000000, 0.7604059656000276002, 0.6494480483301876550 ) ) ;
#21978 = DIRECTION ( 'NONE',  ( -0.000000000000000000, -0.000000000000000000, -1.000000000000000000 ) ) ;
#21979 = AXIS2_PLACEMENT_3D ( 'NONE', #21380, #27399, #28515 ) ;
#21980 = VECTOR ( 'NONE', #1847, 1000.000000000000114 ) ;
#21981 = ADVANCED_FACE ( 'NONE', ( #64782 ), #13264, .T. ) ;
#21982 = CARTESIAN_POINT ( 'NONE',  ( -96.15314808468751551, 88.00268892867056536, 77.84239583420048803 ) ) ;
#21983 = CARTESIAN_POINT ( 'NONE',  ( 97.30629616937498838, -208.6684592857803011, 79.85322916753379729 ) ) ;
#21984 = ORIENTED_EDGE ( 'NONE', *, *, #12407, .T. ) ;
#21985 = CARTESIAN_POINT ( 'NONE',  ( -92.35000000000003695, 90.00000000000004263, 75.07749999999998636 ) ) ;
#21986 = ORIENTED_EDGE ( 'NONE', *, *, #34064, .T. ) ;
#21987 = ADVANCED_FACE ( 'NONE', ( #920 ), #23082, .F. ) ;
#21988 = LINE ( 'NONE', #17824, #44781 ) ;
#21989 = ORIENTED_EDGE ( 'NONE', *, *, #21311, .F. ) ;
#21990 = CARTESIAN_POINT ( 'NONE',  ( -6.938893903907228378E-15, 80.00000000000000000, -110.0000000000000000 ) ) ;
#21991 = ORIENTED_EDGE ( 'NONE', *, *, #1495, .T. ) ;
#21992 = ORIENTED_EDGE ( 'NONE', *, *, #46120, .T. ) ;
#21993 = VERTEX_POINT ( 'NONE', #18168 ) ;
#21994 = LINE ( 'NONE', #27998, #68339 ) ;
#21995 = ADVANCED_FACE ( 'NONE', ( #23445 ), #41111, .T. ) ;
#21996 = EDGE_CURVE ( 'NONE', #16108, #67978, #43405, .T. ) ;
#21997 = EDGE_LOOP ( 'NONE', ( #69555, #69360, #42248, #39610 ) ) ;
#21998 = CARTESIAN_POINT ( 'NONE',  ( -10.00000000000000000, 0.000000000000000000, 0.000000000000000000 ) ) ;
#21999 = CIRCLE ( 'NONE', #12387, 2.650000000000540812 ) ;
#22000 = DIRECTION ( 'NONE',  ( -0.000000000000000000, -0.000000000000000000, 1.000000000000000000 ) ) ;
#22001 =( BOUNDED_CURVE ( )  B_SPLINE_CURVE ( 2, ( #41918, #11487, #46828, #40432, #23514, #64119, #12955, #24621, #46447 ),
 .UNSPECIFIED., .F., .F. ) 
 B_SPLINE_CURVE_WITH_KNOTS ( ( 3, 2, 2, 2, 3 ),
 ( 0.6561861948910820974, 0.6632419608429419577, 0.6702977263838236777, 0.6773534919247052866, 0.6773535682752289677 ),
 .UNSPECIFIED. ) 
 CURVE ( )  GEOMETRIC_REPRESENTATION_ITEM ( )  RATIONAL_B_SPLINE_CURVE ( ( 1.000000000000000000, 0.8660254037844387076, 1.000000000000000000, 0.8660254037844387076, 1.000000000000000000, 0.8660254037844387076, 1.000000000000000000, 0.9999985502592857456, 0.9999971005499468379 ) ) 
 REPRESENTATION_ITEM ( '' )  );
#22002 = CARTESIAN_POINT ( 'NONE',  ( 97.30629616937498838, 90.00000000000002842, 87.57906250086715261 ) ) ;
#22003 = FACE_OUTER_BOUND ( 'NONE', #47334, .T. ) ;
#22004 = CARTESIAN_POINT ( 'NONE',  ( 92.35000000000002274, -208.4700217866474645, 76.61208333333333087 ) ) ;
#22005 = ORIENTED_EDGE ( 'NONE', *, *, #27975, .F. ) ;
#22006 = AXIS2_PLACEMENT_3D ( 'NONE', #20447, #25350, #72311 ) ;
#22007 = EDGE_LOOP ( 'NONE', ( #53301, #18046, #56551, #72572 ) ) ;
#22008 = ORIENTED_EDGE ( 'NONE', *, *, #63001, .T. ) ;
#22009 = VERTEX_POINT ( 'NONE', #26018 ) ;
#22010 = CARTESIAN_POINT ( 'NONE',  ( 97.64999999999990621, -208.4700217866474361, 89.10041666666667481 ) ) ;
#22011 = VECTOR ( 'NONE', #26235, 1000.000000000000000 ) ;
#22012 = CARTESIAN_POINT ( 'NONE',  ( 10.00000000000000000, 12.42422080174688404, -35.38097989696498047 ) ) ;
#22013 = LINE ( 'NONE', #56980, #54283 ) ;
#22014 = DIRECTION ( 'NONE',  ( -1.000000000000000000, 0.000000000000000000, 0.000000000000000000 ) ) ;
#22015 = CARTESIAN_POINT ( 'NONE',  ( -12.74999999999739941, -119.9999999999949267, -65.00000000000034106 ) ) ;
#22016 = CARTESIAN_POINT ( 'NONE',  ( 0.000000000000000000, -20.41045688087772092, -72.35160999960838524 ) ) ;
#22017 = ORIENTED_EDGE ( 'NONE', *, *, #42840, .F. ) ;
#22018 = CARTESIAN_POINT ( 'NONE',  ( -97.64999999999994884, -211.5299782133524502, 81.87729166840097150 ) ) ;
#22019 = ORIENTED_EDGE ( 'NONE', *, *, #23636, .F. ) ;
#22020 = DIRECTION ( 'NONE',  ( -1.000000000000000000, -0.000000000000000000, -0.000000000000000000 ) ) ;
#22021 = ORIENTED_EDGE ( 'NONE', *, *, #42953, .T. ) ;
#22023 = CARTESIAN_POINT ( 'NONE',  ( -95.00000000000002842, 86.94004357329504273, 83.25312500173430408 ) ) ;
#22022 = CARTESIAN_POINT ( 'NONE',  ( 92.34999999999999432, 91.52997821335252127, 83.04145833506763097 ) ) ;
#22024 = VECTOR ( 'NONE', #59264, 1000.000000000000000 ) ;
#22025 = ORIENTED_EDGE ( 'NONE', *, *, #2418, .T. ) ;
#22026 = CARTESIAN_POINT ( 'NONE',  ( 97.30629616937498838, 91.33154071421968467, 83.82197916753382572 ) ) ;
#22027 = VECTOR ( 'NONE', #57033, 1000.000000000000000 ) ;
#22028 = CARTESIAN_POINT ( 'NONE',  ( 0.000000000000000000, 63.97538442413498672, -51.29473840253155714 ) ) ;
#22029 = CARTESIAN_POINT ( 'NONE',  ( -97.64999999950704535, 89.99996796756893502, 85.63541623677065218 ) ) ;
#22030 = PLANE ( 'NONE',  #13378 ) ;
#22031 = DIRECTION ( 'NONE',  ( -1.000000000000000000, -0.000000000000000000, 0.000000000000000000 ) ) ;
#22032 = CARTESIAN_POINT ( 'NONE',  ( 96.32499999999997442, 92.29496732002878900, 87.88333333333332575 ) ) ;
#22033 = ORIENTED_EDGE ( 'NONE', *, *, #54305, .F. ) ;
#22034 = CARTESIAN_POINT ( 'NONE',  ( -92.35000000000003695, 89.99999997928479445, 80.87187500099602744 ) ) ;
#22036 = DIRECTION ( 'NONE',  ( 0.000000000000000000, -0.9510565162951565288, 0.3090169943749382919 ) ) ;
#22035 = AXIS2_PLACEMENT_3D ( 'NONE', #39733, #5527, #22815 ) ;
#22037 = VECTOR ( 'NONE', #3043, 1000.000000000000000 ) ;
#22038 = VECTOR ( 'NONE', #62682, 1000.000000000000114 ) ;
#22039 = CARTESIAN_POINT ( 'NONE',  ( 26.09152095774781799, -124.8716048804687375, 5.500000000000000000 ) ) ;
#22040 = ORIENTED_EDGE ( 'NONE', *, *, #21213, .F. ) ;
#22041 = VERTEX_POINT ( 'NONE', #25655 ) ;
#22042 = EDGE_CURVE ( 'NONE', #58064, #16194, #59884, .T. ) ;
#22043 = DIRECTION ( 'NONE',  ( -1.000000000000000000, 0.000000000000000000, -0.000000000000000000 ) ) ;
#22044 = CARTESIAN_POINT ( 'NONE',  ( -97.65000000000001990, 90.00000000000004263, 90.00000000000000000 ) ) ;
#22045 = DIRECTION ( 'NONE',  ( 0.000000000000000000, 0.000000000000000000, 1.000000000000000000 ) ) ;
#22046 = CARTESIAN_POINT ( 'NONE',  ( -97.30629616937495996, -209.9999999999999716, 82.18156250086715886 ) ) ;
#22047 = ORIENTED_EDGE ( 'NONE', *, *, #54427, .F. ) ;
#22048 = CARTESIAN_POINT ( 'NONE',  ( -235.0000123116479926, -123.0000000000000284, 2.500000000000000000 ) ) ;
#22049 = EDGE_LOOP ( 'NONE', ( #54563, #43345, #50477, #50571 ) ) ;
#22050 = AXIS2_PLACEMENT_3D ( 'NONE', #21352, #61982, #10090 ) ;
#22051 = CARTESIAN_POINT ( 'NONE',  ( -96.32499999999996021, -212.2949673200287179, 77.48520833506763950 ) ) ;
#22052 = CARTESIAN_POINT ( 'NONE',  ( 92.35000000006144205, 90.00001182123735077, 81.82400613091868991 ) ) ;
#22053 = CARTESIAN_POINT ( 'NONE',  ( 0.000000000000000000, 68.27212725128275395, -31.46837873495001503 ) ) ;
#22054 = PLANE ( 'NONE',  #40441 ) ;
#22055 = CARTESIAN_POINT ( 'NONE',  ( 10.00000000000000000, 0.000000000000000000, 0.000000000000000000 ) ) ;
#22056 = DIRECTION ( 'NONE',  ( 0.000000000000000000, -0.9238795325112906243, 0.3826834323650805669 ) ) ;
#22057 = ADVANCED_FACE ( 'NONE', ( #37688 ), #37322, .T. ) ;
#22058 = CARTESIAN_POINT ( 'NONE',  ( 0.000000000000000000, -120.0000000000000000, 2.500000000000000000 ) ) ;
#22059 = DIRECTION ( 'NONE',  ( -1.000000000000000000, 0.000000000000000000, 0.000000000000000000 ) ) ;
#22060 = CARTESIAN_POINT ( 'NONE',  ( -2.499999999999992895, 7.589415207398510330E-16, 0.000000000000000000 ) ) ;
#22061 = EDGE_CURVE ( 'NONE', #9567, #23150, #3484, .T. ) ;
#22062 = CYLINDRICAL_SURFACE ( 'NONE', #51370, 31.99999999999998579 ) ;
#22063 = AXIS2_PLACEMENT_3D ( 'NONE', #37428, #43065, #38526 ) ;
#22064 = DIRECTION ( 'NONE',  ( -0.000000000000000000, -0.6691306063588670083, -0.7431448254773863615 ) ) ;
#22065 = CARTESIAN_POINT ( 'NONE',  ( 10.00000000000000000, -55.38113227695820484, 54.21277698773656084 ) ) ;
#22066 = CIRCLE ( 'NONE', #5288, 11.59999999999999787 ) ;
#22067 = ADVANCED_FACE ( 'NONE', ( #71873 ), #48223, .T. ) ;
#22068 = CARTESIAN_POINT ( 'NONE',  ( -94.99999999999997158, -207.3369185715606307, 89.64281250086715147 ) ) ;
#22069 = CARTESIAN_POINT ( 'NONE',  ( 0.000000000000000000, 0.000000000000000000, 0.000000000000000000 ) ) ;
#22070 = ORIENTED_EDGE ( 'NONE', *, *, #70430, .F. ) ;
#22071 = EDGE_CURVE ( 'NONE', #59943, #24232, #20388, .T. ) ;
#22072 = DIRECTION ( 'NONE',  ( 1.000000000000000000, 0.000000000000000000, 0.000000000000000000 ) ) ;
#22073 = CARTESIAN_POINT ( 'NONE',  ( -96.15314808468751551, 88.00268892867056536, 78.95364583420047211 ) ) ;
#22074 = AXIS2_PLACEMENT_3D ( 'NONE', #12281, #52138, #35582 ) ;
#22075 = CARTESIAN_POINT ( 'NONE',  ( 93.84685191531249870, -208.0026889286704943, 89.53697916753381492 ) ) ;
#22076 = ORIENTED_EDGE ( 'NONE', *, *, #4899, .F. ) ;
#22077 = VECTOR ( 'NONE', #30496, 1000.000000000000000 ) ;
#22078 = CARTESIAN_POINT ( 'NONE',  ( 92.35000000000000853, -211.5299782133524218, 79.97229166840095615 ) ) ;
#22080 = CARTESIAN_POINT ( 'NONE',  ( 97.65000000000009095, 88.47002178664759242, 83.27958333333332064 ) ) ;
#22079 = AXIS2_PLACEMENT_3D ( 'NONE', #30202, #24213, #58041 ) ;
#22081 = EDGE_CURVE ( 'NONE', #11565, #14594, #60621, .T. ) ;
#22082 = CARTESIAN_POINT ( 'NONE',  ( -97.64999999999996305, -209.9999999999999716, 90.00000000000000000 ) ) ;
#22083 = VECTOR ( 'NONE', #5441, 1000.000000000000000 ) ;
#22084 = CARTESIAN_POINT ( 'NONE',  ( 11.99999999999999822, -6.903761155838323837, 77.19088730480521576 ) ) ;
#22085 = VECTOR ( 'NONE', #2314, 1000.000000000000000 ) ;
#22086 = CARTESIAN_POINT ( 'NONE',  ( 92.69370383062501162, -208.6684592857803011, 76.41364583420049428 ) ) ;
#22087 = EDGE_LOOP ( 'NONE', ( #34154, #61338, #53199, #19775 ) ) ;
#22088 = ORIENTED_EDGE ( 'NONE', *, *, #21705, .T. ) ;
#22089 = EDGE_CURVE ( 'NONE', #3728, #29240, #20725, .T. ) ;
#22090 = CARTESIAN_POINT ( 'NONE',  ( 0.000000000000000000, 0.000000000000000000, 0.000000000000000000 ) ) ;
#22091 = CARTESIAN_POINT ( 'NONE',  ( 0.000000000000000000, 14.67089635893819377, -73.72996012237423713 ) ) ;
#22092 = CARTESIAN_POINT ( 'NONE',  ( 0.000000000000000000, 0.8261519478441983200, -77.49459641780885022 ) ) ;
#22093 = DIRECTION ( 'NONE',  ( 0.000000000000000000, 0.7431448254773954654, 0.6691306063588569053 ) ) ;
#22094 = EDGE_CURVE ( 'NONE', #37728, #13957, #43343, .T. ) ;
#22095 = CARTESIAN_POINT ( 'NONE',  ( 93.67500000000001137, -212.2949673200287179, 81.93020833506763267 ) ) ;
#22096 = CARTESIAN_POINT ( 'NONE',  ( 97.64999999999997726, -208.4700217866474645, 89.10041666666667481 ) ) ;
#22097 = AXIS2_PLACEMENT_3D ( 'NONE', #4658, #56140, #34315 ) ;
#22098 = ORIENTED_EDGE ( 'NONE', *, *, #49828, .F. ) ;
#22099 = CARTESIAN_POINT ( 'NONE',  ( 95.00000000000000000, -209.9999999999999716, 73.40771935957695860 ) ) ;
#22100 = VERTEX_POINT ( 'NONE', #19269 ) ;
#22101 = EDGE_LOOP ( 'NONE', ( #38842, #24056, #62946, #19273 ) ) ;
#22102 = LINE ( 'NONE', #10071, #72976 ) ;
#22103 = CARTESIAN_POINT ( 'NONE',  ( 11.99999999999999822, -65.59268652807183742, -36.72794159290312166 ) ) ;
#22104 = ORIENTED_EDGE ( 'NONE', *, *, #47855, .F. ) ;
#22105 = CARTESIAN_POINT ( 'NONE',  ( 3.000000000000000000, -2.935248768560059673, 2.602085213965210642E-15 ) ) ;
#22106 = CARTESIAN_POINT ( 'NONE',  ( 92.35000000000002274, -208.4700217866474645, 77.32645833506762756 ) ) ;
#22107 = CARTESIAN_POINT ( 'NONE',  ( 92.34999999999999432, 88.47002178664753558, 81.16291666666666060 ) ) ;
#22108 = VERTEX_POINT ( 'NONE', #65520 ) ;
#22109 = LINE ( 'NONE', #56329, #43151 ) ;
#22110 = ORIENTED_EDGE ( 'NONE', *, *, #58000, .T. ) ;
#22111 = CARTESIAN_POINT ( 'NONE',  ( 10.00000000000000000, 36.72794159290334903, -65.59268652807170952 ) ) ;
#22112 = AXIS2_PLACEMENT_3D ( 'NONE', #49859, #37496, #32570 ) ;
#22113 = ORIENTED_EDGE ( 'NONE', *, *, #31067, .F. ) ;
#22114 = DIRECTION ( 'NONE',  ( -1.000000000000000000, -0.000000000000000000, 0.000000000000000000 ) ) ;
#22115 = CARTESIAN_POINT ( 'NONE',  ( -93.84685191531254134, 91.99731107132950569, 85.77989583420048803 ) ) ;
#22116 = CARTESIAN_POINT ( 'NONE',  ( 92.69370383062498320, 91.33154071421968467, 77.52489583420046415 ) ) ;
#22117 = ORIENTED_EDGE ( 'NONE', *, *, #25570, .T. ) ;
#22118 = FACE_OUTER_BOUND ( 'NONE', #46049, .T. ) ;
#22119 = VECTOR ( 'NONE', #18183, 1000.000000000000000 ) ;
#22120 = LINE ( 'NONE', #28122, #8847 ) ;
#22121 = DIRECTION ( 'NONE',  ( 0.000000000000000000, 0.000000000000000000, 1.000000000000000000 ) ) ;
#22122 = FACE_OUTER_BOUND ( 'NONE', #2021, .T. ) ;
#22123 = ORIENTED_EDGE ( 'NONE', *, *, #42950, .F. ) ;
#22124 = CARTESIAN_POINT ( 'NONE',  ( 10.00000000000000000, 12.42422080174688404, -35.38097989696498047 ) ) ;
#22125 = CARTESIAN_POINT ( 'NONE',  ( -93.84685191531248449, -208.0026889286704943, 79.27114583420046756 ) ) ;
#22126 = VECTOR ( 'NONE', #48174, 1000.000000000000000 ) ;
#22127 = ORIENTED_EDGE ( 'NONE', *, *, #51883, .F. ) ;
#22128 = ORIENTED_EDGE ( 'NONE', *, *, #30474, .T. ) ;
#22129 = PLANE ( 'NONE',  #48122 ) ;
#22130 = ORIENTED_EDGE ( 'NONE', *, *, #69699, .F. ) ;
#22131 = DIRECTION ( 'NONE',  ( 0.000000000000000000, -0.5000000000000003331, 0.8660254037844383745 ) ) ;
#22132 = EDGE_CURVE ( 'NONE', #52748, #31332, #72357, .T. ) ;
#22133 = VECTOR ( 'NONE', #32251, 1000.000000000000000 ) ;
#22134 = DIRECTION ( 'NONE',  ( 0.000000000000000000, 0.000000000000000000, -1.000000000000000000 ) ) ;
#22135 = ORIENTED_EDGE ( 'NONE', *, *, #33894, .F. ) ;
#22136 = CARTESIAN_POINT ( 'NONE',  ( -97.30629616937497417, -208.6684592857803011, 89.74864583420048803 ) ) ;
#22137 = ORIENTED_EDGE ( 'NONE', *, *, #36168, .F. ) ;
#22138 = AXIS2_PLACEMENT_3D ( 'NONE', #60191, #3418, #53782 ) ;
#22139 = CARTESIAN_POINT ( 'NONE',  ( 10.00000000000000000, -10.74501242461258244, -35.92658777277521409 ) ) ;
#22140 = LINE ( 'NONE', #38692, #63308 ) ;
#22141 = DIRECTION ( 'NONE',  ( -1.000000000000000000, 0.000000000000000000, 0.000000000000000000 ) ) ;
#22142 = CARTESIAN_POINT ( 'NONE',  ( -92.34999999999999432, -208.4700217866474645, 89.17979166840096639 ) ) ;
#22143 = CARTESIAN_POINT ( 'NONE',  ( -3.000000000000000000, -18.13022148937243472, -15.02647892043568767 ) ) ;
#22144 = AXIS2_PLACEMENT_3D ( 'NONE', #47495, #25306, #48234 ) ;
#22145 = CIRCLE ( 'NONE', #24555, 31.99999999999998934 ) ;
#22146 = ADVANCED_FACE ( 'NONE', ( #31654 ), #14737, .F. ) ;
#22147 = LINE ( 'NONE', #5247, #27718 ) ;
#22148 = CARTESIAN_POINT ( 'NONE',  ( 94.99999999999998579, 87.33691857156068750, 83.45156250086714067 ) ) ;
#22149 = DIRECTION ( 'NONE',  ( 0.000000000000000000, 0.000000000000000000, 1.000000000000000000 ) ) ;
#22150 = DIRECTION ( 'NONE',  ( 0.000000000000000000, 0.000000000000000000, 1.000000000000000000 ) ) ;
#22151 = EDGE_CURVE ( 'NONE', #26342, #50832, #55395, .T. ) ;
#22152 = CIRCLE ( 'NONE', #72560, 31.99999999999999289 ) ;
#22153 = CARTESIAN_POINT ( 'NONE',  ( 93.67500000000001137, -207.7050326799711968, 86.71916666666666629 ) ) ;
#22154 = DIRECTION ( 'NONE',  ( 0.1850432970638682395, -0.9827303690289279636, 0.000000000000000000 ) ) ;
#22155 = CARTESIAN_POINT ( 'NONE',  ( 0.000000000000000000, 63.18004540533029001, 44.88180994100398635 ) ) ;
#22156 = CARTESIAN_POINT ( 'NONE',  ( 3.035766082959412415E-15, 5.773502691896260863, -2.080000000000000071 ) ) ;
#22157 = DIRECTION ( 'NONE',  ( 0.000000000000000000, -0.6691306063588586817, 0.7431448254773939111 ) ) ;
#22158 = CIRCLE ( 'NONE', #40195, 77.49900000000000944 ) ;
#22159 = DIRECTION ( 'NONE',  ( -1.000000000000000000, 0.000000000000000000, 0.000000000000000000 ) ) ;
#22160 = FACE_OUTER_BOUND ( 'NONE', #18664, .T. ) ;
#22161 = VECTOR ( 'NONE', #18685, 1000.000000000000000 ) ;
#22162 = EDGE_CURVE ( 'NONE', #68158, #34606, #65014, .T. ) ;
#22163 = CARTESIAN_POINT ( 'NONE',  ( -95.00000000000002842, 92.66308142843932671, 89.48406250086713953 ) ) ;
#22164 = DIRECTION ( 'NONE',  ( -1.000000000000000000, 0.000000000000000000, 0.000000000000000000 ) ) ;
#22165 = CARTESIAN_POINT ( 'NONE',  ( -97.64999999999996305, -209.9999999999999716, 85.55499999999999261 ) ) ;
#22166 = DIRECTION ( 'NONE',  ( 0.000000000000000000, -0.7604059656000228262, -0.6494480483301932061 ) ) ;
#22167 = EDGE_CURVE ( 'NONE', #74246, #8203, #36189, .T. ) ;
#22168 = CARTESIAN_POINT ( 'NONE',  ( 11.41210121379328335, -99.40233154247455616, 2.500000000000000000 ) ) ;
#22169 = EDGE_CURVE ( 'NONE', #26809, #70270, #20751, .T. ) ;
#22170 = CARTESIAN_POINT ( 'NONE',  ( -0.0004442498525516064278, 0.001194404164626844313, -64.00000000000000000 ) ) ;
#22171 = FILL_AREA_STYLE ('',( #9771 ) ) ;
#22172 = LINE ( 'NONE', #10140, #34201 ) ;
#22173 = ADVANCED_FACE ( 'NONE', ( #13626 ), #9778, .T. ) ;
#22174 = VECTOR ( 'NONE', #23671, 1000.000000000000000 ) ;
#22175 = CARTESIAN_POINT ( 'NONE',  ( 97.30629616937498838, -211.3315407142195852, 86.25614583420048120 ) ) ;
#22176 = EDGE_LOOP ( 'NONE', ( #16734, #36277, #30289, #36808 ) ) ;
#22177 = ORIENTED_EDGE ( 'NONE', *, *, #67148, .T. ) ;
#22178 = EDGE_CURVE ( 'NONE', #10732, #12767, #19384, .T. ) ;
#22179 = SURFACE_SIDE_STYLE ('',( #56404 ) ) ;
#22180 = ORIENTED_EDGE ( 'NONE', *, *, #52963, .T. ) ;
#22181 = CARTESIAN_POINT ( 'NONE',  ( -42.50000000000000000, 1.530808498934191521E-15, 12.50000000000000000 ) ) ;
#22182 = CARTESIAN_POINT ( 'NONE',  ( 97.30629616937498838, -208.6684592857803295, 76.67822916753378593 ) ) ;
#22183 = VECTOR ( 'NONE', #45864, 1000.000000000000000 ) ;
#22184 = ORIENTED_EDGE ( 'NONE', *, *, #56794, .T. ) ;
#22185 = AXIS2_PLACEMENT_3D ( 'NONE', #15164, #67418, #16281 ) ;
#22186 = CARTESIAN_POINT ( 'NONE',  ( 92.69370383062501162, -209.9999999999999716, 84.08656250086716000 ) ) ;
#22187 = EDGE_LOOP ( 'NONE', ( #8531, #61499, #54122, #37565 ) ) ;
#22188 = FACE_OUTER_BOUND ( 'NONE', #3, .T. ) ;
#22189 = VERTEX_POINT ( 'NONE', #14376 ) ;
#22190 = VECTOR ( 'NONE', #73747, 1000.000000000000000 ) ;
#22191 = ORIENTED_EDGE ( 'NONE', *, *, #19832, .T. ) ;
#22192 = CARTESIAN_POINT ( 'NONE',  ( -92.34999999999999432, -209.9999999999999716, 77.61749999999999261 ) ) ;
#22193 = DIRECTION ( 'NONE',  ( -1.000000000000000000, 0.000000000000000000, 0.000000000000000000 ) ) ;
#22194 = EDGE_LOOP ( 'NONE', ( #61683, #8697, #49632, #37501 ) ) ;
#22195 = LINE ( 'NONE', #15816, #64155 ) ;
#22196 = CARTESIAN_POINT ( 'NONE',  ( 0.000000000000000000, -30.80686688396994910, -21.53537804866113703 ) ) ;
#22197 = ORIENTED_EDGE ( 'NONE', *, *, #15275, .T. ) ;
#22198 = DIRECTION ( 'NONE',  ( 0.9038112904824853189, -0.4279312458752977388, 0.000000000000000000 ) ) ;
#22199 = CIRCLE ( 'NONE', #39001, 31.99999999999998224 ) ;
#22200 = ORIENTED_EDGE ( 'NONE', *, *, #69530, .T. ) ;
#22201 = CARTESIAN_POINT ( 'NONE',  ( 10.00000000000000000, 37.01155633439068282, -6.555932627142014191 ) ) ;
#22202 = ORIENTED_EDGE ( 'NONE', *, *, #1849, .T. ) ;
#22203 = VECTOR ( 'NONE', #41182, 1000.000000000000000 ) ;
#22204 = ORIENTED_EDGE ( 'NONE', *, *, #64439, .T. ) ;
#22205 = ORIENTED_EDGE ( 'NONE', *, *, #38301, .T. ) ;
#22206 = CARTESIAN_POINT ( 'NONE',  ( 96.15314808468748708, -208.0026889286704943, 76.73114583420047552 ) ) ;
#22207 = ITEM_DEFINED_TRANSFORMATION ( 'NONE', 'NONE', #24376,  #43395 ) ;
#22208 = DIRECTION ( 'NONE',  ( 0.5200609990132993854, 0.8541291221503274356, 0.000000000000000000 ) ) ;
#22209 = VERTEX_POINT ( 'NONE', #3126 ) ;
#22210 = VERTEX_POINT ( 'NONE', #28236 ) ;
#22211 = ORIENTED_EDGE ( 'NONE', *, *, #38465, .T. ) ;
#22212 = CARTESIAN_POINT ( 'NONE',  ( 0.000000000000000000, 5.202137450156907761, -37.22597642581151689 ) ) ;
#22213 = CARTESIAN_POINT ( 'NONE',  ( -3.000000000000000000, -23.29833615347109443, 3.418703333116492438 ) ) ;
#22214 = CARTESIAN_POINT ( 'NONE',  ( -96.15314808468751551, 88.00268892867056536, 76.57239583420049200 ) ) ;
#22215 = ORIENTED_EDGE ( 'NONE', *, *, #32917, .F. ) ;
#22216 = CARTESIAN_POINT ( 'NONE',  ( 94.99999999999998579, 92.66308142843935514, 75.51406250086714067 ) ) ;
#22217 = AXIS2_PLACEMENT_3D ( 'NONE', #61562, #26220, #19835 ) ;
#22218 =( BOUNDED_CURVE ( )  B_SPLINE_CURVE ( 2, ( #69191, #40619, #73702, #78, #34596, #22971, #17313 ),
 .UNSPECIFIED., .F., .F. ) 
 B_SPLINE_CURVE_WITH_KNOTS ( ( 3, 2, 2, 3 ),
 ( 0.8958333333333331483, 0.9027777777777775681, 0.9097222222222218768, 0.9166666666666662966 ),
 .UNSPECIFIED. ) 
 CURVE ( )  GEOMETRIC_REPRESENTATION_ITEM ( )  RATIONAL_B_SPLINE_CURVE ( ( 1.000000000000004219, 0.8660254037844343777, 1.000000000000000000, 0.8660254037844387076, 1.000000000000000000, 0.8660254037844451469, 0.9999999999999935607 ) ) 
 REPRESENTATION_ITEM ( '' )  );
#22219 = ORIENTED_EDGE ( 'NONE', *, *, #62316, .F. ) ;
#22220 = CARTESIAN_POINT ( 'NONE',  ( -94.99999999999997158, -207.3369185715606307, 87.57906250086713840 ) ) ;
#22221 = VERTEX_POINT ( 'NONE', #56833 ) ;
#22222 = CARTESIAN_POINT ( 'NONE',  ( 10.00000000000000000, 25.88420570971400991, 27.13269053701105449 ) ) ;
#22223 = DIRECTION ( 'NONE',  ( -1.343011723336883198E-16, 1.000000000000000000, 0.000000000000000000 ) ) ;
#22224 = DIRECTION ( 'NONE',  ( 0.000000000000000000, 0.3826834323650904479, -0.9238795325112865164 ) ) ;
#22225 = CARTESIAN_POINT ( 'NONE',  ( -93.84685191531248449, -208.0026889286704943, 79.90614583420047268 ) ) ;
#22226 = EDGE_CURVE ( 'NONE', #63342, #56025, #6203, .T. ) ;
#22227 = EDGE_CURVE ( 'NONE', #33646, #24236, #44630, .T. ) ;
#22228 = DIRECTION ( 'NONE',  ( 0.000000000000000000, -1.000000000000000000, -1.047444401652940007E-14 ) ) ;
#22229 = LINE ( 'NONE', #27486, #58366 ) ;
#22230 = CARTESIAN_POINT ( 'NONE',  ( -0.0004442498508594591917, 0.001194404164628348752, -65.00000000000000000 ) ) ;
#22231 = ADVANCED_FACE ( 'NONE', ( #67356 ), #61358, .T. ) ;
#22232 = ORIENTED_EDGE ( 'NONE', *, *, #27848, .F. ) ;
#22233 = CARTESIAN_POINT ( 'NONE',  ( -97.65000000000001990, 90.00000929204281874, 84.99937468035460597 ) ) ;
#22234 = ADVANCED_FACE ( 'NONE', ( #66979, #3853 ), #15105, .F. ) ;
#22235 = CYLINDRICAL_SURFACE ( 'NONE', #63965, 11.59999999999999787 ) ;
#22236 = DIRECTION ( 'NONE',  ( 0.000000000000000000, 0.3826834323650907810, -0.9238795325112864054 ) ) ;
#22237 = CARTESIAN_POINT ( 'NONE',  ( -92.69370383062504004, 90.00000000000004263, 81.70531250086713726 ) ) ;
#22238 = DIRECTION ( 'NONE',  ( -1.000000000000000000, -0.000000000000000000, -0.000000000000000000 ) ) ;
#22239 = DIRECTION ( 'NONE',  ( 1.000000000000000000, 0.000000000000000000, 0.000000000000000000 ) ) ;
#22240 = EDGE_CURVE ( 'NONE', #46961, #57093, #56594, .T. ) ;
#22241 = AXIS2_PLACEMENT_3D ( 'NONE', #52843, #64132, #7354 ) ;
#22242 = EDGE_LOOP ( 'NONE', ( #2520, #32574, #56191, #639 ) ) ;
#22243 = VECTOR ( 'NONE', #28032, 1000.000000000000000 ) ;
#22244 = DIRECTION ( 'NONE',  ( -0.000000000000000000, -0.000000000000000000, -1.000000000000000000 ) ) ;
#22246 = LINE ( 'NONE', #72253, #28086 ) ;
#22245 = AXIS2_PLACEMENT_3D ( 'NONE', #19838, #13092, #59341 ) ;
#22247 = CARTESIAN_POINT ( 'NONE',  ( 15.07208474345548055, -141.7963818439230010, 2.500000000000000000 ) ) ;
#22248 = DIRECTION ( 'NONE',  ( -1.000000000000000000, 0.000000000000000000, -0.000000000000000000 ) ) ;
#22249 = CARTESIAN_POINT ( 'NONE',  ( 3.035766082959412415E-15, 5.773502691896260863, -2.080000000000000071 ) ) ;
#22250 = CYLINDRICAL_SURFACE ( 'NONE', #5360, 77.49899999999999523 ) ;
#22251 = CARTESIAN_POINT ( 'NONE',  ( -96.15314808468745866, -211.9973110713294489, 81.01739583420049939 ) ) ;
#22252 = AXIS2_PLACEMENT_3D ( 'NONE', #56743, #28144, #45836 ) ;
#22253 = CYLINDRICAL_SURFACE ( 'NONE', #58472, 2.649999999999985700 ) ;
#22254 = ORIENTED_EDGE ( 'NONE', *, *, #8517, .F. ) ;
#22255 = CARTESIAN_POINT ( 'NONE',  ( 0.000000000000000000, 0.000000000000000000, 0.000000000000000000 ) ) ;
#22256 = CIRCLE ( 'NONE', #64288, 32.00000000000000000 ) ;
#22257 = DIRECTION ( 'NONE',  ( 0.000000000000000000, 0.000000000000000000, 1.000000000000000000 ) ) ;
#22258 = LINE ( 'NONE', #6096, #5753 ) ;
#22259 = ORIENTED_EDGE ( 'NONE', *, *, #9994, .T. ) ;
#22260 = CARTESIAN_POINT ( 'NONE',  ( 10.00000000000000000, 35.47612816024523141, 22.48208911017513145 ) ) ;
#22261 = DIRECTION ( 'NONE',  ( 0.000000000000000000, -0.9969173337331271867, -0.07845909572785571273 ) ) ;
#22262 = ADVANCED_FACE ( 'NONE', ( #16592 ), #74102, .T. ) ;
#22263 = EDGE_CURVE ( 'NONE', #72991, #43856, #68779, .T. ) ;
#22264 = VECTOR ( 'NONE', #44156, 1000.000000000000000 ) ;
#22265 = LINE ( 'NONE', #55731, #54006 ) ;
#22266 = ORIENTED_EDGE ( 'NONE', *, *, #63237, .T. ) ;
#22267 = CARTESIAN_POINT ( 'NONE',  ( 0.000000000000000000, 35.91791733033476675, 68.67312586195008350 ) ) ;
#22268 = EDGE_CURVE ( 'NONE', #70465, #69052, #73355, .T. ) ;
#22269 = DIRECTION ( 'NONE',  ( -1.000000000000000000, 0.000000000000000000, -0.000000000000000000 ) ) ;
#22270 = VERTEX_POINT ( 'NONE', #39536 ) ;
#22271 = AXIS2_PLACEMENT_3D ( 'NONE', #54798, #14200, #54431 ) ;
#22272 = CARTESIAN_POINT ( 'NONE',  ( 93.84685191531251292, -211.9973110713294489, 87.20864583420046756 ) ) ;
#22273 = CARTESIAN_POINT ( 'NONE',  ( 96.32499999999998863, -207.7050326799711968, 85.97833333333332462 ) ) ;
#22274 = VERTEX_POINT ( 'NONE', #33501 ) ;
#22275 = CARTESIAN_POINT ( 'NONE',  ( 12.50000000000000000, -132.5000000000000000, -2.500000000000000000 ) ) ;
#22276 = ORIENTED_EDGE ( 'NONE', *, *, #60867, .F. ) ;
#22277 = CARTESIAN_POINT ( 'NONE',  ( 11.99999999999999822, 0.000000000000000000, 0.000000000000000000 ) ) ;
#22278 = ORIENTED_EDGE ( 'NONE', *, *, #20562, .T. ) ;
#22279 = CIRCLE ( 'NONE', #16260, 82.00000000000000000 ) ;
#22280 = FACE_OUTER_BOUND ( 'NONE', #14887, .T. ) ;
#22281 = EDGE_LOOP ( 'NONE', ( #65685, #67157, #27246, #17950 ) ) ;
#22282 = ORIENTED_EDGE ( 'NONE', *, *, #66532, .F. ) ;
#22283 = VERTEX_POINT ( 'NONE', #50049 ) ;
#22284 = DIRECTION ( 'NONE',  ( -1.000000000000000000, 0.000000000000000000, -0.000000000000000000 ) ) ;
#22285 = ORIENTED_EDGE ( 'NONE', *, *, #35783, .F. ) ;
#22286 = ORIENTED_EDGE ( 'NONE', *, *, #73058, .F. ) ;
#22287 = CARTESIAN_POINT ( 'NONE',  ( 92.34999999999999432, 88.47002178664753558, 88.78291666666667936 ) ) ;
#22288 = CARTESIAN_POINT ( 'NONE',  ( 12.50000000000000000, -107.5000000000000000, 40.00000000000000000 ) ) ;
#22289 = DIRECTION ( 'NONE',  ( -1.000000000000000000, 0.000000000000000000, -0.000000000000000000 ) ) ;
#22290 = ORIENTED_EDGE ( 'NONE', *, *, #7016, .T. ) ;
#22291 = ORIENTED_EDGE ( 'NONE', *, *, #64167, .F. ) ;
#22292 = EDGE_LOOP ( 'NONE', ( #25893, #33912, #57426, #32900 ) ) ;
#22293 = CARTESIAN_POINT ( 'NONE',  ( 96.15314808468748708, 91.99731107132950569, 84.98614583420047097 ) ) ;
#22294 = ORIENTED_EDGE ( 'NONE', *, *, #46211, .T. ) ;
#22295 = AXIS2_PLACEMENT_3D ( 'NONE', #47905, #30970, #9158 ) ;
#22296 = CARTESIAN_POINT ( 'NONE',  ( 97.30629616937498838, -208.6684592857803011, 85.56822916753380071 ) ) ;
#22297 = APPLICATION_PROTOCOL_DEFINITION ( 'draft international standard', 'automotive_design', 1998, #48408 ) ;
#22298 = DIRECTION ( 'NONE',  ( 1.000000000000000000, 0.000000000000000000, 0.000000000000000000 ) ) ;
#22299 = CARTESIAN_POINT ( 'NONE',  ( -97.64999999999996305, -209.9999999999999716, 80.47499999999999432 ) ) ;
#22300 = CONICAL_SURFACE ( 'NONE', #31886, 1732.050807568857181, 1.047197551196592746 ) ;
#22301 = CARTESIAN_POINT ( 'NONE',  ( -10.00000000000000000, 0.000000000000000000, 0.000000000000000000 ) ) ;
#22302 = AXIS2_PLACEMENT_3D ( 'NONE', #61914, #10398, #18619 ) ;
#22303 = DIRECTION ( 'NONE',  ( 0.000000000000000000, 0.000000000000000000, 1.000000000000000000 ) ) ;
#22304 = DIRECTION ( 'NONE',  ( -1.000000000000000000, -0.000000000000000000, 0.000000000000000000 ) ) ;
#22305 = CARTESIAN_POINT ( 'NONE',  ( -92.69370383062498320, -209.9999999999999716, 87.42031250086714067 ) ) ;
#22306 = CARTESIAN_POINT ( 'NONE',  ( -97.30629616937501680, 91.33154071421968467, 87.20864583420049598 ) ) ;
#22307 = ORIENTED_EDGE ( 'NONE', *, *, #46008, .T. ) ;
#22308 = AXIS2_PLACEMENT_3D ( 'NONE', #35090, #47479, #59135 ) ;
#22310 = CARTESIAN_POINT ( 'NONE',  ( -96.15314808468751551, 88.00268892867056536, 85.30364583420046642 ) ) ;
#22309 = CARTESIAN_POINT ( 'NONE',  ( 96.15314808468748708, 91.99731107132950569, 83.08114583420048405 ) ) ;
#22311 = VECTOR ( 'NONE', #62563, 1000.000000000000000 ) ;
#22312 = ORIENTED_EDGE ( 'NONE', *, *, #60687, .F. ) ;
#22313 = CYLINDRICAL_SURFACE ( 'NONE', #11861, 16.00000000000000000 ) ;
#22314 = DIRECTION ( 'NONE',  ( -1.000000000000000000, 0.000000000000000000, 0.000000000000000000 ) ) ;
#22315 = DIRECTION ( 'NONE',  ( 0.000000000000000000, 0.000000000000000000, 1.000000000000000000 ) ) ;
#22316 = DIRECTION ( 'NONE',  ( 0.000000000000000000, 0.000000000000000000, 1.000000000000000000 ) ) ;
#22317 = CARTESIAN_POINT ( 'NONE',  ( -96.15314808468747287, -208.0026889286704943, 88.26697916753380468 ) ) ;
#22318 = DIRECTION ( 'NONE',  ( -0.000000000000000000, -0.000000000000000000, 1.000000000000000000 ) ) ;
#22319 = CYLINDRICAL_SURFACE ( 'NONE', #32598, 3.000000000000000000 ) ;
#22320 = CARTESIAN_POINT ( 'NONE',  ( -11.59999999999999787, 0.000000000000000000, -43.79999999999998295 ) ) ;
#22321 = CARTESIAN_POINT ( 'NONE',  ( 11.99999999999999822, 0.000000000000000000, 0.000000000000000000 ) ) ;
#22322 = EDGE_LOOP ( 'NONE', ( #67407, #38580, #26981, #25688 ) ) ;
#22323 = EDGE_CURVE ( 'NONE', #26140, #37645, #21109, .T. ) ;
#22324 = CIRCLE ( 'NONE', #15056, 16.00000000000000000 ) ;
#22325 = EDGE_LOOP ( 'NONE', ( #14507, #71175, #36244, #38954 ) ) ;
#22326 = EDGE_CURVE ( 'NONE', #60480, #5309, #49439, .T. ) ;
#22327 = CARTESIAN_POINT ( 'NONE',  ( -95.00000000000002842, 86.94004357329504273, 82.53874999999999318 ) ) ;
#22328 = CARTESIAN_POINT ( 'NONE',  ( 0.000000000000000000, 0.000000000000000000, -1.466666666666671670 ) ) ;
#22329 = CARTESIAN_POINT ( 'NONE',  ( 12.13205353604972991, -140.1820037904669789, 5.500000000000000000 ) ) ;
#22330 = DIRECTION ( 'NONE',  ( 9.814797785686868941E-17, 1.000000000000000000, 0.000000000000000000 ) ) ;
#22331 = CYLINDRICAL_SURFACE ( 'NONE', #45823, 31.99999999999998579 ) ;
#22332 = CARTESIAN_POINT ( 'NONE',  ( -14.09999999999999964, 1.726751986797767995E-15, -1.199999999999999956 ) ) ;
#22333 = CARTESIAN_POINT ( 'NONE',  ( 10.00000000000000000, -10.41901085202107247, 40.68715046381925049 ) ) ;
#22334 = CARTESIAN_POINT ( 'NONE',  ( 0.000000000000000000, -35.92658777277517856, 10.74501242461269257 ) ) ;
#22335 = ADVANCED_FACE ( 'NONE', ( #45180 ), #33132, .F. ) ;
#22336 = ORIENTED_EDGE ( 'NONE', *, *, #1796, .F. ) ;
#22337 = CARTESIAN_POINT ( 'NONE',  ( -95.00000000000002842, 87.33691857156074434, 78.37156250086714238 ) ) ;
#22338 = CARTESIAN_POINT ( 'NONE',  ( 0.000000000000000000, 35.38097989696528600, -12.42422080174602605 ) ) ;
#22339 = DIRECTION ( 'NONE',  ( 1.000000000000000000, 0.000000000000000000, 0.000000000000000000 ) ) ;
#22340 = CARTESIAN_POINT ( 'NONE',  ( 0.000000000000000000, 23.16143007188530234, -73.95703589263949596 ) ) ;
#22341 = DIRECTION ( 'NONE',  ( 0.000000000000000000, 0.000000000000000000, -1.000000000000000000 ) ) ;
#22342 = CARTESIAN_POINT ( 'NONE',  ( -97.65000000000001990, 90.00000000000004263, 82.37999999999999545 ) ) ;
#22343 = CARTESIAN_POINT ( 'NONE',  ( -99.99999999999997158, -214.9999999999999716, -90.00000000000000000 ) ) ;
#22344 = EDGE_CURVE ( 'NONE', #24857, #47239, #4595, .T. ) ;
#22345 = EDGE_CURVE ( 'NONE', #2485, #55377, #26754, .T. ) ;
#22346 = VECTOR ( 'NONE', #41817, 1000.000000000000000 ) ;
#22347 = CARTESIAN_POINT ( 'NONE',  ( 96.15314808468748708, 91.99731107132950569, 78.79489583420048859 ) ) ;
#22348 = CARTESIAN_POINT ( 'NONE',  ( -97.30629616937495996, -209.9999999999999716, 80.27656250086714351 ) ) ;
#22349 = CARTESIAN_POINT ( 'NONE',  ( -93.67500000000003979, 92.29496732002878900, 84.78770833506763438 ) ) ;
#22350 = VERTEX_POINT ( 'NONE', #73724 ) ;
#22351 = DIRECTION ( 'NONE',  ( -1.000000000000000000, -0.000000000000000000, 0.000000000000000000 ) ) ;
#22352 = CARTESIAN_POINT ( 'NONE',  ( -92.34999999999998010, -211.0689551420226735, 75.04052853044679239 ) ) ;
#22353 = FACE_OUTER_BOUND ( 'NONE', #45209, .T. ) ;
#22354 = EDGE_CURVE ( 'NONE', #14707, #44617, #60252, .T. ) ;
#22355 = EDGE_CURVE ( 'NONE', #70908, #18595, #47039, .T. ) ;
#22356 = CONICAL_SURFACE ( 'NONE', #34314, 1732.050807568857181, 1.047197551196592746 ) ;
#22357 = AXIS2_PLACEMENT_3D ( 'NONE', #3220, #48680, #14466 ) ;
#22358 = CARTESIAN_POINT ( 'NONE',  ( -93.84685191531252713, 88.00268892867056536, 77.94822916753382458 ) ) ;
#22359 = CARTESIAN_POINT ( 'NONE',  ( 95.00000000000000000, -207.3369185715606307, 79.32406250086714294 ) ) ;
#22360 = ORIENTED_EDGE ( 'NONE', *, *, #44469, .F. ) ;
#22361 = AXIS2_PLACEMENT_3D ( 'NONE', #46281, #29341, #5703 ) ;
#22362 = DIRECTION ( 'NONE',  ( -1.000000000000000000, -0.000000000000000000, -0.000000000000000000 ) ) ;
#22363 = EDGE_LOOP ( 'NONE', ( #26137, #30722, #27171, #49462 ) ) ;
#22364 = AXIS2_PLACEMENT_3D ( 'NONE', #3758, #49586, #36459 ) ;
#22365 = CARTESIAN_POINT ( 'NONE',  ( 11.99999999999999822, 34.44570377933693806, -69.42325613327405165 ) ) ;
#22366 = ORIENTED_EDGE ( 'NONE', *, *, #29206, .F. ) ;
#22367 = DIRECTION ( 'NONE',  ( -1.000000000000000000, 0.000000000000000000, -0.000000000000000000 ) ) ;
#22368 = VECTOR ( 'NONE', #18462, 1000.000000000000000 ) ;
#22369 = ORIENTED_EDGE ( 'NONE', *, *, #73650, .T. ) ;
#22370 = ORIENTED_EDGE ( 'NONE', *, *, #11855, .F. ) ;
#22371 = ORIENTED_EDGE ( 'NONE', *, *, #42422, .F. ) ;
#22372 = CARTESIAN_POINT ( 'NONE',  ( 92.69370383062501162, -209.9999999999999716, 76.46656250086715545 ) ) ;
#22373 = VERTEX_POINT ( 'NONE', #44808 ) ;
#22374 = CARTESIAN_POINT ( 'NONE',  ( 10.00000000000000000, 2.946379043147425492, -75.11764819372145041 ) ) ;
#22375 = LINE ( 'NONE', #50184, #53247 ) ;
#22376 = CARTESIAN_POINT ( 'NONE',  ( 97.30629616937498838, 90.00000000000002842, 88.21406250086714351 ) ) ;
#22377 = DIRECTION ( 'NONE',  ( -0.000000000000000000, -0.000000000000000000, 1.000000000000000000 ) ) ;
#22378 = CARTESIAN_POINT ( 'NONE',  ( 96.32499999999998863, -207.7050326799711968, 78.99333333333332519 ) ) ;
#22379 = ORIENTED_EDGE ( 'NONE', *, *, #73675, .F. ) ;
#22380 = ORIENTED_EDGE ( 'NONE', *, *, #55159, .T. ) ;
#22381 = ORIENTED_EDGE ( 'NONE', *, *, #32817, .T. ) ;
#22382 = EDGE_LOOP ( 'NONE', ( #48468, #39797, #72217, #6831, #63349, #67024, #32809, #41912, #52402, #7870, #1617, #32138, #73872, #49926, #25887, #6053, #36359, #20790, #64544, #9323, #5599, #5843, #21745, #20555, #66564, #16026, #38452, #40769, #25534, #25264, #14508, #44707, #35749, #68876, #23386, #52539, #67964, #42907, #53433, #64860, #37987, #11100, #56866, #3262, #10385, #67712, #8027, #61351, #59213, #14960 ) ) ;
#22383 = LINE ( 'NONE', #38567, #58604 ) ;
#22384 = CLOSED_SHELL ( 'NONE', ( #52970, #29434, #27739, #33497, #27243, #63273, #55083, #67379, #35833, #19465, #42601, #11854 ) ) ;
#22385 =( NAMED_UNIT ( * ) SI_UNIT ( $, .STERADIAN. ) SOLID_ANGLE_UNIT ( ) );
#22386 = DIRECTION ( 'NONE',  ( -1.000000000000000000, 0.000000000000000000, 0.000000000000000000 ) ) ;
#22387 = LINE ( 'NONE', #4369, #29054 ) ;
#22388 = DIRECTION ( 'NONE',  ( -1.000000000000000000, 0.000000000000000000, 0.000000000000000000 ) ) ;
#22389 = CARTESIAN_POINT ( 'NONE',  ( -11.59517495878806947, -96.12423995607481686, -5.500000000000000000 ) ) ;
#22390 = LINE ( 'NONE', #11831, #15259 ) ;
#22391 = ORIENTED_EDGE ( 'NONE', *, *, #26510, .F. ) ;
#22392 = CARTESIAN_POINT ( 'NONE',  ( -94.99999999999997158, -213.0599564267049857, 81.98312500173430806 ) ) ;
#22393 = ORIENTED_EDGE ( 'NONE', *, *, #24199, .T. ) ;
#22394 = CARTESIAN_POINT ( 'NONE',  ( 11.99999999999999822, 0.000000000000000000, 0.000000000000000000 ) ) ;
#22396 = ORIENTED_EDGE ( 'NONE', *, *, #51865, .F. ) ;
#22395 = EDGE_CURVE ( 'NONE', #2275, #26184, #12249, .T. ) ;
#22398 = CARTESIAN_POINT ( 'NONE',  ( -97.65000000000001990, 88.47002178664754979, 79.33729166840096525 ) ) ;
#22397 = CARTESIAN_POINT ( 'NONE',  ( 92.34999999999999432, 88.47002178664753558, 83.14729166840096752 ) ) ;
#22399 = EDGE_LOOP ( 'NONE', ( #34974, #71024, #67591, #2655 ) ) ;
#22400 = CARTESIAN_POINT ( 'NONE',  ( 96.15314808468748708, 91.99731107132950569, 83.23989583420049598 ) ) ;
#22401 = AXIS2_PLACEMENT_3D ( 'NONE', #67343, #15843, #21847 ) ;
#22402 = CARTESIAN_POINT ( 'NONE',  ( 11.99999999999999822, 0.000000000000000000, 0.000000000000000000 ) ) ;
#22403 = DIRECTION ( 'NONE',  ( 0.000000000000000000, -0.3826834323650969427, 0.9238795325112838519 ) ) ;
#22404 = EDGE_CURVE ( 'NONE', #37315, #70629, #57198, .T. ) ;
#22405 = CARTESIAN_POINT ( 'NONE',  ( 15.00000000000000000, 5.835314593368777558, 22.81335362449846471 ) ) ;
#22406 = DIRECTION ( 'NONE',  ( -1.000000000000000000, 0.000000000000000000, 0.000000000000000000 ) ) ;
#22407 = CARTESIAN_POINT ( 'NONE',  ( -97.64999999953492704, -210.0000309987302956, 83.09538598079114990 ) ) ;
#22408 = VERTEX_POINT ( 'NONE', #24103 ) ;
#22409 = CARTESIAN_POINT ( 'NONE',  ( 10.00000000000000000, 26.79245525562714647, 32.34446384429980981 ) ) ;
#22410 = CARTESIAN_POINT ( 'NONE',  ( -97.64999999960637922, 90.00002930319634231, 82.45844277051273252 ) ) ;
#22411 = DIRECTION ( 'NONE',  ( -0.000000000000000000, -0.000000000000000000, 1.000000000000000000 ) ) ;
#22412 = ORIENTED_EDGE ( 'NONE', *, *, #34368, .T. ) ;
#22413 = EDGE_CURVE ( 'NONE', #39476, #66935, #2691, .T. ) ;
#22414 = VERTEX_POINT ( 'NONE', #17706 ) ;
#22415 = CIRCLE ( 'NONE', #34424, 77.49899999999999523 ) ;
#22416 = DIRECTION ( 'NONE',  ( 0.000000000000000000, 0.000000000000000000, 1.000000000000000000 ) ) ;
#22417 = EDGE_CURVE ( 'NONE', #22556, #1777, #11322, .T. ) ;
#22418 = PRODUCT_DEFINITION_SHAPE ( 'NONE', 'NONE',  #74342 ) ;
#22419 = CARTESIAN_POINT ( 'NONE',  ( 2.499999999999984457, -73.00000000000001421, -251.7000000000000455 ) ) ;
#22420 = AXIS2_PLACEMENT_3D ( 'NONE', #12706, #1117, #11974 ) ;
#22421 = CARTESIAN_POINT ( 'NONE',  ( -92.35000000000005116, 88.47002178664754979, 80.18395833506764347 ) ) ;
#22422 = DIRECTION ( 'NONE',  ( -1.000000000000000000, 0.000000000000000000, 0.000000000000000000 ) ) ;
#22423 = CARTESIAN_POINT ( 'NONE',  ( -97.30629616937497417, -208.6684592857803011, 80.22364583420048234 ) ) ;
#22424 = ORIENTED_EDGE ( 'NONE', *, *, #3341, .F. ) ;
#22425 = EDGE_CURVE ( 'NONE', #35486, #48585, #69828, .T. ) ;
#22426 = CARTESIAN_POINT ( 'NONE',  ( -97.30629616937501680, 88.66845928578038638, 88.42572916753380241 ) ) ;
#22427 = EDGE_LOOP ( 'NONE', ( #11270, #44103, #73410, #25981 ) ) ;
#22428 = FACE_OUTER_BOUND ( 'NONE', #69702, .T. ) ;
#22429 = CARTESIAN_POINT ( 'NONE',  ( 10.00000000000000000, 35.92658777277525672, -10.74501242461245809 ) ) ;
#22430 = VECTOR ( 'NONE', #71343, 1000.000000000000000 ) ;
#22431 = DIRECTION ( 'NONE',  ( -1.000000000000000000, -0.000000000000000000, 0.000000000000000000 ) ) ;
#22432 = CARTESIAN_POINT ( 'NONE',  ( 94.99999999999998579, 92.66308142843932671, 74.87906250086713555 ) ) ;
#22433 = CARTESIAN_POINT ( 'NONE',  ( 12.00000000000000000, 14.60985201121729737, 18.46759930825687235 ) ) ;
#22434 = LINE ( 'NONE', #17162, #73260 ) ;
#22435 = CARTESIAN_POINT ( 'NONE',  ( -95.00000000000002842, 90.00000000000004263, 90.00000000000000000 ) ) ;
#22436 = PLANE ( 'NONE',  #42425 ) ;
#22437 = LINE ( 'NONE', #29167, #44822 ) ;
#22438 = ADVANCED_FACE ( 'NONE', ( #68486 ), #12796, .T. ) ;
#22439 = DIRECTION ( 'NONE',  ( -1.000000000000000000, -0.000000000000000000, 0.000000000000000000 ) ) ;
#22440 = ADVANCED_FACE ( 'NONE', ( #41383 ), #1209, .F. ) ;
#22441 = CARTESIAN_POINT ( 'NONE',  ( -3.000000000000000000, -18.13022148937263012, 15.02647892043544608 ) ) ;
#22442 = CARTESIAN_POINT ( 'NONE',  ( 97.30629616937498838, 91.33154071421968467, 89.53697916753382913 ) ) ;
#22443 = CARTESIAN_POINT ( 'NONE',  ( -97.30629616937497417, -208.6684592857803295, 89.11364583420049712 ) ) ;
#22444 = CARTESIAN_POINT ( 'NONE',  ( -2.981742216678212820, 0.000000000000000000, 15.39727592608509177 ) ) ;
#22445 = ORIENTED_EDGE ( 'NONE', *, *, #32845, .T. ) ;
#22446 = DIRECTION ( 'NONE',  ( -1.000000000000000000, 0.000000000000000000, 0.000000000000000000 ) ) ;
#22447 = CARTESIAN_POINT ( 'NONE',  ( -92.69370383062505425, 91.33154071421968467, 79.85322916753379729 ) ) ;
#22448 = AXIS2_PLACEMENT_3D ( 'NONE', #24192, #47127, #18896 ) ;
#22449 = DIRECTION ( 'NONE',  ( 1.000000000000000000, 0.000000000000000000, 0.000000000000000000 ) ) ;
#22450 = ORIENTED_EDGE ( 'NONE', *, *, #52910, .F. ) ;
#22451 =( BOUNDED_CURVE ( )  B_SPLINE_CURVE ( 2, ( #37780, #8826, #48677, #65987, #14462, #71217, #42670, #49416, #72692 ),
 .UNSPECIFIED., .F., .F. ) 
 B_SPLINE_CURVE_WITH_KNOTS ( ( 3, 2, 2, 2, 3 ),
 ( 0.8678591737214811364, 0.8749149270694133174, 0.8819706926102951483, 0.8890264581511769792, 0.8890265259358467453 ),
 .UNSPECIFIED. ) 
 CURVE ( )  GEOMETRIC_REPRESENTATION_ITEM ( )  RATIONAL_B_SPLINE_CURVE ( ( 1.000000000000000000, 0.8660254037844387076, 1.000000000000000000, 0.8660254037844387076, 1.000000000000000000, 0.8660254037844387076, 1.000000000000000000, 0.9999987129073784065, 0.9999974258394870308 ) ) 
 REPRESENTATION_ITEM ( '' )  );
#22452 = DIRECTION ( 'NONE',  ( -0.000000000000000000, -0.000000000000000000, 1.000000000000000000 ) ) ;
#22453 = DIRECTION ( 'NONE',  ( -0.000000000000000000, -0.000000000000000000, 1.000000000000000000 ) ) ;
#22454 = AXIS2_PLACEMENT_3D ( 'NONE', #20655, #15002, #32287 ) ;
#22455 = CARTESIAN_POINT ( 'NONE',  ( 70.53423027509757048, -217.0820393249931044, 5.500000000000000000 ) ) ;
#22456 = VECTOR ( 'NONE', #63261, 1000.000000000000000 ) ;
#22457 = DIRECTION ( 'NONE',  ( 0.000000000000000000, -0.1564344650402172410, -0.9876883405951399908 ) ) ;
#22458 = CARTESIAN_POINT ( 'NONE',  ( 92.69370383062501162, -211.3315407142195852, 75.24947916753383481 ) ) ;
#22459 = VECTOR ( 'NONE', #64030, 1000.000000000000000 ) ;
#22460 = EDGE_LOOP ( 'NONE', ( #42544, #44278, #11476, #62710 ) ) ;
#22461 = AXIS2_PLACEMENT_3D ( 'NONE', #52066, #44960, #68640 ) ;
#22462 = ORIENTED_EDGE ( 'NONE', *, *, #9583, .T. ) ;
#22463 = CARTESIAN_POINT ( 'NONE',  ( 97.30629616937497417, -209.9999999999998863, 74.79348190356849102 ) ) ;
#22464 = AXIS2_PLACEMENT_3D ( 'NONE', #46565, #7451, #43160 ) ;
#22465 = VECTOR ( 'NONE', #42145, 1000.000000000000000 ) ;
#22466 = FACE_OUTER_BOUND ( 'NONE', #70693, .T. ) ;
#22467 = LINE ( 'NONE', #32982, #35275 ) ;
#22468 = DIRECTION ( 'NONE',  ( 0.000000000000000000, 0.000000000000000000, -1.000000000000000000 ) ) ;
#22469 = LINE ( 'NONE', #51034, #63331 ) ;
#22470 = CARTESIAN_POINT ( 'NONE',  ( 93.67500000000001137, -207.7050326799711968, 86.71916666666666629 ) ) ;
#22471 = ADVANCED_FACE ( 'NONE', ( #64320 ), #39914, .T. ) ;
#22472 = VERTEX_POINT ( 'NONE', #62863 ) ;
#22473 = VERTEX_POINT ( 'NONE', #58301 ) ;
#22474 = CARTESIAN_POINT ( 'NONE',  ( 11.99999999999999822, 0.000000000000000000, 0.000000000000000000 ) ) ;
#22475 = ORIENTED_EDGE ( 'NONE', *, *, #13651, .F. ) ;
#22476 = VERTEX_POINT ( 'NONE', #463 ) ;
#22477 = DIRECTION ( 'NONE',  ( 0.000000000000000000, 0.000000000000000000, 1.000000000000000000 ) ) ;
#22478 = AXIS2_PLACEMENT_3D ( 'NONE', #17555, #40488, #1427 ) ;
#22479 = CARTESIAN_POINT ( 'NONE',  ( -11.68233973192911535, 2.127397731264211754E-15, 17.37152077436032371 ) ) ;
#22480 = ADVANCED_FACE ( 'NONE', ( #6796 ), #23358, .F. ) ;
#22481 = EDGE_LOOP ( 'NONE', ( #56405, #37114, #62885, #42899 ) ) ;
#22482 = CYLINDRICAL_SURFACE ( 'NONE', #48584, 82.00000000000000000 ) ;
#22483 = CARTESIAN_POINT ( 'NONE',  ( 95.00000000000000000, -213.0599564267049857, 75.63312500173429953 ) ) ;
#22484 = CARTESIAN_POINT ( 'NONE',  ( 94.99999999999998579, 86.94004357329500010, 82.53874999999999318 ) ) ;
#22486 = ADVANCED_FACE ( 'NONE', ( #5706 ), #17339, .T. ) ;
#22485 = VECTOR ( 'NONE', #45594, 1000.000000000000000 ) ;
#22487 = ORIENTED_EDGE ( 'NONE', *, *, #5565, .T. ) ;
#22488 = CARTESIAN_POINT ( 'NONE',  ( 95.00000000000000000, -206.9400435732949575, 75.31562500173430408 ) ) ;
#22489 = ORIENTED_EDGE ( 'NONE', *, *, #2162, .F. ) ;
#22490 = CARTESIAN_POINT ( 'NONE',  ( -3.702536634196120335, 8.043911037661892749, -55.00000000000000000 ) ) ;
#22491 = ORIENTED_EDGE ( 'NONE', *, *, #39377, .F. ) ;
#22492 = CARTESIAN_POINT ( 'NONE',  ( 97.64999017507813051, -211.5299838857737029, 88.43895794268867405 ) ) ;
#22493 = CARTESIAN_POINT ( 'NONE',  ( -97.30629616937501680, 91.33154071421968467, 80.22364583420048234 ) ) ;
#22494 = CARTESIAN_POINT ( 'NONE',  ( 94.99999999999998579, 92.66308142843935514, 79.32406250086714294 ) ) ;
#22495 = ORIENTED_EDGE ( 'NONE', *, *, #39813, .T. ) ;
#22496 = CARTESIAN_POINT ( 'NONE',  ( -42.50000000000000000, 0.000000000000000000, -12.50000000000000000 ) ) ;
#22497 = EDGE_CURVE ( 'NONE', #12910, #55755, #26617, .T. ) ;
#22498 = DIRECTION ( 'NONE',  ( -1.000000000000000000, -0.000000000000000000, -0.000000000000000000 ) ) ;
#22499 = CARTESIAN_POINT ( 'NONE',  ( 96.32499999999998863, 87.70503267997126784, 89.02104166840096866 ) ) ;
#22500 = DIRECTION ( 'NONE',  ( 2.603472992746261562E-14, 2.546204323184492723E-14, -1.000000000000000000 ) ) ;
#22501 = ORIENTED_EDGE ( 'NONE', *, *, #25204, .T. ) ;
#22502 = CARTESIAN_POINT ( 'NONE',  ( 11.99999999999999822, 77.49459641780886443, 0.8261519478433866359 ) ) ;
#22503 = CARTESIAN_POINT ( 'NONE',  ( -92.69370383062498320, -211.3315407142195852, 77.84239583420045960 ) ) ;
#22504 = EDGE_LOOP ( 'NONE', ( #5482, #22117, #8191, #63831 ) ) ;
#22505 = ORIENTED_EDGE ( 'NONE', *, *, #54343, .T. ) ;
#22506 = CARTESIAN_POINT ( 'NONE',  ( 97.65000000000000568, 91.52997821335252127, 75.20979166840096752 ) ) ;
#22507 = VERTEX_POINT ( 'NONE', #12065 ) ;
#22508 = CARTESIAN_POINT ( 'NONE',  ( -10.00000000000000000, 0.000000000000000000, 0.000000000000000000 ) ) ;
#22509 =( REPRESENTATION_RELATIONSHIP ('NONE','NONE', #31117, #51769 ) REPRESENTATION_RELATIONSHIP_WITH_TRANSFORMATION ( #59108 )SHAPE_REPRESENTATION_RELATIONSHIP( ) );
#22510 = FACE_OUTER_BOUND ( 'NONE', #18490, .T. ) ;
#22511 = ORIENTED_EDGE ( 'NONE', *, *, #36681, .T. ) ;
#22512 = CARTESIAN_POINT ( 'NONE',  ( -97.30629616937497417, -211.3315407142195852, 75.72572916753381378 ) ) ;
#22513 = ORIENTED_EDGE ( 'NONE', *, *, #21748, .T. ) ;
#22515 = EDGE_CURVE ( 'NONE', #11290, #26437, #58669, .T. ) ;
#22514 = CARTESIAN_POINT ( 'NONE',  ( -97.64999999999996305, -209.9999999999999716, 81.74500000000000455 ) ) ;
#22516 = VECTOR ( 'NONE', #45132, 1000.000000000000000 ) ;
#22517 = DIRECTION ( 'NONE',  ( 0.000000000000000000, -0.8526401643540970632, 0.5224985647159409163 ) ) ;
#22518 = FACE_OUTER_BOUND ( 'NONE', #50874, .T. ) ;
#22519 = CARTESIAN_POINT ( 'NONE',  ( 92.35000000000000853, -209.9999999999999716, 81.74500000000000455 ) ) ;
#22520 = AXIS2_PLACEMENT_3D ( 'NONE', #41351, #34223, #6050 ) ;
#22521 = CARTESIAN_POINT ( 'NONE',  ( 23.49916127795269460, -121.5130826919798039, 5.500000000000000000 ) ) ;
#22522 = CARTESIAN_POINT ( 'NONE',  ( 95.00000000000000000, -206.9400435732949575, 86.11062500173430578 ) ) ;
#22523 = CARTESIAN_POINT ( 'NONE',  ( 97.30629616937498838, 90.00000000000002842, 86.15031250086714465 ) ) ;
#22524 = VECTOR ( 'NONE', #3958, 1000.000000000000000 ) ;
#22525 = CARTESIAN_POINT ( 'NONE',  ( 10.00000000000000000, -40.68715046381921496, -10.41901085202121457 ) ) ;
#22526 = CYLINDRICAL_SURFACE ( 'NONE', #7376, 82.00000000000000000 ) ;
#22527 = CARTESIAN_POINT ( 'NONE',  ( 92.35000000000000853, -209.9999999999999716, 86.82500000000000284 ) ) ;
#22528 = CARTESIAN_POINT ( 'NONE',  ( -5.000000000000000000, -4.846777557549235459E-18, -0.5080592402122449114 ) ) ;
#22529 = LINE ( 'NONE', #16890, #62077 ) ;
#22530 = EDGE_CURVE ( 'NONE', #38967, #4807, #11680, .T. ) ;
#22531 = CARTESIAN_POINT ( 'NONE',  ( 97.65000000000000568, -211.5299782133524218, 87.80395833506766223 ) ) ;
#22532 = CARTESIAN_POINT ( 'NONE',  ( -12.49999999999999822, -120.0000000000000000, 125.0000000000000000 ) ) ;
#22533 = EDGE_CURVE ( 'NONE', #9134, #42185, #6441, .T. ) ;
#22534 = CARTESIAN_POINT ( 'NONE',  ( 0.000000000000000000, -58.39081064771786345, 50.95692526931308919 ) ) ;
#22535 = ADVANCED_FACE ( 'NONE', ( #18441 ), #8602, .T. ) ;
#22536 = CARTESIAN_POINT ( 'NONE',  ( 4.999999999999999112, 9.188173127307898369, -40.98264845739739570 ) ) ;
#22537 = LINE ( 'NONE', #62403, #37348 ) ;
#22538 = DIRECTION ( 'NONE',  ( -1.000000000000000000, 0.000000000000000000, -0.000000000000000000 ) ) ;
#22539 = CARTESIAN_POINT ( 'NONE',  ( 15.00000000000000000, 9.615535125378766423, -24.73947219025917121 ) ) ;
#22540 = CARTESIAN_POINT ( 'NONE',  ( -94.99999999999997158, -206.9400435732949575, 83.49125000000000796 ) ) ;
#22541 = VECTOR ( 'NONE', #39958, 1000.000000000000114 ) ;
#22542 = CARTESIAN_POINT ( 'NONE',  ( -93.67500000000003979, 87.70503267997129626, 80.05166666666666231 ) ) ;
#22543 = ORIENTED_EDGE ( 'NONE', *, *, #65038, .T. ) ;
#22544 = DIRECTION ( 'NONE',  ( 0.000000000000000000, 0.000000000000000000, 1.000000000000000000 ) ) ;
#22545 = CARTESIAN_POINT ( 'NONE',  ( 10.00000000000000000, 0.000000000000000000, 0.000000000000000000 ) ) ;
#22546 = DIRECTION ( 'NONE',  ( 0.000000000000000000, -0.3090169943749573878, 0.9510565162951503115 ) ) ;
#22547 = DIRECTION ( 'NONE',  ( 0.000000000000000000, 0.000000000000000000, 1.000000000000000000 ) ) ;
#22548 = CARTESIAN_POINT ( 'NONE',  ( 92.69370383062501162, -209.9999999999999716, 85.35656250086715602 ) ) ;
#22549 = EDGE_LOOP ( 'NONE', ( #37991, #348, #59005, #40714 ) ) ;
#22550 = ORIENTED_EDGE ( 'NONE', *, *, #19668, .T. ) ;
#22551 = CARTESIAN_POINT ( 'NONE',  ( -19.90058851926621131, -132.5883508287165853, 5.500000000000000000 ) ) ;
#22552 = EDGE_LOOP ( 'NONE', ( #10847, #41766, #6300, #13665 ) ) ;
#22553 = CARTESIAN_POINT ( 'NONE',  ( -0.0004442498508594591917, 0.001194404164628348752, -65.00000000000000000 ) ) ;
#22554 = CARTESIAN_POINT ( 'NONE',  ( 95.00000000000000000, -207.3369185715606307, 77.41906250086714181 ) ) ;
#22555 = AXIS2_PLACEMENT_3D ( 'NONE', #2631, #20231, #31146 ) ;
#22556 = VERTEX_POINT ( 'NONE', #41021 ) ;
#22557 = CARTESIAN_POINT ( 'NONE',  ( 93.84685191531251292, -211.9973110713294489, 82.28739583420048120 ) ) ;
#22558 = AXIS2_PLACEMENT_3D ( 'NONE', #4045, #54412, #43153 ) ;
#22559 = AXIS2_PLACEMENT_3D ( 'NONE', #13364, #12983, #35192 ) ;
#22560 = EDGE_CURVE ( 'NONE', #33726, #26516, #47044, .T. ) ;
#22561 = ORIENTED_EDGE ( 'NONE', *, *, #6798, .F. ) ;
#22562 = FACE_OUTER_BOUND ( 'NONE', #9620, .T. ) ;
#22563 = EDGE_LOOP ( 'NONE', ( #72323, #17770, #6197, #82 ) ) ;
#22564 = ORIENTED_EDGE ( 'NONE', *, *, #26743, .F. ) ;
#22565 = AXIS2_PLACEMENT_3D ( 'NONE', #31372, #54322, #54686 ) ;
#22566 = CARTESIAN_POINT ( 'NONE',  ( 10.00000000000000000, -12.42422080174663712, 35.38097989696507994 ) ) ;
#22567 = VECTOR ( 'NONE', #65904, 1000.000000000000000 ) ;
#22568 = EDGE_CURVE ( 'NONE', #40794, #59498, #71045, .T. ) ;
#22569 = ORIENTED_EDGE ( 'NONE', *, *, #20343, .F. ) ;
#22570 = CARTESIAN_POINT ( 'NONE',  ( 93.67500000000001137, -207.7050326799711968, 86.79854166840097207 ) ) ;
#22571 = EDGE_CURVE ( 'NONE', #36763, #38273, #72239, .T. ) ;
#22572 = VERTEX_POINT ( 'NONE', #36468 ) ;
#22573 = FACE_BOUND ( 'NONE', #22994, .T. ) ;
#22574 = ORIENTED_EDGE ( 'NONE', *, *, #2438, .F. ) ;
#22575 = DIRECTION ( 'NONE',  ( 0.000000000000000000, -0.5877852522924624790, -0.8090169943749552228 ) ) ;
#22576 = ORIENTED_EDGE ( 'NONE', *, *, #19701, .T. ) ;
#22577 = EDGE_CURVE ( 'NONE', #44562, #54121, #30821, .T. ) ;
#22578 = ORIENTED_EDGE ( 'NONE', *, *, #69753, .F. ) ;
#22579 = ORIENTED_EDGE ( 'NONE', *, *, #63115, .T. ) ;
#22580 = CARTESIAN_POINT ( 'NONE',  ( 10.00000000000000000, 0.000000000000000000, 0.000000000000000000 ) ) ;
#22581 = CONTEXT_DEPENDENT_SHAPE_REPRESENTATION ( #59063, #39840 ) ;
#22582 = DIRECTION ( 'NONE',  ( 0.000000000000000000, 0.9510565162951544194, -0.3090169943749446757 ) ) ;
#22583 = ORIENTED_EDGE ( 'NONE', *, *, #30753, .T. ) ;
#22584 = CIRCLE ( 'NONE', #38187, 31.99999999999998579 ) ;
#22585 = ORIENTED_EDGE ( 'NONE', *, *, #51, .F. ) ;
#22586 = AXIS2_PLACEMENT_3D ( 'NONE', #4855, #67984, #66229 ) ;
#22587 = ORIENTED_EDGE ( 'NONE', *, *, #21364, .F. ) ;
#22588 = FACE_OUTER_BOUND ( 'NONE', #5185, .T. ) ;
#22589 = CARTESIAN_POINT ( 'NONE',  ( -0.0004442498525516064278, 0.001194404164626844313, -80.00000000000001421 ) ) ;
#22590 = AXIS2_PLACEMENT_3D ( 'NONE', #13664, #43740, #31326 ) ;
#22591 = AXIS2_PLACEMENT_3D ( 'NONE', #15486, #20397, #9108 ) ;
#22592 = CARTESIAN_POINT ( 'NONE',  ( -97.30629616937501680, 88.66845928578038638, 76.51947916753381662 ) ) ;
#22593 = ORIENTED_EDGE ( 'NONE', *, *, #12579, .T. ) ;
#22594 = EDGE_CURVE ( 'NONE', #4546, #21420, #31199, .T. ) ;
#22595 = LINE ( 'NONE', #23697, #65944 ) ;
#22596 = AXIS2_PLACEMENT_3D ( 'NONE', #71148, #65539, #14009 ) ;
#22597 = ORIENTED_EDGE ( 'NONE', *, *, #6285, .T. ) ;
#22598 = DIRECTION ( 'NONE',  ( -1.000000000000000000, -0.000000000000000000, -0.000000000000000000 ) ) ;
#22599 = CARTESIAN_POINT ( 'NONE',  ( -94.99999999999997158, -212.6630814284392557, 86.62656250086715204 ) ) ;
#22600 = ORIENTED_EDGE ( 'NONE', *, *, #2933, .T. ) ;
#22602 = ADVANCED_FACE ( 'NONE', ( #19546 ), #71411, .T. ) ;
#22601 = FACE_BOUND ( 'NONE', #15319, .T. ) ;
#22603 = CARTESIAN_POINT ( 'NONE',  ( 93.32700159667696482, -211.9834083483116274, 74.96344747200082281 ) ) ;
#22604 = CARTESIAN_POINT ( 'NONE',  ( 92.34999999999999432, 90.00000000000002842, 81.10999999999999943 ) ) ;
#22605 = CARTESIAN_POINT ( 'NONE',  ( 0.000000000000000000, 10.96151621346487914, 35.95386929396260456 ) ) ;
#22606 = DIRECTION ( 'NONE',  ( 1.000000000000000000, -0.000000000000000000, -0.000000000000000000 ) ) ;
#22607 = DIRECTION ( 'NONE',  ( -0.000000000000000000, -0.000000000000000000, -1.000000000000000000 ) ) ;
#22608 = FACE_OUTER_BOUND ( 'NONE', #17189, .T. ) ;
#22609 = CARTESIAN_POINT ( 'NONE',  ( 0.000000000000000000, -80.55351364060578589, -15.33399622253570094 ) ) ;
#22610 = LINE ( 'NONE', #16971, #53592 ) ;
#22611 = EDGE_CURVE ( 'NONE', #16194, #68284, #31565, .T. ) ;
#22612 = CARTESIAN_POINT ( 'NONE',  ( -93.84685191531254134, 91.99731107132950569, 81.17614583420048291 ) ) ;
#22613 = CARTESIAN_POINT ( 'NONE',  ( 4.999999999999999112, -41.91543099594816368, -2.663952781846588014 ) ) ;
#22614 = CARTESIAN_POINT ( 'NONE',  ( 10.00000000000000000, 0.000000000000000000, 0.000000000000000000 ) ) ;
#22615 = EDGE_CURVE ( 'NONE', #9042, #25161, #13172, .T. ) ;
#22616 = AXIS2_PLACEMENT_3D ( 'NONE', #14509, #31057, #70525 ) ;
#22617 = VERTEX_POINT ( 'NONE', #54150 ) ;
#22618 = DIRECTION ( 'NONE',  ( 0.000000000000000000, 0.000000000000000000, 1.000000000000000000 ) ) ;
#22619 = AXIS2_PLACEMENT_3D ( 'NONE', #70873, #19372, #7729 ) ;
#22620 = CARTESIAN_POINT ( 'NONE',  ( -4.182066831946699814, 3.358985280702823761, -5.826062401966626503 ) ) ;
#22621 = CYLINDRICAL_SURFACE ( 'NONE', #21385, 77.49899999999999523 ) ;
#22622 = DIRECTION ( 'NONE',  ( 0.000000000000000000, 0.000000000000000000, 1.000000000000000000 ) ) ;
#22623 = CARTESIAN_POINT ( 'NONE',  ( -10.00000000000000000, 0.000000000000000000, 0.000000000000000000 ) ) ;
#22624 = DIRECTION ( 'NONE',  ( -1.000000000000000000, -0.000000000000000000, -0.000000000000000000 ) ) ;
#22625 = CARTESIAN_POINT ( 'NONE',  ( -97.30629616937495996, -209.9999999999999716, 80.27656250086714351 ) ) ;
#22626 = CIRCLE ( 'NONE', #43019, 42.00000000000000000 ) ;
#22627 = DIRECTION ( 'NONE',  ( 1.000000000000000000, 0.000000000000000000, 0.000000000000000000 ) ) ;
#22628 = ORIENTED_EDGE ( 'NONE', *, *, #8942, .F. ) ;
#22629 = FACE_OUTER_BOUND ( 'NONE', #26068, .T. ) ;
#22630 = CARTESIAN_POINT ( 'NONE',  ( 97.65000000000000568, 91.52997821335252127, 76.47979166840096354 ) ) ;
#22631 = DIRECTION ( 'NONE',  ( -1.000000000000000000, 0.000000000000000000, 0.000000000000000000 ) ) ;
#22632 = PLANE ( 'NONE',  #1780 ) ;
#22633 = LINE ( 'NONE', #14203, #51063 ) ;
#22634 = VECTOR ( 'NONE', #2722, 1000.000000000000227 ) ;
#22636 = DIRECTION ( 'NONE',  ( 0.000000000000000000, -0.9510565162951500895, -0.3090169943749581649 ) ) ;
#22635 = AXIS2_PLACEMENT_3D ( 'NONE', #19215, #13205, #31598 ) ;
#22637 = ORIENTED_EDGE ( 'NONE', *, *, #19184, .F. ) ;
#22638 = AXIS2_PLACEMENT_3D ( 'NONE', #51178, #468, #34631 ) ;
#22639 = DIRECTION ( 'NONE',  ( -1.000000000000000000, 0.000000000000000000, 0.000000000000000000 ) ) ;
#22640 = CYLINDRICAL_SURFACE ( 'NONE', #46368, 82.00000000000000000 ) ;
#22641 = VERTEX_POINT ( 'NONE', #18803 ) ;
#22642 = TOROIDAL_SURFACE ( 'NONE', #62263, 4.700000000000000178, 0.2999999999999999889 ) ;
#22643 = CARTESIAN_POINT ( 'NONE',  ( 97.30629616937498838, -208.6684592857803295, 89.37822916753378877 ) ) ;
#22644 = CARTESIAN_POINT ( 'NONE',  ( -93.67500000000003979, 92.29496732002878900, 82.24770833506762813 ) ) ;
#22645 = ORIENTED_EDGE ( 'NONE', *, *, #36645, .T. ) ;
#22646 = EDGE_CURVE ( 'NONE', #45965, #47718, #53401, .T. ) ;
#22647 = CARTESIAN_POINT ( 'NONE',  ( 97.64999999999999147, -209.9999999999999716, 75.07749999999998636 ) ) ;
#22648 = ORIENTED_EDGE ( 'NONE', *, *, #14785, .T. ) ;
#22649 = FACE_OUTER_BOUND ( 'NONE', #60918, .T. ) ;
#22650 = ORIENTED_EDGE ( 'NONE', *, *, #8668, .F. ) ;
#22651 = CARTESIAN_POINT ( 'NONE',  ( -97.64999999999996305, -209.9999999999999716, 79.91937500173429498 ) ) ;
#22652 = ADVANCED_FACE ( 'NONE', ( #13899 ), #3398, .T. ) ;
#22653 = ORIENTED_EDGE ( 'NONE', *, *, #49158, .F. ) ;
#22654 = DIRECTION ( 'NONE',  ( -1.000000000000000000, -0.000000000000000000, 0.000000000000000000 ) ) ;
#22655 = ORIENTED_EDGE ( 'NONE', *, *, #7460, .F. ) ;
#22656 = ADVANCED_FACE ( 'NONE', ( #65067 ), #36840, .T. ) ;
#22657 = EDGE_LOOP ( 'NONE', ( #15568, #56252, #66649, #41157 ) ) ;
#22658 = CARTESIAN_POINT ( 'NONE',  ( 10.00000000000000000, -31.52238457039580055, -27.75498641678775869 ) ) ;
#22659 = EDGE_LOOP ( 'NONE', ( #34670, #49029, #15935, #50528 ) ) ;
#22660 = VERTEX_POINT ( 'NONE', #48499 ) ;
#22661 =( BOUNDED_CURVE ( )  B_SPLINE_CURVE ( 2, ( #69776, #6275, #52867, #47588, #1405, #69053, #70135, #34837, #18277 ),
 .UNSPECIFIED., .F., .F. ) 
 B_SPLINE_CURVE_WITH_KNOTS ( ( 3, 2, 2, 2, 3 ),
 ( 0.4021785743327781493, 0.4021786358302961717, 0.4092344013711782247, 0.4162901669120602222, 0.4233457466685775494 ),
 .UNSPECIFIED. ) 
 CURVE ( )  GEOMETRIC_REPRESENTATION_ITEM ( )  RATIONAL_B_SPLINE_CURVE ( ( 0.9999976645954902210, 0.9999988322875673630, 1.000000000000000000, 0.8660254037844387076, 1.000000000000000000, 0.8660254037844387076, 1.000000000000000000, 0.8660289314505862368, 0.9999929448534778942 ) ) 
 REPRESENTATION_ITEM ( '' )  );
#22662 = CARTESIAN_POINT ( 'NONE',  ( 97.64999999999997726, 91.52997821335252127, 89.10041666666667481 ) ) ;
#22663 = LINE ( 'NONE', #22288, #10038 ) ;
#22664 = CIRCLE ( 'NONE', #57495, 31.99999999999998579 ) ;
#22665 = DIRECTION ( 'NONE',  ( -0.000000000000000000, -0.000000000000000000, 1.000000000000000000 ) ) ;
#22666 = AXIS2_PLACEMENT_3D ( 'NONE', #8377, #2775, #38053 ) ;
#22667 = EDGE_LOOP ( 'NONE', ( #47702, #49567, #5774, #58983 ) ) ;
#22668 = VECTOR ( 'NONE', #46213, 1000.000000000000000 ) ;
#22669 = ORIENTED_EDGE ( 'NONE', *, *, #20360, .T. ) ;
#22670 = EDGE_CURVE ( 'NONE', #11862, #69710, #53766, .T. ) ;
#22671 = VERTEX_POINT ( 'NONE', #47396 ) ;
#22672 = CARTESIAN_POINT ( 'NONE',  ( 92.69370383062498320, 90.00000000000002842, 85.19781250086714408 ) ) ;
#22673 = ORIENTED_EDGE ( 'NONE', *, *, #59887, .F. ) ;
#22674 = CARTESIAN_POINT ( 'NONE',  ( 96.15314808468748708, -208.0026889286704943, 83.71614583420047495 ) ) ;
#22675 = PRODUCT_CONTEXT ( 'NONE', #6592, 'mechanical' ) ;
#22676 = CARTESIAN_POINT ( 'NONE',  ( 0.000000000000000000, 0.000000000000000000, -25.03750572909317285 ) ) ;
#22677 = CIRCLE ( 'NONE', #53849, 37.49900000000000233 ) ;
#22678 = CARTESIAN_POINT ( 'NONE',  ( 0.000000000000000000, 2.663952781846149254, 41.91543099594818500 ) ) ;
#22679 = CARTESIAN_POINT ( 'NONE',  ( -92.35000000000005116, 91.52997821335253548, 77.74979166840097378 ) ) ;
#22680 = CIRCLE ( 'NONE', #38280, 82.00000000000000000 ) ;
#22681 = LINE ( 'NONE', #69275, #822 ) ;
#22682 = LINE ( 'NONE', #29400, #52850 ) ;
#22683 = CYLINDRICAL_SURFACE ( 'NONE', #55228, 82.00000000000000000 ) ;
#22684 = CARTESIAN_POINT ( 'NONE',  ( -92.69370383062498320, -209.9999999999999716, 86.15031250086714465 ) ) ;
#22685 = CARTESIAN_POINT ( 'NONE',  ( -93.84685191531254134, 91.99731107132950569, 85.14489583420048291 ) ) ;
#22686 = ORIENTED_EDGE ( 'NONE', *, *, #34189, .T. ) ;
#22687 = ADVANCED_FACE ( 'NONE', ( #66177 ), #25562, .T. ) ;
#22689 = CARTESIAN_POINT ( 'NONE',  ( -96.15314808468752972, 91.99731107132950569, 83.82197916753381151 ) ) ;
#22688 = CARTESIAN_POINT ( 'NONE',  ( 97.30629616937498838, 88.66845928578037217, 84.19239583420046813 ) ) ;
#22690 = ORIENTED_EDGE ( 'NONE', *, *, #20009, .F. ) ;
#22691 = CARTESIAN_POINT ( 'NONE',  ( -18.24502636017238899, -100.7225776329765665, -2.500000000000000444 ) ) ;
#22693 = EDGE_CURVE ( 'NONE', #32056, #39300, #45869, .T. ) ;
#22692 = DIRECTION ( 'NONE',  ( 0.000000000000000000, 0.000000000000000000, 1.000000000000000000 ) ) ;
#22694 = DIRECTION ( 'NONE',  ( 0.000000000000000000, 0.8526401643540935105, -0.5224985647159466895 ) ) ;
#22695 = CARTESIAN_POINT ( 'NONE',  ( 94.99999999999998579, 93.05995642670504253, 87.30124999999999602 ) ) ;
#22696 = AXIS2_PLACEMENT_3D ( 'NONE', #5050, #27194, #11404 ) ;
#22697 = CARTESIAN_POINT ( 'NONE',  ( -92.69370383062498320, -211.3315407142195852, 86.73239583420047438 ) ) ;
#22698 = CARTESIAN_POINT ( 'NONE',  ( -94.99999999999997158, -213.0599564267049857, 81.90375000000000227 ) ) ;
#22699 = AXIS2_PLACEMENT_3D ( 'NONE', #30432, #35357, #65048 ) ;
#22700 = CARTESIAN_POINT ( 'NONE',  ( -92.35002509397746451, 88.47000729863293600, 89.07395733288676354 ) ) ;
#22701 = DIRECTION ( 'NONE',  ( 1.000000000000000000, 1.427937372958405461E-15, 7.962523111839130290E-16 ) ) ;
#22702 = EDGE_CURVE ( 'NONE', #61695, #20743, #25930, .T. ) ;
#22703 = EDGE_CURVE ( 'NONE', #62914, #16336, #55456, .T. ) ;
#22704 = CARTESIAN_POINT ( 'NONE',  ( 92.34999999999999432, 90.00000000000002842, 89.36499999999999488 ) ) ;
#22705 = ORIENTED_EDGE ( 'NONE', *, *, #37349, .F. ) ;
#22706 = AXIS2_PLACEMENT_3D ( 'NONE', #45519, #10534, #62818 ) ;
#22707 = ORIENTED_EDGE ( 'NONE', *, *, #70119, .T. ) ;
#22708 = AXIS2_PLACEMENT_3D ( 'NONE', #51566, #39930, #56481 ) ;
#22709 = CARTESIAN_POINT ( 'NONE',  ( -96.32500000000001705, 92.29496732002878900, 79.09916666666666174 ) ) ;
#22710 = DIRECTION ( 'NONE',  ( -1.000000000000000000, -0.000000000000000000, 0.000000000000000000 ) ) ;
#22711 = ADVANCED_FACE ( 'NONE', ( #47753 ), #30454, .F. ) ;
#22712 = CARTESIAN_POINT ( 'NONE',  ( 11.99999999999999822, 0.000000000000000000, 0.000000000000000000 ) ) ;
#22713 = CARTESIAN_POINT ( 'NONE',  ( 0.000000000000000000, 16.23288003029497162, 33.80338159004289622 ) ) ;
#22714 = CARTESIAN_POINT ( 'NONE',  ( -92.34999999999999432, -209.9999999999999716, 89.68250000000000455 ) ) ;
#22715 = CYLINDRICAL_SURFACE ( 'NONE', #27711, 82.00000000000000000 ) ;
#22716 = CARTESIAN_POINT ( 'NONE',  ( -97.64999999999996305, -209.9999999999999716, 79.83999999999998920 ) ) ;
#22717 = CIRCLE ( 'NONE', #15494, 82.00000000000000000 ) ;
#22718 = ORIENTED_EDGE ( 'NONE', *, *, #16450, .T. ) ;
#22719 = CARTESIAN_POINT ( 'NONE',  ( -93.84685191531254134, 91.99731107132950569, 78.00114583420048575 ) ) ;
#22720 = ADVANCED_FACE ( 'NONE', ( #27408 ), #27031, .T. ) ;
#22721 = FACE_OUTER_BOUND ( 'NONE', #11444, .T. ) ;
#22722 = LINE ( 'NONE', #23452, #28214 ) ;
#22723 = CYLINDRICAL_SURFACE ( 'NONE', #14174, 77.49899999999999523 ) ;
#22724 = DIRECTION ( 'NONE',  ( -1.000000000000000000, 0.000000000000000000, 0.000000000000000000 ) ) ;
#22725 = LINE ( 'NONE', #40009, #30490 ) ;
#22726 = DIRECTION ( 'NONE',  ( -1.000000000000000000, -0.000000000000000000, -0.000000000000000000 ) ) ;
#22727 = VECTOR ( 'NONE', #31998, 1000.000000000000000 ) ;
#22728 = PRESENTATION_LAYER_ASSIGNMENT (  '', '', ( #35908 ) ) ;
#22729 = CARTESIAN_POINT ( 'NONE',  ( 96.15314808468748708, 88.00268892867053694, 77.94822916753382458 ) ) ;
#22730 = CIRCLE ( 'NONE', #17934, 82.00000000000000000 ) ;
#22731 = AXIS2_PLACEMENT_3D ( 'NONE', #1860, #47674, #36760 ) ;
#22732 = CARTESIAN_POINT ( 'NONE',  ( -92.69370383062498320, -208.6684592857803295, 79.37697916753381833 ) ) ;
#22733 = DIRECTION ( 'NONE',  ( -1.000000000000000000, -0.000000000000000000, 0.000000000000000000 ) ) ;
#22734 = ORIENTED_EDGE ( 'NONE', *, *, #39381, .T. ) ;
#22735 = DIRECTION ( 'NONE',  ( 0.000000000000000000, 0.000000000000000000, 1.000000000000000000 ) ) ;
#22736 = DIRECTION ( 'NONE',  ( -1.000000000000000000, 0.000000000000000000, -0.000000000000000000 ) ) ;
#22737 = AXIS2_PLACEMENT_3D ( 'NONE', #16863, #5593, #56342 ) ;
#22738 = CARTESIAN_POINT ( 'NONE',  ( 0.000000000000000000, 0.000000000000000000, -184.9999999999999432 ) ) ;
#22739 = VECTOR ( 'NONE', #56374, 1000.000000000000000 ) ;
#22740 = FACE_OUTER_BOUND ( 'NONE', #64570, .T. ) ;
#22741 = CARTESIAN_POINT ( 'NONE',  ( 93.84685191531251292, -211.9973110713294489, 81.49364583420047836 ) ) ;
#22742 = EDGE_LOOP ( 'NONE', ( #37639, #72388, #22967, #38432 ) ) ;
#22743 = CARTESIAN_POINT ( 'NONE',  ( -3.702536634196095910, 8.043911037661889196, 52.00000000000002132 ) ) ;
#22744 = ORIENTED_EDGE ( 'NONE', *, *, #43136, .F. ) ;
#22745 = CARTESIAN_POINT ( 'NONE',  ( 10.00000000000000000, 21.32104025579158701, -30.84782396557194772 ) ) ;
#22746 = ORIENTED_EDGE ( 'NONE', *, *, #15779, .F. ) ;
#22747 = VECTOR ( 'NONE', #72137, 1000.000000000000000 ) ;
#22748 = EDGE_CURVE ( 'NONE', #73349, #42391, #1415, .T. ) ;
#22749 = DIRECTION ( 'NONE',  ( -1.000000000000000000, 0.000000000000000000, 0.000000000000000000 ) ) ;
#22750 = AXIS2_PLACEMENT_3D ( 'NONE', #65700, #25834, #41644 ) ;
#22751 = CIRCLE ( 'NONE', #64774, 31.99999999999999645 ) ;
#22752 = ADVANCED_FACE ( 'NONE', ( #27791 ), #15851, .T. ) ;
#22753 = ORIENTED_EDGE ( 'NONE', *, *, #28076, .T. ) ;
#22754 = ORIENTED_EDGE ( 'NONE', *, *, #3101, .T. ) ;
#22756 = ADVANCED_FACE ( 'NONE', ( #67276 ), #15018, .T. ) ;
#22755 = VERTEX_POINT ( 'NONE', #38706 ) ;
#22757 = AXIS2_PLACEMENT_3D ( 'NONE', #13916, #59066, #31219 ) ;
#22758 = ADVANCED_FACE ( 'NONE', ( #68018 ), #66539, .T. ) ;
#22759 = CARTESIAN_POINT ( 'NONE',  ( 0.000000000000000000, 0.000000000000000000, 0.000000000000000000 ) ) ;
#22760 = ORIENTED_EDGE ( 'NONE', *, *, #22326, .T. ) ;
#22761 = DIRECTION ( 'NONE',  ( -1.000000000000000000, 0.000000000000000000, 0.000000000000000000 ) ) ;
#22762 = ORIENTED_EDGE ( 'NONE', *, *, #51789, .F. ) ;
#22763 = CARTESIAN_POINT ( 'NONE',  ( 93.84685191531248449, 91.99731107132950569, 82.07572916753382231 ) ) ;
#22764 = CARTESIAN_POINT ( 'NONE',  ( 97.64999999999999147, -209.9999999999999716, 78.25249999999999773 ) ) ;
#22765 = ORIENTED_EDGE ( 'NONE', *, *, #49900, .F. ) ;
#22766 = VERTEX_POINT ( 'NONE', #67646 ) ;
#22767 = EDGE_LOOP ( 'NONE', ( #28120, #26012, #43756, #2547, #52416 ) ) ;
#22768 = EDGE_LOOP ( 'NONE', ( #57365, #2143, #23481, #45311 ) ) ;
#22769 = CARTESIAN_POINT ( 'NONE',  ( 0.000000000000000000, 81.34940948281351325, -10.30890764327296161 ) ) ;
#22770 = CARTESIAN_POINT ( 'NONE',  ( 10.00000000000000000, 30.80686688397010542, 21.53537804866092387 ) ) ;
#22771 = DIRECTION ( 'NONE',  ( 0.000000000000000000, 0.000000000000000000, 1.000000000000000000 ) ) ;
#22772 = EDGE_CURVE ( 'NONE', #40406, #28951, #33804, .T. ) ;
#22773 = DIRECTION ( 'NONE',  ( 0.000000000000000000, 0.000000000000000000, 1.000000000000000000 ) ) ;
#22774 = CARTESIAN_POINT ( 'NONE',  ( -92.34999999999999432, -209.9999999999999716, 87.14249999999999829 ) ) ;
#22775 = CARTESIAN_POINT ( 'NONE',  ( 10.00000000000000000, -29.81001611430991360, -22.74946021919165418 ) ) ;
#22776 = EDGE_CURVE ( 'NONE', #63927, #2660, #21902, .T. ) ;
#22777 = ORIENTED_EDGE ( 'NONE', *, *, #15006, .T. ) ;
#22778 = CARTESIAN_POINT ( 'NONE',  ( -94.99999999999997158, -206.9400435732949575, 81.66562500173431260 ) ) ;
#22779 = ORIENTED_EDGE ( 'NONE', *, *, #46325, .T. ) ;
#22780 = CARTESIAN_POINT ( 'NONE',  ( 7.400000000000003908, 1.056673655987569448E-14, 5.892267102770835596E-15 ) ) ;
#22781 = VERTEX_POINT ( 'NONE', #60895 ) ;
#22783 = CARTESIAN_POINT ( 'NONE',  ( -92.35000000000003695, 90.00000000000004263, 78.96687500173429441 ) ) ;
#22782 = CARTESIAN_POINT ( 'NONE',  ( 94.99999999999998579, 93.05995642670504253, 77.85562500173429612 ) ) ;
#22784 = CIRCLE ( 'NONE', #25185, 16.00000000000000355 ) ;
#22785 = ORIENTED_EDGE ( 'NONE', *, *, #49289, .F. ) ;
#22786 = CARTESIAN_POINT ( 'NONE',  ( 96.15314808468748708, 88.00268892867053694, 82.39322916753381776 ) ) ;
#22787 = CARTESIAN_POINT ( 'NONE',  ( 11.99999999999999822, 44.99326035066149387, -68.55367621811095091 ) ) ;
#22788 = LINE ( 'NONE', #4764, #15087 ) ;
#22789 = CIRCLE ( 'NONE', #73149, 37.49900000000000233 ) ;
#22790 = DIRECTION ( 'NONE',  ( 0.000000000000000000, 1.000000000000000000, 0.000000000000000000 ) ) ;
#22791 = CARTESIAN_POINT ( 'NONE',  ( 97.64999999999447766, 89.99999459739470353, 81.50687481489491404 ) ) ;
#22792 = AXIS2_PLACEMENT_3D ( 'NONE', #9081, #26371, #49663 ) ;
#22793 = DIRECTION ( 'NONE',  ( 0.000000000000000000, 0.000000000000000000, -1.000000000000000000 ) ) ;
#22794 = VERTEX_POINT ( 'NONE', #3769 ) ;
#22795 = DIRECTION ( 'NONE',  ( -1.000000000000000000, 0.000000000000000000, -0.000000000000000000 ) ) ;
#22796 = DIRECTION ( 'NONE',  ( 1.000000000000000000, -0.000000000000000000, -0.000000000000000000 ) ) ;
#22797 = ADVANCED_FACE ( 'NONE', ( #10493 ), #39454, .F. ) ;
#22798 = EDGE_CURVE ( 'NONE', #58538, #38048, #9039, .T. ) ;
#22799 = CARTESIAN_POINT ( 'NONE',  ( -7.500000000000014211, -69.70000000000001705, -204.9999999999999716 ) ) ;
#22800 = ORIENTED_EDGE ( 'NONE', *, *, #32496, .F. ) ;
#22801 = ORIENTED_EDGE ( 'NONE', *, *, #27035, .F. ) ;
#22802 = CIRCLE ( 'NONE', #16781, 31.99999999999998934 ) ;
#22803 = DIRECTION ( 'NONE',  ( 0.000000000000000000, 0.8090169943749486725, -0.5877852522924713607 ) ) ;
#22804 = FACE_OUTER_BOUND ( 'NONE', #50111, .T. ) ;
#22805 = LINE ( 'NONE', #21670, #46161 ) ;
#22806 = CARTESIAN_POINT ( 'NONE',  ( -96.15314808468745866, -211.9973110713294489, 81.65239583420049030 ) ) ;
#22807 = ORIENTED_EDGE ( 'NONE', *, *, #32557, .T. ) ;
#22808 = ORIENTED_EDGE ( 'NONE', *, *, #53406, .T. ) ;
#22809 = AXIS2_PLACEMENT_3D ( 'NONE', #20923, #9274, #38216 ) ;
#22810 = CARTESIAN_POINT ( 'NONE',  ( 10.00000000000000000, 35.95386929396256903, -10.96151621346501237 ) ) ;
#22811 = VECTOR ( 'NONE', #46813, 1000.000000000000000 ) ;
#22812 = CARTESIAN_POINT ( 'NONE',  ( -26.29030328629083968, -123.6496510949466341, 5.500000000000000000 ) ) ;
#22813 = DIRECTION ( 'NONE',  ( 0.000000000000000000, 0.000000000000000000, 1.000000000000000000 ) ) ;
#22814 = FACE_OUTER_BOUND ( 'NONE', #71969, .T. ) ;
#22815 = DIRECTION ( 'NONE',  ( 0.000000000000000000, 0.000000000000000000, 1.000000000000000000 ) ) ;
#22816 = CARTESIAN_POINT ( 'NONE',  ( 93.67499999999999716, 87.70503267997126784, 78.12020833506763040 ) ) ;
#22817 = CARTESIAN_POINT ( 'NONE',  ( 15.00000000000000000, 18.84667830672605859, 18.68964196561243796 ) ) ;
#22818 = CARTESIAN_POINT ( 'NONE',  ( 20.85212586905262100, -130.9402397935870965, 5.500000000000000000 ) ) ;
#22819 = CARTESIAN_POINT ( 'NONE',  ( 100.0000000000260201, 95.00000000000001421, -65.00000000000001421 ) ) ;
#22820 = CARTESIAN_POINT ( 'NONE',  ( 0.000000000000000000, -74.18225833017913828, 34.94270380257611919 ) ) ;
#22821 = CARTESIAN_POINT ( 'NONE',  ( 93.84685191531248449, 91.99731107132950569, 85.88572916753381037 ) ) ;
#22822 = CARTESIAN_POINT ( 'NONE',  ( -93.84685191531247028, -211.9973110713294489, 88.74322916753382628 ) ) ;
#22823 = CARTESIAN_POINT ( 'NONE',  ( 92.34999999999999432, 90.00000000000002842, 82.37999999999999545 ) ) ;
#22824 = VERTEX_POINT ( 'NONE', #32673 ) ;
#22825 = CARTESIAN_POINT ( 'NONE',  ( 10.00000000000000000, 22.64427369931169309, 30.00120703465213623 ) ) ;
#22826 = CARTESIAN_POINT ( 'NONE',  ( -92.69370383062505425, 88.66845928578038638, 78.47739583420047893 ) ) ;
#22827 = CARTESIAN_POINT ( 'NONE',  ( 96.15314808468748708, -208.0026889286704943, 89.43114583420047836 ) ) ;
#22828 = ORIENTED_EDGE ( 'NONE', *, *, #58638, .T. ) ;
#22830 = CARTESIAN_POINT ( 'NONE',  ( -26.29030328629083968, -123.6496510949466341, -5.500000000000000000 ) ) ;
#22829 = CIRCLE ( 'NONE', #19208, 77.49899999999999523 ) ;
#22831 = DIRECTION ( 'NONE',  ( -0.3420201433256714330, 4.188538737677025045E-17, 0.9396926207859073177 ) ) ;
#22832 = LINE ( 'NONE', #45775, #39577 ) ;
#22833 = EDGE_CURVE ( 'NONE', #70414, #43461, #4892, .T. ) ;
#22834 = CIRCLE ( 'NONE', #64859, 82.00000000000000000 ) ;
#22835 = EDGE_CURVE ( 'NONE', #3025, #9804, #32679, .T. ) ;
#22836 = CARTESIAN_POINT ( 'NONE',  ( 0.000000000000000000, -21.40280677340345505, -36.13751322684441192 ) ) ;
#22837 = CARTESIAN_POINT ( 'NONE',  ( 0.000000000000000000, 55.16347631943042984, 60.67117009219157353 ) ) ;
#22838 = EDGE_CURVE ( 'NONE', #56792, #38016, #4509, .T. ) ;
#22839 = CIRCLE ( 'NONE', #64865, 2.650000000000540812 ) ;
#22840 = ORIENTED_EDGE ( 'NONE', *, *, #9985, .F. ) ;
#22841 = ORIENTED_EDGE ( 'NONE', *, *, #52210, .F. ) ;
#22842 = ADVANCED_FACE ( 'NONE', ( #57483 ), #11976, .T. ) ;
#22843 = CARTESIAN_POINT ( 'NONE',  ( 97.30629616937498838, -208.6684592857803295, 85.72697916753381264 ) ) ;
#22844 = CARTESIAN_POINT ( 'NONE',  ( 92.35000000000000853, -209.9999999999999716, 89.44437500173430067 ) ) ;
#22845 = CYLINDRICAL_SURFACE ( 'NONE', #25563, 11.59999999999999787 ) ;
#22846 = CARTESIAN_POINT ( 'NONE',  ( -96.32499999999996021, -207.7050326799711968, 85.52854166840096184 ) ) ;
#22847 = CARTESIAN_POINT ( 'NONE',  ( 11.99999999999999822, 75.16055320797030959, 18.89407956138283851 ) ) ;
#22848 = EDGE_CURVE ( 'NONE', #29316, #57242, #5997, .T. ) ;
#22849 = CARTESIAN_POINT ( 'NONE',  ( 0.000000000000000000, 16.83928648764945279, -16.46020748918028076 ) ) ;
#22850 = CARTESIAN_POINT ( 'NONE',  ( 97.64999999999997726, -211.5299782133524502, 89.62958333333332916 ) ) ;
#22851 = AXIS2_PLACEMENT_3D ( 'NONE', #73908, #23167, #61905 ) ;
#22852 = ORIENTED_EDGE ( 'NONE', *, *, #44259, .T. ) ;
#22853 = ORIENTED_EDGE ( 'NONE', *, *, #55443, .F. ) ;
#22854 = ORIENTED_EDGE ( 'NONE', *, *, #21755, .F. ) ;
#22855 = CIRCLE ( 'NONE', #20426, 16.00000000000000000 ) ;
#22856 = VERTEX_POINT ( 'NONE', #41297 ) ;
#22857 = DIRECTION ( 'NONE',  ( -0.000000000000000000, -0.000000000000000000, -1.000000000000000000 ) ) ;
#22858 = VECTOR ( 'NONE', #31264, 1000.000000000000114 ) ;
#22859 = FILL_AREA_STYLE ('',( #65276 ) ) ;
#22860 = DIRECTION ( 'NONE',  ( -1.000000000000000000, -0.000000000000000000, 0.000000000000000000 ) ) ;
#22861 = AXIS2_PLACEMENT_3D ( 'NONE', #50761, #44394, #45523 ) ;
#22862 = CYLINDRICAL_SURFACE ( 'NONE', #37805, 3.299999999999997158 ) ;
#22863 = CARTESIAN_POINT ( 'NONE',  ( 97.64999999999997726, -211.5299782133524502, 77.00895833506763211 ) ) ;
#22865 = AXIS2_PLACEMENT_3D ( 'NONE', #23558, #17917, #40861 ) ;
#22864 = CARTESIAN_POINT ( 'NONE',  ( 97.64999999999997726, 91.52997821335252127, 83.38541666666667140 ) ) ;
#22866 = EDGE_CURVE ( 'NONE', #60498, #65293, #35637, .T. ) ;
#22867 = ORIENTED_EDGE ( 'NONE', *, *, #67586, .F. ) ;
#22868 = CARTESIAN_POINT ( 'NONE',  ( 6.782329983125270800, 10.49999999999999467, 20.00000000000000000 ) ) ;
#22869 = ORIENTED_EDGE ( 'NONE', *, *, #55273, .T. ) ;
#22870 = EDGE_CURVE ( 'NONE', #18595, #9035, #43516, .T. ) ;
#22871 = DIRECTION ( 'NONE',  ( 1.000000000000000000, 0.000000000000000000, 0.000000000000000000 ) ) ;
#22872 = ORIENTED_EDGE ( 'NONE', *, *, #48473, .T. ) ;
#22873 = LINE ( 'NONE', #64200, #48831 ) ;
#22874 = CARTESIAN_POINT ( 'NONE',  ( -97.30629616937501680, 90.00000000000004263, 82.18156250086715886 ) ) ;
#22875 = CARTESIAN_POINT ( 'NONE',  ( 97.30629616937498838, 91.33154071421968467, 76.67822916753378593 ) ) ;
#22876 = ORIENTED_EDGE ( 'NONE', *, *, #5219, .T. ) ;
#22877 = CYLINDRICAL_SURFACE ( 'NONE', #8135, 2.649999999999985700 ) ;
#22878 = DIRECTION ( 'NONE',  ( -1.000000000000000000, -0.000000000000000000, 0.000000000000000000 ) ) ;
#22879 = FACE_OUTER_BOUND ( 'NONE', #64258, .T. ) ;
#22880 = CARTESIAN_POINT ( 'NONE',  ( -92.34999999999993747, -208.4700217866475214, 77.67041666666666799 ) ) ;
#22881 = EDGE_LOOP ( 'NONE', ( #66751, #36245, #27644, #67300 ) ) ;
#22882 = CARTESIAN_POINT ( 'NONE',  ( 5.999999999999999112, -59.75363087400114637, 56.15606465354937171 ) ) ;
#22883 = EDGE_CURVE ( 'NONE', #48642, #22476, #5084, .T. ) ;
#22884 = ADVANCED_FACE ( 'NONE', ( #63142 ), #17623, .T. ) ;
#22885 = CARTESIAN_POINT ( 'NONE',  ( -94.99999999999997158, -207.3369185715606307, 76.14906250086716000 ) ) ;
#22886 = ORIENTED_EDGE ( 'NONE', *, *, #10382, .F. ) ;
#22887 = ORIENTED_EDGE ( 'NONE', *, *, #28004, .T. ) ;
#22888 = FACE_BOUND ( 'NONE', #24321, .T. ) ;
#22889 = VERTEX_POINT ( 'NONE', #22532 ) ;
#22890 = CARTESIAN_POINT ( 'NONE',  ( 10.00000000000000000, 30.00120703465205452, 22.64427369931179967 ) ) ;
#22891 = CARTESIAN_POINT ( 'NONE',  ( -97.64999999999996305, -209.9999999999999716, 77.93499999999998806 ) ) ;
#22892 = ORIENTED_EDGE ( 'NONE', *, *, #53898, .F. ) ;
#22893 = CARTESIAN_POINT ( 'NONE',  ( -92.69370383062498320, -211.3315407142195852, 75.30239583420048177 ) ) ;
#22894 = ORIENTED_EDGE ( 'NONE', *, *, #6858, .F. ) ;
#22895 = LINE ( 'NONE', #63856, #5081 ) ;
#22896 = CARTESIAN_POINT ( 'NONE',  ( 97.64999999999999147, 90.00000000000002842, 83.96750000000000114 ) ) ;
#22897 = CARTESIAN_POINT ( 'NONE',  ( -93.08359813425039420, -211.8303114255588753, 74.99954695036822727 ) ) ;
#22898 = DIRECTION ( 'NONE',  ( 0.000000000000000000, 0.000000000000000000, 1.000000000000000000 ) ) ;
#22899 = AXIS2_PLACEMENT_3D ( 'NONE', #22907, #16137, #5251 ) ;
#22900 = CARTESIAN_POINT ( 'NONE',  ( 0.000000000000000000, -62.20884554314051229, 46.21855187248609553 ) ) ;
#22901 = CIRCLE ( 'NONE', #19276, 82.00000000000000000 ) ;
#22902 = FILL_AREA_STYLE_COLOUR ( '', #64981 ) ;
#22904 = CARTESIAN_POINT ( 'NONE',  ( 92.69370383062498320, 91.33154071421968467, 83.87489583420047268 ) ) ;
#22903 = AXIS2_PLACEMENT_3D ( 'NONE', #47640, #12314, #41268 ) ;
#22905 = DIRECTION ( 'NONE',  ( -1.000000000000000000, -0.000000000000000000, -0.000000000000000000 ) ) ;
#22906 = DIRECTION ( 'NONE',  ( 0.000000000000000000, 0.000000000000000000, 1.000000000000000000 ) ) ;
#22907 = CARTESIAN_POINT ( 'NONE',  ( 11.99999999999999822, -41.76937507738831812, 62.50329211542423025 ) ) ;
#22908 = CARTESIAN_POINT ( 'NONE',  ( 7.543218489614351263, -11.91259227951415056, 0.000000000000000000 ) ) ;
#22909 = CARTESIAN_POINT ( 'NONE',  ( 11.99999999999999822, 16.65972982745045528, -80.28980883073741381 ) ) ;
#22910 = DIRECTION ( 'NONE',  ( 1.000000000000000000, 0.000000000000000000, 0.000000000000000000 ) ) ;
#22911 = DIRECTION ( 'NONE',  ( -1.000000000000000000, 0.000000000000000000, 0.000000000000000000 ) ) ;
#22912 =( BOUNDED_CURVE ( )  B_SPLINE_CURVE ( 2, ( #37423, #3222, #65997, #32495, #8470, #26493, #48683 ),
 .UNSPECIFIED., .F., .F. ) 
 B_SPLINE_CURVE_WITH_KNOTS ( ( 3, 2, 2, 3 ),
 ( 0.7083333333333331483, 0.7152777777777775681, 0.7222222222222220989, 0.7291666666666665186 ),
 .UNSPECIFIED. ) 
 CURVE ( )  GEOMETRIC_REPRESENTATION_ITEM ( )  RATIONAL_B_SPLINE_CURVE ( ( 1.000000000000004219, 0.8660254037844343777, 1.000000000000000000, 0.8660254037844387076, 1.000000000000000000, 0.8660254037844408170, 0.9999999999999978906 ) ) 
 REPRESENTATION_ITEM ( '' )  );
#22913 = DIRECTION ( 'NONE',  ( 1.000000000000000000, -0.000000000000000000, 0.000000000000000000 ) ) ;
#22914 = EDGE_CURVE ( 'NONE', #63709, #58611, #71099, .T. ) ;
#22915 = VECTOR ( 'NONE', #55238, 1000.000000000000000 ) ;
#22916 = DIRECTION ( 'NONE',  ( -0.000000000000000000, -0.000000000000000000, -1.000000000000000000 ) ) ;
#22917 = CARTESIAN_POINT ( 'NONE',  ( -92.69370383062504004, 90.00000000000004263, 89.32531250086714181 ) ) ;
#22918 = AXIS2_PLACEMENT_3D ( 'NONE', #6056, #18056, #27845 ) ;
#22919 = DIRECTION ( 'NONE',  ( -1.000000000000000000, 0.000000000000000000, -0.000000000000000000 ) ) ;
#22920 = AXIS2_PLACEMENT_3D ( 'NONE', #48472, #32275, #54851 ) ;
#22921 = EDGE_CURVE ( 'NONE', #47629, #26649, #34175, .T. ) ;
#22922 = EDGE_CURVE ( 'NONE', #62534, #12399, #11078, .T. ) ;
#22923 = LINE ( 'NONE', #6008, #35653 ) ;
#22924 = EDGE_CURVE ( 'NONE', #8777, #51805, #62725, .T. ) ;
#22925 = ORIENTED_EDGE ( 'NONE', *, *, #29551, .F. ) ;
#22926 = CYLINDRICAL_SURFACE ( 'NONE', #55157, 31.99999999999998579 ) ;
#22927 = CARTESIAN_POINT ( 'NONE',  ( -23.54415474984308787, -120.4156646670583086, -5.500000000000000000 ) ) ;
#22928 = LINE ( 'NONE', #50359, #55054 ) ;
#22929 = EDGE_CURVE ( 'NONE', #25052, #3791, #41080, .T. ) ;
#22930 = CARTESIAN_POINT ( 'NONE',  ( 2.499999999999979572, -80.00000000000000000, -280.0000000000000000 ) ) ;
#22931 = CYLINDRICAL_SURFACE ( 'NONE', #21205, 42.00000000000000000 ) ;
#22932 = CARTESIAN_POINT ( 'NONE',  ( 97.30629616937498838, -209.9999999999999716, 85.67406250086715147 ) ) ;
#22933 = ORIENTED_EDGE ( 'NONE', *, *, #41012, .F. ) ;
#22934 = ORIENTED_EDGE ( 'NONE', *, *, #36644, .F. ) ;
#22935 = CARTESIAN_POINT ( 'NONE',  ( 0.000000000000000000, -5.256550761632340141, -77.32052557432847095 ) ) ;
#22936 = ORIENTED_EDGE ( 'NONE', *, *, #23838, .T. ) ;
#22937 = FACE_OUTER_BOUND ( 'NONE', #59821, .T. ) ;
#22938 = CARTESIAN_POINT ( 'NONE',  ( 97.30629616937498838, -209.9999999999999716, 77.89531250086714920 ) ) ;
#22939 = EDGE_CURVE ( 'NONE', #5395, #45876, #58211, .T. ) ;
#22940 = ORIENTED_EDGE ( 'NONE', *, *, #63102, .T. ) ;
#22941 = CARTESIAN_POINT ( 'NONE',  ( 92.69370383062501162, -211.3315407142195852, 84.13947916753383538 ) ) ;
#22942 = AXIS2_PLACEMENT_3D ( 'NONE', #37760, #31728, #32097 ) ;
#22943 = EDGE_LOOP ( 'NONE', ( #18920, #29406, #40702, #64202 ) ) ;
#22944 = CARTESIAN_POINT ( 'NONE',  ( -96.32499999999996021, -212.2949673200287179, 88.20083333333332121 ) ) ;
#22945 = ORIENTED_EDGE ( 'NONE', *, *, #73510, .T. ) ;
#22946 = AXIS2_PLACEMENT_3D ( 'NONE', #9565, #31375, #3948 ) ;
#22947 = ORIENTED_EDGE ( 'NONE', *, *, #2113, .T. ) ;
#22948 = DIRECTION ( 'NONE',  ( -0.7585478161175716050, -0.6516173805718067369, 0.000000000000000000 ) ) ;
#22949 = CARTESIAN_POINT ( 'NONE',  ( 10.00000000000000000, -56.15606465354917987, -59.75363087400133111 ) ) ;
#22950 = ORIENTED_EDGE ( 'NONE', *, *, #56947, .T. ) ;
#22951 = CARTESIAN_POINT ( 'NONE',  ( -92.35000000000003695, 90.00000000000004263, 77.61749999999999261 ) ) ;
#22952 = CARTESIAN_POINT ( 'NONE',  ( 96.32499999999998863, -207.7050326799711968, 87.32770833506762642 ) ) ;
#22953 = EDGE_CURVE ( 'NONE', #34118, #5113, #30274, .T. ) ;
#22954 = ORIENTED_EDGE ( 'NONE', *, *, #57322, .T. ) ;
#22955 = DIRECTION ( 'NONE',  ( -2.603472992745699578E-14, 2.546204323184531851E-14, -1.000000000000000000 ) ) ;
#22956 = EDGE_CURVE ( 'NONE', #47239, #21165, #63948, .T. ) ;
#22957 = ORIENTED_EDGE ( 'NONE', *, *, #13312, .T. ) ;
#22958 = DIRECTION ( 'NONE',  ( 0.000000000000000000, -0.3090169943749350168, -0.9510565162951576390 ) ) ;
#22959 = EDGE_CURVE ( 'NONE', #52520, #48721, #46567, .T. ) ;
#22960 = ORIENTED_EDGE ( 'NONE', *, *, #69177, .T. ) ;
#22961 = AXIS2_PLACEMENT_3D ( 'NONE', #65335, #58956, #35628 ) ;
#22962 = ORIENTED_EDGE ( 'NONE', *, *, #45634, .T. ) ;
#22963 = ORIENTED_EDGE ( 'NONE', *, *, #56789, .T. ) ;
#22964 = DIRECTION ( 'NONE',  ( -1.000000000000000000, 0.000000000000000000, 0.000000000000000000 ) ) ;
#22965 = AXIS2_PLACEMENT_3D ( 'NONE', #70105, #58105, #24266 ) ;
#22966 = CARTESIAN_POINT ( 'NONE',  ( -5.000000000000000000, -1.349638343847294752, -0.8687551798607462405 ) ) ;
#22967 = ORIENTED_EDGE ( 'NONE', *, *, #3191, .F. ) ;
#22968 = AXIS2_PLACEMENT_3D ( 'NONE', #13056, #58942, #42020 ) ;
#22969 = ORIENTED_EDGE ( 'NONE', *, *, #71813, .T. ) ;
#22970 = VERTEX_POINT ( 'NONE', #46941 ) ;
#22971 = CARTESIAN_POINT ( 'NONE',  ( 92.35000000000009379, -211.5299782133524502, 76.08291666666664810 ) ) ;
#22972 = AXIS2_PLACEMENT_3D ( 'NONE', #35288, #46569, #69498 ) ;
#22973 = DIRECTION ( 'NONE',  ( -1.000000000000000000, -0.000000000000000000, 0.000000000000000000 ) ) ;
#22974 = CARTESIAN_POINT ( 'NONE',  ( -95.00000000000002842, 93.05995642670501411, 86.66624999999999091 ) ) ;
#22975 = EDGE_LOOP ( 'NONE', ( #43942, #67727, #43001, #70809 ) ) ;
#22976 = LINE ( 'NONE', #45907, #39486 ) ;
#22977 = ORIENTED_EDGE ( 'NONE', *, *, #53907, .F. ) ;
#22978 = CARTESIAN_POINT ( 'NONE',  ( -5.565113727472241756, 10.17789316117534959, 42.00000000000001421 ) ) ;
#22979 = CARTESIAN_POINT ( 'NONE',  ( -97.30629616937497417, -208.6684592857803011, 84.50989583420046358 ) ) ;
#22980 = VERTEX_POINT ( 'NONE', #69855 ) ;
#22981 = CARTESIAN_POINT ( 'NONE',  ( 0.000000000000000000, -34.44570377933648331, 69.42325613327426481 ) ) ;
#22982 = DIRECTION ( 'NONE',  ( 0.000000000000000000, 0.6494480483301793283, 0.7604059656000345946 ) ) ;
#22983 = DIRECTION ( 'NONE',  ( -1.000000000000000000, 0.000000000000000000, 0.000000000000000000 ) ) ;
#22984 = CARTESIAN_POINT ( 'NONE',  ( -97.30629616937495996, -209.9999999999999716, 75.03781250086713328 ) ) ;
#22985 = CYLINDRICAL_SURFACE ( 'NONE', #42279, 82.00000000000000000 ) ;
#22986 = DIRECTION ( 'NONE',  ( -1.000000000000000000, -0.000000000000000000, 0.000000000000000000 ) ) ;
#22987 = CARTESIAN_POINT ( 'NONE',  ( 10.00000000000000000, -30.84782396557233142, 21.32104025579104345 ) ) ;
#22988 = FACE_OUTER_BOUND ( 'NONE', #38183, .T. ) ;
#22989 = CARTESIAN_POINT ( 'NONE',  ( 0.000000000000000000, 26.79245525562714292, 32.34446384429980981 ) ) ;
#22990 = EDGE_CURVE ( 'NONE', #27599, #13677, #64236, .T. ) ;
#22991 = CARTESIAN_POINT ( 'NONE',  ( -95.00000000000002842, 92.66308142843932671, 77.41906250086714181 ) ) ;
#22992 = CARTESIAN_POINT ( 'NONE',  ( 12.00000000000000000, 20.85821328998756385, 10.92862929874494249 ) ) ;
#22993 = CARTESIAN_POINT ( 'NONE',  ( 0.000000000000000000, -59.03342792756297541, 46.54456581323783126 ) ) ;
#22994 = EDGE_LOOP ( 'NONE', ( #18145, #32910 ) ) ;
#22995 = CARTESIAN_POINT ( 'NONE',  ( 93.67499999999999716, 87.70503267997126784, 79.39020833506762642 ) ) ;
#22996 = VECTOR ( 'NONE', #8841, 1000.000000000000000 ) ;
#22997 = CIRCLE ( 'NONE', #30167, 82.00000000000000000 ) ;
#22998 = AXIS2_PLACEMENT_3D ( 'NONE', #11971, #16505, #22150 ) ;
#22999 = CARTESIAN_POINT ( 'NONE',  ( 92.35000000000000853, -209.9999999999999716, 89.44437500173430067 ) ) ;
#23000 = DIRECTION ( 'NONE',  ( -0.6575728627325955200, 0.7533909544171996098, 1.230411769795008318E-16 ) ) ;
#23001 = DIRECTION ( 'NONE',  ( 0.000000000000000000, 0.000000000000000000, 1.000000000000000000 ) ) ;
#23002 = VECTOR ( 'NONE', #2405, 1000.000000000000000 ) ;
#23003 = DIRECTION ( 'NONE',  ( -7.381802025433090153E-16, -1.065814103640131188E-14, -1.000000000000000000 ) ) ;
#23004 = CARTESIAN_POINT ( 'NONE',  ( -93.84685191531248449, -208.0026889286704943, 78.79489583420048859 ) ) ;
#23005 = EDGE_CURVE ( 'NONE', #17672, #39865, #27865, .T. ) ;
#23006 = EDGE_CURVE ( 'NONE', #64863, #51313, #68401, .T. ) ;
#23007 = AXIS2_PLACEMENT_3D ( 'NONE', #58459, #6954, #34798 ) ;
#23008 = DIRECTION ( 'NONE',  ( 0.000000000000000000, -0.3826834323650970537, 0.9238795325112838519 ) ) ;
#23009 = ORIENTED_EDGE ( 'NONE', *, *, #6471, .F. ) ;
#23010 = FACE_OUTER_BOUND ( 'NONE', #6656, .T. ) ;
#23011 = LINE ( 'NONE', #51567, #21473 ) ;
#23012 = LINE ( 'NONE', #16993, #34548 ) ;
#23013 = EDGE_CURVE ( 'NONE', #9893, #21904, #7472, .T. ) ;
#23014 = FACE_OUTER_BOUND ( 'NONE', #40043, .T. ) ;
#23015 = EDGE_CURVE ( 'NONE', #13138, #54220, #17089, .T. ) ;
#23016 = AXIS2_PLACEMENT_3D ( 'NONE', #34703, #1289, #68930 ) ;
#23017 = VECTOR ( 'NONE', #3644, 1000.000000000000000 ) ;
#23018 = SHAPE_REPRESENTATION ( 'torque nut 03_iso_ISO 7042-M6-N', ( #43395 ), #47140 ) ;
#23019 = CARTESIAN_POINT ( 'NONE',  ( 0.000000000000000000, 0.000000000000000000, -125.0000000000000000 ) ) ;
#23020 = ORIENTED_EDGE ( 'NONE', *, *, #5196, .T. ) ;
#23021 = CARTESIAN_POINT ( 'NONE',  ( 10.00000000000000000, -39.04073710021333454, -15.48615015657624738 ) ) ;
#23022 = EDGE_LOOP ( 'NONE', ( #59141, #4244, #7953, #62668 ) ) ;
#23023 = CARTESIAN_POINT ( 'NONE',  ( 92.69370383062501162, -208.6684592857803295, 87.68489583420047495 ) ) ;
#23024 = CARTESIAN_POINT ( 'NONE',  ( -93.67499999999998295, -207.7050326799711968, 83.51770833506763836 ) ) ;
#23025 = ADVANCED_FACE ( 'NONE', ( #30734 ), #7453, .F. ) ;
#23026 = ORIENTED_EDGE ( 'NONE', *, *, #64604, .F. ) ;
#23027 = LINE ( 'NONE', #52318, #33249 ) ;
#23028 = ORIENTED_EDGE ( 'NONE', *, *, #15186, .T. ) ;
#23029 = CARTESIAN_POINT ( 'NONE',  ( 10.00000000000000000, 0.000000000000000000, 0.000000000000000000 ) ) ;
#23030 = ORIENTED_EDGE ( 'NONE', *, *, #13475, .T. ) ;
#23031 = DIRECTION ( 'NONE',  ( -0.9781476007338069101, 0.2079116908177532363, 0.000000000000000000 ) ) ;
#23032 = EDGE_LOOP ( 'NONE', ( #18382, #43413, #34392, #22312 ) ) ;
#23033 = DIRECTION ( 'NONE',  ( 0.000000000000000000, -0.1564344650402382242, 0.9876883405951366601 ) ) ;
#23034 = ORIENTED_EDGE ( 'NONE', *, *, #54518, .T. ) ;
#23035 = ORIENTED_EDGE ( 'NONE', *, *, #60584, .F. ) ;
#23036 = CARTESIAN_POINT ( 'NONE',  ( 11.99999999999999822, -81.50828551894220197, -8.966570791701590437 ) ) ;
#23037 = EDGE_CURVE ( 'NONE', #50966, #65467, #13474, .T. ) ;
#23038 = ADVANCED_FACE ( 'NONE', ( #36016 ), #19462, .T. ) ;
#23039 = VERTEX_POINT ( 'NONE', #7078 ) ;
#23040 = PRODUCT_DEFINITION_SHAPE ( 'NONE', 'NONE',  #74374 ) ;
#23041 = EDGE_CURVE ( 'NONE', #43028, #24049, #30369, .T. ) ;
#23042 = ORIENTED_EDGE ( 'NONE', *, *, #41191, .F. ) ;
#23043 = LINE ( 'NONE', #58722, #44437 ) ;
#23044 = EDGE_LOOP ( 'NONE', ( #56034, #59547, #34674, #12365 ) ) ;
#23045 = MECHANICAL_DESIGN_GEOMETRIC_PRESENTATION_REPRESENTATION (  '', ( #2685 ), #6257 ) ;
#23046 = ORIENTED_EDGE ( 'NONE', *, *, #52008, .T. ) ;
#23047 = CARTESIAN_POINT ( 'NONE',  ( 97.30629616937498838, 88.66845928578037217, 86.73239583420047438 ) ) ;
#23048 = VERTEX_POINT ( 'NONE', #24739 ) ;
#23049 = CARTESIAN_POINT ( 'NONE',  ( 93.84685191531249870, -208.0026889286704943, 82.55197916753380127 ) ) ;
#23050 = ITEM_DEFINED_TRANSFORMATION ( 'NONE', 'NONE', #44828,  #43395 ) ;
#23051 = CARTESIAN_POINT ( 'NONE',  ( 0.000000000000000000, 0.000000000000000000, 0.000000000000000000 ) ) ;
#23053 = LINE ( 'NONE', #28668, #48605 ) ;
#23052 = AXIS2_PLACEMENT_3D ( 'NONE', #38330, #22157, #72523 ) ;
#23054 = DIRECTION ( 'NONE',  ( -0.000000000000000000, -0.000000000000000000, 1.000000000000000000 ) ) ;
#23055 = CARTESIAN_POINT ( 'NONE',  ( -93.67499999999998295, -207.7050326799711968, 89.15333333333333599 ) ) ;
#23056 = CARTESIAN_POINT ( 'NONE',  ( 97.64999999999999147, 90.00000000000002842, 90.00000000000000000 ) ) ;
#23057 = DIRECTION ( 'NONE',  ( -1.000000000000000000, -0.000000000000000000, -0.000000000000000000 ) ) ;
#23058 = CARTESIAN_POINT ( 'NONE',  ( -93.84685191531247028, -211.9973110713294489, 85.40947916753380298 ) ) ;
#23059 = CARTESIAN_POINT ( 'NONE',  ( -93.84685191531252713, 88.00268892867056536, 83.66322916753382799 ) ) ;
#23060 = AXIS2_PLACEMENT_3D ( 'NONE', #2101, #65595, #42659 ) ;
#23061 = ORIENTED_EDGE ( 'NONE', *, *, #20014, .T. ) ;
#23063 = CARTESIAN_POINT ( 'NONE',  ( -97.30629616937501680, 88.66845928578038638, 84.61572916753380014 ) ) ;
#23062 = CARTESIAN_POINT ( 'NONE',  ( 93.84685191531248449, 91.99731107132950569, 85.72697916753379843 ) ) ;
#23064 = CIRCLE ( 'NONE', #67483, 16.00000000000000000 ) ;
#23065 = EDGE_LOOP ( 'NONE', ( #60860, #3083, #24859 ) ) ;
#23066 = CARTESIAN_POINT ( 'NONE',  ( -92.35000000000003695, 90.00000000000004263, 78.96687500173429441 ) ) ;
#23067 = CARTESIAN_POINT ( 'NONE',  ( 95.00000000000000000, -213.0599564267049857, 76.26812500173430465 ) ) ;
#23068 = DIRECTION ( 'NONE',  ( -1.000000000000000000, -0.000000000000000000, 0.000000000000000000 ) ) ;
#23069 = CARTESIAN_POINT ( 'NONE',  ( -4.999999999999999112, 0.4881033300985041512, -6.000000000000000000 ) ) ;
#23070 = CARTESIAN_POINT ( 'NONE',  ( -92.69370383062498320, -209.9999999999999716, 87.42031250086714067 ) ) ;
#23071 = PLANE ( 'NONE',  #4305 ) ;
#23072 = DIRECTION ( 'NONE',  ( -1.000000000000000000, 0.000000000000000000, 0.000000000000000000 ) ) ;
#23073 = DIRECTION ( 'NONE',  ( 0.000000000000000000, 0.000000000000000000, 1.000000000000000000 ) ) ;
#23074 = VECTOR ( 'NONE', #44052, 1000.000000000000000 ) ;
#23075 = CARTESIAN_POINT ( 'NONE',  ( 96.32499999999998863, 87.70503267997126784, 89.57666666666666799 ) ) ;
#23076 = ORIENTED_EDGE ( 'NONE', *, *, #7962, .F. ) ;
#23077 = ORIENTED_EDGE ( 'NONE', *, *, #16325, .T. ) ;
#23078 = AXIS2_PLACEMENT_3D ( 'NONE', #70786, #18550, #40759 ) ;
#23079 = CARTESIAN_POINT ( 'NONE',  ( -93.67500000000003979, 87.70503267997129626, 76.87666666666666515 ) ) ;
#23080 = CARTESIAN_POINT ( 'NONE',  ( 97.64999999999999147, -209.9999999999999716, 90.00000000000000000 ) ) ;
#23081 = CARTESIAN_POINT ( 'NONE',  ( 11.99999999999999822, 71.21200624218852226, -40.65526001592539984 ) ) ;
#23082 = PLANE ( 'NONE',  #72177 ) ;
#23083 = DIRECTION ( 'NONE',  ( 0.1850432970638667407, -0.9827303690289282967, 0.000000000000000000 ) ) ;
#23084 = EDGE_CURVE ( 'NONE', #21420, #53605, #42404, .T. ) ;
#23085 = DIRECTION ( 'NONE',  ( -1.000000000000000000, 0.000000000000000000, 0.000000000000000000 ) ) ;
#23086 = DIRECTION ( 'NONE',  ( -0.000000000000000000, -0.000000000000000000, 1.000000000000000000 ) ) ;
#23087 = VERTEX_POINT ( 'NONE', #19094 ) ;
#23088 = CARTESIAN_POINT ( 'NONE',  ( -97.30629616937501680, 90.00000000000004263, 76.94281250086713442 ) ) ;
#23089 = EDGE_CURVE ( 'NONE', #32106, #67992, #1488, .T. ) ;
#23090 = CARTESIAN_POINT ( 'NONE',  ( 10.00000000000000000, 46.21855187248629449, 62.20884554314036308 ) ) ;
#23091 = DIRECTION ( 'NONE',  ( -1.000000000000000000, 0.000000000000000000, 0.000000000000000000 ) ) ;
#23092 = EDGE_CURVE ( 'NONE', #61621, #58605, #11897, .T. ) ;
#23093 = DIRECTION ( 'NONE',  ( -1.000000000000000000, 0.000000000000000000, 0.000000000000000000 ) ) ;
#23094 = CARTESIAN_POINT ( 'NONE',  ( 0.000000000000000000, -54.21277698773715059, 55.38113227695762930 ) ) ;
#23095 = LINE ( 'NONE', #18178, #56817 ) ;
#23096 = CARTESIAN_POINT ( 'NONE',  ( -92.69370383062498320, -211.3315407142195852, 88.79614583420050167 ) ) ;
#23097 = ADVANCED_FACE ( 'NONE', ( #45712 ), #29861, .T. ) ;
#23098 = CARTESIAN_POINT ( 'NONE',  ( 97.30629616937498838, 91.33154071421968467, 78.10697916753383652 ) ) ;
#23099 = CARTESIAN_POINT ( 'NONE',  ( -97.30629616937495996, -209.9999999999999716, 79.00656250086716170 ) ) ;
#23100 = PLANE ( 'NONE',  #21817 ) ;
#23101 = ORIENTED_EDGE ( 'NONE', *, *, #16645, .F. ) ;
#23102 = EDGE_CURVE ( 'NONE', #57628, #28591, #29090, .T. ) ;
#23103 = CARTESIAN_POINT ( 'NONE',  ( 97.65000000000000568, 88.47002178664752137, 87.80395833506766223 ) ) ;
#23104 = AXIS2_PLACEMENT_3D ( 'NONE', #52181, #6698, #5983 ) ;
#23105 = CARTESIAN_POINT ( 'NONE',  ( -96.32499999999996021, -207.7050326799711968, 75.28916666666665947 ) ) ;
#23106 = CARTESIAN_POINT ( 'NONE',  ( -94.99999999999997158, -209.9999999999999716, 90.00000000000000000 ) ) ;
#23107 = VECTOR ( 'NONE', #47667, 1000.000000000000000 ) ;
#23108 = CARTESIAN_POINT ( 'NONE',  ( -95.00000000000002842, 87.33691857156074434, 75.35531250086715715 ) ) ;
#23109 = CARTESIAN_POINT ( 'NONE',  ( 95.00000000000000000, -207.3369185715606307, 81.86406250086714920 ) ) ;
#23110 = ORIENTED_EDGE ( 'NONE', *, *, #54305, .T. ) ;
#23111 = VECTOR ( 'NONE', #21574, 1000.000000000000000 ) ;
#23112 = PLANE ( 'NONE',  #12699 ) ;
#23113 = EDGE_CURVE ( 'NONE', #25431, #15633, #67533, .T. ) ;
#23114 = ORIENTED_EDGE ( 'NONE', *, *, #49334, .F. ) ;
#23115 = CIRCLE ( 'NONE', #33889, 77.49899999999999523 ) ;
#23116 =( BOUNDED_CURVE ( )  B_SPLINE_CURVE ( 2, ( #1169, #39876, #62820, #11284, #3000, #37563, #60496, #1900, #8616, #54466, #66136, #70630, #24785, #2270, #48823, #42090, #47716, #71740, #3365, #8230, #19145, #13505, #30780, #65029, #36431, #36800, #31902, #26256, #2644, #31162, #59376, #49194, #42456, #14614, #18768, #7864, #53725, #60134, #54839, #25894, #20243, #25166, #41705, #14237, #48092, #71006, #31527, #43214, #19509, #59747, #64644, #13861, #13129, #65394, #8976, #36067, #53359, #54112, #59011, #7504, #25523, #48457, #30414, #37191, #71369, #19876, #42824, #65753, #45054, #9337, #67981, #15347, #72848, #28118, #49932, #66502, #22115, #21347, #21735, #61977, #50300, #20631, #32638, #38291, #73235, #72121, #44692, #67607, #20991, #44306, #60858, #73605, #32263, #4852, #43945, #37927, #33373, #16100, #16475, #67238, #55211, #27365, #39412, #27753, #43585, #14983, #5217, #3730, #9719, #26632, #49562, #62357, #39038, #10458, #15734, #72491, #50678, #55583, #55955, #66861, #4102, #61238, #38670, #56334, #10840, #26997, #33761, #61600, #10086, #56718, #33007, #4471, #40898, #346, #63833, #17217, #1078, #57441, #23237, #704, #51418, #45433, #6674, #44889, #22874, #68362, #12307, #69453, #51797, #68734, #5587, #39787, #40152, #16857, #23598, #35245, #11206, #63105, #40516, #52160, #58176, #11935, #29221, #63460, #11563, #46165, #5958, #57080, #34498, #51053, #62738, #29580, #28866, #34133, #17584, #46527, #52525, #73978, #69097, #28482, #45809, #22493, #34882, #17953, #57815, #6321, #27232, #50164, #21606, #28353, #56196, #27985, #39283, #62215, #27624, #16343, #73843, #62598, #32874, #21224, #55825, #50547, #32512, #4342, #38908, #56583, #73099, #44556, #10702, #55457, #15227, #15967, #5085, #33631, #67477, #73473, #61844, #66741, #44175, #50921, #10328, #33246, #4718, #45304, #22358, #74221, #21982, #3973, #44927, #38538, #67851, #67101, #72720, #68222, #56948, #51290, #16723, #39659, #15607, #43821, #11079, #34001, #5457, #38157, #61099, #61475, #9597, #26870, #49800, #9956, #58792, #18193, #46038, #51669, #12547, #29825, #68966, #216, #35481, #52783, #40382, #12176, #18555, #6191, #53148, #69324, #35114, #6910, #17452, #34751, #1327, #35841, #24216, #23108, #47146, #41136, #17090, #63333, #11435, #23835, #70054, #34370, #41494, #64434, #28730, #57692, #46777 ),
 .UNSPECIFIED., .F., .F. ) 
 B_SPLINE_CURVE_WITH_KNOTS ( ( 3, 2, 2, 2, 2, 2, 2, 2, 2, 2, 2, 2, 2, 2, 2, 2, 2, 2, 2, 2, 2, 2, 2, 2, 2, 2, 2, 2, 2, 2, 2, 2, 2, 2, 2, 2, 2, 2, 2, 2, 2, 2, 2, 2, 2, 2, 2, 2, 2, 2, 2, 2, 2, 2, 2, 2, 2, 2, 2, 2, 2, 2, 2, 2, 2, 2, 2, 2, 2, 2, 2, 2, 2, 2, 2, 2, 2, 2, 2, 2, 2, 2, 2, 2, 2, 2, 2, 2, 2, 2, 2, 2, 2, 2, 2, 2, 2, 2, 2, 2, 2, 2, 2, 2, 2, 2, 2, 2, 2, 2, 2, 2, 2, 2, 2, 2, 2, 2, 2, 2, 2, 2, 2, 2, 2, 2, 2, 2, 2, 2, 2, 2, 2, 2, 2, 2, 2, 2, 2, 2, 2, 2, 2, 3 ),
 ( 0.000000000000000000, 0.007055764916269566256, 0.01411152983253913251, 0.02116729474880869877, 0.02822305966507826502, 0.03527882458134783822, 0.04233458949761739754, 0.04939035441388697073, 0.05644611933015653005, 0.06350188424642609630, 0.07055764916269567644, 0.07761341407896524269, 0.08466917899523479507, 0.09172494391150436133, 0.09878070882777394146, 0.1058364737440435077, 0.1128922386603130601, 0.1199480035765826264, 0.1270037684928521926, 0.1340595334091217727, 0.1411152983253913529, 0.1481710632416609053, 0.1552268281579304854, 0.1622825930742000100, 0.1693383579904695901, 0.1763941229067391703, 0.1834498878230087227, 0.1905056527392783028, 0.1975614176555478829, 0.2046171825718174353, 0.2116729474880870154, 0.2187287124043565678, 0.2257844773206261202, 0.2328402422368957003, 0.2398960071531652527, 0.2469517720694348328, 0.2540075369857043852, 0.2610633019019739653, 0.2681190668182435455, 0.2751748317345130701, 0.2822305966507827057, 0.2892863615670522304, 0.2963421264833218105, 0.3033978913995913906, 0.3104536563158609708, 0.3175094212321304954, 0.3245651861484000200, 0.3316209510646696557, 0.3386767159809391803, 0.3457324808972087604, 0.3527882458134783406, 0.3598440107297479207, 0.3668997756460174453, 0.3739555405622870810, 0.3810113054785566056, 0.3880670703948261302, 0.3951228353110957658, 0.4021786002273652905, 0.4092343651436348706, 0.4162901300599044507, 0.4233458949761740309, 0.4304016598924435555, 0.4374574248087131356, 0.4445131897249827158, 0.4515689546412522404, 0.4586247195575218205, 0.4656804844737914006, 0.4727362493900609808, 0.4797920143063305054, 0.4868477792226001410, 0.4939035441388696657, 0.5009593090551393013, 0.5080150739714087704, 0.5150708388876783506, 0.5221266038039479307, 0.5291823687202175108, 0.5362381336364870910, 0.5432938985527566711, 0.5503496634690261402, 0.5574054283852958314, 0.5644611933015654115, 0.5715169582178348806, 0.5785727231341044607, 0.5856284880503740409, 0.5926842529666436210, 0.5997400178829132011, 0.6067957827991827813, 0.6138515477154522504, 0.6209073126317219415, 0.6279630775479914107, 0.6350188424642609908, 0.6420746073805305709, 0.6491303722968000400, 0.6561861372130697312, 0.6632419021293393113, 0.6702976670456087804, 0.6773534319618783606, 0.6844091968781480517, 0.6914649617944175208, 0.6985207267106871010, 0.7055764916269566811, 0.7126322565432261502, 0.7196880214594958414, 0.7267437863757654215, 0.7337995512920348906, 0.7408553162083044707, 0.7479110811245741619, 0.7549668460408436310, 0.7620226109571132111, 0.7690783758733827913, 0.7761341407896522604, 0.7831899057059219516, 0.7902456706221915317, 0.7973014355384610008, 0.8043572004547305809, 0.8114129653710002721, 0.8184687302872697412, 0.8255244952035393213, 0.8325802601198089015, 0.8396360250360783706, 0.8466917899523480617, 0.8537475548686176419, 0.8608033197848871110, 0.8678590847011566911, 0.8749148496174262712, 0.8819706145336958514, 0.8890263794499654315, 0.8960821443662349006, 0.9031379092825044808, 0.9101936741987741719, 0.9172494391150436410, 0.9243052040313132212, 0.9313609689475828013, 0.9384167338638523814, 0.9454724987801219616, 0.9525282636963915417, 0.9595840286126610108, 0.9666397935289305909, 0.9736955584452002821, 0.9807513233614697512, 0.9878070882777393313, 0.9948628531940089115, 0.9999999123559573100, 1.000000000000000000 ),
 .UNSPECIFIED. ) 
 CURVE ( )  GEOMETRIC_REPRESENTATION_ITEM ( )  RATIONAL_B_SPLINE_CURVE ( ( 1.000000000000000000, 0.8660254037844387076, 1.000000000000000000, 0.8660254037844387076, 1.000000000000000000, 0.8660254037844387076, 1.000000000000000000, 0.8660254037844387076, 1.000000000000000000, 0.8660254037844387076, 1.000000000000000000, 0.8660254037844387076, 1.000000000000000000, 0.8660254037844387076, 1.000000000000000000, 0.8660254037844387076, 1.000000000000000000, 0.8660254037844387076, 1.000000000000000000, 0.8660254037844387076, 1.000000000000000000, 0.8660254037844387076, 1.000000000000000000, 0.8660254037844387076, 1.000000000000000000, 0.8660254037844387076, 1.000000000000000000, 0.8660254037844387076, 1.000000000000000000, 0.8660254037844387076, 1.000000000000000000, 0.8660254037844387076, 1.000000000000000000, 0.8660254037844387076, 1.000000000000000000, 0.8660254037844387076, 1.000000000000000000, 0.8660254037844387076, 1.000000000000000000, 0.8660254037844387076, 1.000000000000000000, 0.8660254037844387076, 1.000000000000000000, 0.8660254037844387076, 1.000000000000000000, 0.8660254037844387076, 1.000000000000000000, 0.8660254037844387076, 1.000000000000000000, 0.8660254037844387076, 1.000000000000000000, 0.8660254037844387076, 1.000000000000000000, 0.8660254037844387076, 1.000000000000000000, 0.8660254037844387076, 1.000000000000000000, 0.8660254037844387076, 1.000000000000000000, 0.8660254037844387076, 1.000000000000000000, 0.8660254037844387076, 1.000000000000000000, 0.8660254037844387076, 1.000000000000000000, 0.8660254037844387076, 1.000000000000000000, 0.8660254037844387076, 1.000000000000000000, 0.8660254037844387076, 1.000000000000000000, 0.8660254037844387076, 1.000000000000000000, 0.8660254037844387076, 1.000000000000000000, 0.8660254037844387076, 1.000000000000000000, 0.8660254037844387076, 1.000000000000000000, 0.8660254037844387076, 1.000000000000000000, 0.8660254037844387076, 1.000000000000000000, 0.8660254037844387076, 1.000000000000000000, 0.8660254037844387076, 1.000000000000000000, 0.8660254037844387076, 1.000000000000000000, 0.8660254037844387076, 1.000000000000000000, 0.8660254037844387076, 1.000000000000000000, 0.8660254037844387076, 1.000000000000000000, 0.8660254037844387076, 1.000000000000000000, 0.8660254037844387076, 1.000000000000000000, 0.8660254037844387076, 1.000000000000000000, 0.8660254037844387076, 1.000000000000000000, 0.8660254037844387076, 1.000000000000000000, 0.8660254037844387076, 1.000000000000000000, 0.8660254037844387076, 1.000000000000000000, 0.8660254037844387076, 1.000000000000000000, 0.8660254037844387076, 1.000000000000000000, 0.8660254037844387076, 1.000000000000000000, 0.8660254037844387076, 1.000000000000000000, 0.8660254037844387076, 1.000000000000000000, 0.8660254037844387076, 1.000000000000000000, 0.8660254037844387076, 1.000000000000000000, 0.8660254037844387076, 1.000000000000000000, 0.8660254037844387076, 1.000000000000000000, 0.8660254037844387076, 1.000000000000000000, 0.8660254037844387076, 1.000000000000000000, 0.8660254037844387076, 1.000000000000000000, 0.8660254037844387076, 1.000000000000000000, 0.8660254037844387076, 1.000000000000000000, 0.8660254037844387076, 1.000000000000000000, 0.8660254037844387076, 1.000000000000000000, 0.8660254037844387076, 1.000000000000000000, 0.8660254037844387076, 1.000000000000000000, 0.8660254037844387076, 1.000000000000000000, 0.8660254037844387076, 1.000000000000000000, 0.8660254037844387076, 1.000000000000000000, 0.8660254037844387076, 1.000000000000000000, 0.8660254037844387076, 1.000000000000000000, 0.8660254037844387076, 1.000000000000000000, 0.8660254037844387076, 1.000000000000000000, 0.8660254037844387076, 1.000000000000000000, 0.8660254037844387076, 1.000000000000000000, 0.8660254037844387076, 1.000000000000000000, 0.8660254037844387076, 1.000000000000000000, 0.8660254037844387076, 1.000000000000000000, 0.8660254037844387076, 1.000000000000000000, 0.8660254037844387076, 1.000000000000000000, 0.8660254037844387076, 1.000000000000000000, 0.8660254037844387076, 1.000000000000000000, 0.8660254037844387076, 1.000000000000000000, 0.8660254037844387076, 1.000000000000000000, 0.8660254037844387076, 1.000000000000000000, 0.8660254037844387076, 1.000000000000000000, 0.8660254037844387076, 1.000000000000000000, 0.8660254037844387076, 1.000000000000000000, 0.8660254037844387076, 1.000000000000000000, 0.8660254037844387076, 1.000000000000000000, 0.8660254037844387076, 1.000000000000000000, 0.8660254037844387076, 1.000000000000000000, 0.8660254037844387076, 1.000000000000000000, 0.8660254037844387076, 1.000000000000000000, 0.8660254037844387076, 1.000000000000000000, 0.8660254037844387076, 1.000000000000000000, 0.8660254037844387076, 1.000000000000000000, 0.8660254037844387076, 1.000000000000000000, 0.8660254037844387076, 1.000000000000000000, 0.8660254037844387076, 1.000000000000000000, 0.8660254037844387076, 1.000000000000000000, 0.8660254037844387076, 1.000000000000000000, 0.8660254037844387076, 1.000000000000000000, 0.8660254037844387076, 1.000000000000000000, 0.8660254037844387076, 1.000000000000000000, 0.8660254037844387076, 1.000000000000000000, 0.8660254037844387076, 1.000000000000000000, 0.8660254037844387076, 1.000000000000000000, 0.8660254037844387076, 1.000000000000000000, 0.8660254037844387076, 1.000000000000000000, 0.8660254037844387076, 1.000000000000000000, 0.8660254037844387076, 1.000000000000000000, 0.8660254037844387076, 1.000000000000000000, 0.8660254037844387076, 1.000000000000000000, 0.8660254037844387076, 1.000000000000000000, 0.8660254037844387076, 1.000000000000000000, 0.8660254037844387076, 1.000000000000000000, 0.8660254037844387076, 1.000000000000000000, 0.8660254037844387076, 1.000000000000000000, 0.8660254037844387076, 1.000000000000000000, 0.8660254037844387076, 1.000000000000000000, 0.8660254037844387076, 1.000000000000000000, 0.8660254037844387076, 1.000000000000000000, 0.8660254037844387076, 1.000000000000000000, 0.8660254037844387076, 1.000000000000000000, 0.8660254037844387076, 1.000000000000000000, 0.8660254037844387076, 1.000000000000000000, 0.8660254037844387076, 1.000000000000000000, 0.8660254037844387076, 1.000000000000000000, 0.8660254037844387076, 1.000000000000000000, 0.8660254037844387076, 1.000000000000000000, 0.8660254037844387076, 1.000000000000000000, 0.8660254037844387076, 1.000000000000000000, 0.8660254037844387076, 1.000000000000000000, 0.8660254037844387076, 1.000000000000000000, 0.9024577157650887083, 0.9469497795711399046, 0.9469497795711399046, 0.9469497795711399046 ) ) 
 REPRESENTATION_ITEM ( '' )  );
#23117 = DIRECTION ( 'NONE',  ( 1.000000000000000000, 0.000000000000000000, -0.000000000000000000 ) ) ;
#23118 = ADVANCED_FACE ( 'NONE', ( #69354 ), #18586, .T. ) ;
#23119 = ORIENTED_EDGE ( 'NONE', *, *, #35573, .F. ) ;
#23120 = AXIS2_PLACEMENT_3D ( 'NONE', #27346, #16080, #39767 ) ;
#23121 = DIRECTION ( 'NONE',  ( -0.000000000000000000, 0.8090169943749426773, 0.5877852522924797984 ) ) ;
#23122 = ADVANCED_FACE ( 'NONE', ( #29125 ), #64100, .T. ) ;
#23123 = AXIS2_PLACEMENT_3D ( 'NONE', #1933, #25556, #29702 ) ;
#23124 = VERTEX_POINT ( 'NONE', #58825 ) ;
#23125 = VERTEX_POINT ( 'NONE', #248 ) ;
#23126 = EDGE_LOOP ( 'NONE', ( #6040, #27084, #37480, #44401 ) ) ;
#23127 = CARTESIAN_POINT ( 'NONE',  ( 10.00000000000000000, -70.52718814184240159, -26.02418014898383802 ) ) ;
#23128 = ADVANCED_FACE ( 'NONE', ( #46429 ), #41527, .T. ) ;
#23129 = ORIENTED_EDGE ( 'NONE', *, *, #53726, .F. ) ;
#23130 = ORIENTED_EDGE ( 'NONE', *, *, #9865, .T. ) ;
#23131 = CARTESIAN_POINT ( 'NONE',  ( 97.30629616937498838, 88.66845928578037217, 83.71614583420050337 ) ) ;
#23132 = DIRECTION ( 'NONE',  ( 2.603472992746261562E-14, 2.546204323184492723E-14, -1.000000000000000000 ) ) ;
#23133 = ORIENTED_EDGE ( 'NONE', *, *, #41345, .T. ) ;
#23134 = EDGE_CURVE ( 'NONE', #68521, #37253, #12581, .T. ) ;
#23135 = VERTEX_POINT ( 'NONE', #24248 ) ;
#23136 = VERTEX_POINT ( 'NONE', #47172 ) ;
#23137 = EDGE_LOOP ( 'NONE', ( #4665, #46863, #56132, #44486 ) ) ;
#23138 = PLANE ( 'NONE',  #9450 ) ;
#23139 = DIRECTION ( 'NONE',  ( 0.000000000000000000, 0.000000000000000000, 1.000000000000000000 ) ) ;
#23140 = CARTESIAN_POINT ( 'NONE',  ( 92.34999999999995168, 91.52997821335250705, 84.23208333333334963 ) ) ;
#23141 = DIRECTION ( 'NONE',  ( 0.000000000000000000, -1.000000000000000000, -1.040834085586084257E-14 ) ) ;
#23142 = DIRECTION ( 'NONE',  ( 0.000000000000000000, 0.4539904997395479702, -0.8910065241883673437 ) ) ;
#23143 = CARTESIAN_POINT ( 'NONE',  ( 10.00000000000000000, 0.000000000000000000, 0.000000000000000000 ) ) ;
#23144 = DIRECTION ( 'NONE',  ( 0.000000000000000000, 0.9510565162951503115, 0.3090169943749573878 ) ) ;
#23145 = DIRECTION ( 'NONE',  ( 1.000000000000000000, 0.000000000000000000, 0.000000000000000000 ) ) ;
#23146 = EDGE_LOOP ( 'NONE', ( #59673, #5840, #56798, #67205 ) ) ;
#23147 = CARTESIAN_POINT ( 'NONE',  ( -92.34999999999999432, -209.9999999999999716, 81.50687500173430067 ) ) ;
#23148 = ORIENTED_EDGE ( 'NONE', *, *, #26203, .T. ) ;
#23149 = CARTESIAN_POINT ( 'NONE',  ( 0.000000000000000000, -73.44644590900077219, 24.73286445877675632 ) ) ;
#23150 = VERTEX_POINT ( 'NONE', #70083 ) ;
#23152 = CARTESIAN_POINT ( 'NONE',  ( -95.00000000000002842, 86.94004357329504273, 79.44312500173428759 ) ) ;
#23151 = CARTESIAN_POINT ( 'NONE',  ( 97.64999999999997726, 88.47002178664753558, 77.64395833506762301 ) ) ;
#23153 = ORIENTED_EDGE ( 'NONE', *, *, #40250, .F. ) ;
#23154 = CARTESIAN_POINT ( 'NONE',  ( 97.30629616937498838, 91.33154071421968467, 80.01197916753380923 ) ) ;
#23155 = DIRECTION ( 'NONE',  ( 0.000000000000000000, 0.1564344650402312298, -0.9876883405951375483 ) ) ;
#23156 = CARTESIAN_POINT ( 'NONE',  ( -0.8815729230226008184, -93.47222532549339746, 5.500000000000000000 ) ) ;
#23157 = LINE ( 'NONE', #18242, #66260 ) ;
#23158 = CARTESIAN_POINT ( 'NONE',  ( 92.35000000006144205, 90.00001182123735077, 81.82400613091868991 ) ) ;
#23159 = STYLED_ITEM ( 'NONE', ( #17116 ), #74006 ) ;
#23160 = ORIENTED_EDGE ( 'NONE', *, *, #73381, .T. ) ;
#23161 = CARTESIAN_POINT ( 'NONE',  ( -97.64999999999994884, 91.52997821335257811, 80.42208333333330472 ) ) ;
#23162 = DIRECTION ( 'NONE',  ( 0.000000000000000000, 0.000000000000000000, 1.000000000000000000 ) ) ;
#23163 = CARTESIAN_POINT ( 'NONE',  ( 10.00000000000000000, 59.03342792756328095, -46.54456581323744757 ) ) ;
#23164 = ORIENTED_EDGE ( 'NONE', *, *, #46282, .F. ) ;
#23165 = AXIS2_PLACEMENT_3D ( 'NONE', #29101, #5091, #68608 ) ;
#23166 = ORIENTED_EDGE ( 'NONE', *, *, #330, .T. ) ;
#23167 = DIRECTION ( 'NONE',  ( -1.000000000000000000, 0.000000000000000000, 0.000000000000000000 ) ) ;
#23168 = CARTESIAN_POINT ( 'NONE',  ( 0.000000000000000000, -29.01471420065616513, 76.69515212746007649 ) ) ;
#23169 = DIRECTION ( 'NONE',  ( -1.000000000000000000, 0.000000000000000000, 0.000000000000000000 ) ) ;
#23170 = CARTESIAN_POINT ( 'NONE',  ( -92.69370383062498320, -209.9999999999999716, 79.95906250086714806 ) ) ;
#23171 = ORIENTED_EDGE ( 'NONE', *, *, #68867, .T. ) ;
#23172 = EDGE_CURVE ( 'NONE', #65045, #35341, #17118, .T. ) ;
#23173 = CARTESIAN_POINT ( 'NONE',  ( -10.00000000000000000, 0.000000000000000000, 0.000000000000000000 ) ) ;
#23174 = CIRCLE ( 'NONE', #35124, 32.00000000000000711 ) ;
#23175 = CIRCLE ( 'NONE', #399, 16.00000000000000000 ) ;
#23176 = PLANE ( 'NONE',  #66647 ) ;
#23177 = EDGE_CURVE ( 'NONE', #45415, #27271, #5851, .T. ) ;
#23178 = FACE_OUTER_BOUND ( 'NONE', #12772, .T. ) ;
#23179 = FACE_OUTER_BOUND ( 'NONE', #55924, .T. ) ;
#23180 = DIRECTION ( 'NONE',  ( 0.000000000000000000, -0.9510565162951503115, 0.3090169943749573878 ) ) ;
#23181 = LINE ( 'NONE', #11874, #6099 ) ;
#23182 = LINE ( 'NONE', #73180, #28932 ) ;
#23183 = CARTESIAN_POINT ( 'NONE',  ( -21.67772167707813935, -110.8034581014852762, -5.500000000000000000 ) ) ;
#23184 = EDGE_CURVE ( 'NONE', #71821, #24035, #55552, .T. ) ;
#23185 = DIRECTION ( 'NONE',  ( 0.000000000000000000, -0.4539904997395542430, 0.8910065241883641241 ) ) ;
#23186 = DIRECTION ( 'NONE',  ( 0.000000000000000000, 0.000000000000000000, 1.000000000000000000 ) ) ;
#23187 = CARTESIAN_POINT ( 'NONE',  ( 97.30629616937498838, 88.66845928578035796, 88.16114583420048234 ) ) ;
#23188 = CARTESIAN_POINT ( 'NONE',  ( 10.00000000000000000, 59.46389618801964616, 49.70050353004912580 ) ) ;
#23189 = DIRECTION ( 'NONE',  ( 1.000000000000000000, 0.000000000000000000, 0.000000000000000000 ) ) ;
#23190 = ORIENTED_EDGE ( 'NONE', *, *, #37965, .F. ) ;
#23191 = CARTESIAN_POINT ( 'NONE',  ( -92.35000000000003695, 90.00000000000004263, 78.25249999999999773 ) ) ;
#23192 = CARTESIAN_POINT ( 'NONE',  ( -92.69370383062505425, 91.33154071421968467, 80.48822916753380241 ) ) ;
#23193 = EDGE_CURVE ( 'NONE', #46802, #50648, #62787, .T. ) ;
#23194 = CARTESIAN_POINT ( 'NONE',  ( 0.000000000000000000, 0.000000000000000000, 0.000000000000000000 ) ) ;
#23195 = AXIS2_PLACEMENT_3D ( 'NONE', #60809, #43895, #50247 ) ;
#23196 = VERTEX_POINT ( 'NONE', #68996 ) ;
#23197 = DIRECTION ( 'NONE',  ( 0.000000000000000000, 0.000000000000000000, 1.000000000000000000 ) ) ;
#23198 = FACE_OUTER_BOUND ( 'NONE', #24666, .T. ) ;
#23199 = DIRECTION ( 'NONE',  ( -1.000000000000000000, 7.571541139944061634E-15, 2.603472992745718826E-14 ) ) ;
#23200 = AXIS2_PLACEMENT_3D ( 'NONE', #40797, #63732, #17483 ) ;
#23201 = CARTESIAN_POINT ( 'NONE',  ( 96.32499999999998863, -212.2949673200287179, 85.84604166840097150 ) ) ;
#23202 = EDGE_CURVE ( 'NONE', #31895, #24576, #72350, .T. ) ;
#23203 = EDGE_CURVE ( 'NONE', #38625, #4854, #12208, .T. ) ;
#23204 = CARTESIAN_POINT ( 'NONE',  ( 92.69370383062501162, -208.6684592857803011, 75.77864583420048916 ) ) ;
#23205 = LINE ( 'NONE', #46135, #54644 ) ;
#23206 = VECTOR ( 'NONE', #25142, 1000.000000000000000 ) ;
#23207 = ORIENTED_EDGE ( 'NONE', *, *, #58810, .T. ) ;
#23208 = ORIENTED_EDGE ( 'NONE', *, *, #46269, .F. ) ;
#23209 = CARTESIAN_POINT ( 'NONE',  ( 95.00000000000000000, -207.3369185715606307, 80.75281250086716511 ) ) ;
#23210 = DIRECTION ( 'NONE',  ( -1.000000000000000000, -0.000000000000000000, -0.000000000000000000 ) ) ;
#23211 = EDGE_CURVE ( 'NONE', #40041, #19435, #63361, .T. ) ;
#23212 = DIRECTION ( 'NONE',  ( -1.000000000000000000, 0.000000000000000000, 0.000000000000000000 ) ) ;
#23213 = VECTOR ( 'NONE', #26887, 1000.000000000000000 ) ;
#23214 = CARTESIAN_POINT ( 'NONE',  ( -97.64999999953586496, -210.0000309672219601, 77.38038495123339544 ) ) ;
#23215 = CARTESIAN_POINT ( 'NONE',  ( 92.34999999999999432, 89.99996406046703612, 83.72937624475873974 ) ) ;
#23216 = AXIS2_PLACEMENT_3D ( 'NONE', #59895, #48601, #31666 ) ;
#23217 = CARTESIAN_POINT ( 'NONE',  ( 11.99999999999999822, 65.64334221924909230, 41.19522573413756561 ) ) ;
#23218 = CARTESIAN_POINT ( 'NONE',  ( 97.64999999999997726, -208.4700217866474645, 87.19541666666667368 ) ) ;
#23219 = ORIENTED_EDGE ( 'NONE', *, *, #24676, .F. ) ;
#23220 = AXIS2_PLACEMENT_3D ( 'NONE', #5488, #45713, #57341 ) ;
#23221 = ORIENTED_EDGE ( 'NONE', *, *, #3324, .T. ) ;
#23222 = VERTEX_POINT ( 'NONE', #57719 ) ;
#23223 = CIRCLE ( 'NONE', #27982, 31.99999999999999289 ) ;
#23224 = VERTEX_POINT ( 'NONE', #6224 ) ;
#23225 =( NAMED_UNIT ( * ) SI_UNIT ( $, .STERADIAN. ) SOLID_ANGLE_UNIT ( ) );
#23226 = VECTOR ( 'NONE', #29531, 1000.000000000000000 ) ;
#23227 = CARTESIAN_POINT ( 'NONE',  ( -92.69370383062504004, 90.00000000000004263, 86.30906250086715659 ) ) ;
#23228 = CARTESIAN_POINT ( 'NONE',  ( 4.592054218142288313, 3.122278952918447814, -5.689399939901071512 ) ) ;
#23229 = CARTESIAN_POINT ( 'NONE',  ( 96.32499999999998863, -207.7050326799711968, 77.80270833506763495 ) ) ;
#23230 = CARTESIAN_POINT ( 'NONE',  ( 92.34999999999999432, 91.52997821335252127, 79.78708333333332803 ) ) ;
#23231 = ORIENTED_EDGE ( 'NONE', *, *, #37192, .F. ) ;
#23232 = DIRECTION ( 'NONE',  ( 1.000000000000000000, 0.000000000000000000, 0.000000000000000000 ) ) ;
#23233 = VERTEX_POINT ( 'NONE', #35145 ) ;
#23234 = DIRECTION ( 'NONE',  ( -0.000000000000000000, -0.9510565162951506446, -0.3090169943749562220 ) ) ;
#23235 = ORIENTED_EDGE ( 'NONE', *, *, #45450, .T. ) ;
#23236 = CARTESIAN_POINT ( 'NONE',  ( 93.67500000000001137, -212.2949673200287179, 88.28020833506764120 ) ) ;
#23237 = CARTESIAN_POINT ( 'NONE',  ( -92.69370383062504004, 90.00000000000004263, 82.49906250086715431 ) ) ;
#23238 = CARTESIAN_POINT ( 'NONE',  ( 92.69370383062498320, 88.66845928578037217, 89.21947916753381946 ) ) ;
#23239 = EDGE_LOOP ( 'NONE', ( #3798, #33751, #13103, #20473 ) ) ;
#23240 = FACE_OUTER_BOUND ( 'NONE', #39583, .T. ) ;
#23241 = DIRECTION ( 'NONE',  ( 0.000000000000000000, 0.000000000000000000, 1.000000000000000000 ) ) ;
#23242 = DIRECTION ( 'NONE',  ( 1.000000000000000000, 0.000000000000000000, 0.000000000000000000 ) ) ;
#23243 = LINE ( 'NONE', #712, #55128 ) ;
#23244 = ORIENTED_EDGE ( 'NONE', *, *, #2782, .T. ) ;
#23245 = CARTESIAN_POINT ( 'NONE',  ( -5.000000000000000000, 0.000000000000000000, -6.000000000000000000 ) ) ;
#23246 = CARTESIAN_POINT ( 'NONE',  ( -94.99999999999997158, -212.6630814284392557, 77.73656250086713726 ) ) ;
#23247 = ORIENTED_EDGE ( 'NONE', *, *, #46280, .T. ) ;
#23248 = EDGE_LOOP ( 'NONE', ( #44367, #47919, #20320, #3890 ) ) ;
#23249 = PLANE ( 'NONE',  #20532 ) ;
#23250 = ORIENTED_EDGE ( 'NONE', *, *, #14136, .F. ) ;
#23251 = PLANE ( 'NONE',  #8356 ) ;
#23252 = DIRECTION ( 'NONE',  ( 0.000000000000000000, 0.000000000000000000, 1.000000000000000000 ) ) ;
#23253 = VERTEX_POINT ( 'NONE', #58082 ) ;
#23254 = CARTESIAN_POINT ( 'NONE',  ( -92.69370383062498320, -208.6684592857803011, 77.31322916753380525 ) ) ;
#23255 = EDGE_LOOP ( 'NONE', ( #51693, #29095, #73116, #13034 ) ) ;
#23256 = CARTESIAN_POINT ( 'NONE',  ( 5.999999999999999112, 77.16300072079660310, 27.74655509720697211 ) ) ;
#23257 = CARTESIAN_POINT ( 'NONE',  ( 11.99999999999999822, 0.000000000000000000, 0.000000000000000000 ) ) ;
#23258 = CARTESIAN_POINT ( 'NONE',  ( 92.34999999999999432, -208.4700217866474645, 81.69208333333332916 ) ) ;
#23259 = ORIENTED_EDGE ( 'NONE', *, *, #15615, .F. ) ;
#23260 = DIRECTION ( 'NONE',  ( 0.000000000000000000, 0.000000000000000000, 1.000000000000000000 ) ) ;
#23261 = ADVANCED_FACE ( 'NONE', ( #6584 ), #42284, .T. ) ;
#23262 = CARTESIAN_POINT ( 'NONE',  ( 10.00000000000000000, 0.000000000000000000, 0.000000000000000000 ) ) ;
#23263 = AXIS2_PLACEMENT_3D ( 'NONE', #41981, #13759, #36696 ) ;
#23264 = EDGE_CURVE ( 'NONE', #26052, #68973, #1564, .T. ) ;
#23265 = CARTESIAN_POINT ( 'NONE',  ( 97.64999999999999147, -210.0000000198592716, 85.95187500101400246 ) ) ;
#23266 = CARTESIAN_POINT ( 'NONE',  ( 97.30629616937498838, 91.33154071421968467, 83.66322916753381378 ) ) ;
#23267 = CARTESIAN_POINT ( 'NONE',  ( 10.00000000000000000, 59.03342792756328095, -46.54456581323744757 ) ) ;
#23268 = CARTESIAN_POINT ( 'NONE',  ( -97.65000000000007674, 88.47002178664759242, 88.14791666666667425 ) ) ;
#23269 = FACE_OUTER_BOUND ( 'NONE', #62047, .T. ) ;
#23270 = CARTESIAN_POINT ( 'NONE',  ( 11.99999999999999822, 36.73666225445894185, 65.58780272294090707 ) ) ;
#23272 = EDGE_CURVE ( 'NONE', #44625, #45506, #57973, .T. ) ;
#23271 = DIRECTION ( 'NONE',  ( -1.000000000000000000, 0.000000000000000000, 0.000000000000000000 ) ) ;
#23273 = FACE_OUTER_BOUND ( 'NONE', #51675, .T. ) ;
#23274 = CARTESIAN_POINT ( 'NONE',  ( 10.00000000000000000, 0.000000000000000000, 0.000000000000000000 ) ) ;
#23275 = AXIS2_PLACEMENT_3D ( 'NONE', #7212, #24498, #30129 ) ;
#23276 = EDGE_CURVE ( 'NONE', #48441, #10439, #1716, .T. ) ;
#23277 = CIRCLE ( 'NONE', #58035, 37.49900000000000233 ) ;
#23278 = LINE ( 'NONE', #22536, #69694 ) ;
#23279 = CARTESIAN_POINT ( 'NONE',  ( 0.000000000000000000, -73.73191006444582740, 14.66109333815435889 ) ) ;
#23280 = AXIS2_PLACEMENT_3D ( 'NONE', #11153, #74301, #38612 ) ;
#23281 = DIRECTION ( 'NONE',  ( 0.000000000000000000, 0.000000000000000000, 1.000000000000000000 ) ) ;
#23282 = LINE ( 'NONE', #63880, #13043 ) ;
#23283 = EDGE_CURVE ( 'NONE', #8457, #6569, #2821, .T. ) ;
#23284 = CARTESIAN_POINT ( 'NONE',  ( -26.50044424985255276, 0.001194404164626844313, -64.00000000000000000 ) ) ;
#23285 = EDGE_CURVE ( 'NONE', #47150, #64948, #15376, .T. ) ;
#23286 = CARTESIAN_POINT ( 'NONE',  ( -23.97194136764370498, -131.3950000906648938, 5.500000000000000000 ) ) ;
#23287 = CARTESIAN_POINT ( 'NONE',  ( 11.99999999999999822, 20.41045688087930898, -72.35160999960793049 ) ) ;
#23288 = CYLINDRICAL_SURFACE ( 'NONE', #21390, 31.99999999999999289 ) ;
#23289 = CIRCLE ( 'NONE', #68901, 77.49899999999999523 ) ;
#23290 = FACE_OUTER_BOUND ( 'NONE', #6557, .T. ) ;
#23291 = CARTESIAN_POINT ( 'NONE',  ( 0.000000000000000000, 15.48615015657581750, 39.04073710021349797 ) ) ;
#23292 = EDGE_CURVE ( 'NONE', #63726, #18161, #25552, .T. ) ;
#23293 = ADVANCED_FACE ( 'NONE', ( #48279 ), #19693, .F. ) ;
#23294 = CARTESIAN_POINT ( 'NONE',  ( 92.69370383062501162, -208.6684592857803011, 84.66864583420047552 ) ) ;
#23295 = ORIENTED_EDGE ( 'NONE', *, *, #67253, .F. ) ;
#23296 = ORIENTED_EDGE ( 'NONE', *, *, #69999, .F. ) ;
#23297 = CARTESIAN_POINT ( 'NONE',  ( -94.99999999999997158, -206.9400435732949575, 86.03125000000000000 ) ) ;
#23298 = VERTEX_POINT ( 'NONE', #65581 ) ;
#23299 = CIRCLE ( 'NONE', #20924, 23.50000000000489919 ) ;
#23300 = CARTESIAN_POINT ( 'NONE',  ( -97.64999999978461176, -209.9999789922612479, 79.91868729551984529 ) ) ;
#23301 = DIRECTION ( 'NONE',  ( -0.000000000000000000, -0.000000000000000000, 1.000000000000000000 ) ) ;
#23302 = ORIENTED_EDGE ( 'NONE', *, *, #51264, .F. ) ;
#23303 = CARTESIAN_POINT ( 'NONE',  ( 93.84685191531249870, -208.0026889286704943, 82.07572916753382231 ) ) ;
#23304 = VERTEX_POINT ( 'NONE', #14048 ) ;
#23305 = CARTESIAN_POINT ( 'NONE',  ( -97.65000000000003411, -211.5299782133523934, 88.14791666666667425 ) ) ;
#23306 = ORIENTED_EDGE ( 'NONE', *, *, #63152, .F. ) ;
#23307 = ORIENTED_EDGE ( 'NONE', *, *, #10335, .F. ) ;
#23308 = CARTESIAN_POINT ( 'NONE',  ( 10.00000000000000000, -2.663952781845854378, -41.91543099594820632 ) ) ;
#23309 = UNCERTAINTY_MEASURE_WITH_UNIT (LENGTH_MEASURE( 1.000000000000000082E-05 ), #52190, 'distance_accuracy_value', 'NONE');
#23310 = VECTOR ( 'NONE', #25972, 1000.000000000000000 ) ;
#23311 = CARTESIAN_POINT ( 'NONE',  ( -94.99999999999997158, -209.9999999999999716, 90.00000000000000000 ) ) ;
#23312 = ORIENTED_EDGE ( 'NONE', *, *, #26210, .T. ) ;
#23313 = CARTESIAN_POINT ( 'NONE',  ( -93.67500000000003979, 87.70503267997129626, 77.51166666666665606 ) ) ;
#23314 = CARTESIAN_POINT ( 'NONE',  ( 95.00000000000000000, -206.9400435732949575, 86.11062500173430578 ) ) ;
#23315 = ORIENTED_EDGE ( 'NONE', *, *, #72724, .F. ) ;
#23316 = DIRECTION ( 'NONE',  ( -1.000000000000000000, 0.000000000000000000, 0.000000000000000000 ) ) ;
#23317 = ORIENTED_EDGE ( 'NONE', *, *, #59013, .T. ) ;
#23318 =( BOUNDED_CURVE ( )  B_SPLINE_CURVE ( 2, ( #55774, #166, #51613, #32823, #61795, #39231, #11025, #73422, #45987 ),
 .UNSPECIFIED., .F., .F. ) 
 B_SPLINE_CURVE_WITH_KNOTS ( ( 3, 2, 2, 2, 3 ),
 ( 0.2751748541904413536, 0.2822306216352944985, 0.2892863871761765515, 0.2963421527170586600, 0.2963422021981248489 ),
 .UNSPECIFIED. ) 
 CURVE ( )  GEOMETRIC_REPRESENTATION_ITEM ( )  RATIONAL_B_SPLINE_CURVE ( ( 1.000000000000000000, 0.8660254037844387076, 1.000000000000000000, 0.8660254037844387076, 1.000000000000000000, 0.8660254037844387076, 1.000000000000000000, 0.9999990604554780393, 0.9999981209241337599 ) ) 
 REPRESENTATION_ITEM ( '' )  );
#23319 = CARTESIAN_POINT ( 'NONE',  ( 10.00000000000000000, -29.81001611431024756, 22.74946021919122785 ) ) ;
#23320 = AXIS2_PLACEMENT_3D ( 'NONE', #38534, #73839, #27228 ) ;
#23321 = ORIENTED_EDGE ( 'NONE', *, *, #2328, .F. ) ;
#23322 = EDGE_LOOP ( 'NONE', ( #54266, #55590, #35223, #45885 ) ) ;
#23323 = VERTEX_POINT ( 'NONE', #59193 ) ;
#23324 = CARTESIAN_POINT ( 'NONE',  ( -97.64998927314393029, -211.5299844065056334, 78.06729209680057124 ) ) ;
#23325 = VECTOR ( 'NONE', #38712, 1000.000000000000000 ) ;
#23326 = CARTESIAN_POINT ( 'NONE',  ( -5.000000000000000000, -0.5603747650654237189, -0.5678343202077608121 ) ) ;
#23327 = EDGE_LOOP ( 'NONE', ( #33852, #43681, #66865, #19753 ) ) ;
#23328 = ORIENTED_EDGE ( 'NONE', *, *, #50391, .F. ) ;
#23330 = EDGE_CURVE ( 'NONE', #52246, #27844, #41188, .T. ) ;
#23329 = ORIENTED_EDGE ( 'NONE', *, *, #30205, .F. ) ;
#23331 = CARTESIAN_POINT ( 'NONE',  ( 0.000000000000000000, 0.000000000000000000, 125.0000000000000000 ) ) ;
#23332 = CARTESIAN_POINT ( 'NONE',  ( 3.000000000000000000, 1.467624384280025174, -2.542000000000001592 ) ) ;
#23333 = EDGE_CURVE ( 'NONE', #15290, #49569, #66360, .T. ) ;
#23334 = CARTESIAN_POINT ( 'NONE',  ( -93.67500000000003979, 87.70503267997129626, 88.94166666666666288 ) ) ;
#23335 = ORIENTED_EDGE ( 'NONE', *, *, #71887, .T. ) ;
#23336 = CARTESIAN_POINT ( 'NONE',  ( 96.15314808468748708, 88.00268892867053694, 75.88447916753381151 ) ) ;
#23337 = VECTOR ( 'NONE', #64399, 1000.000000000000000 ) ;
#23338 = EDGE_CURVE ( 'NONE', #2660, #54637, #37383, .T. ) ;
#23339 = ORIENTED_EDGE ( 'NONE', *, *, #21793, .T. ) ;
#23340 =( BOUNDED_CURVE ( )  B_SPLINE_CURVE ( 2, ( #6428, #51904, #23344, #46271, #17694, #40631, #29328, #52272, #815 ),
 .UNSPECIFIED., .F., .F. ) 
 B_SPLINE_CURVE_WITH_KNOTS ( ( 3, 2, 2, 2, 3 ),
 ( 0.6561861948943049638, 0.6632419608461993521, 0.6702977263871157110, 0.6773534919280320699, 0.6773535682785479795 ),
 .UNSPECIFIED. ) 
 CURVE ( )  GEOMETRIC_REPRESENTATION_ITEM ( )  RATIONAL_B_SPLINE_CURVE ( ( 1.000000000000000000, 0.8660254037844387076, 1.000000000000000000, 0.8660254037844387076, 1.000000000000000000, 0.8660254037844387076, 1.000000000000000000, 0.9999985502594314069, 0.9999971005502381605 ) ) 
 REPRESENTATION_ITEM ( '' )  );
#23341 = CARTESIAN_POINT ( 'NONE',  ( -5.250000000000000888, -13.95926121303099343, -1.199999999999999956 ) ) ;
#23342 = CARTESIAN_POINT ( 'NONE',  ( -96.15314808468747287, -208.0026889286704943, 86.36197916753381776 ) ) ;
#23343 = VERTEX_POINT ( 'NONE', #43017 ) ;
#23344 = CARTESIAN_POINT ( 'NONE',  ( -93.67499999999998295, -212.2949673200287179, 79.49604166840096298 ) ) ;
#23345 = CARTESIAN_POINT ( 'NONE',  ( 12.50000000000000000, -132.5000000000000000, 2.500000000000000000 ) ) ;
#23346 = DIRECTION ( 'NONE',  ( -1.000000000000000000, 0.000000000000000000, 0.000000000000000000 ) ) ;
#23347 = CARTESIAN_POINT ( 'NONE',  ( -92.69370383062498320, -208.6684592857803295, 76.04322916753380923 ) ) ;
#23348 = VECTOR ( 'NONE', #54658, 1000.000000000000000 ) ;
#23349 = ADVANCED_FACE ( 'NONE', ( #20062 ), #24972, .F. ) ;
#23350 = CARTESIAN_POINT ( 'NONE',  ( -10.00000000000000000, 0.000000000000000000, 0.000000000000000000 ) ) ;
#23351 = DIRECTION ( 'NONE',  ( -1.000000000000000000, 0.000000000000000000, 0.000000000000000000 ) ) ;
#23352 = EDGE_CURVE ( 'NONE', #25525, #60600, #47145, .T. ) ;
#23353 = CARTESIAN_POINT ( 'NONE',  ( 11.99999999999999822, 0.000000000000000000, 0.000000000000000000 ) ) ;
#23354 = CARTESIAN_POINT ( 'NONE',  ( -92.35000000000003695, 90.00000000000004263, 90.00000000000000000 ) ) ;
#23355 = CARTESIAN_POINT ( 'NONE',  ( 10.00000000000000000, 77.16300072079698680, -27.74655509720590274 ) ) ;
#23356 = CARTESIAN_POINT ( 'NONE',  ( -97.30629616937501680, 90.00000000000004263, 76.94281250086713442 ) ) ;
#23357 = CYLINDRICAL_SURFACE ( 'NONE', #35852, 31.99999999999999289 ) ;
#23358 = PLANE ( 'NONE',  #5027 ) ;
#23359 = CIRCLE ( 'NONE', #65369, 37.49900000000000233 ) ;
#23360 = EDGE_CURVE ( 'NONE', #29293, #70940, #45310, .T. ) ;
#23361 = VERTEX_POINT ( 'NONE', #582 ) ;
#23362 = CARTESIAN_POINT ( 'NONE',  ( 10.00000000000000000, 0.000000000000000000, 0.000000000000000000 ) ) ;
#23363 = CARTESIAN_POINT ( 'NONE',  ( 11.99999999999999822, 0.000000000000000000, 0.000000000000000000 ) ) ;
#23364 = CARTESIAN_POINT ( 'NONE',  ( 0.000000000000000000, 0.000000000000000000, 0.000000000000000000 ) ) ;
#23365 = CIRCLE ( 'NONE', #2986, 16.00000000000000711 ) ;
#23366 = DIRECTION ( 'NONE',  ( -1.000000000000000000, 0.000000000000000000, 0.000000000000000000 ) ) ;
#23367 = CARTESIAN_POINT ( 'NONE',  ( 10.00000000000000000, -36.72794159290197769, -65.59268652807249111 ) ) ;
#23368 = CARTESIAN_POINT ( 'NONE',  ( -3.000000000000000000, 26.50000000000000000, -1.500000000000001332 ) ) ;
#23369 = CARTESIAN_POINT ( 'NONE',  ( -97.30629616937497417, -211.3315407142195852, 76.51947916753381662 ) ) ;
#23370 = ADVANCED_FACE ( 'NONE', ( #39289 ), #11085, .T. ) ;
#23371 = CARTESIAN_POINT ( 'NONE',  ( 11.99999999999999822, 35.91791733033570466, -68.67312586194960033 ) ) ;
#23372 = EDGE_CURVE ( 'NONE', #40539, #62152, #21988, .T. ) ;
#23373 = VECTOR ( 'NONE', #63821, 999.9999999999998863 ) ;
#23374 = VERTEX_POINT ( 'NONE', #22745 ) ;
#23375 = DIRECTION ( 'NONE',  ( -0.5687579148473765889, 0.8225049752423776450, 0.000000000000000000 ) ) ;
#23376 = VECTOR ( 'NONE', #1992, 1000.000000000000000 ) ;
#23377 = LINE ( 'NONE', #53419, #17832 ) ;
#23378 = CARTESIAN_POINT ( 'NONE',  ( 15.00000000000000000, -22.67460108101774452, 6.353146135318220367 ) ) ;
#23379 = CYLINDRICAL_SURFACE ( 'NONE', #17353, 31.99999999999999289 ) ;
#23380 = CIRCLE ( 'NONE', #59436, 12.49999999999999645 ) ;
#23381 = AXIS2_PLACEMENT_3D ( 'NONE', #14379, #54606, #72251 ) ;
#23382 = DIRECTION ( 'NONE',  ( 0.000000000000000000, 0.3090169943749412340, 0.9510565162951556406 ) ) ;
#23383 = EDGE_LOOP ( 'NONE', ( #62806, #3991, #53794, #22936 ) ) ;
#23384 = DIRECTION ( 'NONE',  ( -1.000000000000000000, 0.000000000000000000, -0.000000000000000000 ) ) ;
#23385 = CARTESIAN_POINT ( 'NONE',  ( 0.000000000000000000, 41.81611651403868990, -3.925862922255709542 ) ) ;
#23386 = ORIENTED_EDGE ( 'NONE', *, *, #32057, .T. ) ;
#23387 = CIRCLE ( 'NONE', #65357, 42.00000000000000000 ) ;
#23388 = CARTESIAN_POINT ( 'NONE',  ( 95.00000000000000000, -212.6630814284392557, 85.35656250086714181 ) ) ;
#23389 = DIRECTION ( 'NONE',  ( 0.000000000000000000, -0.8910065241883626808, -0.4539904997395570740 ) ) ;
#23390 = EDGE_LOOP ( 'NONE', ( #63896, #2335, #21065, #14173 ) ) ;
#23391 = AXIS2_PLACEMENT_3D ( 'NONE', #40157, #73610, #22121 ) ;
#23392 = DIRECTION ( 'NONE',  ( 0.000000000000000000, 1.000000000000000000, 0.000000000000000000 ) ) ;
#23393 = ORIENTED_EDGE ( 'NONE', *, *, #15553, .T. ) ;
#23394 = DIRECTION ( 'NONE',  ( 0.000000000000000000, -0.5877852522924624790, -0.8090169943749550008 ) ) ;
#23395 = VERTEX_POINT ( 'NONE', #50552 ) ;
#23396 = CARTESIAN_POINT ( 'NONE',  ( -97.30629616937501680, 90.00000000000004263, 82.18156250086715886 ) ) ;
#23397 = ORIENTED_EDGE ( 'NONE', *, *, #33273, .T. ) ;
#23398 = DIRECTION ( 'NONE',  ( 1.000000000000000000, 0.000000000000000000, 0.000000000000000000 ) ) ;
#23399 = ORIENTED_EDGE ( 'NONE', *, *, #47196, .T. ) ;
#23400 = VERTEX_POINT ( 'NONE', #46406 ) ;
#23401 = DIRECTION ( 'NONE',  ( -1.000000000000000000, 0.000000000000000000, 0.000000000000000000 ) ) ;
#23402 = EDGE_CURVE ( 'NONE', #44417, #30226, #62222, .T. ) ;
#23403 = ORIENTED_EDGE ( 'NONE', *, *, #47685, .T. ) ;
#23404 = VERTEX_POINT ( 'NONE', #62605 ) ;
#23405 = CARTESIAN_POINT ( 'NONE',  ( 97.65000000000000568, -211.5299782133524218, 80.81895833506763438 ) ) ;
#23406 = ORIENTED_EDGE ( 'NONE', *, *, #41832, .F. ) ;
#23407 = ORIENTED_EDGE ( 'NONE', *, *, #24015, .T. ) ;
#23408 = CARTESIAN_POINT ( 'NONE',  ( 92.69370383062498320, 88.66845928578037217, 86.52072916753381548 ) ) ;
#23409 = ORIENTED_EDGE ( 'NONE', *, *, #36584, .F. ) ;
#23410 = CARTESIAN_POINT ( 'NONE',  ( 97.30629616937498838, -211.3315407142195852, 82.92239583420045790 ) ) ;
#23411 = AXIS2_PLACEMENT_3D ( 'NONE', #5948, #47264, #52902 ) ;
#23412 = APPLICATION_PROTOCOL_DEFINITION ( 'draft international standard', 'automotive_design', 1998, #63796 ) ;
#23413 = CARTESIAN_POINT ( 'NONE',  ( -97.64999999947046661, -209.9999663481462164, 81.18829462297327382 ) ) ;
#23414 = CARTESIAN_POINT ( 'NONE',  ( -93.09170270117142820, -211.8387227684682159, 74.99954709728268654 ) ) ;
#23415 = CARTESIAN_POINT ( 'NONE',  ( 94.99999999999998579, 86.94004357329502852, 85.07875000000001364 ) ) ;
#23416 = DIRECTION ( 'NONE',  ( 0.000000000000000000, -0.4539904997395350361, -0.8910065241883738940 ) ) ;
#23417 = ADVANCED_FACE ( 'NONE', ( #34006 ), #46045, .F. ) ;
#23418 = CARTESIAN_POINT ( 'NONE',  ( -95.00000000000002842, 86.94004357329504273, 79.36374999999996760 ) ) ;
#23419 = CARTESIAN_POINT ( 'NONE',  ( -92.69370383062498320, -209.9999999999999716, 83.61031250086713840 ) ) ;
#23420 = EDGE_CURVE ( 'NONE', #29989, #68978, #6213, .T. ) ;
#23421 = CARTESIAN_POINT ( 'NONE',  ( -97.30629616937501680, 90.00000000000004263, 81.54656250086715374 ) ) ;
#23422 = ORIENTED_EDGE ( 'NONE', *, *, #48564, .T. ) ;
#23423 = CARTESIAN_POINT ( 'NONE',  ( 93.84685191531248449, 91.99731107132950569, 85.09197916753380753 ) ) ;
#23424 = ORIENTED_EDGE ( 'NONE', *, *, #51618, .F. ) ;
#23425 = CARTESIAN_POINT ( 'NONE',  ( 92.35000000002543175, -209.9999999999998863, -74.99999999999342037 ) ) ;
#23426 = AXIS2_PLACEMENT_3D ( 'NONE', #32689, #55636, #4152 ) ;
#23427 = DIRECTION ( 'NONE',  ( 0.3311129884571281101, 0.9435911131814402886, -0.000000000000000000 ) ) ;
#23428 = CIRCLE ( 'NONE', #48639, 77.49900000000000944 ) ;
#23429 = CARTESIAN_POINT ( 'NONE',  ( 0.000000000000000000, 0.000000000000000000, 0.000000000000000000 ) ) ;
#23430 = FACE_OUTER_BOUND ( 'NONE', #9440, .T. ) ;
#23431 = CARTESIAN_POINT ( 'NONE',  ( -93.84685191531248449, -208.0026889286704943, 87.52614583420047722 ) ) ;
#23432 = LINE ( 'NONE', #1288, #27063 ) ;
#23433 = ADVANCED_FACE ( 'NONE', ( #68228 ), #11800, .F. ) ;
#23434 = ADVANCED_FACE ( 'NONE', ( #63712 ), #49531, .F. ) ;
#23435 = CYLINDRICAL_SURFACE ( 'NONE', #56610, 16.00000000000000000 ) ;
#23436 = DIRECTION ( 'NONE',  ( 0.000000000000000000, 0.000000000000000000, 1.000000000000000000 ) ) ;
#23437 = CIRCLE ( 'NONE', #63063, 31.99999999999998934 ) ;
#23438 = CARTESIAN_POINT ( 'NONE',  ( 10.00000000000000000, -10.74501242461258244, -35.92658777277521409 ) ) ;
#23439 = ORIENTED_EDGE ( 'NONE', *, *, #20211, .F. ) ;
#23440 = ORIENTED_EDGE ( 'NONE', *, *, #4280, .F. ) ;
#23441 = AXIS2_PLACEMENT_3D ( 'NONE', #53669, #26195, #37869 ) ;
#23442 = CARTESIAN_POINT ( 'NONE',  ( -92.35000000000003695, 90.00000000000004263, 78.88750000000000284 ) ) ;
#23443 = CARTESIAN_POINT ( 'NONE',  ( 92.35000000000000853, -209.9999999999999716, 88.73000000000000398 ) ) ;
#23444 = CARTESIAN_POINT ( 'NONE',  ( 92.35000000000000853, -209.9999999999999716, 81.10999999999999943 ) ) ;
#23445 = FACE_OUTER_BOUND ( 'NONE', #6546, .T. ) ;
#23446 = DIRECTION ( 'NONE',  ( -1.000000000000000000, -0.000000000000000000, 0.000000000000000000 ) ) ;
#23447 = DIRECTION ( 'NONE',  ( -1.000000000000000000, -0.000000000000000000, -0.000000000000000000 ) ) ;
#23448 = EDGE_CURVE ( 'NONE', #29601, #31522, #45688, .T. ) ;
#23449 = ORIENTED_EDGE ( 'NONE', *, *, #46457, .T. ) ;
#23450 = CARTESIAN_POINT ( 'NONE',  ( -97.30629616937501680, 91.33154071421968467, 79.42989583420046529 ) ) ;
#23451 = DIRECTION ( 'NONE',  ( -1.000000000000000000, 0.000000000000000000, 0.000000000000000000 ) ) ;
#23452 = CARTESIAN_POINT ( 'NONE',  ( 10.00000000000000000, 63.18004540533092239, -44.88180994100307686 ) ) ;
#23453 = DIRECTION ( 'NONE',  ( 7.943659481576819828E-16, 1.065814103640131188E-14, 1.000000000000000000 ) ) ;
#23454 = CARTESIAN_POINT ( 'NONE',  ( 0.000000000000000000, -2.935248768560059673, 2.602085213965210642E-15 ) ) ;
#23455 = AXIS2_PLACEMENT_3D ( 'NONE', #40366, #51270, #35101 ) ;
#23456 = CARTESIAN_POINT ( 'NONE',  ( -97.30629616937495996, -209.9999999999999716, 86.62656250086715204 ) ) ;
#23457 = SHAPE_REPRESENTATION ( 'key', ( #43395 ), #59100 ) ;
#23458 = EDGE_CURVE ( 'NONE', #63855, #60337, #24325, .T. ) ;
#23459 = EDGE_CURVE ( 'NONE', #32352, #69078, #34377, .T. ) ;
#23460 = CARTESIAN_POINT ( 'NONE',  ( 94.99999999999998579, 87.33691857156068750, 76.62531250086715318 ) ) ;
#23461 = CARTESIAN_POINT ( 'NONE',  ( -92.69370383062498320, -209.9999999999999716, 78.68906250086715204 ) ) ;
#23462 = DIRECTION ( 'NONE',  ( 0.000000000000000000, 0.000000000000000000, 1.000000000000000000 ) ) ;
#23463 = ORIENTED_EDGE ( 'NONE', *, *, #14846, .T. ) ;
#23464 = LINE ( 'NONE', #6907, #47314 ) ;
#23465 = DIRECTION ( 'NONE',  ( 0.000000000000000000, 0.000000000000000000, 1.000000000000000000 ) ) ;
#23466 = DIRECTION ( 'NONE',  ( 0.000000000000000000, -0.8910065241883721177, 0.4539904997395382003 ) ) ;
#23467 = AXIS2_PLACEMENT_3D ( 'NONE', #11470, #69728, #52815 ) ;
#23468 = CARTESIAN_POINT ( 'NONE',  ( 0.000000000000000000, -81.90746397400386059, -3.894527615418773347 ) ) ;
#23469 = CARTESIAN_POINT ( 'NONE',  ( 95.00000000000000000, -207.3369185715606307, 78.05406250086714692 ) ) ;
#23470 = VERTEX_POINT ( 'NONE', #5828 ) ;
#23471 = CARTESIAN_POINT ( 'NONE',  ( -92.34999999999998010, 91.52997821335249284, 75.13041666666666174 ) ) ;
#23472 = VERTEX_POINT ( 'NONE', #6196 ) ;
#23473 = AXIS2_PLACEMENT_3D ( 'NONE', #53994, #38824, #61764 ) ;
#23474 = DIRECTION ( 'NONE',  ( -1.000000000000000000, -0.000000000000000000, 0.000000000000000000 ) ) ;
#23475 = AXIS2_PLACEMENT_3D ( 'NONE', #57736, #13334, #23513 ) ;
#23476 = ORIENTED_EDGE ( 'NONE', *, *, #1060, .T. ) ;
#23477 = DIRECTION ( 'NONE',  ( -1.000000000000000000, 7.571543891232750625E-15, 2.563413034563919882E-14 ) ) ;
#23478 = VECTOR ( 'NONE', #72086, 1000.000000000000000 ) ;
#23479 = ORIENTED_EDGE ( 'NONE', *, *, #46671, .F. ) ;
#23480 = VERTEX_POINT ( 'NONE', #22365 ) ;
#23481 = ORIENTED_EDGE ( 'NONE', *, *, #50167, .F. ) ;
#23482 = DIRECTION ( 'NONE',  ( 1.000000000000000000, -0.000000000000000000, -0.000000000000000000 ) ) ;
#23483 = ORIENTED_EDGE ( 'NONE', *, *, #34559, .T. ) ;
#23484 = AXIS2_PLACEMENT_3D ( 'NONE', #5786, #17418, #40351 ) ;
#23485 = ORIENTED_EDGE ( 'NONE', *, *, #68003, .T. ) ;
#23486 = CARTESIAN_POINT ( 'NONE',  ( 92.69370383062498320, 91.33154071421968467, 83.39864583420050792 ) ) ;
#23487 = CARTESIAN_POINT ( 'NONE',  ( 95.00000000000000000, -213.0599564267049857, 75.55375000000000796 ) ) ;
#23488 = ORIENTED_EDGE ( 'NONE', *, *, #60170, .T. ) ;
#23489 = VERTEX_POINT ( 'NONE', #28735 ) ;
#23490 = ADVANCED_FACE ( 'NONE', ( #51674 ), #222, .F. ) ;
#23491 = ORIENTED_EDGE ( 'NONE', *, *, #839, .F. ) ;
#23492 = VERTEX_POINT ( 'NONE', #19304 ) ;
#23493 = DIRECTION ( 'NONE',  ( -2.628368902995175337E-16, -1.000000000000000000, 0.000000000000000000 ) ) ;
#23494 = DIRECTION ( 'NONE',  ( -0.9974137572422395737, -0.07187347816767440667, 0.000000000000000000 ) ) ;
#23495 = CARTESIAN_POINT ( 'NONE',  ( 10.00000000000000000, -30.00120703465222149, 22.64427369931158296 ) ) ;
#23496 = VECTOR ( 'NONE', #37354, 1000.000000000000000 ) ;
#23497 = DIRECTION ( 'NONE',  ( 0.000000000000000000, 0.000000000000000000, 1.000000000000000000 ) ) ;
#23498 = DIRECTION ( 'NONE',  ( -0.000000000000000000, -0.000000000000000000, 1.000000000000000000 ) ) ;
#23499 = ADVANCED_FACE ( 'NONE', ( #12181 ), #6558, .T. ) ;
#23500 = CARTESIAN_POINT ( 'NONE',  ( 62.50000000000000000, 7.654042494670957804E-15, -184.9999999999999432 ) ) ;
#23501 = FACE_OUTER_BOUND ( 'NONE', #12839, .T. ) ;
#23502 = ORIENTED_EDGE ( 'NONE', *, *, #15971, .F. ) ;
#23503 = CARTESIAN_POINT ( 'NONE',  ( -97.64999999999994884, -211.5299782133524502, 78.70229166840096013 ) ) ;
#23504 = ORIENTED_EDGE ( 'NONE', *, *, #49900, .T. ) ;
#23505 = EDGE_CURVE ( 'NONE', #38633, #9962, #58420, .T. ) ;
#23506 = CYLINDRICAL_SURFACE ( 'NONE', #32647, 82.00000000000000000 ) ;
#23507 = ORIENTED_EDGE ( 'NONE', *, *, #21266, .F. ) ;
#23509 = CARTESIAN_POINT ( 'NONE',  ( -97.65000000000001990, 91.52997821335253548, 79.23145833506762870 ) ) ;
#23508 = CARTESIAN_POINT ( 'NONE',  ( 97.64999999999997726, 88.47002178664753558, 80.18395833506764347 ) ) ;
#23510 = ORIENTED_EDGE ( 'NONE', *, *, #36711, .T. ) ;
#23511 = CARTESIAN_POINT ( 'NONE',  ( 94.99999999999998579, 87.33691857156068750, 79.16531250086715943 ) ) ;
#23512 = CARTESIAN_POINT ( 'NONE',  ( -94.99999999999997158, -206.9400435732949575, 82.22124999999999773 ) ) ;
#23513 = DIRECTION ( 'NONE',  ( 0.000000000000000000, 0.07845909572783790753, 0.9969173337331285190 ) ) ;
#23514 = CARTESIAN_POINT ( 'NONE',  ( 93.67500000000001137, -212.2949673200287179, 79.39020833506762642 ) ) ;
#23515 = DIRECTION ( 'NONE',  ( 0.000000000000000000, -0.5000000000000003331, -0.8660254037844383745 ) ) ;
#23516 = EDGE_CURVE ( 'NONE', #33091, #2294, #70419, .T. ) ;
#23517 = VERTEX_POINT ( 'NONE', #53521 ) ;
#23518 = CARTESIAN_POINT ( 'NONE',  ( 0.000000000000000000, 0.000000000000000000, 0.000000000000000000 ) ) ;
#23519 = CARTESIAN_POINT ( 'NONE',  ( 96.32499999999998863, -207.7050326799711968, 77.08833333333332405 ) ) ;
#23520 = CARTESIAN_POINT ( 'NONE',  ( -92.35000000000179909, 90.00000306648279036, 75.79187510780352000 ) ) ;
#23521 = VERTEX_POINT ( 'NONE', #7299 ) ;
#23522 = ORIENTED_EDGE ( 'NONE', *, *, #72158, .F. ) ;
#23523 = DIRECTION ( 'NONE',  ( 0.000000000000000000, 0.000000000000000000, -1.000000000000000000 ) ) ;
#23524 = EDGE_CURVE ( 'NONE', #16575, #36199, #13533, .T. ) ;
#23525 = CARTESIAN_POINT ( 'NONE',  ( -4.651285141664999401, -3.088081963278269004, -1.686035282245272215 ) ) ;
#23526 = CARTESIAN_POINT ( 'NONE',  ( -93.33864827736697123, -211.6008015735577033, 74.79754476654878204 ) ) ;
#23527 = CARTESIAN_POINT ( 'NONE',  ( -94.99999999999997158, -212.6630814284392557, 77.26031250086714408 ) ) ;
#23528 = ADVANCED_FACE ( 'NONE', ( #71164 ), #12916, .T. ) ;
#23529 = AXIS2_PLACEMENT_3D ( 'NONE', #41454, #58371, #29783 ) ;
#23530 = VERTEX_POINT ( 'NONE', #13661 ) ;
#23531 = DIRECTION ( 'NONE',  ( -1.000000000000000000, 0.000000000000000000, -0.000000000000000000 ) ) ;
#23532 = CIRCLE ( 'NONE', #9090, 16.00000000000000355 ) ;
#23533 = FACE_OUTER_BOUND ( 'NONE', #73958, .T. ) ;
#23534 = DIRECTION ( 'NONE',  ( -1.000000000000000000, 0.000000000000000000, 0.000000000000000000 ) ) ;
#23535 = AXIS2_PLACEMENT_3D ( 'NONE', #51938, #483, #23382 ) ;
#23536 = CARTESIAN_POINT ( 'NONE',  ( 96.73972734126400042, 91.51405112163766375, 74.79348190356853365 ) ) ;
#23537 = LINE ( 'NONE', #6618, #50835 ) ;
#23538 = DIRECTION ( 'NONE',  ( 1.000000000000000000, -0.000000000000000000, 0.000000000000000000 ) ) ;
#23539 = AXIS2_PLACEMENT_3D ( 'NONE', #12153, #28331, #57670 ) ;
#23540 = LINE ( 'NONE', #36663, #39745 ) ;
#23541 = CARTESIAN_POINT ( 'NONE',  ( 10.00000000000000000, -62.50329211542407393, -41.76937507738853839 ) ) ;
#23542 = FACE_OUTER_BOUND ( 'NONE', #6042, .T. ) ;
#23543 = CARTESIAN_POINT ( 'NONE',  ( 92.35000000052950497, -209.9999663481461027, 81.18829462297289012 ) ) ;
#23544 = EDGE_CURVE ( 'NONE', #43675, #71815, #36333, .T. ) ;
#23545 = AXIS2_PLACEMENT_3D ( 'NONE', #18524, #7262, #23805 ) ;
#23546 = CIRCLE ( 'NONE', #59614, 42.00000000000000000 ) ;
#23547 =( BOUNDED_CURVE ( )  B_SPLINE_CURVE ( 2, ( #29411, #46361, #52359, #11039, #35077, #17414, #23792 ),
 .UNSPECIFIED., .F., .F. ) 
 B_SPLINE_CURVE_WITH_KNOTS ( ( 3, 2, 2, 3 ),
 ( 0.2916666666666669072, 0.2986111111111113270, 0.3055555555555557468, 0.3125000000000001665 ),
 .UNSPECIFIED. ) 
 CURVE ( )  GEOMETRIC_REPRESENTATION_ITEM ( )  RATIONAL_B_SPLINE_CURVE ( ( 0.9999999999999956701, 0.8660254037844430375, 1.000000000000000000, 0.8660254037844387076, 1.000000000000000000, 0.8660254037844354880, 1.000000000000003109 ) ) 
 REPRESENTATION_ITEM ( '' )  );
#23548 = CARTESIAN_POINT ( 'NONE',  ( 96.15314808468748708, 88.00268892867053694, 88.74322916753382628 ) ) ;
#23549 = CARTESIAN_POINT ( 'NONE',  ( 0.000000000000000000, 75.11764819372149304, -2.946379043146603482 ) ) ;
#23550 = CARTESIAN_POINT ( 'NONE',  ( 12.00000000000000000, -26.23277895567251861, -4.042438405569750870 ) ) ;
#23551 = VERTEX_POINT ( 'NONE', #42254 ) ;
#23552 = CARTESIAN_POINT ( 'NONE',  ( 11.99999999999999822, -18.89407956138204980, -75.16055320797050854 ) ) ;
#23553 = CARTESIAN_POINT ( 'NONE',  ( -92.69370383062505425, 91.33154071421968467, 79.21822916753380639 ) ) ;
#23554 = VECTOR ( 'NONE', #28264, 1000.000000000000000 ) ;
#23555 = CARTESIAN_POINT ( 'NONE',  ( 96.15314808468748708, -208.0026889286704943, 88.16114583420046813 ) ) ;
#23556 = VERTEX_POINT ( 'NONE', #53894 ) ;
#23557 = CARTESIAN_POINT ( 'NONE',  ( 97.65000000000000568, -211.5299782133524218, 80.18395833506764347 ) ) ;
#23558 = CARTESIAN_POINT ( 'NONE',  ( 2.500000000000000000, 16.00000000000000000, -19.01812422950394676 ) ) ;
#23559 = VERTEX_POINT ( 'NONE', #59541 ) ;
#23560 = CARTESIAN_POINT ( 'NONE',  ( 10.00000000000000000, 0.000000000000000000, 0.000000000000000000 ) ) ;
#23562 = CIRCLE ( 'NONE', #800, 16.00000000000000355 ) ;
#23561 = PLANE ( 'NONE',  #33055 ) ;
#23563 = VERTEX_POINT ( 'NONE', #58798 ) ;
#23564 = ORIENTED_EDGE ( 'NONE', *, *, #7709, .F. ) ;
#23565 = CARTESIAN_POINT ( 'NONE',  ( 97.30629616937498838, -209.9999999999999716, 81.22906250086715829 ) ) ;
#23566 = CARTESIAN_POINT ( 'NONE',  ( 11.99999999999999822, -39.47590169984795239, -71.87247863392457248 ) ) ;
#23567 = CARTESIAN_POINT ( 'NONE',  ( 0.000000000000000000, -120.0000000000000000, 2.500000000000000000 ) ) ;
#23568 = LINE ( 'NONE', #63082, #8864 ) ;
#23569 = FACE_OUTER_BOUND ( 'NONE', #34403, .T. ) ;
#23570 = VECTOR ( 'NONE', #51534, 1000.000000000000000 ) ;
#23571 = LINE ( 'NONE', #35584, #41781 ) ;
#23572 = CARTESIAN_POINT ( 'NONE',  ( 92.35000000000002274, -208.4700217866474645, 84.86708333333334053 ) ) ;
#23573 = EDGE_CURVE ( 'NONE', #45686, #63002, #17144, .T. ) ;
#23574 = VERTEX_POINT ( 'NONE', #70801 ) ;
#23575 = ORIENTED_EDGE ( 'NONE', *, *, #72485, .T. ) ;
#23576 = ORIENTED_EDGE ( 'NONE', *, *, #51159, .F. ) ;
#23577 = VERTEX_POINT ( 'NONE', #41498 ) ;
#23578 = CARTESIAN_POINT ( 'NONE',  ( 0.000000000000000000, 5.202137450156907761, -37.22597642581151689 ) ) ;
#23579 = ADVANCED_FACE ( 'NONE', ( #65188 ), #2440, .T. ) ;
#23580 = CARTESIAN_POINT ( 'NONE',  ( -93.84685191531254134, 91.99731107132950569, 85.77989583420048803 ) ) ;
#23581 = AXIS2_PLACEMENT_3D ( 'NONE', #1635, #1996, #13603 ) ;
#23582 = CYLINDRICAL_SURFACE ( 'NONE', #68981, 77.49899999999999523 ) ;
#23583 = EDGE_CURVE ( 'NONE', #31033, #47197, #24223, .T. ) ;
#23584 = VECTOR ( 'NONE', #48731, 1000.000000000000000 ) ;
#23585 = CARTESIAN_POINT ( 'NONE',  ( -1.066668064568189757E-15, -1.540743955509788682E-30, -10.00000000000000178 ) ) ;
#23586 = CARTESIAN_POINT ( 'NONE',  ( 93.67500000000001137, -212.2949673200287179, 76.21520833506762926 ) ) ;
#23587 = EDGE_CURVE ( 'NONE', #14622, #57906, #53157, .T. ) ;
#23588 = CARTESIAN_POINT ( 'NONE',  ( 93.67499999999999716, 87.70503267997126784, 78.04083333333333883 ) ) ;
#23589 = EDGE_LOOP ( 'NONE', ( #35973, #18783, #61295, #19516, #40630, #31363 ) ) ;
#23590 = CARTESIAN_POINT ( 'NONE',  ( -92.34999999999999432, -211.5299782133524502, 89.07395833506762983 ) ) ;
#23591 = ORIENTED_EDGE ( 'NONE', *, *, #2011, .F. ) ;
#23592 = DIRECTION ( 'NONE',  ( 0.000000000000000000, 0.9945218953682732899, -0.1045284632676548031 ) ) ;
#23593 = AXIS2_PLACEMENT_3D ( 'NONE', #8649, #41741, #14646 ) ;
#23594 = EDGE_LOOP ( 'NONE', ( #62149, #3477, #30593, #47801 ) ) ;
#23595 = AXIS2_PLACEMENT_3D ( 'NONE', #66081, #8170, #2941 ) ;
#23596 = CARTESIAN_POINT ( 'NONE',  ( -96.32500000000001705, 92.29496732002878900, 88.06854166840095388 ) ) ;
#23597 = EDGE_CURVE ( 'NONE', #37377, #36873, #42360, .T. ) ;
#23598 = CARTESIAN_POINT ( 'NONE',  ( -96.15314808468751551, 88.00268892867056536, 81.65239583420049030 ) ) ;
#23599 = CARTESIAN_POINT ( 'NONE',  ( 97.30629616937498838, 90.00000000000002842, 88.84906250086716284 ) ) ;
#23600 = EDGE_LOOP ( 'NONE', ( #3172, #59014, #40426, #56720 ) ) ;
#23601 = CARTESIAN_POINT ( 'NONE',  ( -92.34999999999999432, -209.9999999999999716, 84.60249999999999204 ) ) ;
#23602 = CYLINDRICAL_SURFACE ( 'NONE', #18208, 32.00000000000000000 ) ;
#23603 = CARTESIAN_POINT ( 'NONE',  ( 11.99999999999999822, 0.000000000000000000, 0.000000000000000000 ) ) ;
#23604 = EDGE_CURVE ( 'NONE', #24357, #18771, #9939, .T. ) ;
#23605 = DIRECTION ( 'NONE',  ( -1.000000000000000000, -0.000000000000000000, -0.000000000000000000 ) ) ;
#23606 = ORIENTED_EDGE ( 'NONE', *, *, #31985, .F. ) ;
#23607 = LINE ( 'NONE', #52168, #24292 ) ;
#23608 = CARTESIAN_POINT ( 'NONE',  ( -97.30629616937497417, -211.3315407142195852, 78.26572916753380582 ) ) ;
#23609 = EDGE_LOOP ( 'NONE', ( #5860, #22307, #11479, #54895 ) ) ;
#23610 =( GEOMETRIC_REPRESENTATION_CONTEXT ( 3 ) GLOBAL_UNCERTAINTY_ASSIGNED_CONTEXT ( ( #36844 ) ) GLOBAL_UNIT_ASSIGNED_CONTEXT ( ( #18373, #18741, #7102 ) ) REPRESENTATION_CONTEXT ( 'NONE', 'WORKASPACE' ) );
#23611 = ORIENTED_EDGE ( 'NONE', *, *, #62214, .T. ) ;
#23612 = CARTESIAN_POINT ( 'NONE',  ( 97.64999999999999147, 90.00002660292301471, 78.96687592183759818 ) ) ;
#23613 = ORIENTED_EDGE ( 'NONE', *, *, #3016, .F. ) ;
#23614 = FACE_OUTER_BOUND ( 'NONE', #9813, .T. ) ;
#23615 = DIRECTION ( 'NONE',  ( -0.5000000000000051070, 1.060575238724903217E-16, -0.8660254037844355990 ) ) ;
#23616 = VERTEX_POINT ( 'NONE', #64077 ) ;
#23617 = CARTESIAN_POINT ( 'NONE',  ( -92.69370383062498320, -211.3315407142195852, 89.43114583420049257 ) ) ;
#23618 = ORIENTED_EDGE ( 'NONE', *, *, #44288, .F. ) ;
#23619 = LINE ( 'NONE', #23256, #20669 ) ;
#23620 = DIRECTION ( 'NONE',  ( -0.7273375899149802093, 0.6862798483830544471, 0.000000000000000000 ) ) ;
#23621 = EDGE_CURVE ( 'NONE', #28446, #40627, #38759, .T. ) ;
#23622 = ORIENTED_EDGE ( 'NONE', *, *, #52531, .T. ) ;
#23623 = ORIENTED_EDGE ( 'NONE', *, *, #5102, .F. ) ;
#23624 = DIRECTION ( 'NONE',  ( -1.000000000000000000, 0.000000000000000000, -0.000000000000000000 ) ) ;
#23625 = EDGE_CURVE ( 'NONE', #19963, #30236, #24380, .T. ) ;
#23626 = ADVANCED_FACE ( 'NONE', ( #7660 ), #30578, .T. ) ;
#23627 = DIRECTION ( 'NONE',  ( -1.000000000000000000, -0.000000000000000000, -0.000000000000000000 ) ) ;
#23628 = CARTESIAN_POINT ( 'NONE',  ( 97.30629616937498838, 91.33154071421968467, 84.29822916753380468 ) ) ;
#23629 = DIRECTION ( 'NONE',  ( -0.9966891607226785466, -0.08130631524009969413, 0.000000000000000000 ) ) ;
#23630 = CARTESIAN_POINT ( 'NONE',  ( 2.369999999999999662, 0.000000000000000000, 0.000000000000000000 ) ) ;
#23631 = DIRECTION ( 'NONE',  ( -0.000000000000000000, -0.000000000000000000, 1.000000000000000000 ) ) ;
#23632 = CARTESIAN_POINT ( 'NONE',  ( -95.00000000002611955, 90.00000000000007105, -75.00000000000000000 ) ) ;
#23633 = DIRECTION ( 'NONE',  ( 0.000000000000000000, 0.000000000000000000, 1.000000000000000000 ) ) ;
#23634 = CARTESIAN_POINT ( 'NONE',  ( 92.35000000000000853, -211.5299782133524218, 87.59229166840096070 ) ) ;
#23635 = DIRECTION ( 'NONE',  ( -1.000000000000000000, 0.000000000000000000, 0.000000000000000000 ) ) ;
#23636 = EDGE_CURVE ( 'NONE', #11405, #7655, #68823, .T. ) ;
#23637 = AXIS2_PLACEMENT_3D ( 'NONE', #9364, #27388, #50330 ) ;
#23638 = CARTESIAN_POINT ( 'NONE',  ( -92.34999999999999432, -209.9999999999999716, 85.23749999999999716 ) ) ;
#23639 = CYLINDRICAL_SURFACE ( 'NONE', #22972, 12.75000000000265388 ) ;
#23640 = FACE_OUTER_BOUND ( 'NONE', #40690, .T. ) ;
#23641 = DIRECTION ( 'NONE',  ( -0.000000000000000000, -0.000000000000000000, -1.000000000000000000 ) ) ;
#23642 = VECTOR ( 'NONE', #27239, 1000.000000000000114 ) ;
#23643 = VECTOR ( 'NONE', #24252, 1000.000000000000000 ) ;
#23644 = LINE ( 'NONE', #6365, #69265 ) ;
#23645 = CIRCLE ( 'NONE', #2056, 77.49900000000000944 ) ;
#23646 = ORIENTED_EDGE ( 'NONE', *, *, #72287, .T. ) ;
#23647 = LINE ( 'NONE', #36767, #7185 ) ;
#23648 = DIRECTION ( 'NONE',  ( 0.000000000000000000, 0.000000000000000000, 1.000000000000000000 ) ) ;
#23649 = DIRECTION ( 'NONE',  ( -1.000000000000000000, 0.000000000000000000, 0.000000000000000000 ) ) ;
#23650 = DIRECTION ( 'NONE',  ( -1.000000000000000000, 0.000000000000000000, 0.000000000000000000 ) ) ;
#23651 = CARTESIAN_POINT ( 'NONE',  ( 92.69370383062501162, -211.3315407142195852, 85.40947916753380298 ) ) ;
#23652 = CIRCLE ( 'NONE', #2066, 31.99999999999998579 ) ;
#23653 = ORIENTED_EDGE ( 'NONE', *, *, #20818, .F. ) ;
#23654 = ORIENTED_EDGE ( 'NONE', *, *, #30022, .F. ) ;
#23655 = CIRCLE ( 'NONE', #70428, 37.49900000000000233 ) ;
#23656 = ORIENTED_EDGE ( 'NONE', *, *, #2614, .F. ) ;
#23657 = CARTESIAN_POINT ( 'NONE',  ( 96.32499999999998863, -207.7050326799711968, 88.51833333333333087 ) ) ;
#23658 = LINE ( 'NONE', #29287, #42413 ) ;
#23659 = VERTEX_POINT ( 'NONE', #3884 ) ;
#23660 = CARTESIAN_POINT ( 'NONE',  ( 97.30629616937498838, -208.6684592857803011, 78.74197916753382742 ) ) ;
#23661 = EDGE_LOOP ( 'NONE', ( #61330, #46600, #66400, #71545 ) ) ;
#23662 = EDGE_CURVE ( 'NONE', #42171, #56693, #44090, .T. ) ;
#23663 = CARTESIAN_POINT ( 'NONE',  ( -7.469491406282116053, 4.756046723998915482, -45.00000000000000000 ) ) ;
#23664 = ORIENTED_EDGE ( 'NONE', *, *, #23754, .T. ) ;
#23665 = ORIENTED_EDGE ( 'NONE', *, *, #14699, .T. ) ;
#23666 = CARTESIAN_POINT ( 'NONE',  ( 2.500000000000034639, 90.00000000000000000, -310.0000000000000000 ) ) ;
#23667 = EDGE_CURVE ( 'NONE', #73780, #11355, #54993, .T. ) ;
#23668 =( LENGTH_UNIT ( ) NAMED_UNIT ( * ) SI_UNIT ( .MILLI., .METRE. ) );
#23669 = CARTESIAN_POINT ( 'NONE',  ( 5.000000000000000000, 46.11716303203188261, 67.80270845531904911 ) ) ;
#23670 = ORIENTED_EDGE ( 'NONE', *, *, #14406, .F. ) ;
#23671 = DIRECTION ( 'NONE',  ( -1.000000000000000000, 0.000000000000000000, 0.000000000000000000 ) ) ;
#23672 = CARTESIAN_POINT ( 'NONE',  ( 96.32499999999998863, -207.7050326799711968, 86.05770833506763040 ) ) ;
#23673 = EDGE_CURVE ( 'NONE', #68825, #16929, #60455, .T. ) ;
#23674 = ADVANCED_FACE ( 'NONE', ( #71906 ), #49711, .T. ) ;
#23675 = VERTEX_POINT ( 'NONE', #31688 ) ;
#23676 = CARTESIAN_POINT ( 'NONE',  ( 0.000000000000000000, 0.000000000000000000, 0.000000000000000000 ) ) ;
#23677 = EDGE_LOOP ( 'NONE', ( #8039, #18598, #29548, #70254 ) ) ;
#23678 = DIRECTION ( 'NONE',  ( -1.000000000000000000, -0.000000000000000000, 0.000000000000000000 ) ) ;
#23679 = VECTOR ( 'NONE', #18705, 1000.000000000000000 ) ;
#23680 = ORIENTED_EDGE ( 'NONE', *, *, #26501, .F. ) ;
#23682 = CARTESIAN_POINT ( 'NONE',  ( 96.32499999999998863, 87.70503267997126784, 84.57604166840096127 ) ) ;
#23681 = CIRCLE ( 'NONE', #20080, 82.00000000000000000 ) ;
#23683 = ORIENTED_EDGE ( 'NONE', *, *, #57213, .T. ) ;
#23684 = VERTEX_POINT ( 'NONE', #72635 ) ;
#23685 = DIRECTION ( 'NONE',  ( 1.000000000000000000, -0.000000000000000000, -0.000000000000000000 ) ) ;
#23686 = DIRECTION ( 'NONE',  ( -0.000000000000000000, -0.000000000000000000, -1.000000000000000000 ) ) ;
#23687 = ORIENTED_EDGE ( 'NONE', *, *, #7165, .F. ) ;
#23688 = VERTEX_POINT ( 'NONE', #4254 ) ;
#23689 = AXIS2_PLACEMENT_3D ( 'NONE', #68471, #73712, #22224 ) ;
#23690 = ORIENTED_EDGE ( 'NONE', *, *, #27988, .F. ) ;
#23691 = VECTOR ( 'NONE', #66362, 1000.000000000000000 ) ;
#23692 = CARTESIAN_POINT ( 'NONE',  ( 93.67499999999998295, 92.29496732002878900, 79.81354166840095843 ) ) ;
#23693 = CARTESIAN_POINT ( 'NONE',  ( 94.99999999999998579, 90.00000000000002842, 90.00000000000000000 ) ) ;
#23694 = EDGE_CURVE ( 'NONE', #6687, #21322, #37356, .T. ) ;
#23695 = CARTESIAN_POINT ( 'NONE',  ( -92.35000000000003695, 90.00000000000004263, 87.77749999999998920 ) ) ;
#23696 = ORIENTED_EDGE ( 'NONE', *, *, #48973, .T. ) ;
#23697 = CARTESIAN_POINT ( 'NONE',  ( -97.64999999999996305, -209.9999999999999716, 90.00000000000000000 ) ) ;
#23698 = EDGE_LOOP ( 'NONE', ( #20982, #24932, #43056, #72648 ) ) ;
#23699 = CARTESIAN_POINT ( 'NONE',  ( 14.09999999999999964, 0.000000000000000000, -1.199999999999999956 ) ) ;
#23700 = CARTESIAN_POINT ( 'NONE',  ( -93.84685191531247028, -211.9973110713294489, 84.13947916753380696 ) ) ;
#23701 = ORIENTED_EDGE ( 'NONE', *, *, #57302, .T. ) ;
#23702 = CARTESIAN_POINT ( 'NONE',  ( 0.000000000000000000, -46.21855187248585395, -62.20884554314068993 ) ) ;
#23703 = FACE_OUTER_BOUND ( 'NONE', #64373, .T. ) ;
#23704 = DIRECTION ( 'NONE',  ( -1.000000000000000000, 0.000000000000000000, 0.000000000000000000 ) ) ;
#23705 = CARTESIAN_POINT ( 'NONE',  ( -93.26027265873587169, -208.4859488783624215, 74.79348190356851944 ) ) ;
#23706 = CARTESIAN_POINT ( 'NONE',  ( 0.000000000000000000, -0.8660254037844384856, 1.500000000000000000 ) ) ;
#23707 = LINE ( 'NONE', #59043, #42756 ) ;
#23708 = ADVANCED_FACE ( 'NONE', ( #48622 ), #32424, .T. ) ;
#23709 = EDGE_CURVE ( 'NONE', #13504, #65473, #20780, .T. ) ;
#23710 = AXIS2_PLACEMENT_3D ( 'NONE', #26608, #72468, #73955 ) ;
#23711 = CARTESIAN_POINT ( 'NONE',  ( -119.3426274441927433, -132.5434155921188619, 5.500000000000000000 ) ) ;
#23712 = CARTESIAN_POINT ( 'NONE',  ( -17.26469406256017791, -140.1601175325492648, 5.500000000000000000 ) ) ;
#23713 = CYLINDRICAL_SURFACE ( 'NONE', #31515, 31.99999999999999289 ) ;
#23714 = CIRCLE ( 'NONE', #32124, 77.49899999999999523 ) ;
#23715 = CARTESIAN_POINT ( 'NONE',  ( 10.00000000000000000, 35.92658777277511462, 10.74501242461295014 ) ) ;
#23716 = CARTESIAN_POINT ( 'NONE',  ( -95.00000000000002842, 92.66308142843932671, 76.78406250086712248 ) ) ;
#23717 = DIRECTION ( 'NONE',  ( -1.000000000000000000, 0.000000000000000000, -0.000000000000000000 ) ) ;
#23718 = DIRECTION ( 'NONE',  ( -0.9918136447140101231, 0.1276937514489694114, 0.000000000000000000 ) ) ;
#23719 = VERTEX_POINT ( 'NONE', #21140 ) ;
#23720 = DIRECTION ( 'NONE',  ( 0.000000000000000000, 0.000000000000000000, 1.000000000000000000 ) ) ;
#23721 = DIRECTION ( 'NONE',  ( 0.000000000000000000, 0.9135454576426002005, 0.4067366430758017071 ) ) ;
#23722 = CARTESIAN_POINT ( 'NONE',  ( 0.000000000000000000, 40.68715046381943523, -10.41901085202036370 ) ) ;
#23723 = DIRECTION ( 'NONE',  ( 1.000000000000000000, -7.571539615859142926E-15, -2.592266024478009537E-14 ) ) ;
#23724 = FACE_OUTER_BOUND ( 'NONE', #23698, .T. ) ;
#23725 = CYLINDRICAL_SURFACE ( 'NONE', #36392, 12.75000000000000000 ) ;
#23726 = CARTESIAN_POINT ( 'NONE',  ( -97.30629616937497417, -208.6684592857803011, 77.04864583420048518 ) ) ;
#23727 = DIRECTION ( 'NONE',  ( 0.000000000000000000, -6.982962677686267499E-15, 1.000000000000000000 ) ) ;
#23728 = ORIENTED_EDGE ( 'NONE', *, *, #73905, .T. ) ;
#23729 = VECTOR ( 'NONE', #55196, 1000.000000000000000 ) ;
#23730 = DIRECTION ( 'NONE',  ( -1.000000000000000000, -0.000000000000000000, -0.000000000000000000 ) ) ;
#23731 = DIRECTION ( 'NONE',  ( -1.000000000000000000, 0.000000000000000000, 0.000000000000000000 ) ) ;
#23732 = FILL_AREA_STYLE_COLOUR ( '', #48977 ) ;
#23733 = DIRECTION ( 'NONE',  ( 1.000000000000000000, 0.000000000000000000, 0.000000000000000000 ) ) ;
#23734 = AXIS2_PLACEMENT_3D ( 'NONE', #59216, #31001, #65604 ) ;
#23735 = AXIS2_PLACEMENT_3D ( 'NONE', #29353, #47403, #63227 ) ;
#23736 = DIRECTION ( 'NONE',  ( 0.000000000000000000, 0.000000000000000000, 1.000000000000000000 ) ) ;
#23737 = VERTEX_POINT ( 'NONE', #60290 ) ;
#23738 = DIRECTION ( 'NONE',  ( 0.000000000000000000, 0.000000000000000000, 1.000000000000000000 ) ) ;
#23739 = CARTESIAN_POINT ( 'NONE',  ( 0.000000000000000000, 33.71516098798849015, -74.74816331893394761 ) ) ;
#23740 = VERTEX_POINT ( 'NONE', #43734 ) ;
#23741 =( BOUNDED_CURVE ( )  B_SPLINE_CURVE ( 2, ( #64805, #23103, #58407, #68963, #41487, #17448, #57686, #6188, #14759 ),
 .UNSPECIFIED., .F., .F. ) 
 B_SPLINE_CURVE_WITH_KNOTS ( ( 3, 2, 2, 2, 3 ),
 ( 0.1058364832022827134, 0.1128922486541179548, 0.1199480141950002993, 0.1270037797358826437, 0.1270039290051391268 ),
 .UNSPECIFIED. ) 
 CURVE ( )  GEOMETRIC_REPRESENTATION_ITEM ( )  RATIONAL_B_SPLINE_CURVE ( ( 1.000000000000000000, 0.8660254037844387076, 1.000000000000000000, 0.8660254037844387076, 1.000000000000000000, 0.8660254037844387076, 1.000000000000000000, 0.9999971656812787213, 0.9999943314824810692 ) ) 
 REPRESENTATION_ITEM ( '' )  );
#23742 = CARTESIAN_POINT ( 'NONE',  ( 96.15314808468750130, -211.9973110713294489, 85.40947916753380298 ) ) ;
#23743 = CARTESIAN_POINT ( 'NONE',  ( -20.63750000000000284, -2.946905753441389499E-14, -1.643265707204933640E-14 ) ) ;
#23744 = ORIENTED_EDGE ( 'NONE', *, *, #63338, .T. ) ;
#23745 = PRODUCT_DEFINITION ( 'UNKNOWN', '', #36436, #9293 ) ;
#23746 = ADVANCED_FACE ( 'NONE', ( #66654 ), #8771, .T. ) ;
#23747 = CARTESIAN_POINT ( 'NONE',  ( 10.00000000000000000, -46.11716303203234446, 67.80270845531873647 ) ) ;
#23748 = EDGE_LOOP ( 'NONE', ( #48354, #51887, #35349, #14547 ) ) ;
#23749 = CYLINDRICAL_SURFACE ( 'NONE', #4682, 11.59999999999999964 ) ;
#23750 = ORIENTED_EDGE ( 'NONE', *, *, #5299, .T. ) ;
#23751 = CARTESIAN_POINT ( 'NONE',  ( -92.69370383062502583, 88.66845928578038638, 80.54114583420049200 ) ) ;
#23752 = AXIS2_PLACEMENT_3D ( 'NONE', #73496, #4740, #62621 ) ;
#23753 = ORIENTED_EDGE ( 'NONE', *, *, #10595, .F. ) ;
#23754 = EDGE_CURVE ( 'NONE', #63641, #13981, #17188, .T. ) ;
#23755 = ORIENTED_EDGE ( 'NONE', *, *, #44211, .T. ) ;
#23756 = VECTOR ( 'NONE', #46168, 1000.000000000000000 ) ;
#23757 = VECTOR ( 'NONE', #21233, 1000.000000000000000 ) ;
#23758 = ORIENTED_EDGE ( 'NONE', *, *, #26796, .T. ) ;
#23759 = LINE ( 'NONE', #13578, #44939 ) ;
#23760 = CARTESIAN_POINT ( 'NONE',  ( 10.00000000000000000, -55.19960302592104284, 51.03279382321070301 ) ) ;
#23761 = AXIS2_PLACEMENT_3D ( 'NONE', #33138, #4603, #48947 ) ;
#23762 = EDGE_CURVE ( 'NONE', #7032, #14681, #37722, .T. ) ;
#23763 = VERTEX_POINT ( 'NONE', #26423 ) ;
#23764 = CARTESIAN_POINT ( 'NONE',  ( -3.961125083139900749, -143.2122702051246677, 5.500000000000000000 ) ) ;
#23765 = ORIENTED_EDGE ( 'NONE', *, *, #16751, .T. ) ;
#23766 = AXIS2_PLACEMENT_3D ( 'NONE', #68120, #50449, #16611 ) ;
#23767 = B_SPLINE_CURVE_WITH_KNOTS ( 'NONE', 3,
 ( #22528, #68398, #16138, #51455, #377, #11592, #57480, #14, #63139, #46202 ),
 .UNSPECIFIED., .F., .F.,
 ( 4, 2, 2, 2, 4 ),
 ( 0.01815567983891738443, 0.01899359644517026671, 0.01983151305142314552, 0.02066942965767602780, 0.02150734626392890661 ),
 .UNSPECIFIED. ) ;
#23768 =( BOUNDED_CURVE ( )  B_SPLINE_CURVE ( 2, ( #19254, #37671, #42205, #65140, #13613, #42566, #10191 ),
 .UNSPECIFIED., .F., .F. ) 
 B_SPLINE_CURVE_WITH_KNOTS ( ( 3, 2, 2, 3 ),
 ( 0.7831899741065913023, 0.7902457405788253508, 0.7973015061197076259, 0.8043570860654228882 ),
 .UNSPECIFIED. ) 
 CURVE ( )  GEOMETRIC_REPRESENTATION_ITEM ( )  RATIONAL_B_SPLINE_CURVE ( ( 1.000000000000000000, 0.8660254037844387076, 1.000000000000000000, 0.8660254037844387076, 1.000000000000000000, 0.8660289278581101424, 0.9999929520380519410 ) ) 
 REPRESENTATION_ITEM ( '' )  );
#23769 = CARTESIAN_POINT ( 'NONE',  ( 95.00000000000000000, -213.0599564267049857, 80.71312500173429783 ) ) ;
#23770 = EDGE_CURVE ( 'NONE', #30840, #26458, #15134, .T. ) ;
#23771 = VERTEX_POINT ( 'NONE', #61390 ) ;
#23772 = VERTEX_POINT ( 'NONE', #9872 ) ;
#23773 = ORIENTED_EDGE ( 'NONE', *, *, #53370, .T. ) ;
#23774 = CARTESIAN_POINT ( 'NONE',  ( 97.30629616937498838, -211.3315407142195852, 82.28739583420048120 ) ) ;
#23775 = APPLICATION_PROTOCOL_DEFINITION ( 'draft international standard', 'automotive_design', 1998, #59957 ) ;
#23776 = CARTESIAN_POINT ( 'NONE',  ( 10.00000000000000000, 44.88180994100376608, 63.18004540533043922 ) ) ;
#23777 = DIRECTION ( 'NONE',  ( -0.000000000000000000, -0.000000000000000000, 1.000000000000000000 ) ) ;
#23778 = CARTESIAN_POINT ( 'NONE',  ( 10.00000000000000000, -5.202137450156129717, -37.22597642581163768 ) ) ;
#23779 = LINE ( 'NONE', #57260, #41560 ) ;
#23780 = DIRECTION ( 'NONE',  ( -0.000000000000000000, -1.000000000000000000, -0.000000000000000000 ) ) ;
#23781 = CARTESIAN_POINT ( 'NONE',  ( -97.65000000000001990, 90.00000000000004263, 82.37999999999999545 ) ) ;
#23782 = CARTESIAN_POINT ( 'NONE',  ( -94.99999999999997158, -212.6630814284392557, 85.35656250086714181 ) ) ;
#23783 = ADVANCED_FACE ( 'NONE', ( #55369 ), #61007, .T. ) ;
#23784 = CARTESIAN_POINT ( 'NONE',  ( -97.30629616937501680, 90.00000000000004263, 80.91156250086716284 ) ) ;
#23785 = EDGE_CURVE ( 'NONE', #9630, #4678, #26773, .T. ) ;
#23786 = ORIENTED_EDGE ( 'NONE', *, *, #20727, .F. ) ;
#23787 = CARTESIAN_POINT ( 'NONE',  ( 92.69370383062498320, 88.66845928578037217, 84.61572916753380014 ) ) ;
#23788 = ORIENTED_EDGE ( 'NONE', *, *, #33009, .F. ) ;
#23789 = DIRECTION ( 'NONE',  ( 0.000000000000000000, 1.078060571631605808E-14, 1.000000000000000000 ) ) ;
#23790 = VECTOR ( 'NONE', #15994, 1000.000000000000000 ) ;
#23791 = CARTESIAN_POINT ( 'NONE',  ( 10.00000000000000000, 33.71516098798847594, -74.74816331893393340 ) ) ;
#23792 = CARTESIAN_POINT ( 'NONE',  ( 97.64999999999999147, -209.9999999999999716, 85.23749999999999716 ) ) ;
#23793 = CARTESIAN_POINT ( 'NONE',  ( -97.30629616937497417, -211.3315407142195852, 85.25072916753379104 ) ) ;
#23794 = CIRCLE ( 'NONE', #32142, 31.99999999999998224 ) ;
#23795 = LINE ( 'NONE', #18152, #733 ) ;
#23796 = DIRECTION ( 'NONE',  ( 0.000000000000000000, 0.9510565162951544194, -0.3090169943749447867 ) ) ;
#23797 = CARTESIAN_POINT ( 'NONE',  ( 0.000000000000000000, 74.65374052328660071, -8.840884882374309583 ) ) ;
#23798 = CARTESIAN_POINT ( 'NONE',  ( 5.000000000000000000, -2.886751345948134428, -6.000000000000000000 ) ) ;
#23799 = ORIENTED_EDGE ( 'NONE', *, *, #21475, .T. ) ;
#23800 = EDGE_CURVE ( 'NONE', #69032, #14021, #31322, .T. ) ;
#23801 = CIRCLE ( 'NONE', #65818, 37.49900000000000233 ) ;
#23802 = ORIENTED_EDGE ( 'NONE', *, *, #65880, .T. ) ;
#23803 = AXIS2_PLACEMENT_3D ( 'NONE', #31304, #37338, #55723 ) ;
#23804 = CARTESIAN_POINT ( 'NONE',  ( -92.35000000000005116, 91.52997821335253548, 77.03541666666666288 ) ) ;
#23805 = DIRECTION ( 'NONE',  ( 0.000000000000000000, 0.000000000000000000, -1.000000000000000000 ) ) ;
#23806 = CARTESIAN_POINT ( 'NONE',  ( -97.30629616937501680, 90.00000000000004263, 87.10281250086714522 ) ) ;
#23807 = FACE_OUTER_BOUND ( 'NONE', #24307, .T. ) ;
#23808 = CARTESIAN_POINT ( 'NONE',  ( 0.000000000000000000, -0.8299999999999999600, 0.000000000000000000 ) ) ;
#23809 = CARTESIAN_POINT ( 'NONE',  ( 11.99999999999999822, -68.55367621811173251, 44.99326035066031437 ) ) ;
#23810 = CARTESIAN_POINT ( 'NONE',  ( -8.000000000000012434, -2.554949287172803747E-13, -22.90000000000042490 ) ) ;
#23811 = VERTEX_POINT ( 'NONE', #50829 ) ;
#23812 = CARTESIAN_POINT ( 'NONE',  ( -97.30629616937501680, 90.00000000000004263, 80.11781250086713158 ) ) ;
#23813 = CARTESIAN_POINT ( 'NONE',  ( 0.000000000000000000, 34.44570377933598593, 69.42325613327452061 ) ) ;
#23814 = DIRECTION ( 'NONE',  ( -1.000000000000000000, -0.000000000000000000, 0.000000000000000000 ) ) ;
#23815 = AXIS2_PLACEMENT_3D ( 'NONE', #42915, #30137, #65843 ) ;
#23816 = FACE_OUTER_BOUND ( 'NONE', #14781, .T. ) ;
#23817 = DIRECTION ( 'NONE',  ( -1.000000000000000000, 0.000000000000000000, 0.000000000000000000 ) ) ;
#23818 = AXIS2_PLACEMENT_3D ( 'NONE', #49483, #71289, #31072 ) ;
#23819 = CARTESIAN_POINT ( 'NONE',  ( 0.000000000000000000, 0.000000000000000000, 0.000000000000000000 ) ) ;
#23820 = CARTESIAN_POINT ( 'NONE',  ( -96.15314808468745866, -211.9973110713294489, 84.82739583420048746 ) ) ;
#23821 =( NAMED_UNIT ( * ) SI_UNIT ( $, .STERADIAN. ) SOLID_ANGLE_UNIT ( ) );
#23822 = AXIS2_PLACEMENT_3D ( 'NONE', #47882, #59173, #7662 ) ;
#23823 = CIRCLE ( 'NONE', #73003, 82.00000000000000000 ) ;
#23824 = LINE ( 'NONE', #69685, #22119 ) ;
#23825 = AXIS2_PLACEMENT_3D ( 'NONE', #9030, #20681, #3784 ) ;
#23826 = CARTESIAN_POINT ( 'NONE',  ( 92.69370383062498320, 88.66845928578035796, 77.78947916753381264 ) ) ;
#23827 = ADVANCED_FACE ( 'NONE', ( #56859 ), #11709, .F. ) ;
#23828 = CARTESIAN_POINT ( 'NONE',  ( -94.99999999999997158, -207.3369185715606307, 76.30781250086715772 ) ) ;
#23829 = LINE ( 'NONE', #63698, #37452 ) ;
#23830 = ORIENTED_EDGE ( 'NONE', *, *, #29973, .T. ) ;
#23831 = CARTESIAN_POINT ( 'NONE',  ( 0.000000000000000000, 0.000000000000000000, 0.000000000000000000 ) ) ;
#23832 = DIRECTION ( 'NONE',  ( 0.000000000000000000, 0.000000000000000000, 1.000000000000000000 ) ) ;
#23833 = LINE ( 'NONE', #18190, #40221 ) ;
#23834 = EDGE_CURVE ( 'NONE', #50224, #5801, #13860, .T. ) ;
#23835 = CARTESIAN_POINT ( 'NONE',  ( -95.00000000000002842, 92.66308142843932671, 75.03781250086714749 ) ) ;
#23836 = CARTESIAN_POINT ( 'NONE',  ( 96.15314808468750130, -211.9973110713294489, 77.15447916753380753 ) ) ;
#23837 = ORIENTED_EDGE ( 'NONE', *, *, #69365, .F. ) ;
#23838 = EDGE_CURVE ( 'NONE', #59443, #12497, #63899, .T. ) ;
#23839 = DIRECTION ( 'NONE',  ( -1.000000000000000000, 0.000000000000000000, -0.000000000000000000 ) ) ;
#23840 = ORIENTED_EDGE ( 'NONE', *, *, #54491, .F. ) ;
#23841 = AXIS2_PLACEMENT_3D ( 'NONE', #29948, #45796, #52146 ) ;
#23842 = DIRECTION ( 'NONE',  ( -2.628368902995175337E-16, -1.000000000000000000, 0.000000000000000000 ) ) ;
#23843 = ORIENTED_EDGE ( 'NONE', *, *, #56543, .T. ) ;
#23844 = CIRCLE ( 'NONE', #33432, 82.00000000000000000 ) ;
#23845 = EDGE_CURVE ( 'NONE', #20436, #29463, #1145, .T. ) ;
#23846 = CARTESIAN_POINT ( 'NONE',  ( 5.000000000000002665, -68.55367621811173251, 44.99326035066031437 ) ) ;
#23847 = CIRCLE ( 'NONE', #27428, 16.00000000000000000 ) ;
#23848 = ORIENTED_EDGE ( 'NONE', *, *, #66878, .T. ) ;
#23849 = ORIENTED_EDGE ( 'NONE', *, *, #26845, .T. ) ;
#23850 = CIRCLE ( 'NONE', #35855, 82.00000000000000000 ) ;
#23851 = VERTEX_POINT ( 'NONE', #57883 ) ;
#23852 = DIRECTION ( 'NONE',  ( 1.000000000000000000, 0.000000000000000000, 0.000000000000000000 ) ) ;
#23853 = ORIENTED_EDGE ( 'NONE', *, *, #36572, .F. ) ;
#23854 = ORIENTED_EDGE ( 'NONE', *, *, #62423, .F. ) ;
#23855 = CARTESIAN_POINT ( 'NONE',  ( 97.30629616937498838, 88.66845928578037217, 84.35114583420049428 ) ) ;
#23856 = DIRECTION ( 'NONE',  ( -1.000000000000000000, -0.000000000000000000, -0.000000000000000000 ) ) ;
#23857 = EDGE_CURVE ( 'NONE', #54220, #27635, #3998, .T. ) ;
#23858 = DIRECTION ( 'NONE',  ( -1.000000000000000000, -0.000000000000000000, -0.000000000000000000 ) ) ;
#23859 = ORIENTED_EDGE ( 'NONE', *, *, #18438, .F. ) ;
#23861 = ORIENTED_EDGE ( 'NONE', *, *, #68432, .T. ) ;
#23860 = AXIS2_PLACEMENT_3D ( 'NONE', #61461, #9578, #72703 ) ;
#23862 = ORIENTED_EDGE ( 'NONE', *, *, #58465, .F. ) ;
#23863 = ORIENTED_EDGE ( 'NONE', *, *, #63417, .F. ) ;
#23864 = FACE_OUTER_BOUND ( 'NONE', #52126, .T. ) ;
#23865 = ORIENTED_EDGE ( 'NONE', *, *, #70191, .F. ) ;
#23866 = AXIS2_PLACEMENT_3D ( 'NONE', #59371, #18393, #36063 ) ;
#23867 = CARTESIAN_POINT ( 'NONE',  ( 1.257674520083185143E-13, -3.848917712323540741E-15, 36.50000000000000711 ) ) ;
#23868 = CARTESIAN_POINT ( 'NONE',  ( -92.34999999999995168, -208.4700217866474929, 85.29041666666665833 ) ) ;
#23869 = CARTESIAN_POINT ( 'NONE',  ( 0.000000000000000000, 73.72996012237460661, -14.67089635893632504 ) ) ;
#23870 = CARTESIAN_POINT ( 'NONE',  ( -22.53294031248082163, -134.0273518838794757, 2.500000000000000000 ) ) ;
#23871 = CARTESIAN_POINT ( 'NONE',  ( 26.50000000000218847, -120.0000000000000000, -48.99999999999928946 ) ) ;
#23872 = CARTESIAN_POINT ( 'NONE',  ( -42.50000000000000000, 0.000000000000000000, 0.000000000000000000 ) ) ;
#23873 = AXIS2_PLACEMENT_3D ( 'NONE', #27066, #20699, #72917 ) ;
#23874 = DIRECTION ( 'NONE',  ( -1.000000000000000000, 0.000000000000000000, 0.000000000000000000 ) ) ;
#23875 = AXIS2_PLACEMENT_3D ( 'NONE', #74119, #73742, #33903 ) ;
#23876 = ORIENTED_EDGE ( 'NONE', *, *, #52866, .F. ) ;
#23877 = CARTESIAN_POINT ( 'NONE',  ( -92.34999999999999432, -208.4700217866474645, 77.74979166840097378 ) ) ;
#23879 = ORIENTED_EDGE ( 'NONE', *, *, #72375, .T. ) ;
#23878 = EDGE_CURVE ( 'NONE', #37933, #62989, #34563, .T. ) ;
#23880 = FACE_OUTER_BOUND ( 'NONE', #51583, .T. ) ;
#23881 = EDGE_CURVE ( 'NONE', #69032, #68072, #7481, .T. ) ;
#23882 = ORIENTED_EDGE ( 'NONE', *, *, #56037, .T. ) ;
#23884 = CARTESIAN_POINT ( 'NONE',  ( -92.35000000000003695, 90.00000000000004263, 80.87187500173430976 ) ) ;
#23883 = CARTESIAN_POINT ( 'NONE',  ( 97.64999999999999147, 90.00000000000002842, 80.87187500173430976 ) ) ;
#23885 = CIRCLE ( 'NONE', #65912, 42.00000000000000000 ) ;
#23887 = EDGE_CURVE ( 'NONE', #6682, #65091, #23658, .T. ) ;
#23886 = ORIENTED_EDGE ( 'NONE', *, *, #73993, .F. ) ;
#23888 = CARTESIAN_POINT ( 'NONE',  ( 93.84685191531248449, 91.99731107132950569, 81.44072916753381719 ) ) ;
#23889 = CARTESIAN_POINT ( 'NONE',  ( 24.95699195200416654, -110.9640411295978595, 5.500000000000000000 ) ) ;
#23890 = CARTESIAN_POINT ( 'NONE',  ( 0.000000000000000000, -68.67312586195022561, 35.91791733033451806 ) ) ;
#23891 = DIRECTION ( 'NONE',  ( -1.000000000000000000, 0.000000000000000000, 0.000000000000000000 ) ) ;
#23892 = LINE ( 'NONE', #7700, #54616 ) ;
#23893 = VERTEX_POINT ( 'NONE', #28927 ) ;
#23894 = CARTESIAN_POINT ( 'NONE',  ( 10.00000000000000000, 30.84782396557248418, -21.32104025579081252 ) ) ;
#23895 = VERTEX_POINT ( 'NONE', #46227 ) ;
#23896 = ORIENTED_EDGE ( 'NONE', *, *, #10535, .T. ) ;
#23897 = SHAPE_REPRESENTATION ( 'Sliding Dog Clutch Collar', ( #43395 ), #7372 ) ;
#23898 = VECTOR ( 'NONE', #62458, 1000.000000000000000 ) ;
#23899 = CARTESIAN_POINT ( 'NONE',  ( -1.546821644788046735, -4.880444798889548963, -0.7375898304884659362 ) ) ;
#23900 = CARTESIAN_POINT ( 'NONE',  ( -93.25528180581923721, -211.6811075874705352, 74.86350982016035971 ) ) ;
#23901 = CARTESIAN_POINT ( 'NONE',  ( -97.30629616937497417, -208.6684592857803011, 78.31864583420050963 ) ) ;
#23902 = AXIS2_PLACEMENT_3D ( 'NONE', #71929, #12933, #2081 ) ;
#23903 = VERTEX_POINT ( 'NONE', #69521 ) ;
#23904 = AXIS2_PLACEMENT_3D ( 'NONE', #3047, #19555, #65072 ) ;
#23905 = FACE_OUTER_BOUND ( 'NONE', #10187, .T. ) ;
#23906 = CARTESIAN_POINT ( 'NONE',  ( 5.000000000000002665, -74.18225833017864090, -34.94270380257719211 ) ) ;
#23907 = VECTOR ( 'NONE', #13812, 1000.000000000000000 ) ;
#23908 = CARTESIAN_POINT ( 'NONE',  ( 97.64999999999999147, 89.99999998014077107, 85.95187500101400246 ) ) ;
#23909 = DIRECTION ( 'NONE',  ( -1.000000000000000000, 0.000000000000000000, 0.000000000000000000 ) ) ;
#23910 = AXIS2_PLACEMENT_3D ( 'NONE', #63149, #7467, #64612 ) ;
#23911 = FACE_OUTER_BOUND ( 'NONE', #55679, .T. ) ;
#23912 = CARTESIAN_POINT ( 'NONE',  ( 0.000000000000000000, -77.32052557432845674, 5.256550761632577284 ) ) ;
#23913 = CARTESIAN_POINT ( 'NONE',  ( 0.000000000000000000, 0.000000000000000000, 0.000000000000000000 ) ) ;
#23914 = CARTESIAN_POINT ( 'NONE',  ( 93.67499999999998295, 92.29496732002878900, 86.16354166840096696 ) ) ;
#23915 = PLANE ( 'NONE',  #6401 ) ;
#23916 = FACE_OUTER_BOUND ( 'NONE', #47648, .T. ) ;
#23917 = CARTESIAN_POINT ( 'NONE',  ( 92.69370383062498320, 88.66845928578035796, 87.31447916753381833 ) ) ;
#23918 = CIRCLE ( 'NONE', #1148, 31.99999999999998224 ) ;
#23919 = CARTESIAN_POINT ( 'NONE',  ( -92.69370383062498320, -211.3315407142195852, 85.62114583420047609 ) ) ;
#23920 = DIRECTION ( 'NONE',  ( 0.000000000000000000, 0.000000000000000000, 1.000000000000000000 ) ) ;
#23921 = VECTOR ( 'NONE', #54487, 1000.000000000000000 ) ;
#23923 = EDGE_CURVE ( 'NONE', #1787, #41677, #30395, .T. ) ;
#23922 = VERTEX_POINT ( 'NONE', #57512 ) ;
#23924 = DIRECTION ( 'NONE',  ( 0.000000000000000000, 1.000000000000000000, 0.000000000000000000 ) ) ;
#23925 = CARTESIAN_POINT ( 'NONE',  ( -94.99999999999997158, -213.0599564267049857, 80.63375000000000625 ) ) ;
#23926 = CARTESIAN_POINT ( 'NONE',  ( 10.00000000000000000, -26.08949754953005495, -27.05870788708258701 ) ) ;
#23927 = CIRCLE ( 'NONE', #3548, 31.99999999999998579 ) ;
#23928 = AXIS2_PLACEMENT_3D ( 'NONE', #15279, #38593, #32929 ) ;
#23929 = EDGE_CURVE ( 'NONE', #6219, #28446, #51864, .T. ) ;
#23930 = CIRCLE ( 'NONE', #11890, 77.49900000000000944 ) ;
#23931 = CARTESIAN_POINT ( 'NONE',  ( 96.15314808468748708, -208.0026889286704943, 86.25614583420048120 ) ) ;
#23932 = EDGE_CURVE ( 'NONE', #2456, #10395, #41224, .T. ) ;
#23933 =( REPRESENTATION_RELATIONSHIP ('NONE','NONE', #31117, #65179 ) REPRESENTATION_RELATIONSHIP_WITH_TRANSFORMATION ( #66230 )SHAPE_REPRESENTATION_RELATIONSHIP( ) );
#23934 = ORIENTED_EDGE ( 'NONE', *, *, #66976, .T. ) ;
#23935 = AXIS2_PLACEMENT_3D ( 'NONE', #12272, #40865, #18287 ) ;
#23936 = ORIENTED_EDGE ( 'NONE', *, *, #30719, .F. ) ;
#23937 = ADVANCED_FACE ( 'NONE', ( #19485 ), #65733, .T. ) ;
#23938 = CARTESIAN_POINT ( 'NONE',  ( 11.99999999999999822, 77.32052557432849937, -5.256550761632002633 ) ) ;
#23939 = PLANE ( 'NONE',  #12621 ) ;
#23940 = ORIENTED_EDGE ( 'NONE', *, *, #67126, .F. ) ;
#23941 = ORIENTED_EDGE ( 'NONE', *, *, #23878, .F. ) ;
#23942 = CARTESIAN_POINT ( 'NONE',  ( 92.69370383062501162, -208.6684592857803295, 82.76364583420048859 ) ) ;
#23943 = CARTESIAN_POINT ( 'NONE',  ( 10.00000000000000000, -22.74946021919110706, -29.81001611431033282 ) ) ;
#23944 = CARTESIAN_POINT ( 'NONE',  ( 0.000000000000000000, -55.19960302592104284, 51.03279382321070301 ) ) ;
#23945 = LINE ( 'NONE', #29935, #28073 ) ;
#23946 = LINE ( 'NONE', #22847, #73484 ) ;
#23947 = VECTOR ( 'NONE', #46357, 1000.000000000000000 ) ;
#23948 = ADVANCED_FACE ( 'NONE', ( #37540 ), #59726, .F. ) ;
#23949 = FACE_OUTER_BOUND ( 'NONE', #69969, .T. ) ;
#23950 = CARTESIAN_POINT ( 'NONE',  ( 97.64999999999999147, -209.9999999999999716, 85.23749999999999716 ) ) ;
#23951 = CIRCLE ( 'NONE', #63575, 12.50000000000022560 ) ;
#23952 = AXIS2_PLACEMENT_3D ( 'NONE', #7340, #13335, #43032 ) ;
#23953 = ORIENTED_EDGE ( 'NONE', *, *, #32730, .F. ) ;
#23954 = ORIENTED_EDGE ( 'NONE', *, *, #39567, .T. ) ;
#23955 = AXIS2_PLACEMENT_3D ( 'NONE', #49851, #4024, #16775 ) ;
#23956 = ORIENTED_EDGE ( 'NONE', *, *, #58148, .T. ) ;
#23957 = ORIENTED_EDGE ( 'NONE', *, *, #54932, .F. ) ;
#23958 = DIRECTION ( 'NONE',  ( 0.000000000000000000, 0.000000000000000000, 1.000000000000000000 ) ) ;
#23959 = FILL_AREA_STYLE ('',( #1065 ) ) ;
#23960 = CARTESIAN_POINT ( 'NONE',  ( -97.30629616937501680, 88.66845928578038638, 86.67947916753382742 ) ) ;
#23961 = CARTESIAN_POINT ( 'NONE',  ( 0.000000000000000000, 35.91791733033475253, 68.67312586195009771 ) ) ;
#23962 = AXIS2_PLACEMENT_3D ( 'NONE', #70416, #53518, #6283 ) ;
#23963 = DIRECTION ( 'NONE',  ( 0.000000000000000000, 0.000000000000000000, 1.000000000000000000 ) ) ;
#23964 = CARTESIAN_POINT ( 'NONE',  ( 95.00000000000000000, -207.3369185715606307, 88.21406250086714351 ) ) ;
#23965 = CARTESIAN_POINT ( 'NONE',  ( 97.64999999999997726, 91.52997821335252127, 79.57541666666665492 ) ) ;
#23966 = ORIENTED_EDGE ( 'NONE', *, *, #45421, .F. ) ;
#23967 = FACE_OUTER_BOUND ( 'NONE', #43123, .T. ) ;
#23968 = VERTEX_POINT ( 'NONE', #60111 ) ;
#23969 = ADVANCED_FACE ( 'NONE', ( #30759 ), #72100, .F. ) ;
#23970 = CARTESIAN_POINT ( 'NONE',  ( 11.99999999999999822, -12.93880638057260946, -76.41127070299286572 ) ) ;
#23971 = ADVANCED_FACE ( 'NONE', ( #2622 ), #25503, .T. ) ;
#23972 = ORIENTED_EDGE ( 'NONE', *, *, #17167, .F. ) ;
#23973 = CARTESIAN_POINT ( 'NONE',  ( -97.65000000000001990, 91.52997821335253548, 88.12145833506762926 ) ) ;
#23974 = CARTESIAN_POINT ( 'NONE',  ( 92.69370383062498320, 91.33154071421968467, 76.25489583420049655 ) ) ;
#23975 = EDGE_LOOP ( 'NONE', ( #678, #256, #4406, #4352 ) ) ;
#23976 = DIRECTION ( 'NONE',  ( 0.000000000000000000, 0.000000000000000000, 1.000000000000000000 ) ) ;
#23977 = FACE_OUTER_BOUND ( 'NONE', #24947, .T. ) ;
#23978 = AXIS2_PLACEMENT_3D ( 'NONE', #69918, #18417, #42476 ) ;
#23979 = CYLINDRICAL_SURFACE ( 'NONE', #47385, 2.649999999999985700 ) ;
#23980 = CARTESIAN_POINT ( 'NONE',  ( 11.99999999999999822, 70.52718814184260054, 26.02418014898334420 ) ) ;
#23981 = ORIENTED_EDGE ( 'NONE', *, *, #32237, .T. ) ;
#23982 = LINE ( 'NONE', #22502, #73536 ) ;
#23983 = AXIS2_PLACEMENT_3D ( 'NONE', #38942, #39695, #10739 ) ;
#23985 = CARTESIAN_POINT ( 'NONE',  ( 0.000000000000000000, -27.74655509720617275, -77.16300072079690153 ) ) ;
#23984 = CIRCLE ( 'NONE', #25212, 31.99999999999999289 ) ;
#23986 = ORIENTED_EDGE ( 'NONE', *, *, #29706, .T. ) ;
#23987 = ORIENTED_EDGE ( 'NONE', *, *, #59502, .F. ) ;
#23988 = CARTESIAN_POINT ( 'NONE',  ( -12.50000000000000000, -107.5000000000000000, 40.00000000000000000 ) ) ;
#23989 = CIRCLE ( 'NONE', #33571, 31.99999999999999289 ) ;
#23990 = CIRCLE ( 'NONE', #55205, 15.99999999999999822 ) ;
#23991 = EDGE_LOOP ( 'NONE', ( #72285, #72734, #57510, #39519 ) ) ;
#23992 = LINE ( 'NONE', #35995, #37234 ) ;
#23993 = CARTESIAN_POINT ( 'NONE',  ( -11.59517495878806947, -96.12423995607481686, -2.500000000000000000 ) ) ;
#23994 = ORIENTED_EDGE ( 'NONE', *, *, #8345, .T. ) ;
#23995 =( BOUNDED_CURVE ( )  B_SPLINE_CURVE ( 2, ( #49919, #21336, #44293, #42814, #48812, #55940, #49552, #14973, #61224 ),
 .UNSPECIFIED., .F., .F. ) 
 B_SPLINE_CURVE_WITH_KNOTS ( ( 3, 2, 2, 2, 3 ),
 ( 0.000000000000000000, 0.007055765540882369576, 0.01411153108176473915, 0.02116729662264710959, 0.02116741234826251261 ),
 .UNSPECIFIED. ) 
 CURVE ( )  GEOMETRIC_REPRESENTATION_ITEM ( )  RATIONAL_B_SPLINE_CURVE ( ( 1.000000000000000000, 0.8660254037844387076, 1.000000000000000000, 0.8660254037844387076, 1.000000000000000000, 0.8660254037844387076, 1.000000000000000000, 0.9999978026066050907, 0.9999956052852916333 ) ) 
 REPRESENTATION_ITEM ( '' )  );
#23996 = CARTESIAN_POINT ( 'NONE',  ( -92.69370383062498320, -208.6684592857803011, 88.90197916753382401 ) ) ;
#23997 = ORIENTED_EDGE ( 'NONE', *, *, #42435, .F. ) ;
#23998 = DIRECTION ( 'NONE',  ( -1.000000000000000000, -0.000000000000000000, -0.000000000000000000 ) ) ;
#23999 = DIRECTION ( 'NONE',  ( -1.000000000000000000, -0.000000000000000000, 0.000000000000000000 ) ) ;
#24000 = VERTEX_POINT ( 'NONE', #66479 ) ;
#24001 = ORIENTED_EDGE ( 'NONE', *, *, #19583, .F. ) ;
#24002 = DIRECTION ( 'NONE',  ( -1.000000000000000000, -0.000000000000000000, 0.000000000000000000 ) ) ;
#24003 =( LENGTH_UNIT ( ) NAMED_UNIT ( * ) SI_UNIT ( .MILLI., .METRE. ) );
#24004 = CARTESIAN_POINT ( 'NONE',  ( 94.99999999999998579, 87.33691857156068750, 82.18156250086715886 ) ) ;
#24005 = DIRECTION ( 'NONE',  ( 0.000000000000000000, 0.000000000000000000, 1.000000000000000000 ) ) ;
#24006 = DIRECTION ( 'NONE',  ( -1.000000000000000000, -0.000000000000000000, -0.000000000000000000 ) ) ;
#24007 = CARTESIAN_POINT ( 'NONE',  ( 11.99999999999999822, -6.903761155838323837, 77.19088730480521576 ) ) ;
#24008 = DIRECTION ( 'NONE',  ( 1.000000000000000000, 0.000000000000000000, 0.000000000000000000 ) ) ;
#24009 = CARTESIAN_POINT ( 'NONE',  ( 5.000000000000000000, -38.55633173626998911, -16.65560815589452304 ) ) ;
#24010 = CARTESIAN_POINT ( 'NONE',  ( 92.35000000000000853, -209.9999999999999716, 90.00000000000000000 ) ) ;
#24011 = CARTESIAN_POINT ( 'NONE',  ( 11.99999999999999822, -63.18004540533059554, 44.88180994100355292 ) ) ;
#24012 = EDGE_CURVE ( 'NONE', #11350, #51481, #47195, .T. ) ;
#24013 = CYLINDRICAL_SURFACE ( 'NONE', #13227, 31.99999999999998579 ) ;
#24014 = CIRCLE ( 'NONE', #64801, 77.49900000000000944 ) ;
#24015 = EDGE_CURVE ( 'NONE', #55862, #34944, #12400, .T. ) ;
#24016 = LINE ( 'NONE', #40940, #45781 ) ;
#24017 = AXIS2_PLACEMENT_3D ( 'NONE', #26484, #9566, #32486 ) ;
#24018 = CARTESIAN_POINT ( 'NONE',  ( -95.00000000000002842, 92.66308142843932671, 86.94406250086714749 ) ) ;
#24019 = DIRECTION ( 'NONE',  ( 0.000000000000000000, -0.3826834323650772363, -0.9238795325112919565 ) ) ;
#24020 = EDGE_CURVE ( 'NONE', #15645, #27772, #55188, .T. ) ;
#24021 = AXIS2_PLACEMENT_3D ( 'NONE', #59781, #25194, #36102 ) ;
#24022 = EDGE_CURVE ( 'NONE', #54357, #62567, #31136, .T. ) ;
#24023 = LINE ( 'NONE', #1494, #14027 ) ;
#24024 = ORIENTED_EDGE ( 'NONE', *, *, #64536, .F. ) ;
#24025 = CARTESIAN_POINT ( 'NONE',  ( 0.000000000000000000, 75.11725578898467859, 2.956366410620910656 ) ) ;
#24026 = CARTESIAN_POINT ( 'NONE',  ( -30.50000000000000000, -120.0000000000000000, 2.500000000000000000 ) ) ;
#24027 = AXIS2_PLACEMENT_3D ( 'NONE', #61935, #27327, #304 ) ;
#24028 = CARTESIAN_POINT ( 'NONE',  ( 92.34999999999999432, 90.00000000000002842, 77.29999999999999716 ) ) ;
#24029 = EDGE_CURVE ( 'NONE', #9630, #30413, #49173, .T. ) ;
#24030 = DIRECTION ( 'NONE',  ( -3.061616997868382648E-16, -1.000000000000000000, -5.966227995846078450E-16 ) ) ;
#24031 = AXIS2_PLACEMENT_3D ( 'NONE', #61556, #4802, #5166 ) ;
#24032 = CIRCLE ( 'NONE', #6015, 37.49900000000000233 ) ;
#24033 = VECTOR ( 'NONE', #64402, 1000.000000000000000 ) ;
#24034 = CARTESIAN_POINT ( 'NONE',  ( 92.69370383062501162, -209.9999999999999716, 80.91156250086716284 ) ) ;
#24035 = VERTEX_POINT ( 'NONE', #43189 ) ;
#24036 = AXIS2_PLACEMENT_3D ( 'NONE', #53814, #2359, #71090 ) ;
#24037 = ORIENTED_EDGE ( 'NONE', *, *, #18849, .F. ) ;
#24038 = VECTOR ( 'NONE', #49707, 1000.000000000000000 ) ;
#24039 = SURFACE_STYLE_USAGE ( .BOTH. , #22179 ) ;
#24040 = ORIENTED_EDGE ( 'NONE', *, *, #60381, .F. ) ;
#24041 = EDGE_CURVE ( 'NONE', #105, #54047, #48073, .T. ) ;
#24042 = CARTESIAN_POINT ( 'NONE',  ( 20.10151712711562766, -102.7321394148470830, 2.500000000000000000 ) ) ;
#24043 = CARTESIAN_POINT ( 'NONE',  ( 96.15314808468750130, -211.9973110713294489, 76.51947916753380241 ) ) ;
#24045 = VERTEX_POINT ( 'NONE', #19850 ) ;
#24044 = EDGE_CURVE ( 'NONE', #40343, #26594, #8819, .T. ) ;
#24046 = CARTESIAN_POINT ( 'NONE',  ( 93.84685191531251292, -211.9973110713294489, 81.01739583420049939 ) ) ;
#24047 = ORIENTED_EDGE ( 'NONE', *, *, #11353, .F. ) ;
#24048 = DIRECTION ( 'NONE',  ( -0.9918136447140101231, 0.1276937514489694114, 0.000000000000000000 ) ) ;
#24049 = VERTEX_POINT ( 'NONE', #2976 ) ;
#24050 = AXIS2_PLACEMENT_3D ( 'NONE', #35647, #30742, #58973 ) ;
#24051 = ADVANCED_FACE ( 'NONE', ( #48434 ), #60834, .T. ) ;
#24052 = ORIENTED_EDGE ( 'NONE', *, *, #15712, .F. ) ;
#24053 = CYLINDRICAL_SURFACE ( 'NONE', #56151, 31.99999999999999289 ) ;
#24054 = SURFACE_STYLE_FILL_AREA ( #1525 ) ;
#24055 = DIRECTION ( 'NONE',  ( 0.000000000000000000, 0.000000000000000000, 1.000000000000000000 ) ) ;
#24056 = ORIENTED_EDGE ( 'NONE', *, *, #33586, .F. ) ;
#24057 = FACE_OUTER_BOUND ( 'NONE', #17635, .T. ) ;
#24058 = CARTESIAN_POINT ( 'NONE',  ( 96.32499999999998863, -207.7050326799711968, 85.42270833506762528 ) ) ;
#24059 = CARTESIAN_POINT ( 'NONE',  ( 92.34999999999999432, 88.47002178664753558, 87.51291666666666913 ) ) ;
#24060 = VERTEX_POINT ( 'NONE', #48800 ) ;
#24061 = CARTESIAN_POINT ( 'NONE',  ( 0.000000000000000000, 70.53064760720316428, -26.01480285779861035 ) ) ;
#24062 = EDGE_CURVE ( 'NONE', #42442, #21857, #50819, .T. ) ;
#24063 = LINE ( 'NONE', #13126, #39343 ) ;
#24064 = ORIENTED_EDGE ( 'NONE', *, *, #6461, .F. ) ;
#24065 = ORIENTED_EDGE ( 'NONE', *, *, #61283, .T. ) ;
#24066 = DIRECTION ( 'NONE',  ( -1.000000000000000000, 0.000000000000000000, 0.000000000000000000 ) ) ;
#24067 = EDGE_LOOP ( 'NONE', ( #24441, #13023, #24540, #20713 ) ) ;
#24068 = CARTESIAN_POINT ( 'NONE',  ( 92.34999999999999432, 91.52997821335252127, 86.85145833506763324 ) ) ;
#24069 = EDGE_CURVE ( 'NONE', #50948, #6766, #56802, .T. ) ;
#24070 = VECTOR ( 'NONE', #49513, 1000.000000000000000 ) ;
#24071 = ORIENTED_EDGE ( 'NONE', *, *, #47204, .T. ) ;
#24072 = SURFACE_STYLE_USAGE ( .BOTH. , #29308 ) ;
#24073 = VERTEX_POINT ( 'NONE', #20969 ) ;
#24074 = FACE_OUTER_BOUND ( 'NONE', #3535, .T. ) ;
#24075 = DIRECTION ( 'NONE',  ( -1.000000000000000000, 0.000000000000000000, 0.000000000000000000 ) ) ;
#24076 = ORIENTED_EDGE ( 'NONE', *, *, #64799, .T. ) ;
#24077 = ORIENTED_EDGE ( 'NONE', *, *, #34957, .T. ) ;
#24078 = CONICAL_SURFACE ( 'NONE', #13097, 17.30399999999999849, 0.2094395102393129815 ) ;
#24079 = ORIENTED_EDGE ( 'NONE', *, *, #10538, .T. ) ;
#24080 = DIRECTION ( 'NONE',  ( 0.000000000000000000, 0.000000000000000000, 1.000000000000000000 ) ) ;
#24081 = CARTESIAN_POINT ( 'NONE',  ( 6.377742925735834234, -145.7647898336708181, 5.500000000000000000 ) ) ;
#24082 = CARTESIAN_POINT ( 'NONE',  ( -97.65000000000001990, 90.00000000000004263, 88.09499999999999886 ) ) ;
#24083 = VERTEX_POINT ( 'NONE', #43920 ) ;
#24084 = CARTESIAN_POINT ( 'NONE',  ( -92.35000000000003695, 90.00000000000004263, 90.00000000000000000 ) ) ;
#24085 = DIRECTION ( 'NONE',  ( -1.000000000000000000, -0.000000000000000000, 0.000000000000000000 ) ) ;
#24086 = ORIENTED_EDGE ( 'NONE', *, *, #48207, .T. ) ;
#24087 = CARTESIAN_POINT ( 'NONE',  ( 92.35000000000005116, 91.52997821335254969, 75.34208333333333485 ) ) ;
#24088 = CARTESIAN_POINT ( 'NONE',  ( -97.30629616937497417, -211.3315407142195852, 83.98072916753380923 ) ) ;
#24089 = EDGE_LOOP ( 'NONE', ( #14428, #23312, #32716, #20543 ) ) ;
#24090 = CARTESIAN_POINT ( 'NONE',  ( -93.09170270117147084, 88.16127723153178408, 74.99954709728267233 ) ) ;
#24091 = DIRECTION ( 'NONE',  ( 0.000000000000000000, 0.000000000000000000, -1.000000000000000000 ) ) ;
#24092 = CARTESIAN_POINT ( 'NONE',  ( 10.00000000000000000, 0.000000000000000000, 0.000000000000000000 ) ) ;
#24093 = CARTESIAN_POINT ( 'NONE',  ( -96.15314808468747287, -208.0026889286704943, 76.20197916753380696 ) ) ;
#24094 = DIRECTION ( 'NONE',  ( 0.000000000000000000, 0.000000000000000000, -1.000000000000000000 ) ) ;
#24095 = VECTOR ( 'NONE', #71386, 1000.000000000000000 ) ;
#24096 = SURFACE_SIDE_STYLE ('',( #59780 ) ) ;
#24097 = CARTESIAN_POINT ( 'NONE',  ( 2.500000000000029754, 73.00000000000001421, -251.7000000000000455 ) ) ;
#24098 = CIRCLE ( 'NONE', #56507, 31.99999999999998579 ) ;
#24099 = CARTESIAN_POINT ( 'NONE',  ( 92.35000000003290666, -209.9999916046337205, 84.99910573348564924 ) ) ;
#24100 = CARTESIAN_POINT ( 'NONE',  ( -12.50000000000000000, -107.5000000000000000, -2.500000000000000000 ) ) ;
#24101 = CARTESIAN_POINT ( 'NONE',  ( -95.00000000000002842, 92.66308142843932671, 78.05406250086714692 ) ) ;
#24102 = FACE_OUTER_BOUND ( 'NONE', #42524, .T. ) ;
#24103 = CARTESIAN_POINT ( 'NONE',  ( -97.65000000000001990, 90.00000000000004263, 76.03000000000000114 ) ) ;
#24104 = ORIENTED_EDGE ( 'NONE', *, *, #42778, .F. ) ;
#24105 = DIRECTION ( 'NONE',  ( 0.000000000000000000, -0.7071067811865536790, 0.7071067811865414665 ) ) ;
#24106 = B_SPLINE_CURVE_WITH_KNOTS ( 'NONE', 1,
 ( #16954, #39891 ),
 .UNSPECIFIED., .F., .F.,
 ( 2, 2 ),
 ( 0.000000000000000000, 1.000000000000000000 ),
 .UNSPECIFIED. ) ;
#24107 = EDGE_CURVE ( 'NONE', #50232, #13102, #55559, .T. ) ;
#24108 = DIRECTION ( 'NONE',  ( -1.000000000000000000, 0.000000000000000000, 0.000000000000000000 ) ) ;
#24109 = CYLINDRICAL_SURFACE ( 'NONE', #26219, 37.49900000000000233 ) ;
#24110 = DIRECTION ( 'NONE',  ( 1.000000000000000000, 0.000000000000000000, 0.000000000000000000 ) ) ;
#24111 = EDGE_CURVE ( 'NONE', #46803, #43453, #56309, .T. ) ;
#24112 = CARTESIAN_POINT ( 'NONE',  ( 96.32499999999998863, -212.2949673200287179, 75.05104166840095559 ) ) ;
#24113 = CARTESIAN_POINT ( 'NONE',  ( -95.00000000000002842, 93.05995642670504253, 87.38062500173430180 ) ) ;
#24114 = CARTESIAN_POINT ( 'NONE',  ( -92.69370383062498320, -211.3315407142195852, 75.46114583420049371 ) ) ;
#24115 = ADVANCED_FACE ( 'NONE', ( #10062 ), #45410, .T. ) ;
#24116 = EDGE_CURVE ( 'NONE', #62043, #18290, #63307, .T. ) ;
#24117 = CYLINDRICAL_SURFACE ( 'NONE', #5685, 2.649999999999999467 ) ;
#24118 = VERTEX_POINT ( 'NONE', #21713 ) ;
#24119 = CARTESIAN_POINT ( 'NONE',  ( -42.50000000000000000, 0.000000000000000000, 0.000000000000000000 ) ) ;
#24120 = CARTESIAN_POINT ( 'NONE',  ( 0.000000000000000000, 0.6853352020795618893, -37.58145647212453611 ) ) ;
#24121 = CYLINDRICAL_SURFACE ( 'NONE', #68984, 2.650000000000540812 ) ;
#24122 = AXIS2_PLACEMENT_3D ( 'NONE', #17527, #57022, #40458 ) ;
#24123 = CIRCLE ( 'NONE', #51754, 16.00000000000000000 ) ;
#24124 = EDGE_CURVE ( 'NONE', #29107, #57325, #56686, .T. ) ;
#24125 = CYLINDRICAL_SURFACE ( 'NONE', #57137, 16.00000000000000000 ) ;
#24126 = ADVANCED_FACE ( 'NONE', ( #10814 ), #68334, .F. ) ;
#24127 = VERTEX_POINT ( 'NONE', #51031 ) ;
#24128 = DIRECTION ( 'NONE',  ( 1.000000000000000000, 0.000000000000000000, 0.000000000000000000 ) ) ;
#24129 = PRESENTATION_STYLE_ASSIGNMENT (( #1598 ) ) ;
#24130 = VERTEX_POINT ( 'NONE', #33352 ) ;
#24131 = CARTESIAN_POINT ( 'NONE',  ( 97.30629616937498838, -209.9999999999999716, 86.15031250086714465 ) ) ;
#24132 = CARTESIAN_POINT ( 'NONE',  ( 22.75000000000000000, 2.516649172247811061E-16, -2.055000000000000160 ) ) ;
#24133 = ORIENTED_EDGE ( 'NONE', *, *, #67756, .T. ) ;
#24134 = CARTESIAN_POINT ( 'NONE',  ( 92.69370383062501162, -211.3315407142195852, 89.21947916753381946 ) ) ;
#24135 = COLOUR_RGB ( '', 0.09019608, 0.27058824, 0.51372549) ;
#24136 = EDGE_LOOP ( 'NONE', ( #55271, #52681, #67349, #34059 ) ) ;
#24137 = FACE_OUTER_BOUND ( 'NONE', #25414, .T. ) ;
#24138 = EDGE_LOOP ( 'NONE', ( #18244, #17659, #37355, #54020 ) ) ;
#24139 = VECTOR ( 'NONE', #5137, 1000.000000000000227 ) ;
#24140 = EDGE_CURVE ( 'NONE', #10445, #21534, #16828, .T. ) ;
#24141 = EDGE_CURVE ( 'NONE', #31995, #40041, #16078, .T. ) ;
#24142 = CARTESIAN_POINT ( 'NONE',  ( -93.84685191531252713, 88.00268892867056536, 79.85322916753381151 ) ) ;
#24143 = VECTOR ( 'NONE', #6417, 1000.000000000000000 ) ;
#24144 = EDGE_LOOP ( 'NONE', ( #1555, #41415, #22511, #17213 ) ) ;
#24145 = ORIENTED_EDGE ( 'NONE', *, *, #72482, .F. ) ;
#24146 = PLANE ( 'NONE',  #71218 ) ;
#24147 = ORIENTED_EDGE ( 'NONE', *, *, #46130, .F. ) ;
#24148 = CARTESIAN_POINT ( 'NONE',  ( 0.000000000000000000, 16.83928648764923253, 16.46020748918050458 ) ) ;
#24149 = DIRECTION ( 'NONE',  ( 0.000000000000000000, 0.000000000000000000, -1.000000000000000000 ) ) ;
#24150 = VERTEX_POINT ( 'NONE', #61578 ) ;
#24151 = CARTESIAN_POINT ( 'NONE',  ( -25.50183398199384754, -112.6408924756582053, -5.500000000000000000 ) ) ;
#24152 = VERTEX_POINT ( 'NONE', #73952 ) ;
#24153 = CARTESIAN_POINT ( 'NONE',  ( 92.35000000009274856, -209.9999861897330788, 80.55392363656960697 ) ) ;
#24154 = EDGE_LOOP ( 'NONE', ( #40388, #34027, #11273, #43927 ) ) ;
#24155 = ORIENTED_EDGE ( 'NONE', *, *, #60218, .F. ) ;
#24156 = ORIENTED_EDGE ( 'NONE', *, *, #21105, .T. ) ;
#24157 = CARTESIAN_POINT ( 'NONE',  ( 92.69370383062501162, -208.6684592857803011, 80.69989583420048973 ) ) ;
#24158 = APPLICATION_PROTOCOL_DEFINITION ( 'draft international standard', 'automotive_design', 1998, #921 ) ;
#24159 = FACE_OUTER_BOUND ( 'NONE', #58621, .T. ) ;
#24160 = CARTESIAN_POINT ( 'NONE',  ( 11.99999999999999822, -74.74816331893404708, -33.71516098798819172 ) ) ;
#24161 = CARTESIAN_POINT ( 'NONE',  ( 0.000000000000000000, 29.01471420065674423, -76.69515212745984911 ) ) ;
#24162 = CARTESIAN_POINT ( 'NONE',  ( 99.99999999999997158, -90.00000000000000000, -90.00000000000014211 ) ) ;
#24163 = DIRECTION ( 'NONE',  ( 0.000000000000000000, -0.9723699203976741146, -0.2334453638559159938 ) ) ;
#24164 = CARTESIAN_POINT ( 'NONE',  ( -97.30629616937497417, -211.3315407142195852, 83.98072916753380923 ) ) ;
#24165 = CARTESIAN_POINT ( 'NONE',  ( -92.69370383062502583, 91.33154071421968467, 83.82197916753382572 ) ) ;
#24166 = ORIENTED_EDGE ( 'NONE', *, *, #39758, .T. ) ;
#24167 = CARTESIAN_POINT ( 'NONE',  ( 97.30629616937498838, 88.66845928578037217, 82.28739583420048120 ) ) ;
#24168 = ORIENTED_EDGE ( 'NONE', *, *, #67013, .F. ) ;
#24169 = CARTESIAN_POINT ( 'NONE',  ( -97.65000000000001990, 90.00000000000004263, 78.64937500173429896 ) ) ;
#24170 = LINE ( 'NONE', #70371, #1200 ) ;
#24171 = DIRECTION ( 'NONE',  ( 0.000000000000000000, -6.982962677686267499E-15, 1.000000000000000000 ) ) ;
#24172 = CARTESIAN_POINT ( 'NONE',  ( 5.000000000000000000, 2.543863470248396208, 81.96053171279903893 ) ) ;
#24173 = CARTESIAN_POINT ( 'NONE',  ( -97.30629616937497417, -211.3315407142195852, 87.15572916753380639 ) ) ;
#24174 = CARTESIAN_POINT ( 'NONE',  ( 15.00000000000000000, -1.278221433540145391, 26.51162292216073979 ) ) ;
#24175 = STYLED_ITEM ( 'NONE', ( #18180 ), #58845 ) ;
#24176 = AXIS2_PLACEMENT_3D ( 'NONE', #42296, #7696, #8447 ) ;
#24177 = CARTESIAN_POINT ( 'NONE',  ( -95.00000000000002842, 90.00000000000004263, 90.00000000000000000 ) ) ;
#24178 = CARTESIAN_POINT ( 'NONE',  ( -97.65000000000001990, 90.00000000000004263, 87.45999999999999375 ) ) ;
#24179 = AXIS2_PLACEMENT_3D ( 'NONE', #23630, #39447, #63868 ) ;
#24180 = LINE ( 'NONE', #47834, #19075 ) ;
#24181 = ORIENTED_EDGE ( 'NONE', *, *, #49690, .F. ) ;
#24182 = VECTOR ( 'NONE', #61724, 1000.000000000000000 ) ;
#24183 = ORIENTED_EDGE ( 'NONE', *, *, #23762, .F. ) ;
#24184 = CARTESIAN_POINT ( 'NONE',  ( -92.35000000000003695, 90.00000000000004263, 79.52249999999999375 ) ) ;
#24185 = DIRECTION ( 'NONE',  ( 0.000000000000000000, 0.000000000000000000, -1.000000000000000000 ) ) ;
#24186 = CARTESIAN_POINT ( 'NONE',  ( -93.84685191531252713, 88.00268892867056536, 88.58447916753381435 ) ) ;
#24187 = DIRECTION ( 'NONE',  ( -1.000000000000000000, 0.000000000000000000, 0.000000000000000000 ) ) ;
#24188 = CARTESIAN_POINT ( 'NONE',  ( 92.34999999999993747, 91.52997821335250705, 76.61208333333333087 ) ) ;
#24189 = DIRECTION ( 'NONE',  ( 1.000000000000000000, 1.427937372958405461E-15, 7.962523111839130290E-16 ) ) ;
#24190 = CARTESIAN_POINT ( 'NONE',  ( -92.34999999999999432, -209.9999999999999716, 78.25249999999999773 ) ) ;
#24191 = VERTEX_POINT ( 'NONE', #22092 ) ;
#24192 = CARTESIAN_POINT ( 'NONE',  ( 11.99999999999999822, 0.000000000000000000, 0.000000000000000000 ) ) ;
#24193 = SPHERICAL_SURFACE ( 'NONE', #11509, 5.315148208181397216 ) ;
#24194 = ADVANCED_FACE ( 'NONE', ( #26974 ), #61207, .T. ) ;
#24195 = VECTOR ( 'NONE', #10294, 1000.000000000000114 ) ;
#24196 = CARTESIAN_POINT ( 'NONE',  ( 10.00000000000000000, -73.73191006444582740, 14.66109333815435889 ) ) ;
#24197 = AXIS2_PLACEMENT_3D ( 'NONE', #183, #11045, #51630 ) ;
#24198 = LINE ( 'NONE', #7273, #10632 ) ;
#24199 = EDGE_CURVE ( 'NONE', #42171, #61202, #22467, .T. ) ;
#24200 = DIRECTION ( 'NONE',  ( -1.000000000000000000, 0.000000000000000000, 0.000000000000000000 ) ) ;
#24201 = DIRECTION ( 'NONE',  ( 0.000000000000000000, 0.4539904997395479702, -0.8910065241883673437 ) ) ;
#24202 = CARTESIAN_POINT ( 'NONE',  ( -97.30629616937495996, -209.9999999999999716, 85.99156250086716113 ) ) ;
#24203 = AXIS2_PLACEMENT_3D ( 'NONE', #35563, #70878, #64150 ) ;
#24204 = ADVANCED_FACE ( 'NONE', ( #62713 ), #61949, .F. ) ;
#24205 = DIRECTION ( 'NONE',  ( -1.000000000000000000, 0.000000000000000000, -0.000000000000000000 ) ) ;
#24206 =( BOUNDED_CURVE ( )  B_SPLINE_CURVE ( 2, ( #6136, #6853, #51608, #519, #34312, #11379, #51231, #45624, #23413 ),
 .UNSPECIFIED., .F., .F. ) 
 B_SPLINE_CURVE_WITH_KNOTS ( ( 3, 2, 2, 2, 3 ),
 ( 0.5291824299534890752, 0.5362381811096936790, 0.5432939466506105930, 0.5503497121915276180, 0.5503499107253647660 ),
 .UNSPECIFIED. ) 
 CURVE ( )  GEOMETRIC_REPRESENTATION_ITEM ( )  RATIONAL_B_SPLINE_CURVE ( ( 1.000000000000000000, 0.8660254037844387076, 1.000000000000000000, 0.8660254037844387076, 1.000000000000000000, 0.8660254037844387076, 1.000000000000000000, 0.9999962302473756059, 0.9999924607068964022 ) ) 
 REPRESENTATION_ITEM ( '' )  );
#24207 = CIRCLE ( 'NONE', #1430, 12.49999999999999645 ) ;
#24208 = EDGE_CURVE ( 'NONE', #27575, #38312, #71252, .T. ) ;
#24209 = DIRECTION ( 'NONE',  ( -1.000000000000000000, -0.000000000000000000, -0.000000000000000000 ) ) ;
#24210 = CARTESIAN_POINT ( 'NONE',  ( -97.30629616937497417, -208.6684592857803295, 75.14364583420049826 ) ) ;
#24211 = CARTESIAN_POINT ( 'NONE',  ( 5.000000000000002665, 22.90783923731741112, -78.73519480814930205 ) ) ;
#24212 = ORIENTED_EDGE ( 'NONE', *, *, #55359, .T. ) ;
#24213 = DIRECTION ( 'NONE',  ( -1.000000000000000000, 0.000000000000000000, 0.000000000000000000 ) ) ;
#24214 = FACE_OUTER_BOUND ( 'NONE', #63098, .T. ) ;
#24215 = DIRECTION ( 'NONE',  ( 0.000000000000000000, 0.000000000000000000, -1.000000000000000000 ) ) ;
#24216 = CARTESIAN_POINT ( 'NONE',  ( -93.84685191531252713, 88.00268892867056536, 75.40822916753381833 ) ) ;
#24218 = ADVANCED_FACE ( 'NONE', ( #4446 ), #66841, .F. ) ;
#24217 = CARTESIAN_POINT ( 'NONE',  ( 97.30629616937498838, -209.9999999999999716, 77.26031250086714408 ) ) ;
#24219 = VERTEX_POINT ( 'NONE', #50276 ) ;
#24220 = ADVANCED_FACE ( 'NONE', ( #67584 ), #53254, .F. ) ;
#24221 = CYLINDRICAL_SURFACE ( 'NONE', #71512, 16.00000000000000000 ) ;
#24222 = ORIENTED_EDGE ( 'NONE', *, *, #25117, .T. ) ;
#24223 = LINE ( 'NONE', #58056, #26719 ) ;
#24224 = VERTEX_POINT ( 'NONE', #58153 ) ;
#24225 = CIRCLE ( 'NONE', #72175, 82.00000000000000000 ) ;
#24226 = CARTESIAN_POINT ( 'NONE',  ( -92.35003071823130938, 91.52999594853163501, 79.01979289519825045 ) ) ;
#24227 = ADVANCED_FACE ( 'NONE', ( #70154 ), #1431, .T. ) ;
#24228 = EDGE_CURVE ( 'NONE', #29135, #2794, #29238, .T. ) ;
#24229 = VECTOR ( 'NONE', #13541, 1000.000000000000000 ) ;
#24230 = VERTEX_POINT ( 'NONE', #69795 ) ;
#24231 = ORIENTED_EDGE ( 'NONE', *, *, #36343, .T. ) ;
#24232 = VERTEX_POINT ( 'NONE', #6652 ) ;
#24233 = DIRECTION ( 'NONE',  ( 0.000000000000000000, -0.2334453638559126909, 0.9723699203976748917 ) ) ;
#24234 = AXIS2_PLACEMENT_3D ( 'NONE', #266, #17870, #41543 ) ;
#24235 = ORIENTED_EDGE ( 'NONE', *, *, #68418, .F. ) ;
#24236 = VERTEX_POINT ( 'NONE', #57793 ) ;
#24237 = CARTESIAN_POINT ( 'NONE',  ( 97.30629616937498838, 91.33154071421968467, 79.37697916753381833 ) ) ;
#24238 = CARTESIAN_POINT ( 'NONE',  ( -93.67500000000003979, 87.70503267997129626, 81.40104166840096411 ) ) ;
#24239 = CARTESIAN_POINT ( 'NONE',  ( 97.64999999999997726, -208.4700217866474645, 75.13041666666666174 ) ) ;
#24240 = ORIENTED_EDGE ( 'NONE', *, *, #63413, .F. ) ;
#24241 = VERTEX_POINT ( 'NONE', #68710 ) ;
#24242 = ORIENTED_EDGE ( 'NONE', *, *, #956, .T. ) ;
#24243 = DIRECTION ( 'NONE',  ( -1.000000000000000000, 0.000000000000000000, 0.000000000000000000 ) ) ;
#24244 = EDGE_LOOP ( 'NONE', ( #39133, #52167, #53836, #19077 ) ) ;
#24245 = AXIS2_PLACEMENT_3D ( 'NONE', #17578, #28479, #22871 ) ;
#24246 = SURFACE_STYLE_FILL_AREA ( #41897 ) ;
#24247 = CARTESIAN_POINT ( 'NONE',  ( -93.67499999999998295, -207.7050326799711968, 75.26270833506764291 ) ) ;
#24248 = CARTESIAN_POINT ( 'NONE',  ( 0.000000000000000000, -2.543863470248951320, 81.96053171279901051 ) ) ;
#24249 = DIRECTION ( 'NONE',  ( -1.000000000000000000, 0.000000000000000000, 0.000000000000000000 ) ) ;
#24250 = DIRECTION ( 'NONE',  ( 1.000000000000000000, 0.000000000000000000, 0.000000000000000000 ) ) ;
#24251 = DIRECTION ( 'NONE',  ( 0.000000000000000000, 0.000000000000000000, 1.000000000000000000 ) ) ;
#24252 = DIRECTION ( 'NONE',  ( -1.000000000000000000, 0.000000000000000000, -0.000000000000000000 ) ) ;
#24253 = CARTESIAN_POINT ( 'NONE',  ( -97.64999999999994884, -211.5299782133524502, 79.33729166840096525 ) ) ;
#24254 = ORIENTED_EDGE ( 'NONE', *, *, #12629, .T. ) ;
#24255 = CARTESIAN_POINT ( 'NONE',  ( 0.000000000000000000, 71.91182617369187824, 28.89263327155770256 ) ) ;
#24256 = ORIENTED_EDGE ( 'NONE', *, *, #58943, .F. ) ;
#24258 = CARTESIAN_POINT ( 'NONE',  ( -92.35000000000005116, 88.47002178664754979, 75.73895833506765030 ) ) ;
#24257 = CARTESIAN_POINT ( 'NONE',  ( 94.99999999999998579, 93.05995642670504253, 79.76062500173429726 ) ) ;
#24259 = EDGE_LOOP ( 'NONE', ( #73975, #54793 ) ) ;
#24260 = CARTESIAN_POINT ( 'NONE',  ( 96.15314808468748708, 91.99731107132950569, 79.42989583420049371 ) ) ;
#24261 = CARTESIAN_POINT ( 'NONE',  ( -0.0004442498525516064278, 0.001194404164626844313, -80.00000000000000000 ) ) ;
#24262 = DIRECTION ( 'NONE',  ( -0.000000000000000000, -0.000000000000000000, 1.000000000000000000 ) ) ;
#24263 = DIRECTION ( 'NONE',  ( 1.000000000000000000, -0.000000000000000000, -0.000000000000000000 ) ) ;
#24264 = DIRECTION ( 'NONE',  ( 0.000000000000000000, 0.000000000000000000, 1.000000000000000000 ) ) ;
#24265 = VERTEX_POINT ( 'NONE', #17195 ) ;
#24266 = DIRECTION ( 'NONE',  ( -1.000000000000000000, 0.000000000000000000, 0.000000000000000000 ) ) ;
#24267 = DIRECTION ( 'NONE',  ( 1.000000000000000000, 0.000000000000000000, 0.000000000000000000 ) ) ;
#24268 = VERTEX_POINT ( 'NONE', #682 ) ;
#24269 = EDGE_LOOP ( 'NONE', ( #48986, #9258, #21612, #56889 ) ) ;
#24270 = EDGE_CURVE ( 'NONE', #66690, #35348, #62876, .T. ) ;
#24271 = EDGE_CURVE ( 'NONE', #47528, #40220, #54795, .T. ) ;
#24272 = DIRECTION ( 'NONE',  ( -1.000000000000000000, 0.000000000000000000, 0.000000000000000000 ) ) ;
#24273 = EDGE_CURVE ( 'NONE', #15802, #45606, #23568, .T. ) ;
#24274 = CARTESIAN_POINT ( 'NONE',  ( -5.000000000000000000, -2.886751345948134428, -2.080000000000000071 ) ) ;
#24275 = LINE ( 'NONE', #35176, #61774 ) ;
#24276 = CARTESIAN_POINT ( 'NONE',  ( -97.30629616937495996, -209.9999999999999716, 77.73656250086715147 ) ) ;
#24277 = EDGE_LOOP ( 'NONE', ( #37302, #70006, #61988, #13746 ) ) ;
#24278 = ADVANCED_FACE ( 'NONE', ( #41596 ), #40491, .T. ) ;
#24279 = VECTOR ( 'NONE', #49581, 1000.000000000000000 ) ;
#24280 = LINE ( 'NONE', #63397, #6688 ) ;
#24281 = CARTESIAN_POINT ( 'NONE',  ( 10.00000000000000000, -69.42325613327466272, 34.44570377933573724 ) ) ;
#24282 = VECTOR ( 'NONE', #22911, 1000.000000000000000 ) ;
#24283 = DIRECTION ( 'NONE',  ( -0.000000000000000000, -0.000000000000000000, 1.000000000000000000 ) ) ;
#24284 = EDGE_CURVE ( 'NONE', #68149, #3543, #64538, .T. ) ;
#24285 = DIRECTION ( 'NONE',  ( -0.000000000000000000, -0.000000000000000000, 1.000000000000000000 ) ) ;
#24286 = DIRECTION ( 'NONE',  ( 0.000000000000000000, 0.000000000000000000, 1.000000000000000000 ) ) ;
#24287 = DIRECTION ( 'NONE',  ( -1.000000000000000000, 0.000000000000000000, 0.000000000000000000 ) ) ;
#24288 = LINE ( 'NONE', #41947, #56545 ) ;
#24289 = CARTESIAN_POINT ( 'NONE',  ( -92.35000000000006537, -209.9999992849074317, 85.31687502647974952 ) ) ;
#24290 = CYLINDRICAL_SURFACE ( 'NONE', #38856, 31.99999999999998579 ) ;
#24291 = CARTESIAN_POINT ( 'NONE',  ( 0.000000000000000000, 74.65491531819118620, -8.830959090342659579 ) ) ;
#24292 = VECTOR ( 'NONE', #56726, 1000.000000000000000 ) ;
#24293 = ADVANCED_FACE ( 'NONE', ( #52498 ), #1055, .T. ) ;
#24294 = CARTESIAN_POINT ( 'NONE',  ( 92.69370383062498320, 91.33154071421968467, 85.93864583420051417 ) ) ;
#24295 = CARTESIAN_POINT ( 'NONE',  ( -92.69370383062498320, -211.3315407142195852, 86.89114583420048632 ) ) ;
#24296 = CARTESIAN_POINT ( 'NONE',  ( 93.67500000000001137, -212.2949673200287179, 83.83520833506763381 ) ) ;
#24297 = ORIENTED_EDGE ( 'NONE', *, *, #44165, .F. ) ;
#24298 = CARTESIAN_POINT ( 'NONE',  ( 10.00000000000000000, -35.92658777277517856, 10.74501242461269257 ) ) ;
#24299 = CARTESIAN_POINT ( 'NONE',  ( -93.67499999999998295, -212.2949673200287179, 80.05166666666666231 ) ) ;
#24300 = CARTESIAN_POINT ( 'NONE',  ( -93.84685191531254134, 91.99731107132950569, 75.46114583420047950 ) ) ;
#24301 = AXIS2_PLACEMENT_3D ( 'NONE', #52887, #1432, #28841 ) ;
#24302 = AXIS2_PLACEMENT_3D ( 'NONE', #73886, #22020, #10744 ) ;
#24304 = EDGE_CURVE ( 'NONE', #52685, #9960, #23945, .T. ) ;
#24303 = CARTESIAN_POINT ( 'NONE',  ( 97.30629616937498838, -208.6684592857803011, 85.56822916753380071 ) ) ;
#24305 = ORIENTED_EDGE ( 'NONE', *, *, #62118, .F. ) ;
#24306 = EDGE_CURVE ( 'NONE', #28882, #4362, #70034, .T. ) ;
#24307 = EDGE_LOOP ( 'NONE', ( #43380, #66789, #50375, #2546 ) ) ;
#24308 = ORIENTED_EDGE ( 'NONE', *, *, #8517, .T. ) ;
#24309 = FACE_OUTER_BOUND ( 'NONE', #38170, .T. ) ;
#24310 = DIRECTION ( 'NONE',  ( -0.9227826878668545785, -0.3853207896976533209, 0.000000000000000000 ) ) ;
#24311 = ORIENTED_EDGE ( 'NONE', *, *, #43906, .F. ) ;
#24312 = ORIENTED_EDGE ( 'NONE', *, *, #29177, .T. ) ;
#24313 = CARTESIAN_POINT ( 'NONE',  ( 96.15314808468748708, -208.0026889286704943, 81.96989583420048575 ) ) ;
#24314 = CARTESIAN_POINT ( 'NONE',  ( 94.99999999999998579, 93.05995642670504253, 89.84125000000000227 ) ) ;
#24315 = CARTESIAN_POINT ( 'NONE',  ( 10.00000000000000000, 28.89263327155850902, -71.91182617369157981 ) ) ;
#24316 = CARTESIAN_POINT ( 'NONE',  ( 5.000000000000000000, 2.488344183252611419, -1.689918788536298289 ) ) ;
#24317 = DIRECTION ( 'NONE',  ( 0.000000000000000000, 0.000000000000000000, 1.000000000000000000 ) ) ;
#24318 = CARTESIAN_POINT ( 'NONE',  ( 10.00000000000000000, 17.67226234102874116, -33.17418723428288274 ) ) ;
#24319 = CARTESIAN_POINT ( 'NONE',  ( 96.32499999999998863, -207.7050326799711968, 85.97833333333332462 ) ) ;
#24320 = ORIENTED_EDGE ( 'NONE', *, *, #51631, .F. ) ;
#24321 = EDGE_LOOP ( 'NONE', ( #23863, #32508, #8878, #64545 ) ) ;
#24322 = ORIENTED_EDGE ( 'NONE', *, *, #60782, .F. ) ;
#24323 = ORIENTED_EDGE ( 'NONE', *, *, #35646, .F. ) ;
#24324 = LINE ( 'NONE', #57427, #37045 ) ;
#24325 = CIRCLE ( 'NONE', #18360, 37.49900000000000233 ) ;
#24326 = CARTESIAN_POINT ( 'NONE',  ( -97.30629616937501680, 91.33154071421968467, 88.47864583420047779 ) ) ;
#24327 = DIRECTION ( 'NONE',  ( -1.000000000000000000, 0.000000000000000000, 0.000000000000000000 ) ) ;
#24328 = CARTESIAN_POINT ( 'NONE',  ( 10.00000000000000000, -49.70050353004846500, -59.46389618802017907 ) ) ;
#24329 = CARTESIAN_POINT ( 'NONE',  ( 96.32499999999998863, -207.7050326799711968, 74.62770833506762358 ) ) ;
#24330 = CARTESIAN_POINT ( 'NONE',  ( 93.67499999999998295, 92.29496732002878900, 78.46416666666667084 ) ) ;
#24331 = EDGE_LOOP ( 'NONE', ( #37690, #26350, #39992, #2367 ) ) ;
#24332 = CARTESIAN_POINT ( 'NONE',  ( -97.64999999999994884, -208.4700217866474645, 89.39145833506763950 ) ) ;
#24333 = EDGE_CURVE ( 'NONE', #74276, #19944, #47987, .T. ) ;
#24334 = ORIENTED_EDGE ( 'NONE', *, *, #26060, .T. ) ;
#24335 = CARTESIAN_POINT ( 'NONE',  ( 15.00000000000000000, -1.278221433540507546, -26.51162292216071492 ) ) ;
#24336 = VERTEX_POINT ( 'NONE', #25787 ) ;
#24337 = CARTESIAN_POINT ( 'NONE',  ( -97.65000000000001990, 88.47002178664754979, 86.95729166840096980 ) ) ;
#24338 = AXIS2_PLACEMENT_3D ( 'NONE', #32980, #55927, #73575 ) ;
#24339 = CARTESIAN_POINT ( 'NONE',  ( 92.69370383062498320, 91.33154071421968467, 74.98489583420048632 ) ) ;
#24340 = VERTEX_POINT ( 'NONE', #71261 ) ;
#24341 = FACE_OUTER_BOUND ( 'NONE', #59560, .T. ) ;
#24342 = DIRECTION ( 'NONE',  ( -1.000000000000000000, 0.000000000000000000, 0.000000000000000000 ) ) ;
#24343 = CYLINDRICAL_SURFACE ( 'NONE', #2970, 16.00000000000000000 ) ;
#24344 = CARTESIAN_POINT ( 'NONE',  ( -95.00000000000002842, 90.00000000000004263, 90.00000000000000000 ) ) ;
#24345 = ORIENTED_EDGE ( 'NONE', *, *, #46673, .F. ) ;
#24346 = DIRECTION ( 'NONE',  ( -1.000000000000000000, -0.000000000000000000, -0.000000000000000000 ) ) ;
#24347 = AXIS2_PLACEMENT_3D ( 'NONE', #70660, #62574, #33976 ) ;
#24348 = CIRCLE ( 'NONE', #56769, 77.49899999999999523 ) ;
#24349 = CARTESIAN_POINT ( 'NONE',  ( -0.4301293587032979371, -118.5629931333561871, -2.500000000000000000 ) ) ;
#24350 = ORIENTED_EDGE ( 'NONE', *, *, #7280, .F. ) ;
#24351 = ORIENTED_EDGE ( 'NONE', *, *, #31196, .T. ) ;
#24352 = EDGE_CURVE ( 'NONE', #54048, #8287, #70080, .T. ) ;
#24353 = CARTESIAN_POINT ( 'NONE',  ( -10.00000000000000000, 0.000000000000000000, 0.000000000000000000 ) ) ;
#24354 = EDGE_CURVE ( 'NONE', #51153, #15251, #54475, .T. ) ;
#24355 = LINE ( 'NONE', #13436, #30012 ) ;
#24356 = DIRECTION ( 'NONE',  ( 1.000000000000000000, 0.000000000000000000, 0.000000000000000000 ) ) ;
#24357 = VERTEX_POINT ( 'NONE', #20135 ) ;
#24358 = CARTESIAN_POINT ( 'NONE',  ( -96.15314808468745866, -211.9973110713294489, 89.27239583420049485 ) ) ;
#24359 = ORIENTED_EDGE ( 'NONE', *, *, #25330, .F. ) ;
#24360 = CARTESIAN_POINT ( 'NONE',  ( 0.000000000000000000, 0.8660254037844389297, 1.500000000000000000 ) ) ;
#24361 = ORIENTED_EDGE ( 'NONE', *, *, #34472, .F. ) ;
#24362 = EDGE_CURVE ( 'NONE', #36877, #60490, #58079, .T. ) ;
#24363 = EDGE_CURVE ( 'NONE', #9807, #6402, #50326, .T. ) ;
#24364 = ORIENTED_EDGE ( 'NONE', *, *, #58896, .F. ) ;
#24365 = CARTESIAN_POINT ( 'NONE',  ( 10.00000000000000000, -33.80338159004273280, -16.23288003029533044 ) ) ;
#24366 = DIRECTION ( 'NONE',  ( 0.000000000000000000, -0.4999999999999998335, 0.8660254037844387076 ) ) ;
#24367 = CARTESIAN_POINT ( 'NONE',  ( 94.99999999999998579, 92.66308142843932671, 83.13406250086714522 ) ) ;
#24368 = CARTESIAN_POINT ( 'NONE',  ( -10.00000000000000000, 0.000000000000000000, 0.000000000000000000 ) ) ;
#24369 = CARTESIAN_POINT ( 'NONE',  ( 10.00000000000000000, 73.73191006444572793, -14.66109333815486515 ) ) ;
#24370 = CARTESIAN_POINT ( 'NONE',  ( 94.99999999999998579, 90.00000000000002842, 90.00000000000000000 ) ) ;
#24371 = CARTESIAN_POINT ( 'NONE',  ( 10.00000000000000000, 0.000000000000000000, 0.000000000000000000 ) ) ;
#24372 = DIRECTION ( 'NONE',  ( -1.000000000000000000, -0.000000000000000000, 0.000000000000000000 ) ) ;
#24373 = CARTESIAN_POINT ( 'NONE',  ( -10.00000000000000000, 0.000000000000000000, 0.000000000000000000 ) ) ;
#24374 = ADVANCED_FACE ( 'NONE', ( #30674 ), #19766, .T. ) ;
#24375 = CARTESIAN_POINT ( 'NONE',  ( -2.500000000000015543, -73.00000000000001421, -255.0000000000000000 ) ) ;
#24376 = AXIS2_PLACEMENT_3D ( 'NONE', #65208, #48647, #13682 ) ;
#24377 = LINE ( 'NONE', #41658, #62588 ) ;
#24378 = CARTESIAN_POINT ( 'NONE',  ( -92.69370383062504004, 90.00000000000004263, 86.78531250086714977 ) ) ;
#24379 = DIRECTION ( 'NONE',  ( 1.000000000000000000, 0.000000000000000000, 0.000000000000000000 ) ) ;
#24380 = CIRCLE ( 'NONE', #38812, 31.99999999999998579 ) ;
#24382 = ADVANCED_FACE ( 'NONE', ( #70517 ), #25048, .T. ) ;
#24381 = DIRECTION ( 'NONE',  ( -1.000000000000000000, 0.000000000000000000, 0.000000000000000000 ) ) ;
#24383 = ORIENTED_EDGE ( 'NONE', *, *, #73019, .F. ) ;
#24384 = CIRCLE ( 'NONE', #54434, 31.99999999999999289 ) ;
#24385 = CARTESIAN_POINT ( 'NONE',  ( 0.000000000000000000, 62.50884508063487033, -41.76106447765422303 ) ) ;
#24386 = EDGE_CURVE ( 'NONE', #47511, #73508, #42715, .T. ) ;
#24388 = CARTESIAN_POINT ( 'NONE',  ( 0.000000000000000000, 35.53030884539084866, 12.26510123303271982 ) ) ;
#24387 = AXIS2_PLACEMENT_3D ( 'NONE', #24924, #53504, #2038 ) ;
#24389 = FACE_OUTER_BOUND ( 'NONE', #9780, .T. ) ;
#24390 = LINE ( 'NONE', #13098, #41661 ) ;
#24391 = AXIS2_PLACEMENT_3D ( 'NONE', #60890, #15381, #31193 ) ;
#24392 = VECTOR ( 'NONE', #72520, 1000.000000000000114 ) ;
#24393 = CARTESIAN_POINT ( 'NONE',  ( 97.30629616937498838, -211.3315407142195852, 83.08114583420048405 ) ) ;
#24394 = EDGE_LOOP ( 'NONE', ( #22211, #6216, #61901, #31803 ) ) ;
#24395 = EDGE_LOOP ( 'NONE', ( #49523, #3085, #71543, #34339 ) ) ;
#24396 = ORIENTED_EDGE ( 'NONE', *, *, #71170, .T. ) ;
#24397 = LINE ( 'NONE', #35313, #67766 ) ;
#24398 = CARTESIAN_POINT ( 'NONE',  ( 6.000000000000000000, -3.894527615418457600, 81.90746397400387480 ) ) ;
#24399 = ORIENTED_EDGE ( 'NONE', *, *, #42515, .T. ) ;
#24400 = CARTESIAN_POINT ( 'NONE',  ( 96.15314808468750130, -211.9973110713294489, 79.21822916753382060 ) ) ;
#24401 = EDGE_LOOP ( 'NONE', ( #45036, #51770, #5667, #37065 ) ) ;
#24402 = LINE ( 'NONE', #47337, #68381 ) ;
#24403 = ORIENTED_EDGE ( 'NONE', *, *, #37301, .F. ) ;
#24404 = ORIENTED_EDGE ( 'NONE', *, *, #71596, .T. ) ;
#24405 = CARTESIAN_POINT ( 'NONE',  ( 93.67500000000001137, -207.7050326799711968, 86.79854166840097207 ) ) ;
#24406 = PLANE ( 'NONE',  #40112 ) ;
#24407 = EDGE_LOOP ( 'NONE', ( #63043, #58762, #51993, #50007 ) ) ;
#24408 = CARTESIAN_POINT ( 'NONE',  ( -93.67500000000003979, 92.29496732002878900, 84.07333333333333769 ) ) ;
#24409 = CARTESIAN_POINT ( 'NONE',  ( 93.67500000000001137, -212.2949673200287179, 83.20020833506764291 ) ) ;
#24410 = CARTESIAN_POINT ( 'NONE',  ( 96.32499999999998863, 87.70503267997126784, 89.57666666666666799 ) ) ;
#24411 = ORIENTED_EDGE ( 'NONE', *, *, #26585, .F. ) ;
#24412 = CARTESIAN_POINT ( 'NONE',  ( 13.83832728059186046, -142.6495187161941089, -2.500000000000000444 ) ) ;
#24413 = DIRECTION ( 'NONE',  ( 1.000000000000000000, 0.000000000000000000, 0.000000000000000000 ) ) ;
#24414 = ADVANCED_FACE ( 'NONE', ( #65286 ), #60021, .T. ) ;
#24415 = EDGE_LOOP ( 'NONE', ( #67017, #23307, #16179, #46125 ) ) ;
#24416 = ORIENTED_EDGE ( 'NONE', *, *, #27334, .T. ) ;
#24417 =( BOUNDED_CURVE ( )  B_SPLINE_CURVE ( 2, ( #62185, #33598, #27959, #17429, #24545, #40736, #51640 ),
 .UNSPECIFIED., .F., .F. ) 
 B_SPLINE_CURVE_WITH_KNOTS ( ( 3, 2, 2, 3 ),
 ( 0.6350190250571088324, 0.6420746642202955767, 0.6491304297611778518, 0.6561861948910822084 ),
 .UNSPECIFIED. ) 
 CURVE ( )  GEOMETRIC_REPRESENTATION_ITEM ( )  RATIONAL_B_SPLINE_CURVE ( ( 0.9999952007766184092, 0.8660278034391103441, 1.000000000000000000, 0.8660254037844387076, 1.000000000000000000, 0.8660254037844387076, 1.000000000000000000 ) ) 
 REPRESENTATION_ITEM ( '' )  );
#24418 = CARTESIAN_POINT ( 'NONE',  ( 4.999999999999999112, -0.1416384297035287454, -0.5080592402122392492 ) ) ;
#24419 = ORIENTED_EDGE ( 'NONE', *, *, #39161, .F. ) ;
#24420 = CARTESIAN_POINT ( 'NONE',  ( 94.99999999999998579, 86.94004357329500010, 87.69812500173429726 ) ) ;
#24421 = VERTEX_POINT ( 'NONE', #2892 ) ;
#24422 = ORIENTED_EDGE ( 'NONE', *, *, #38002, .T. ) ;
#24423 = DIRECTION ( 'NONE',  ( 0.000000000000000000, 0.000000000000000000, 1.000000000000000000 ) ) ;
#24424 = DIRECTION ( 'NONE',  ( -0.000000000000000000, -0.9945218953682741780, 0.1045284632676447834 ) ) ;
#24426 = ADVANCED_FACE ( 'NONE', ( #64913 ), #48716, .T. ) ;
#24425 = ORIENTED_EDGE ( 'NONE', *, *, #55067, .T. ) ;
#24427 = VECTOR ( 'NONE', #16451, 1000.000000000000000 ) ;
#24428 = ORIENTED_EDGE ( 'NONE', *, *, #74018, .T. ) ;
#24429 = VERTEX_POINT ( 'NONE', #19401 ) ;
#24430 = CARTESIAN_POINT ( 'NONE',  ( -96.32500000000001705, 92.29496732002878900, 86.08416666666666117 ) ) ;
#24431 = ADVANCED_FACE ( 'NONE', ( #66026 ), #60388, .T. ) ;
#24432 = DIRECTION ( 'NONE',  ( -0.000000000000000000, -0.000000000000000000, -1.000000000000000000 ) ) ;
#24433 = CARTESIAN_POINT ( 'NONE',  ( -97.65000000000001990, 88.47002178664754979, 87.51291666666666913 ) ) ;
#24434 = VERTEX_POINT ( 'NONE', #2160 ) ;
#24435 = DIRECTION ( 'NONE',  ( 0.000000000000000000, 0.1564344650402243742, 0.9876883405951387696 ) ) ;
#24436 = VECTOR ( 'NONE', #45133, 1000.000000000000000 ) ;
#24437 = DIRECTION ( 'NONE',  ( 0.000000000000000000, -0.1564344650402170744, -0.9876883405951398798 ) ) ;
#24438 = ORIENTED_EDGE ( 'NONE', *, *, #57368, .F. ) ;
#24439 = FACE_OUTER_BOUND ( 'NONE', #30389, .T. ) ;
#24440 = CARTESIAN_POINT ( 'NONE',  ( -93.84685191531248449, -208.0026889286704943, 84.35114583420048007 ) ) ;
#24441 = ORIENTED_EDGE ( 'NONE', *, *, #214, .F. ) ;
#24442 = AXIS2_PLACEMENT_3D ( 'NONE', #14658, #3776, #9022 ) ;
#24443 = DIRECTION ( 'NONE',  ( 0.000000000000000000, 0.000000000000000000, 1.000000000000000000 ) ) ;
#24444 = LINE ( 'NONE', #65779, #51265 ) ;
#24445 = DIRECTION ( 'NONE',  ( 0.000000000000000000, 0.000000000000000000, 1.000000000000000000 ) ) ;
#24446 = CARTESIAN_POINT ( 'NONE',  ( 10.00000000000000000, -76.66974797899844418, 11.30684508768314522 ) ) ;
#24447 = EDGE_CURVE ( 'NONE', #64948, #37629, #63731, .T. ) ;
#24448 = CYLINDRICAL_SURFACE ( 'NONE', #69218, 37.49900000000000233 ) ;
#24449 = AXIS2_PLACEMENT_3D ( 'NONE', #35550, #52467, #23180 ) ;
#24450 = AXIS2_PLACEMENT_3D ( 'NONE', #5532, #288, #73550 ) ;
#24451 = DIRECTION ( 'NONE',  ( -1.000000000000000000, -0.000000000000000000, -0.000000000000000000 ) ) ;
#24452 = DIRECTION ( 'NONE',  ( -1.000000000000000000, 0.000000000000000000, -0.000000000000000000 ) ) ;
#24453 = CARTESIAN_POINT ( 'NONE',  ( -10.00000000000000000, 0.000000000000000000, 0.000000000000000000 ) ) ;
#24454 = LINE ( 'NONE', #13537, #44746 ) ;
#24455 = CARTESIAN_POINT ( 'NONE',  ( 0.000000000000000000, -36.73666225445940370, 65.58780272294062286 ) ) ;
#24456 = CARTESIAN_POINT ( 'NONE',  ( -95.00000000000002842, 87.33691857156074434, 77.73656250086713726 ) ) ;
#24457 = DIRECTION ( 'NONE',  ( -0.000000000000000000, -0.5000000000000004441, 0.8660254037844383745 ) ) ;
#24458 = DIRECTION ( 'NONE',  ( 0.000000000000000000, 0.6494480483301793283, 0.7604059656000345946 ) ) ;
#24459 = EDGE_CURVE ( 'NONE', #12324, #31904, #22375, .T. ) ;
#24460 = EDGE_CURVE ( 'NONE', #32358, #59815, #16059, .T. ) ;
#24461 = DIRECTION ( 'NONE',  ( -1.000000000000000000, -0.000000000000000000, -0.000000000000000000 ) ) ;
#24462 = EDGE_CURVE ( 'NONE', #16859, #67669, #27640, .T. ) ;
#24463 = VECTOR ( 'NONE', #68367, 1000.000000000000000 ) ;
#24464 = EDGE_CURVE ( 'NONE', #30036, #72747, #62883, .T. ) ;
#24465 = CARTESIAN_POINT ( 'NONE',  ( -97.64997399466339800, -211.5299932275404728, 84.41729270697886989 ) ) ;
#24466 = DIRECTION ( 'NONE',  ( 0.000000000000000000, 0.000000000000000000, 1.000000000000000000 ) ) ;
#24467 = CYLINDRICAL_SURFACE ( 'NONE', #53897, 31.99999999999998579 ) ;
#24468 = CYLINDRICAL_SURFACE ( 'NONE', #11761, 31.99999999999999289 ) ;
#24469 = FACE_OUTER_BOUND ( 'NONE', #65006, .T. ) ;
#24470 = CARTESIAN_POINT ( 'NONE',  ( -94.53673242685059108, -212.8430781844921569, 74.72378867588408013 ) ) ;
#24471 = CARTESIAN_POINT ( 'NONE',  ( -95.00000000000002842, 90.00000000000004263, 90.00000000000000000 ) ) ;
#24472 = EDGE_CURVE ( 'NONE', #34276, #67063, #4059, .T. ) ;
#24473 = ORIENTED_EDGE ( 'NONE', *, *, #38044, .T. ) ;
#24474 = DIRECTION ( 'NONE',  ( 0.000000000000000000, -0.07845909572783058006, -0.9969173337331290741 ) ) ;
#24475 = CARTESIAN_POINT ( 'NONE',  ( -2.449999999999998845, 3.000384657911014384E-16, -0.3851141460153411078 ) ) ;
#24476 = CARTESIAN_POINT ( 'NONE',  ( 0.000000000000000000, 0.000000000000000000, 0.000000000000000000 ) ) ;
#24477 = CIRCLE ( 'NONE', #43705, 31.99999999999999289 ) ;
#24478 = DIRECTION ( 'NONE',  ( -1.000000000000000000, -0.000000000000000000, -0.000000000000000000 ) ) ;
#24479 = VECTOR ( 'NONE', #64636, 1000.000000000000000 ) ;
#24480 = FACE_OUTER_BOUND ( 'NONE', #52437, .T. ) ;
#24481 = VERTEX_POINT ( 'NONE', #67869 ) ;
#24482 = CARTESIAN_POINT ( 'NONE',  ( 0.000000000000000000, 74.74816331893430288, 33.71516098798768724 ) ) ;
#24483 = DIRECTION ( 'NONE',  ( -1.000000000000000000, -0.000000000000000000, 0.000000000000000000 ) ) ;
#24484 = ORIENTED_EDGE ( 'NONE', *, *, #27426, .T. ) ;
#24485 = AXIS2_PLACEMENT_3D ( 'NONE', #7580, #1976, #24864 ) ;
#24486 = CARTESIAN_POINT ( 'NONE',  ( 93.84685191531251292, -211.9973110713294489, 84.66864583420047552 ) ) ;
#24487 = CARTESIAN_POINT ( 'NONE',  ( 92.69370383062501162, -211.3315407142195852, 87.31447916753381833 ) ) ;
#24488 = VERTEX_POINT ( 'NONE', #49456 ) ;
#24489 = CARTESIAN_POINT ( 'NONE',  ( 10.00000000000000000, 0.000000000000000000, 0.000000000000000000 ) ) ;
#24490 = ORIENTED_EDGE ( 'NONE', *, *, #15432, .F. ) ;
#24491 = AXIS2_PLACEMENT_3D ( 'NONE', #69682, #70037, #24201 ) ;
#24492 = LINE ( 'NONE', #64356, #11830 ) ;
#24493 = VERTEX_POINT ( 'NONE', #61122 ) ;
#24494 = AXIS2_PLACEMENT_3D ( 'NONE', #72610, #55712, #4229 ) ;
#24495 = CARTESIAN_POINT ( 'NONE',  ( -93.84685191531254134, 91.99731107132950569, 80.69989583420047552 ) ) ;
#24496 = ORIENTED_EDGE ( 'NONE', *, *, #69686, .F. ) ;
#24497 = VERTEX_POINT ( 'NONE', #4738 ) ;
#24498 = DIRECTION ( 'NONE',  ( -1.000000000000000000, 0.000000000000000000, -0.000000000000000000 ) ) ;
#24499 = ORIENTED_EDGE ( 'NONE', *, *, #52201, .T. ) ;
#24500 = DIRECTION ( 'NONE',  ( 0.000000000000000000, 0.7604059656000323741, -0.6494480483301819929 ) ) ;
#24501 = CARTESIAN_POINT ( 'NONE',  ( -7.670864526094549163, -97.73662565058241114, 5.500000000000000000 ) ) ;
#24502 = ORIENTED_EDGE ( 'NONE', *, *, #5951, .T. ) ;
#24503 = CARTESIAN_POINT ( 'NONE',  ( 0.000000000000000000, 0.000000000000000000, -5.974599999999999689 ) ) ;
#24504 = ORIENTED_EDGE ( 'NONE', *, *, #70600, .F. ) ;
#24505 = DIRECTION ( 'NONE',  ( -1.000000000000000000, -1.776356839400250465E-15, 0.000000000000000000 ) ) ;
#24506 = ORIENTED_EDGE ( 'NONE', *, *, #27304, .F. ) ;
#24507 = EDGE_CURVE ( 'NONE', #68917, #59010, #5246, .T. ) ;
#24508 = EDGE_CURVE ( 'NONE', #39310, #29971, #40047, .T. ) ;
#24509 = VERTEX_POINT ( 'NONE', #4356 ) ;
#24510 = ORIENTED_EDGE ( 'NONE', *, *, #55094, .F. ) ;
#24511 = CARTESIAN_POINT ( 'NONE',  ( 92.69370383062501162, -209.9999999999999716, 82.02281250086714692 ) ) ;
#24512 = CARTESIAN_POINT ( 'NONE',  ( -97.65000000000010516, 91.52997821335250705, 83.59708333333334451 ) ) ;
#24513 = CARTESIAN_POINT ( 'NONE',  ( -94.99999999999997158, -213.0599564267049857, 85.79312500173431033 ) ) ;
#24514 = EDGE_CURVE ( 'NONE', #3169, #32383, #29665, .T. ) ;
#24515 = DIRECTION ( 'NONE',  ( -0.000000000000000000, -0.000000000000000000, 1.000000000000000000 ) ) ;
#24516 = CARTESIAN_POINT ( 'NONE',  ( 0.000000000000000000, 0.000000000000000000, 0.000000000000000000 ) ) ;
#24517 = CARTESIAN_POINT ( 'NONE',  ( 15.00000000000000000, -3.948201729842355068, -23.21447184625292692 ) ) ;
#24518 = CARTESIAN_POINT ( 'NONE',  ( -3.000000000000000000, 22.07842321921492612, -8.187992925817130896 ) ) ;
#24519 = ADVANCED_FACE ( 'NONE', ( #38557 ), #39678, .T. ) ;
#24520 = DIRECTION ( 'NONE',  ( 0.000000000000000000, 0.000000000000000000, 1.000000000000000000 ) ) ;
#24521 = CARTESIAN_POINT ( 'NONE',  ( -96.15314808468745866, -211.9973110713294489, 84.03364583420047040 ) ) ;
#24522 = CARTESIAN_POINT ( 'NONE',  ( -97.30629616937501680, 90.00000000000004263, 82.81656250086714977 ) ) ;
#24523 = EDGE_LOOP ( 'NONE', ( #32977, #30492, #25615, #35817 ) ) ;
#24524 = CIRCLE ( 'NONE', #31698, 15.99999999999999822 ) ;
#24525 = CARTESIAN_POINT ( 'NONE',  ( 92.69370383062498320, 90.00000000000002842, 79.48281250086714067 ) ) ;
#24526 = ADVANCED_FACE ( 'NONE', ( #62235 ), #56219, .T. ) ;
#24527 = EDGE_LOOP ( 'NONE', ( #33369, #12594, #59288, #15727 ) ) ;
#24528 = CARTESIAN_POINT ( 'NONE',  ( 0.000000000000000000, 22.64427369931169309, 30.00120703465213623 ) ) ;
#24529 = DIRECTION ( 'NONE',  ( 1.000000000000000000, -0.000000000000000000, 0.000000000000000000 ) ) ;
#24530 = CYLINDRICAL_SURFACE ( 'NONE', #36181, 77.49899999999999523 ) ;
#24531 = LINE ( 'NONE', #11397, #30746 ) ;
#24532 = DIRECTION ( 'NONE',  ( -1.000000000000000000, 0.000000000000000000, 0.000000000000000000 ) ) ;
#24533 = CARTESIAN_POINT ( 'NONE',  ( -93.84685191531248449, -208.0026889286704943, 83.08114583420048405 ) ) ;
#24534 = DIRECTION ( 'NONE',  ( -1.000000000000000000, -0.000000000000000000, 0.000000000000000000 ) ) ;
#24535 = CARTESIAN_POINT ( 'NONE',  ( 10.00000000000000000, 59.03961581697465277, -46.53671651293886669 ) ) ;
#24536 = DIRECTION ( 'NONE',  ( 0.000000000000000000, -0.8910065241883627918, -0.4539904997395569630 ) ) ;
#24537 = CARTESIAN_POINT ( 'NONE',  ( -7.499999999999970690, 69.70000000000003126, -255.0000000000000000 ) ) ;
#24538 = ORIENTED_EDGE ( 'NONE', *, *, #6450, .F. ) ;
#24539 = CIRCLE ( 'NONE', #31768, 16.00000000000000000 ) ;
#24540 = ORIENTED_EDGE ( 'NONE', *, *, #18471, .T. ) ;
#24541 = CARTESIAN_POINT ( 'NONE',  ( 15.00000000000000000, -3.948201729842032215, 23.21447184625297666 ) ) ;
#24542 = CARTESIAN_POINT ( 'NONE',  ( 2.500000000000000444, 8.494897427831771708, 0.000000000000000000 ) ) ;
#24543 = CARTESIAN_POINT ( 'NONE',  ( -95.00000000000002842, 92.66308142843932671, 88.21406250086714351 ) ) ;
#24544 = CARTESIAN_POINT ( 'NONE',  ( 0.000000000000000000, 16.65972982745045528, -80.28980883073738539 ) ) ;
#24545 = CARTESIAN_POINT ( 'NONE',  ( -93.67500000000003979, 92.29496732002878900, 79.70770833506762187 ) ) ;
#24546 = DIRECTION ( 'NONE',  ( -1.000000000000000000, -0.000000000000000000, -0.000000000000000000 ) ) ;
#24547 = CIRCLE ( 'NONE', #20881, 31.99999999999998579 ) ;
#24548 = CARTESIAN_POINT ( 'NONE',  ( 0.000000000000000000, -120.0000000000000000, 2.500000000000000000 ) ) ;
#24549 = AXIS2_PLACEMENT_3D ( 'NONE', #2427, #54620, #9120 ) ;
#24550 = ORIENTED_EDGE ( 'NONE', *, *, #56694, .F. ) ;
#24551 = ADVANCED_FACE ( 'NONE', ( #72380 ), #49818, .F. ) ;
#24552 = CARTESIAN_POINT ( 'NONE',  ( -96.15314808468751551, 88.00268892867056536, 76.41364583420048007 ) ) ;
#24553 = CIRCLE ( 'NONE', #11338, 82.00000000000000000 ) ;
#24554 = EDGE_CURVE ( 'NONE', #66848, #27381, #10044, .T. ) ;
#24556 = EDGE_CURVE ( 'NONE', #55829, #15433, #62428, .T. ) ;
#24555 = AXIS2_PLACEMENT_3D ( 'NONE', #14857, #37803, #60735 ) ;
#24557 = CARTESIAN_POINT ( 'NONE',  ( -95.00000000002617639, -209.9999999999999432, -74.99999999999349143 ) ) ;
#24558 = FACE_OUTER_BOUND ( 'NONE', #17923, .T. ) ;
#24559 = CARTESIAN_POINT ( 'NONE',  ( 4.999999999999999112, 10.41901085202078292, 40.68715046381932865 ) ) ;
#24560 = DIRECTION ( 'NONE',  ( 0.000000000000000000, 1.000000000000000000, -1.224646799147353207E-16 ) ) ;
#24561 = CARTESIAN_POINT ( 'NONE',  ( -92.69370383062498320, -211.3315407142195852, 85.62114583420047609 ) ) ;
#24562 = AXIS2_PLACEMENT_3D ( 'NONE', #65069, #35376, #59795 ) ;
#24563 = CARTESIAN_POINT ( 'NONE',  ( 10.00000000000000000, -51.29473840253269401, 63.97538442413405591 ) ) ;
#24564 = ADVANCED_FACE ( 'NONE', ( #47797 ), #13941, .T. ) ;
#24565 = AXIS2_PLACEMENT_3D ( 'NONE', #25141, #70982, #66478 ) ;
#24566 = CARTESIAN_POINT ( 'NONE',  ( 97.30629616937498838, 89.06968786819598449, 74.84209103131392737 ) ) ;
#24567 = AXIS2_PLACEMENT_3D ( 'NONE', #68909, #25625, #7600 ) ;
#24568 = CARTESIAN_POINT ( 'NONE',  ( -94.99999999999997158, -212.6630814284392557, 76.62531250086715318 ) ) ;
#24569 = DIRECTION ( 'NONE',  ( -1.000000000000000000, -0.000000000000000000, -0.000000000000000000 ) ) ;
#24570 = VERTEX_POINT ( 'NONE', #5477 ) ;
#24571 = DIRECTION ( 'NONE',  ( -1.000000000000000000, -0.000000000000000000, -0.000000000000000000 ) ) ;
#24572 = CARTESIAN_POINT ( 'NONE',  ( 96.32499999999997442, 92.29496732002878900, 75.81833333333332803 ) ) ;
#24573 = LINE ( 'NONE', #35113, #28146 ) ;
#24574 = DIRECTION ( 'NONE',  ( -1.000000000000000000, -0.000000000000000000, 0.000000000000000000 ) ) ;
#24575 = CARTESIAN_POINT ( 'NONE',  ( 93.84685191531249870, -208.0026889286704943, 76.83697916753381207 ) ) ;
#24576 = VERTEX_POINT ( 'NONE', #13214 ) ;
#24577 = CARTESIAN_POINT ( 'NONE',  ( 0.000000000000000000, 74.65491531819118620, -8.830959090342659579 ) ) ;
#24578 = DIRECTION ( 'NONE',  ( 0.000000000000000000, 0.000000000000000000, 1.000000000000000000 ) ) ;
#24579 = ORIENTED_EDGE ( 'NONE', *, *, #1796, .T. ) ;
#24580 = CARTESIAN_POINT ( 'NONE',  ( 3.000000000000000000, 1.467624384280025174, -2.542000000000001592 ) ) ;
#24581 = ORIENTED_EDGE ( 'NONE', *, *, #36261, .F. ) ;
#24582 = CARTESIAN_POINT ( 'NONE',  ( -3.000000000000000000, -19.89357724624987256, -12.59942793731086041 ) ) ;
#24583 = VECTOR ( 'NONE', #64190, 1000.000000000000000 ) ;
#24584 = ORIENTED_EDGE ( 'NONE', *, *, #65546, .T. ) ;
#24585 = ORIENTED_EDGE ( 'NONE', *, *, #7550, .F. ) ;
#24586 = EDGE_LOOP ( 'NONE', ( #23696, #61957, #65387, #18397 ) ) ;
#24587 = CARTESIAN_POINT ( 'NONE',  ( 0.000000000000000000, 0.000000000000000000, 0.000000000000000000 ) ) ;
#24588 = ORIENTED_EDGE ( 'NONE', *, *, #34209, .F. ) ;
#24589 = ORIENTED_EDGE ( 'NONE', *, *, #39240, .F. ) ;
#24590 = CARTESIAN_POINT ( 'NONE',  ( 92.69370383062498320, 90.00000000000002842, 81.54656250086715374 ) ) ;
#24591 = CIRCLE ( 'NONE', #64221, 82.00000000000000000 ) ;
#24592 = CARTESIAN_POINT ( 'NONE',  ( -95.00000000000002842, 86.94004357329504273, 81.34812500173430294 ) ) ;
#24594 = CARTESIAN_POINT ( 'NONE',  ( -0.0004442498512760095037, 0.001194404164628348752, -49.00000000000000000 ) ) ;
#24593 = VECTOR ( 'NONE', #65121, 999.9999999999998863 ) ;
#24595 = ORIENTED_EDGE ( 'NONE', *, *, #16274, .F. ) ;
#24596 = EDGE_LOOP ( 'NONE', ( #67989, #12727, #61703, #21001 ) ) ;
#24597 = ORIENTED_EDGE ( 'NONE', *, *, #19411, .T. ) ;
#24598 = DIRECTION ( 'NONE',  ( 1.000000000000000000, 0.000000000000000000, 0.000000000000000000 ) ) ;
#24599 = ORIENTED_EDGE ( 'NONE', *, *, #56192, .T. ) ;
#24600 = VECTOR ( 'NONE', #4246, 1000.000000000000000 ) ;
#24601 = DIRECTION ( 'NONE',  ( 0.000000000000000000, 0.000000000000000000, 1.000000000000000000 ) ) ;
#24602 = EDGE_CURVE ( 'NONE', #18738, #11035, #30498, .T. ) ;
#24603 = CARTESIAN_POINT ( 'NONE',  ( -96.13030974027475395, 92.14422361751735480, 74.86230178910948041 ) ) ;
#24604 = CARTESIAN_POINT ( 'NONE',  ( -23.30023580412278505, -123.4057321492263384, -5.500000000000000000 ) ) ;
#24605 = DIRECTION ( 'NONE',  ( -0.000000000000000000, -0.5000000000000003331, -0.8660254037844384856 ) ) ;
#24606 = CARTESIAN_POINT ( 'NONE',  ( 10.00000000000000000, -8.830959090341869100, -74.65491531819127147 ) ) ;
#24607 = CARTESIAN_POINT ( 'NONE',  ( 96.32499999999997442, 92.29496732002878900, 77.72333333333332916 ) ) ;
#24608 = EDGE_CURVE ( 'NONE', #16444, #23574, #66510, .T. ) ;
#24609 = CARTESIAN_POINT ( 'NONE',  ( -94.99999999999997158, -213.0599564267049857, 78.80812500173429669 ) ) ;
#24610 = CARTESIAN_POINT ( 'NONE',  ( 26.47460221209471598, -121.8961639463267090, 5.500000000000000000 ) ) ;
#24611 = ORIENTED_EDGE ( 'NONE', *, *, #27702, .F. ) ;
#24613 = CARTESIAN_POINT ( 'NONE',  ( -97.65000000000001990, 90.00000000000004263, 75.47437500173430180 ) ) ;
#24612 = CARTESIAN_POINT ( 'NONE',  ( 92.34999999999999432, 90.00000000000002842, 75.47437500173430180 ) ) ;
#24614 = ADVANCED_FACE ( 'NONE', ( #70714 ), #36511, .T. ) ;
#24615 = ORIENTED_EDGE ( 'NONE', *, *, #19446, .F. ) ;
#24616 = CARTESIAN_POINT ( 'NONE',  ( 96.15314808468748708, 88.00268892867053694, 77.31322916753381946 ) ) ;
#24617 = CARTESIAN_POINT ( 'NONE',  ( -97.64999999999996305, -208.4700217866474645, 82.32708333333334849 ) ) ;
#24618 = CYLINDRICAL_SURFACE ( 'NONE', #17460, 31.99999999999998579 ) ;
#24619 = LINE ( 'NONE', #42298, #73200 ) ;
#24620 = CIRCLE ( 'NONE', #40237, 77.49900000000000944 ) ;
#24621 = CARTESIAN_POINT ( 'NONE',  ( 92.35000000000000853, -209.9999856621383003, 79.28437450583713542 ) ) ;
#24622 = CARTESIAN_POINT ( 'NONE',  ( 0.000000000000000000, 0.000000000000000000, -6.000000000000000000 ) ) ;
#24623 = ORIENTED_EDGE ( 'NONE', *, *, #5529, .F. ) ;
#24624 = FACE_OUTER_BOUND ( 'NONE', #61074, .T. ) ;
#24625 = DIRECTION ( 'NONE',  ( 0.000000000000000000, 0.000000000000000000, 1.000000000000000000 ) ) ;
#24626 = ORIENTED_EDGE ( 'NONE', *, *, #12719, .T. ) ;
#24627 = VECTOR ( 'NONE', #11774, 1000.000000000000000 ) ;
#24628 = VERTEX_POINT ( 'NONE', #7214 ) ;
#24629 = ADVANCED_FACE ( 'NONE', ( #69626 ), #42176, .T. ) ;
#24630 = EDGE_CURVE ( 'NONE', #40375, #22856, #41063, .T. ) ;
#24631 = LINE ( 'NONE', #51444, #35743 ) ;
#24632 = FACE_OUTER_BOUND ( 'NONE', #16053, .T. ) ;
#24633 = CARTESIAN_POINT ( 'NONE',  ( 0.000000000000000000, 72.35160999960844208, -20.41045688087747223 ) ) ;
#24634 = CYLINDRICAL_SURFACE ( 'NONE', #62564, 31.99999999999998579 ) ;
#24635 =( BOUNDED_CURVE ( )  B_SPLINE_CURVE ( 2, ( #6087, #12072, #16982, #16231, #68490, #17343, #51556 ),
 .UNSPECIFIED., .F., .F. ) 
 B_SPLINE_CURVE_WITH_KNOTS ( ( 3, 2, 2, 3 ),
 ( 0.1905056698837211959, 0.1975614351447063655, 0.2046172006855887515, 0.2116728463006670169 ),
 .UNSPECIFIED. ) 
 CURVE ( )  GEOMETRIC_REPRESENTATION_ITEM ( )  RATIONAL_B_SPLINE_CURVE ( ( 1.000000000000000000, 0.8660254037844387076, 1.000000000000000000, 0.8660254037844387076, 1.000000000000000000, 0.8660276809308509183, 0.9999954457845842137 ) ) 
 REPRESENTATION_ITEM ( '' )  );
#24636 = CARTESIAN_POINT ( 'NONE',  ( -97.30629616937497417, -208.6684592857803011, 77.04864583420048518 ) ) ;
#24637 = ORIENTED_EDGE ( 'NONE', *, *, #4518, .F. ) ;
#24638 = DIRECTION ( 'NONE',  ( -1.000000000000000000, 0.000000000000000000, 0.000000000000000000 ) ) ;
#24639 = EDGE_CURVE ( 'NONE', #51781, #14126, #873, .T. ) ;
#24640 = EDGE_CURVE ( 'NONE', #10916, #36728, #16111, .T. ) ;
#24641 = AXIS2_PLACEMENT_3D ( 'NONE', #30324, #1805, #335 ) ;
#24642 = DIRECTION ( 'NONE',  ( 0.000000000000000000, 0.000000000000000000, -1.000000000000000000 ) ) ;
#24643 = LINE ( 'NONE', #43059, #34627 ) ;
#24644 = CYLINDRICAL_SURFACE ( 'NONE', #70471, 16.00000000000000000 ) ;
#24645 = CARTESIAN_POINT ( 'NONE',  ( -34.02017708624681092, -130.1428571428571388, -2.500000000000000000 ) ) ;
#24646 = CARTESIAN_POINT ( 'NONE',  ( 12.00000000000000000, -22.32062822937488988, -14.36278369418800160 ) ) ;
#24647 = PLANE ( 'NONE',  #33718 ) ;
#24648 = DIRECTION ( 'NONE',  ( -1.000000000000000000, 0.000000000000000000, 0.000000000000000000 ) ) ;
#24649 = CARTESIAN_POINT ( 'NONE',  ( -1.233757462863590115, -120.8531368722710795, -2.500000000000000000 ) ) ;
#24650 = CARTESIAN_POINT ( 'NONE',  ( 10.00000000000000000, -26.08949754953005495, -27.05870788708258701 ) ) ;
#24651 = AXIS2_PLACEMENT_3D ( 'NONE', #21515, #4257, #72281 ) ;
#24652 = AXIS2_PLACEMENT_3D ( 'NONE', #64293, #43505, #49484 ) ;
#24653 = CARTESIAN_POINT ( 'NONE',  ( 92.69370383062498320, 91.33154071421968467, 85.30364583420048064 ) ) ;
#24654 = CARTESIAN_POINT ( 'NONE',  ( -92.69370383062498320, -209.9999999999999716, 86.94406250086716170 ) ) ;
#24655 = CARTESIAN_POINT ( 'NONE',  ( 0.000000000000000000, 0.000000000000000000, -4.400000000000001243 ) ) ;
#24656 = ORIENTED_EDGE ( 'NONE', *, *, #59319, .T. ) ;
#24657 = CARTESIAN_POINT ( 'NONE',  ( -92.35000000000009379, 91.52997821335256390, 81.48041666666665606 ) ) ;
#24658 = CARTESIAN_POINT ( 'NONE',  ( -97.64999999999994884, -208.4700217866474645, 82.32708333333332007 ) ) ;
#24659 = CARTESIAN_POINT ( 'NONE',  ( -96.15314808468752972, 91.99731107132950569, 77.47197916753380298 ) ) ;
#24660 = VECTOR ( 'NONE', #11898, 1000.000000000000000 ) ;
#24661 = AXIS2_PLACEMENT_3D ( 'NONE', #41557, #57379, #29897 ) ;
#24662 = CARTESIAN_POINT ( 'NONE',  ( 95.00000000000000000, -212.6630814284392557, 87.89656250086713385 ) ) ;
#24663 = EDGE_LOOP ( 'NONE', ( #15923, #22396 ) ) ;
#24664 = VERTEX_POINT ( 'NONE', #29750 ) ;
#24665 = AXIS2_PLACEMENT_3D ( 'NONE', #69291, #6873, #70013 ) ;
#24666 = EDGE_LOOP ( 'NONE', ( #27491, #13938, #42584, #38000 ) ) ;
#24667 = DIRECTION ( 'NONE',  ( -1.000000000000000000, 0.000000000000000000, 0.000000000000000000 ) ) ;
#24668 = CARTESIAN_POINT ( 'NONE',  ( -3.000000000000000000, -22.32062822937469804, -14.36278369418829826 ) ) ;
#24669 = CIRCLE ( 'NONE', #43904, 16.00000000000000000 ) ;
#24670 = ORIENTED_EDGE ( 'NONE', *, *, #58501, .F. ) ;
#24671 = ORIENTED_EDGE ( 'NONE', *, *, #40087, .F. ) ;
#24672 = DIRECTION ( 'NONE',  ( 0.000000000000000000, 0.000000000000000000, 1.000000000000000000 ) ) ;
#24673 = CARTESIAN_POINT ( 'NONE',  ( 95.00000000000000000, -207.3369185715606307, 82.65781250086715204 ) ) ;
#24674 = CARTESIAN_POINT ( 'NONE',  ( 0.000000000000000000, 0.000000000000000000, 0.000000000000000000 ) ) ;
#24675 = LINE ( 'NONE', #24315, #18418 ) ;
#24676 = EDGE_CURVE ( 'NONE', #15642, #44823, #23759, .T. ) ;
#24677 = CARTESIAN_POINT ( 'NONE',  ( 93.67500000000001137, -212.2949673200287179, 80.58083333333331666 ) ) ;
#24678 = CARTESIAN_POINT ( 'NONE',  ( 92.35000000000003695, 88.47002178664747873, 76.71791666666666742 ) ) ;
#24679 = DIRECTION ( 'NONE',  ( 1.000000000000000000, 0.000000000000000000, 0.000000000000000000 ) ) ;
#24680 = CARTESIAN_POINT ( 'NONE',  ( 96.32499999999998863, -212.2949673200287179, 84.49666666666666970 ) ) ;
#24681 = PRODUCT_DEFINITION ( 'UNKNOWN', '', #3992, #8566 ) ;
#24682 = EDGE_CURVE ( 'NONE', #54289, #48877, #61735, .T. ) ;
#24683 = ORIENTED_EDGE ( 'NONE', *, *, #57389, .F. ) ;
#24684 = ORIENTED_EDGE ( 'NONE', *, *, #55586, .T. ) ;
#24685 = VERTEX_POINT ( 'NONE', #1979 ) ;
#24686 = VERTEX_POINT ( 'NONE', #47437 ) ;
#24687 = CARTESIAN_POINT ( 'NONE',  ( 0.000000000000000000, -33.79645857604525361, 16.45098606841114730 ) ) ;
#24688 = CARTESIAN_POINT ( 'NONE',  ( -97.30629616937501680, 88.66845928578038638, 87.94947916753382344 ) ) ;
#24689 = ADVANCED_FACE ( 'NONE', ( #36148 ), #59459, .T. ) ;
#24690 = CARTESIAN_POINT ( 'NONE',  ( 11.99999999999999822, 68.67312586195046720, -35.91791733033404199 ) ) ;
#24691 = CARTESIAN_POINT ( 'NONE',  ( -92.35000000000003695, 90.00000000000004263, 83.96750000000000114 ) ) ;
#24692 = CARTESIAN_POINT ( 'NONE',  ( 96.15314808468748708, -208.0026889286704943, 87.52614583420047722 ) ) ;
#24693 = CARTESIAN_POINT ( 'NONE',  ( 94.99999999999998579, 86.94004357329500010, 79.99874999999998693 ) ) ;
#24695 = ORIENTED_EDGE ( 'NONE', *, *, #19018, .T. ) ;
#24694 = EDGE_CURVE ( 'NONE', #31534, #34228, #30863, .T. ) ;
#24696 = CARTESIAN_POINT ( 'NONE',  ( -96.32499999999996021, -207.7050326799711968, 88.70354166840097321 ) ) ;
#24697 = VERTEX_POINT ( 'NONE', #47075 ) ;
#24698 = CARTESIAN_POINT ( 'NONE',  ( 96.32499999999998863, -212.2949673200287179, 80.05166666666666231 ) ) ;
#24699 = VERTEX_POINT ( 'NONE', #69979 ) ;
#24700 = CARTESIAN_POINT ( 'NONE',  ( -96.32500000000001705, 92.29496732002878900, 86.16354166840096696 ) ) ;
#24701 = EDGE_CURVE ( 'NONE', #38079, #22373, #25710, .T. ) ;
#24702 = CARTESIAN_POINT ( 'NONE',  ( 96.15314808468748708, 91.99731107132950569, 89.58989583420049030 ) ) ;
#24703 = VECTOR ( 'NONE', #66341, 1000.000000000000114 ) ;
#24704 = ORIENTED_EDGE ( 'NONE', *, *, #5445, .T. ) ;
#24705 = DIRECTION ( 'NONE',  ( 0.000000000000000000, 0.000000000000000000, 1.000000000000000000 ) ) ;
#24706 = DIRECTION ( 'NONE',  ( 1.000000000000000000, 0.000000000000000000, -0.000000000000000000 ) ) ;
#24707 = DIRECTION ( 'NONE',  ( 0.000000000000000000, -1.000000000000000000, 0.000000000000000000 ) ) ;
#24708 = CARTESIAN_POINT ( 'NONE',  ( -12.49999999999999645, 0.000000000000000000, 40.80000000000001847 ) ) ;
#24709 = ORIENTED_EDGE ( 'NONE', *, *, #50315, .T. ) ;
#24710 = CYLINDRICAL_SURFACE ( 'NONE', #17098, 2.649999999999999467 ) ;
#24711 = VECTOR ( 'NONE', #4655, 1000.000000000000000 ) ;
#24712 = CARTESIAN_POINT ( 'NONE',  ( -96.15314808468745866, -211.9973110713294489, 75.14364583420046984 ) ) ;
#24713 = ORIENTED_EDGE ( 'NONE', *, *, #68586, .T. ) ;
#24714 = AXIS2_PLACEMENT_3D ( 'NONE', #5363, #51570, #123 ) ;
#24715 = ORIENTED_EDGE ( 'NONE', *, *, #73691, .F. ) ;
#24717 = CARTESIAN_POINT ( 'NONE',  ( 11.99999999999999822, -46.54456581323762521, -59.03342792756313884 ) ) ;
#24716 = AXIS2_PLACEMENT_3D ( 'NONE', #71972, #20486, #31750 ) ;
#24718 = EDGE_CURVE ( 'NONE', #72660, #74057, #40234, .T. ) ;
#24719 = ADVANCED_FACE ( 'NONE', ( #3811 ), #21066, .T. ) ;
#24720 = CARTESIAN_POINT ( 'NONE',  ( 10.00000000000000000, 0.000000000000000000, 0.000000000000000000 ) ) ;
#24721 = VECTOR ( 'NONE', #1296, 1000.000000000000114 ) ;
#24722 = DIRECTION ( 'NONE',  ( -1.000000000000000000, -0.000000000000000000, 0.000000000000000000 ) ) ;
#24723 = CARTESIAN_POINT ( 'NONE',  ( -97.30629616937497417, -211.3315407142195852, 87.31447916753381833 ) ) ;
#24724 = ORIENTED_EDGE ( 'NONE', *, *, #41231, .F. ) ;
#24725 = LINE ( 'NONE', #25467, #57330 ) ;
#24726 = VERTEX_POINT ( 'NONE', #31244 ) ;
#24727 = VERTEX_POINT ( 'NONE', #44017 ) ;
#24728 = CARTESIAN_POINT ( 'NONE',  ( 1.560000000000000053, 0.8660254037844389297, -1.500000000000000000 ) ) ;
#24729 = CARTESIAN_POINT ( 'NONE',  ( -97.65000000000001990, 90.00000000000004263, 86.82500000000000284 ) ) ;
#24730 = AXIS2_PLACEMENT_3D ( 'NONE', #25585, #48518, #14307 ) ;
#24731 = LINE ( 'NONE', #7069, #65756 ) ;
#24732 = CARTESIAN_POINT ( 'NONE',  ( 92.69370383062498320, 90.00000000000002842, 82.02281250086714692 ) ) ;
#24733 = DIRECTION ( 'NONE',  ( -1.000000000000000000, 0.000000000000000000, 0.000000000000000000 ) ) ;
#24734 = FACE_BOUND ( 'NONE', #34859, .T. ) ;
#24735 = CARTESIAN_POINT ( 'NONE',  ( -95.00000000000002842, 93.05995642670504253, 85.39624999999998067 ) ) ;
#24736 = CARTESIAN_POINT ( 'NONE',  ( 0.000000000000000000, 0.000000000000000000, -54.99999999999998579 ) ) ;
#24737 = CARTESIAN_POINT ( 'NONE',  ( 10.00000000000000000, 0.000000000000000000, 0.000000000000000000 ) ) ;
#24738 = CARTESIAN_POINT ( 'NONE',  ( 0.000000000000000000, 0.000000000000000000, -105.0000000000000000 ) ) ;
#24739 = CARTESIAN_POINT ( 'NONE',  ( 10.00000000000000000, 33.00180498840046539, 17.80606268964551120 ) ) ;
#24740 = CARTESIAN_POINT ( 'NONE',  ( 93.67500000000001137, -207.7050326799711968, 85.52854166840096184 ) ) ;
#24741 = CARTESIAN_POINT ( 'NONE',  ( 17.50000000000000355, 2.143131898507868643E-15, 20.00000000000000000 ) ) ;
#24742 = EDGE_LOOP ( 'NONE', ( #10619, #15926, #63367, #52418 ) ) ;
#24743 = CARTESIAN_POINT ( 'NONE',  ( -97.30629616937501680, 91.33154071421968467, 86.41489583420047893 ) ) ;
#24744 = CARTESIAN_POINT ( 'NONE',  ( 6.000000000000000000, -71.21200624218825226, 40.65526001592589722 ) ) ;
#24745 = DIRECTION ( 'NONE',  ( 1.000000000000000000, -0.000000000000000000, -0.000000000000000000 ) ) ;
#24746 = ORIENTED_EDGE ( 'NONE', *, *, #19786, .F. ) ;
#24747 = LINE ( 'NONE', #53692, #16229 ) ;
#24748 = DIRECTION ( 'NONE',  ( 1.000000000000000000, 0.000000000000000000, 0.000000000000000000 ) ) ;
#24749 = AXIS2_PLACEMENT_3D ( 'NONE', #23429, #18512, #64396 ) ;
#24750 = DIRECTION ( 'NONE',  ( -1.000000000000000000, -0.000000000000000000, 0.000000000000000000 ) ) ;
#24751 = EDGE_CURVE ( 'NONE', #66932, #55194, #53303, .T. ) ;
#24752 = CYLINDRICAL_SURFACE ( 'NONE', #64486, 32.00000000000000000 ) ;
#24753 = CARTESIAN_POINT ( 'NONE',  ( 96.15314808468748708, -208.0026889286704943, 81.33489583420049485 ) ) ;
#24754 = VECTOR ( 'NONE', #71103, 1000.000000000000000 ) ;
#24755 = VERTEX_POINT ( 'NONE', #66933 ) ;
#24756 = ADVANCED_FACE ( 'NONE', ( #2719 ), #72925, .T. ) ;
#24757 = AXIS2_PLACEMENT_3D ( 'NONE', #30634, #24638, #37421 ) ;
#24758 = ORIENTED_EDGE ( 'NONE', *, *, #70284, .T. ) ;
#24759 = EDGE_CURVE ( 'NONE', #45705, #56648, #15429, .T. ) ;
#24760 = DIRECTION ( 'NONE',  ( -1.000000000000000000, 0.000000000000000000, -0.000000000000000000 ) ) ;
#24761 = ORIENTED_EDGE ( 'NONE', *, *, #4506, .F. ) ;
#24762 = AXIS2_PLACEMENT_3D ( 'NONE', #43339, #66620, #8369 ) ;
#24763 = LINE ( 'NONE', #24042, #32966 ) ;
#24764 = AXIS2_PLACEMENT_3D ( 'NONE', #71769, #72148, #48487 ) ;
#24765 = CARTESIAN_POINT ( 'NONE',  ( 92.69370383062501162, -211.3315407142195852, 75.72572916753381378 ) ) ;
#24766 = VERTEX_POINT ( 'NONE', #66581 ) ;
#24767 = CARTESIAN_POINT ( 'NONE',  ( 97.30629616937498838, -209.9999999999999716, 79.95906250086714806 ) ) ;
#24768 = EDGE_CURVE ( 'NONE', #50378, #6415, #47299, .T. ) ;
#24769 = ORIENTED_EDGE ( 'NONE', *, *, #28168, .F. ) ;
#24770 = LINE ( 'NONE', #53711, #26325 ) ;
#24771 = ORIENTED_EDGE ( 'NONE', *, *, #23667, .T. ) ;
#24772 = VERTEX_POINT ( 'NONE', #25601 ) ;
#24773 = DIRECTION ( 'NONE',  ( -1.000000000000000000, 0.000000000000000000, 0.000000000000000000 ) ) ;
#24774 = AXIS2_PLACEMENT_3D ( 'NONE', #32232, #19481, #2974 ) ;
#24775 = CARTESIAN_POINT ( 'NONE',  ( -10.00000000000000000, 0.000000000000000000, 0.000000000000000000 ) ) ;
#24776 = ORIENTED_EDGE ( 'NONE', *, *, #8913, .T. ) ;
#24777 = DIRECTION ( 'NONE',  ( -1.000000000000000000, -0.000000000000000000, -0.000000000000000000 ) ) ;
#24778 = CARTESIAN_POINT ( 'NONE',  ( 95.00000000000000000, -206.9400435732949575, 83.57062500173429953 ) ) ;
#24779 = CARTESIAN_POINT ( 'NONE',  ( 96.32499999999997442, 92.29496732002878900, 89.15333333333333599 ) ) ;
#24780 = ORIENTED_EDGE ( 'NONE', *, *, #69370, .F. ) ;
#24781 = CARTESIAN_POINT ( 'NONE',  ( -10.00000000000000000, 0.000000000000000000, 0.000000000000000000 ) ) ;
#24782 = DIRECTION ( 'NONE',  ( 0.000000000000000000, 0.000000000000000000, -1.000000000000000000 ) ) ;
#24783 = ORIENTED_EDGE ( 'NONE', *, *, #5102, .T. ) ;
#24784 = ORIENTED_EDGE ( 'NONE', *, *, #29091, .F. ) ;
#24785 = CARTESIAN_POINT ( 'NONE',  ( -97.30629616937501680, 90.00000000000004263, 89.16656250086715829 ) ) ;
#24786 = EDGE_CURVE ( 'NONE', #70328, #26342, #19955, .T. ) ;
#24787 = CARTESIAN_POINT ( 'NONE',  ( 92.69370383062498320, 88.66845928578037217, 83.98072916753380923 ) ) ;
#24788 = ORIENTED_EDGE ( 'NONE', *, *, #58047, .F. ) ;
#24789 = CARTESIAN_POINT ( 'NONE',  ( 96.32499999999998863, 87.70503267997126784, 85.84604166840097150 ) ) ;
#24790 = PRESENTATION_STYLE_ASSIGNMENT (( #12762 ) ) ;
#24791 = ORIENTED_EDGE ( 'NONE', *, *, #60381, .T. ) ;
#24792 = FACE_OUTER_BOUND ( 'NONE', #13876, .T. ) ;
#24793 = CARTESIAN_POINT ( 'NONE',  ( 92.35000000021533140, 90.00002100773845370, 79.91868729553033290 ) ) ;
#24794 = VERTEX_POINT ( 'NONE', #8693 ) ;
#24795 = ORIENTED_EDGE ( 'NONE', *, *, #47047, .T. ) ;
#24796 = VERTEX_POINT ( 'NONE', #55292 ) ;
#24797 = FACE_OUTER_BOUND ( 'NONE', #60289, .T. ) ;
#24798 = DIRECTION ( 'NONE',  ( -1.000000000000000000, 0.000000000000000000, 0.000000000000000000 ) ) ;
#24799 = CARTESIAN_POINT ( 'NONE',  ( -97.65000000000001990, 90.00000000000004263, 84.92000000000000171 ) ) ;
#24800 = ADVANCED_FACE ( 'NONE', ( #72562 ), #15060, .T. ) ;
#24801 = ORIENTED_EDGE ( 'NONE', *, *, #60554, .T. ) ;
#24802 = EDGE_CURVE ( 'NONE', #23521, #30219, #65839, .T. ) ;
#24803 = CARTESIAN_POINT ( 'NONE',  ( 94.99999999999998579, 86.94004357329502852, 81.90375000000000227 ) ) ;
#24804 = CYLINDRICAL_SURFACE ( 'NONE', #25094, 32.00000000000000000 ) ;
#24805 = VERTEX_POINT ( 'NONE', #61314 ) ;
#24806 = CARTESIAN_POINT ( 'NONE',  ( -7.500000000000016875, -80.00000000000001421, -269.9999999999999432 ) ) ;
#24807 = CARTESIAN_POINT ( 'NONE',  ( -92.69370383062498320, -209.9999999999999716, 83.61031250086713840 ) ) ;
#24808 = ORIENTED_EDGE ( 'NONE', *, *, #6732, .F. ) ;
#24809 = EDGE_CURVE ( 'NONE', #61936, #37997, #49275, .T. ) ;
#24810 = CARTESIAN_POINT ( 'NONE',  ( 10.00000000000000000, 26.02418014898407961, -70.52718814184231633 ) ) ;
#24811 = VECTOR ( 'NONE', #25919, 1000.000000000000000 ) ;
#24812 = CARTESIAN_POINT ( 'NONE',  ( 5.999999999999999112, 81.96053171279902472, -2.543863470248677316 ) ) ;
#24813 = DIRECTION ( 'NONE',  ( -1.000000000000000000, 0.000000000000000000, 0.000000000000000000 ) ) ;
#24814 = LINE ( 'NONE', #37219, #48262 ) ;
#24815 = AXIS2_PLACEMENT_3D ( 'NONE', #72202, #50755, #16550 ) ;
#24816 = DIRECTION ( 'NONE',  ( -1.000000000000000000, -0.000000000000000000, 0.000000000000000000 ) ) ;
#24817 = CIRCLE ( 'NONE', #74073, 31.99999999999999289 ) ;
#24818 = CARTESIAN_POINT ( 'NONE',  ( 0.000000000000000000, 0.000000000000000000, -184.9999999999999432 ) ) ;
#24819 = FACE_OUTER_BOUND ( 'NONE', #69159, .T. ) ;
#24820 = CIRCLE ( 'NONE', #59608, 77.49899999999999523 ) ;
#24821 = LINE ( 'NONE', #64679, #73542 ) ;
#24822 = CARTESIAN_POINT ( 'NONE',  ( 92.34999999999999432, 90.00000000000002842, 83.09437500173430635 ) ) ;
#24823 = LINE ( 'NONE', #19907, #65624 ) ;
#24824 = CARTESIAN_POINT ( 'NONE',  ( -93.84685191531254134, 91.99731107132950569, 76.09614583420047040 ) ) ;
#24825 = CARTESIAN_POINT ( 'NONE',  ( 0.000000000000000000, -75.54627589209931671, -17.28742895386164591 ) ) ;
#24826 = DIRECTION ( 'NONE',  ( 0.000000000000000000, 0.000000000000000000, 1.000000000000000000 ) ) ;
#24827 = AXIS2_PLACEMENT_3D ( 'NONE', #65792, #8267, #9011 ) ;
#24828 = CARTESIAN_POINT ( 'NONE',  ( 10.00000000000000000, 0.000000000000000000, 0.000000000000000000 ) ) ;
#24829 = PLANE ( 'NONE',  #72515 ) ;
#24830 = CARTESIAN_POINT ( 'NONE',  ( -17.26469406256017791, -140.1601175325492648, 2.500000000000000000 ) ) ;
#24831 = CARTESIAN_POINT ( 'NONE',  ( 93.67500000000001137, -212.2949673200287179, 77.40583333333331950 ) ) ;
#24832 = CYLINDRICAL_SURFACE ( 'NONE', #46560, 82.00000000000000000 ) ;
#24833 = CARTESIAN_POINT ( 'NONE',  ( 96.32499999999998863, 87.70503267997126784, 75.68604166840097491 ) ) ;
#24834 = CARTESIAN_POINT ( 'NONE',  ( -97.30629616937497417, -211.3315407142195852, 75.24947916753383481 ) ) ;
#24835 = CARTESIAN_POINT ( 'NONE',  ( 5.000000000000000888, 0.000000000000000000, -6.000000000000000000 ) ) ;
#24836 = VERTEX_POINT ( 'NONE', #55660 ) ;
#24837 = CARTESIAN_POINT ( 'NONE',  ( 10.00000000000000000, -35.47612816024539484, 22.48208911017487921 ) ) ;
#24838 = CARTESIAN_POINT ( 'NONE',  ( 97.64999999999992042, -211.5299782133524786, 88.35958333333334735 ) ) ;
#24839 = LINE ( 'NONE', #7560, #10557 ) ;
#24840 = DIRECTION ( 'NONE',  ( 1.000000000000000000, -0.000000000000000000, -0.000000000000000000 ) ) ;
#24841 = EDGE_CURVE ( 'NONE', #53437, #16864, #35323, .T. ) ;
#24842 = EDGE_CURVE ( 'NONE', #36680, #71004, #50003, .T. ) ;
#24843 = CARTESIAN_POINT ( 'NONE',  ( -10.00000000000000000, 0.000000000000000000, 0.000000000000000000 ) ) ;
#24844 = VERTEX_POINT ( 'NONE', #48901 ) ;
#24846 = EDGE_CURVE ( 'NONE', #21322, #32442, #34089, .T. ) ;
#24845 = LINE ( 'NONE', #7926, #37129 ) ;
#24847 = DIRECTION ( 'NONE',  ( -1.000000000000000000, -0.000000000000000000, 0.000000000000000000 ) ) ;
#24848 = ORIENTED_EDGE ( 'NONE', *, *, #61477, .F. ) ;
#24849 =( BOUNDED_CURVE ( )  B_SPLINE_CURVE ( 2, ( #4026, #38964, #37854, #31818, #3657, #26557, #22034 ),
 .UNSPECIFIED., .F., .F. ) 
 B_SPLINE_CURVE_WITH_KNOTS ( ( 3, 2, 2, 3 ),
 ( 0.5503499107226623721, 0.5574054777297072771, 0.5644612432705895522, 0.5715170088666297055 ),
 .UNSPECIFIED. ) 
 CURVE ( )  GEOMETRIC_REPRESENTATION_ITEM ( )  RATIONAL_B_SPLINE_CURVE ( ( 0.9999924607068793048, 0.8660291735370716504, 1.000000000000000000, 0.8660254037844387076, 1.000000000000000000, 0.8660254037844387076, 1.000000000000000000 ) ) 
 REPRESENTATION_ITEM ( '' )  );
#24850 = CARTESIAN_POINT ( 'NONE',  ( 95.00000000000000000, -212.6630814284392557, 84.08656250086714579 ) ) ;
#24851 = CARTESIAN_POINT ( 'NONE',  ( 11.99999999999999822, 0.000000000000000000, 0.000000000000000000 ) ) ;
#24852 = VECTOR ( 'NONE', #57104, 1000.000000000000000 ) ;
#24853 = ORIENTED_EDGE ( 'NONE', *, *, #36217, .T. ) ;
#24854 = CARTESIAN_POINT ( 'NONE',  ( 0.000000000000000000, 0.000000000000000000, 0.000000000000000000 ) ) ;
#24855 = CIRCLE ( 'NONE', #34464, 31.99999999999998579 ) ;
#24856 = EDGE_CURVE ( 'NONE', #359, #17023, #1713, .T. ) ;
#24857 = VERTEX_POINT ( 'NONE', #72201 ) ;
#24858 = FACE_BOUND ( 'NONE', #51780, .T. ) ;
#24859 = ORIENTED_EDGE ( 'NONE', *, *, #23172, .F. ) ;
#24860 = CARTESIAN_POINT ( 'NONE',  ( -95.00000000000002842, 87.33691857156074434, 81.70531250086715147 ) ) ;
#24861 = ORIENTED_EDGE ( 'NONE', *, *, #16245, .F. ) ;
#24862 = VECTOR ( 'NONE', #56065, 1000.000000000000000 ) ;
#24863 = EDGE_LOOP ( 'NONE', ( #72018, #68822, #47376, #25178 ) ) ;
#24864 = DIRECTION ( 'NONE',  ( 0.000000000000000000, 0.000000000000000000, 1.000000000000000000 ) ) ;
#24865 = CIRCLE ( 'NONE', #26041, 32.00000000000000000 ) ;
#24866 = ORIENTED_EDGE ( 'NONE', *, *, #56873, .F. ) ;
#24867 = DIRECTION ( 'NONE',  ( -1.000000000000000000, 0.000000000000000000, -0.000000000000000000 ) ) ;
#24868 = DIRECTION ( 'NONE',  ( 0.000000000000000000, 0.000000000000000000, 1.000000000000000000 ) ) ;
#24869 = ORIENTED_EDGE ( 'NONE', *, *, #33916, .F. ) ;
#24871 = LINE ( 'NONE', #41792, #69419 ) ;
#24870 = PRODUCT_DEFINITION_SHAPE ( 'NONE', 'NONE',  #74370 ) ;
#24872 = AXIS2_PLACEMENT_3D ( 'NONE', #28250, #17715, #23727 ) ;
#24873 = VERTEX_POINT ( 'NONE', #37998 ) ;
#24874 = CARTESIAN_POINT ( 'NONE',  ( 0.000000000000000000, 0.000000000000000000, 0.000000000000000000 ) ) ;
#24875 = EDGE_CURVE ( 'NONE', #24493, #54754, #2943, .T. ) ;
#24876 = ORIENTED_EDGE ( 'NONE', *, *, #45269, .F. ) ;
#24877 = ORIENTED_EDGE ( 'NONE', *, *, #39377, .T. ) ;
#24878 = VERTEX_POINT ( 'NONE', #45889 ) ;
#24879 = CARTESIAN_POINT ( 'NONE',  ( 92.69370383062501162, -209.9999999999999716, 79.48281250086714067 ) ) ;
#24880 = CYLINDRICAL_SURFACE ( 'NONE', #32828, 16.00000000000000000 ) ;
#24881 = ITEM_DEFINED_TRANSFORMATION ( 'NONE', 'NONE', #52005,  #43395 ) ;
#24882 = DIRECTION ( 'NONE',  ( 1.000000000000000000, -0.000000000000000000, -0.000000000000000000 ) ) ;
#24883 = CIRCLE ( 'NONE', #6854, 42.00000000000000000 ) ;
#24884 = DIRECTION ( 'NONE',  ( 0.000000000000000000, 0.000000000000000000, 1.000000000000000000 ) ) ;
#24885 = CARTESIAN_POINT ( 'NONE',  ( -97.64999999999996305, -209.9999999999999716, 90.00000000000000000 ) ) ;
#24886 = CARTESIAN_POINT ( 'NONE',  ( -11.59999999999999787, 0.000000000000000000, 42.00000000000001421 ) ) ;
#24887 = DIRECTION ( 'NONE',  ( 1.000000000000000000, -0.000000000000000000, -0.000000000000000000 ) ) ;
#24888 = CARTESIAN_POINT ( 'NONE',  ( -89.99999999999998579, -124.0000000000000142, 39.99999999999996447 ) ) ;
#24889 = CARTESIAN_POINT ( 'NONE',  ( -96.15314808468745866, -211.9973110713294489, 80.22364583420046813 ) ) ;
#24890 = VECTOR ( 'NONE', #49192, 1000.000000000000000 ) ;
#24891 = CARTESIAN_POINT ( 'NONE',  ( -93.84685191531254134, 91.99731107132950569, 80.69989583420047552 ) ) ;
#24892 = EDGE_CURVE ( 'NONE', #31231, #1337, #12513, .T. ) ;
#24893 = EDGE_LOOP ( 'NONE', ( #43011, #73885, #51635, #22380 ) ) ;
#24894 = EDGE_CURVE ( 'NONE', #48383, #60757, #65709, .T. ) ;
#24895 = CARTESIAN_POINT ( 'NONE',  ( 94.99999999999998579, 87.33691857156068750, 80.91156250086714863 ) ) ;
#24896 = ORIENTED_EDGE ( 'NONE', *, *, #47883, .F. ) ;
#24897 = CARTESIAN_POINT ( 'NONE',  ( 94.99999999999998579, 90.00000000000002842, 73.40771935957695860 ) ) ;
#24898 = LINE ( 'NONE', #47825, #50349 ) ;
#24899 = CARTESIAN_POINT ( 'NONE',  ( -3.000000000000000000, 9.615535125378775305, 24.73947219025917121 ) ) ;
#24900 = CARTESIAN_POINT ( 'NONE',  ( 10.00000000000000000, 0.000000000000000000, 0.000000000000000000 ) ) ;
#24901 = CARTESIAN_POINT ( 'NONE',  ( -94.99999999999997158, -212.6630814284392557, 83.45156250086714067 ) ) ;
#24902 = FACE_OUTER_BOUND ( 'NONE', #51950, .T. ) ;
#24903 = CARTESIAN_POINT ( 'NONE',  ( 10.00000000000000000, 35.92658777277525672, -10.74501242461245809 ) ) ;
#24904 = DIRECTION ( 'NONE',  ( 1.000000000000000000, 0.000000000000000000, 0.000000000000000000 ) ) ;
#24905 = EDGE_LOOP ( 'NONE', ( #497, #44323, #43483, #8680 ) ) ;
#24906 = ORIENTED_EDGE ( 'NONE', *, *, #29338, .T. ) ;
#24907 = DIRECTION ( 'NONE',  ( -1.000000000000000000, 0.000000000000000000, 0.000000000000000000 ) ) ;
#24908 = DIRECTION ( 'NONE',  ( -1.000000000000000000, 0.000000000000000000, 0.000000000000000000 ) ) ;
#24909 = DIRECTION ( 'NONE',  ( 1.000000000000000000, 0.000000000000000000, 0.000000000000000000 ) ) ;
#24910 = CARTESIAN_POINT ( 'NONE',  ( -92.69370383062502583, 88.66845928578038638, 84.82739583420045903 ) ) ;
#24911 = CARTESIAN_POINT ( 'NONE',  ( -97.50991008589724629, -209.8784921249854563, 74.91582548749271098 ) ) ;
#24912 = DIRECTION ( 'NONE',  ( -1.000000000000000000, 0.000000000000000000, 0.000000000000000000 ) ) ;
#24913 =( REPRESENTATION_RELATIONSHIP ('NONE','NONE', #31117, #42128 ) REPRESENTATION_RELATIONSHIP_WITH_TRANSFORMATION ( #54206 )SHAPE_REPRESENTATION_RELATIONSHIP( ) );
#24914 = DIRECTION ( 'NONE',  ( -0.9966891607226785466, -0.08130631524010122069, 0.000000000000000000 ) ) ;
#24915 = CARTESIAN_POINT ( 'NONE',  ( 0.000000000000000000, 46.21855187248719687, -62.20884554313968806 ) ) ;
#24916 = AXIS2_PLACEMENT_3D ( 'NONE', #70941, #65694, #64577 ) ;
#24917 = ORIENTED_EDGE ( 'NONE', *, *, #61876, .T. ) ;
#24918 = DIRECTION ( 'NONE',  ( 0.000000000000000000, 0.000000000000000000, 1.000000000000000000 ) ) ;
#24919 = VECTOR ( 'NONE', #22431, 1000.000000000000000 ) ;
#24920 = DIRECTION ( 'NONE',  ( -2.603472992746261562E-14, -2.546204323184492723E-14, 1.000000000000000000 ) ) ;
#24921 = DIRECTION ( 'NONE',  ( 0.000000000000000000, -0.2334453638559126909, 0.9723699203976748917 ) ) ;
#24922 = AXIS2_PLACEMENT_3D ( 'NONE', #32662, #60520, #55231 ) ;
#24923 = CARTESIAN_POINT ( 'NONE',  ( 96.32499999999998863, -207.7050326799711968, 84.15270833506762926 ) ) ;
#24924 = CARTESIAN_POINT ( 'NONE',  ( 10.00000000000000000, -22.64427369931148348, -30.00120703465229965 ) ) ;
#24925 = CARTESIAN_POINT ( 'NONE',  ( -97.30629616937497417, -208.6684592857803011, 85.30364583420048064 ) ) ;
#24926 = SHAPE_REPRESENTATION_RELATIONSHIP ( 'NONE' , 'NONE' ,  #23897, #28332 ) ;
#24927 = DIRECTION ( 'NONE',  ( -1.000000000000000000, 0.000000000000000000, 0.000000000000000000 ) ) ;
#24928 = DIRECTION ( 'NONE',  ( -1.000000000000000000, -0.000000000000000000, 0.000000000000000000 ) ) ;
#24929 = EDGE_CURVE ( 'NONE', #14882, #9779, #5297, .T. ) ;
#24930 = CARTESIAN_POINT ( 'NONE',  ( -92.69370383062498320, -211.3315407142195852, 77.36614583420048064 ) ) ;
#24931 = DIRECTION ( 'NONE',  ( -1.000000000000000000, -0.000000000000000000, -0.000000000000000000 ) ) ;
#24932 = ORIENTED_EDGE ( 'NONE', *, *, #17264, .F. ) ;
#24933 = DIRECTION ( 'NONE',  ( -0.000000000000000000, -0.000000000000000000, 1.000000000000000000 ) ) ;
#24934 = CARTESIAN_POINT ( 'NONE',  ( 92.34999999999999432, 90.00000000000002842, 76.03000000000000114 ) ) ;
#24935 = DIRECTION ( 'NONE',  ( 0.000000000000000000, 0.8910065241883688980, -0.4539904997395445840 ) ) ;
#24936 = EDGE_CURVE ( 'NONE', #66201, #61596, #22195, .T. ) ;
#24937 = CIRCLE ( 'NONE', #35714, 77.49900000000000944 ) ;
#24938 = ADVANCED_FACE ( 'NONE', ( #27828 ), #40228, .T. ) ;
#24939 = DIRECTION ( 'NONE',  ( 1.000000000000000000, 1.427937372958405461E-15, 7.962523111839130290E-16 ) ) ;
#24940 = CARTESIAN_POINT ( 'NONE',  ( 96.15314808468750130, -211.9973110713294489, 75.88447916753381151 ) ) ;
#24941 = EDGE_LOOP ( 'NONE', ( #2252, #62147, #5364, #6412 ) ) ;
#24942 = CIRCLE ( 'NONE', #70535, 23.50000000000489919 ) ;
#24943 = FACE_OUTER_BOUND ( 'NONE', #29138, .T. ) ;
#24944 = EDGE_LOOP ( 'NONE', ( #56353, #29882, #41366, #74135 ) ) ;
#24945 = AXIS2_PLACEMENT_3D ( 'NONE', #10593, #39555, #33149 ) ;
#24946 = CARTESIAN_POINT ( 'NONE',  ( 10.00000000000000000, 0.000000000000000000, 0.000000000000000000 ) ) ;
#24947 = EDGE_LOOP ( 'NONE', ( #12377, #9601, #53016, #22475 ) ) ;
#24948 = EDGE_CURVE ( 'NONE', #58812, #24509, #73730, .T. ) ;
#24949 = DIRECTION ( 'NONE',  ( -1.000000000000000000, 0.000000000000000000, 0.000000000000000000 ) ) ;
#24950 = EDGE_LOOP ( 'NONE', ( #29085, #11769 ) ) ;
#24951 = ORIENTED_EDGE ( 'NONE', *, *, #55359, .F. ) ;
#24952 = ORIENTED_EDGE ( 'NONE', *, *, #31733, .T. ) ;
#24953 = CARTESIAN_POINT ( 'NONE',  ( -92.35000000000003695, 90.00000000000004263, 90.00000000000000000 ) ) ;
#24954 = VERTEX_POINT ( 'NONE', #45515 ) ;
#24955 = EDGE_CURVE ( 'NONE', #45415, #19936, #73368, .T. ) ;
#24956 = ORIENTED_EDGE ( 'NONE', *, *, #74005, .F. ) ;
#24957 = CARTESIAN_POINT ( 'NONE',  ( 93.84685191531248449, 91.99731107132950569, 79.53572916753381605 ) ) ;
#24958 = CARTESIAN_POINT ( 'NONE',  ( 97.64997490601828645, -211.5299927013694798, 89.07395733288659301 ) ) ;
#24959 = CIRCLE ( 'NONE', #34564, 3.000000000000000444 ) ;
#24960 = ADVANCED_FACE ( 'NONE', ( #38746 ), #17292, .F. ) ;
#24961 = CARTESIAN_POINT ( 'NONE',  ( -97.65000000000001990, 91.52997821335253548, 88.12145833506765769 ) ) ;
#24962 = VERTEX_POINT ( 'NONE', #5663 ) ;
#24963 = AXIS2_PLACEMENT_3D ( 'NONE', #57388, #34831, #68306 ) ;
#24964 = VERTEX_POINT ( 'NONE', #63178 ) ;
#24965 = ORIENTED_EDGE ( 'NONE', *, *, #19180, .T. ) ;
#24966 = CARTESIAN_POINT ( 'NONE',  ( 92.34999999999999432, 90.00000000000002842, 90.00000000000000000 ) ) ;
#24968 = ADVANCED_FACE ( 'NONE', ( #74055 ), #11636, .F. ) ;
#24967 = ORIENTED_EDGE ( 'NONE', *, *, #46092, .F. ) ;
#24969 = EDGE_CURVE ( 'NONE', #49448, #41714, #32094, .T. ) ;
#24970 = CARTESIAN_POINT ( 'NONE',  ( -13.49999999999997691, 73.00000000000001421, -205.0000000000000284 ) ) ;
#24971 = CARTESIAN_POINT ( 'NONE',  ( 10.00000000000000000, -17.80606268964516659, -33.00180498840066434 ) ) ;
#24972 = PLANE ( 'NONE',  #67576 ) ;
#24973 = CARTESIAN_POINT ( 'NONE',  ( 0.000000000000000000, -15.48615015657556171, -39.04073710021360455 ) ) ;
#24974 = DIRECTION ( 'NONE',  ( 0.000000000000000000, 0.000000000000000000, 1.000000000000000000 ) ) ;
#24975 = DIRECTION ( 'NONE',  ( 0.000000000000000000, -0.9781476007338065770, -0.2079116908177544853 ) ) ;
#24976 = FACE_OUTER_BOUND ( 'NONE', #50753, .T. ) ;
#24977 = CARTESIAN_POINT ( 'NONE',  ( -92.34999999999999432, -209.9999999999999716, 79.60187500173429953 ) ) ;
#24978 = CARTESIAN_POINT ( 'NONE',  ( 10.00000000000000000, 0.000000000000000000, 0.000000000000000000 ) ) ;
#24979 = ADVANCED_FACE ( 'NONE', ( #39118, #10531 ), #33456, .T. ) ;
#24981 = CARTESIAN_POINT ( 'NONE',  ( -93.67500000000003979, 87.70503267997129626, 75.68604166840097491 ) ) ;
#24980 = CARTESIAN_POINT ( 'NONE',  ( 94.99999999999998579, 93.05995642670504253, 77.22062500173429100 ) ) ;
#24982 = ORIENTED_EDGE ( 'NONE', *, *, #8442, .F. ) ;
#24983 = CARTESIAN_POINT ( 'NONE',  ( 92.69370383062498320, 91.33154071421968467, 77.04864583420048518 ) ) ;
#24984 = CARTESIAN_POINT ( 'NONE',  ( 6.000000000000000000, -81.50828551894234408, 8.966570791700414489 ) ) ;
#24985 = CARTESIAN_POINT ( 'NONE',  ( 6.782329983125267248, 10.49999999999999645, -105.0000000000000000 ) ) ;
#24986 = DIRECTION ( 'NONE',  ( -1.000000000000000000, 0.000000000000000000, 0.000000000000000000 ) ) ;
#24987 = CARTESIAN_POINT ( 'NONE',  ( 96.32499999999998863, -212.2949673200287179, 77.59104166840097605 ) ) ;
#24988 = ADVANCED_FACE ( 'NONE', ( #24057 ), #17663, .T. ) ;
#24989 = DIRECTION ( 'NONE',  ( -1.000000000000000000, -0.000000000000000000, 0.000000000000000000 ) ) ;
#24990 = ORIENTED_EDGE ( 'NONE', *, *, #52280, .F. ) ;
#24991 = CARTESIAN_POINT ( 'NONE',  ( 0.000000000000000000, -107.5000000000000000, -40.00000000000000711 ) ) ;
#24992 = CARTESIAN_POINT ( 'NONE',  ( -1.443735181952766622, 4.939961795957295898, -5.918341802876230240 ) ) ;
#24993 = VERTEX_POINT ( 'NONE', #69538 ) ;
#24994 = AXIS2_PLACEMENT_3D ( 'NONE', #55100, #25789, #72012 ) ;
#24995 = ORIENTED_EDGE ( 'NONE', *, *, #63794, .T. ) ;
#24996 = VECTOR ( 'NONE', #50469, 999.9999999999998863 ) ;
#24997 = AXIS2_PLACEMENT_3D ( 'NONE', #14388, #42239, #14007 ) ;
#24998 = CARTESIAN_POINT ( 'NONE',  ( 10.00000000000000000, -46.54456581323847786, 59.03342792756247093 ) ) ;
#24999 = CARTESIAN_POINT ( 'NONE',  ( 92.35000000000002274, -210.0000065184971163, 88.17437522718662990 ) ) ;
#25000 = CARTESIAN_POINT ( 'NONE',  ( -35.50000000000000711, -120.0000000000000000, 2.500000000000000000 ) ) ;
#25001 = DIRECTION ( 'NONE',  ( 0.000000000000000000, 0.000000000000000000, 1.000000000000000000 ) ) ;
#25002 = CARTESIAN_POINT ( 'NONE',  ( -96.15314808468747287, -208.0026889286704943, 75.09072916753380866 ) ) ;
#25003 = CIRCLE ( 'NONE', #47860, 0.5999999999999998668 ) ;
#25004 = VERTEX_POINT ( 'NONE', #59002 ) ;
#25005 = DIRECTION ( 'NONE',  ( 1.000000000000000000, 0.000000000000000000, 0.000000000000000000 ) ) ;
#25006 = LINE ( 'NONE', #1754, #29439 ) ;
#25007 = DIRECTION ( 'NONE',  ( -1.000000000000000000, 0.000000000000000000, -0.000000000000000000 ) ) ;
#25008 = CARTESIAN_POINT ( 'NONE',  ( 4.999999999999999112, -36.13751322684434797, 21.40280677340357940 ) ) ;
#25009 = CARTESIAN_POINT ( 'NONE',  ( -95.00000000000002842, 90.00000000000004263, 90.00000000000000000 ) ) ;
#25010 = DIRECTION ( 'NONE',  ( -1.000000000000000000, 0.000000000000000000, 0.000000000000000000 ) ) ;
#25011 = DIRECTION ( 'NONE',  ( 0.000000000000000000, -0.9781476007338041345, 0.2079116908177664480 ) ) ;
#25012 = CARTESIAN_POINT ( 'NONE',  ( -93.67499999999998295, -212.2949673200287179, 85.21104166840096639 ) ) ;
#25013 = CARTESIAN_POINT ( 'NONE',  ( -97.64999999999997726, -210.0000092897485899, 78.01437532303467037 ) ) ;
#25014 = DIRECTION ( 'NONE',  ( 1.000000000000000000, -0.000000000000000000, -0.000000000000000000 ) ) ;
#25015 = CARTESIAN_POINT ( 'NONE',  ( 92.69370383062498320, 91.33154071421968467, 83.39864583420049371 ) ) ;
#25016 = AXIS2_PLACEMENT_3D ( 'NONE', #8091, #23534, #53583 ) ;
#25017 = AXIS2_PLACEMENT_3D ( 'NONE', #24291, #41950, #18629 ) ;
#25018 = CARTESIAN_POINT ( 'NONE',  ( -93.84685191531248449, -208.0026889286704943, 87.68489583420048916 ) ) ;
#25019 = CARTESIAN_POINT ( 'NONE',  ( 10.00000000000000000, 74.65374052328660071, -8.840884882374309583 ) ) ;
#25020 = EDGE_LOOP ( 'NONE', ( #3371, #31580, #68801, #56902, #28771 ) ) ;
#25021 = CARTESIAN_POINT ( 'NONE',  ( 11.99999999999999822, 68.27212725128275395, -31.46837873495001503 ) ) ;
#25022 = CARTESIAN_POINT ( 'NONE',  ( -97.64999999999996305, -209.9999999999999716, 79.83999999999998920 ) ) ;
#25023 = EDGE_CURVE ( 'NONE', #11010, #33943, #38919, .T. ) ;
#25024 = CARTESIAN_POINT ( 'NONE',  ( -92.69370383062505425, 91.33154071421968467, 75.40822916753381833 ) ) ;
#25025 = AXIS2_PLACEMENT_3D ( 'NONE', #50048, #26393, #4969 ) ;
#25026 = ADVANCED_FACE ( 'NONE', ( #30405 ), #41335, .F. ) ;
#25027 = CIRCLE ( 'NONE', #45448, 42.00000000000000000 ) ;
#25028 = EDGE_CURVE ( 'NONE', #70067, #21866, #53717, .T. ) ;
#25029 = EDGE_CURVE ( 'NONE', #26516, #43747, #7856, .T. ) ;
#25030 = CARTESIAN_POINT ( 'NONE',  ( 95.00000000000000000, -212.6630814284392557, 85.99156250086714692 ) ) ;
#25031 = ORIENTED_EDGE ( 'NONE', *, *, #48628, .T. ) ;
#25032 = FACE_OUTER_BOUND ( 'NONE', #50222, .T. ) ;
#25033 = ORIENTED_EDGE ( 'NONE', *, *, #24639, .F. ) ;
#25034 = ORIENTED_EDGE ( 'NONE', *, *, #13143, .T. ) ;
#25035 = AXIS2_PLACEMENT_3D ( 'NONE', #62975, #10698, #51285 ) ;
#25036 = CARTESIAN_POINT ( 'NONE',  ( 95.00000000000000000, -206.9400435732949575, 84.12624999999999886 ) ) ;
#25037 = DIRECTION ( 'NONE',  ( -0.9227826878668540234, -0.3853207896976547642, 0.000000000000000000 ) ) ;
#25038 = CIRCLE ( 'NONE', #26216, 37.49900000000000944 ) ;
#25039 = ORIENTED_EDGE ( 'NONE', *, *, #65686, .T. ) ;
#25040 = EDGE_LOOP ( 'NONE', ( #14208, #65406, #38920, #66038 ) ) ;
#25041 = EDGE_CURVE ( 'NONE', #1142, #3906, #44996, .T. ) ;
#25042 = LINE ( 'NONE', #31419, #12024 ) ;
#25043 = AXIS2_PLACEMENT_3D ( 'NONE', #5354, #6094, #51186 ) ;
#25044 = CARTESIAN_POINT ( 'NONE',  ( 93.84685191531251292, -211.9973110713294489, 77.84239583420048803 ) ) ;
#25045 = DIRECTION ( 'NONE',  ( 0.000000000000000000, 0.000000000000000000, -1.000000000000000000 ) ) ;
#25046 = CARTESIAN_POINT ( 'NONE',  ( -92.35000000000005116, 91.52997821335253548, 76.47979166840096354 ) ) ;
#25047 = CIRCLE ( 'NONE', #14258, 31.99999999999999645 ) ;
#25048 = CYLINDRICAL_SURFACE ( 'NONE', #23263, 77.49899999999999523 ) ;
#25049 = CARTESIAN_POINT ( 'NONE',  ( 10.00000000000000000, 0.000000000000000000, 0.000000000000000000 ) ) ;
#25050 = DIRECTION ( 'NONE',  ( -1.000000000000000000, 0.000000000000000000, 0.000000000000000000 ) ) ;
#25051 = CARTESIAN_POINT ( 'NONE',  ( 97.64999999999999147, -209.9999999999999716, 83.33250000000001023 ) ) ;
#25052 = VERTEX_POINT ( 'NONE', #7495 ) ;
#25053 = ORIENTED_EDGE ( 'NONE', *, *, #27830, .T. ) ;
#25054 = ORIENTED_EDGE ( 'NONE', *, *, #7562, .F. ) ;
#25055 = ORIENTED_EDGE ( 'NONE', *, *, #20876, .T. ) ;
#25056 = CARTESIAN_POINT ( 'NONE',  ( -97.64999999980587120, -210.0000198427943587, 86.27002759516035724 ) ) ;
#25057 = EDGE_CURVE ( 'NONE', #766, #35203, #6752, .T. ) ;
#25058 = EDGE_CURVE ( 'NONE', #22781, #21262, #8964, .T. ) ;
#25059 = CARTESIAN_POINT ( 'NONE',  ( -93.84685191531252713, 88.00268892867056536, 84.93322916753382401 ) ) ;
#25060 = DIRECTION ( 'NONE',  ( 0.000000000000000000, 0.000000000000000000, 1.000000000000000000 ) ) ;
#25061 = CARTESIAN_POINT ( 'NONE',  ( -17.26469406256017791, -140.1601175325492648, -5.500000000000000000 ) ) ;
#25062 = PLANE ( 'NONE',  #41895 ) ;
#25063 = ORIENTED_EDGE ( 'NONE', *, *, #403, .F. ) ;
#25064 = AXIS2_PLACEMENT_3D ( 'NONE', #48654, #14435, #14803 ) ;
#25065 = CYLINDRICAL_SURFACE ( 'NONE', #40729, 12.49999999999999645 ) ;
#25066 = ORIENTED_EDGE ( 'NONE', *, *, #12819, .T. ) ;
#25067 = CARTESIAN_POINT ( 'NONE',  ( 0.000000000000000000, 30.41916302227216562, -71.27951684757994144 ) ) ;
#25068 = VERTEX_POINT ( 'NONE', #35327 ) ;
#25069 = CARTESIAN_POINT ( 'NONE',  ( -92.35000000000005116, 88.47002178664754979, 85.26395833506762756 ) ) ;
#25070 =( BOUNDED_CURVE ( )  B_SPLINE_CURVE ( 2, ( #322, #23215, #63441, #11910, #34854, #57794, #29195, #46503, #683 ),
 .UNSPECIFIED., .F., .F. ) 
 B_SPLINE_CURVE_WITH_KNOTS ( ( 3, 2, 2, 2, 3 ),
 ( 0.3810111478265181262, 0.3810113392076479033, 0.3880671047485306779, 0.3951228702894135081, 0.4021785743327794815 ),
 .UNSPECIFIED. ) 
 CURVE ( )  GEOMETRIC_REPRESENTATION_ITEM ( )  RATIONAL_B_SPLINE_CURVE ( ( 0.9999927323225317188, 0.9999963660626987050, 1.000000000000000000, 0.8660254037844387076, 1.000000000000000000, 0.8660254037844387076, 1.000000000000000000, 0.8660265714968488071, 0.9999976645955351851 ) ) 
 REPRESENTATION_ITEM ( '' )  );
#25071 = AXIS2_PLACEMENT_3D ( 'NONE', #8046, #53918, #8428 ) ;
#25072 = CARTESIAN_POINT ( 'NONE',  ( 97.30629616937498838, 90.00000000000002842, 85.67406250086715147 ) ) ;
#25073 = FACE_OUTER_BOUND ( 'NONE', #38602, .T. ) ;
#25074 = CIRCLE ( 'NONE', #35911, 16.00000000000000000 ) ;
#25075 = AXIS2_PLACEMENT_3D ( 'NONE', #70675, #19190, #48505 ) ;
#25076 = DIRECTION ( 'NONE',  ( 0.000000000000000000, 0.5224985647159440250, 0.8526401643540951758 ) ) ;
#25077 = CARTESIAN_POINT ( 'NONE',  ( -97.64998056384295921, -208.4700105651770627, 78.59645755884375262 ) ) ;
#25078 = CARTESIAN_POINT ( 'NONE',  ( -114.1267819554185365, -82.91796067500661138, -5.500000000000000000 ) ) ;
#25079 = EDGE_LOOP ( 'NONE', ( #31259, #1552, #17971, #40675 ) ) ;
#25080 = DIRECTION ( 'NONE',  ( -1.000000000000000000, 0.000000000000000000, 0.000000000000000000 ) ) ;
#25081 = CARTESIAN_POINT ( 'NONE',  ( -93.33921309982507353, -211.6002465100980316, 74.64190636928354650 ) ) ;
#25082 = VERTEX_POINT ( 'NONE', #1528 ) ;
#25083 = CIRCLE ( 'NONE', #1136, 77.49899999999999523 ) ;
#25084 = ORIENTED_EDGE ( 'NONE', *, *, #46082, .F. ) ;
#25085 = VECTOR ( 'NONE', #36120, 1000.000000000000000 ) ;
#25086 = CARTESIAN_POINT ( 'NONE',  ( 96.32499999999998863, 87.70503267997126784, 78.86104166840097207 ) ) ;
#25087 = DIRECTION ( 'NONE',  ( -1.000000000000000000, -0.000000000000000000, 0.000000000000000000 ) ) ;
#25088 = DIRECTION ( 'NONE',  ( 0.000000000000000000, -0.3826834323650772363, -0.9238795325112919565 ) ) ;
#25089 = CARTESIAN_POINT ( 'NONE',  ( -92.69370383062498320, -209.9999999999999716, 88.84906250086716284 ) ) ;
#25090 = ORIENTED_EDGE ( 'NONE', *, *, #33926, .F. ) ;
#25091 = DIRECTION ( 'NONE',  ( -0.000000000000000000, -0.000000000000000000, 1.000000000000000000 ) ) ;
#25092 = EDGE_LOOP ( 'NONE', ( #69164, #61586, #799, #33665 ) ) ;
#25093 = VECTOR ( 'NONE', #59495, 1000.000000000000000 ) ;
#25094 = AXIS2_PLACEMENT_3D ( 'NONE', #29688, #53019, #18782 ) ;
#25095 = ORIENTED_EDGE ( 'NONE', *, *, #61209, .F. ) ;
#25096 = DIRECTION ( 'NONE',  ( 0.000000000000000000, 0.000000000000000000, -1.000000000000000000 ) ) ;
#25097 = AXIS2_PLACEMENT_3D ( 'NONE', #14893, #70916, #9247 ) ;
#25098 = AXIS2_PLACEMENT_3D ( 'NONE', #62056, #10920, #69180 ) ;
#25099 = CARTESIAN_POINT ( 'NONE',  ( 94.99999999999998579, 87.33691857156068750, 89.32531250086715602 ) ) ;
#25100 = CARTESIAN_POINT ( 'NONE',  ( 97.64999999999999147, 89.99999990163419739, 80.23687499810812085 ) ) ;
#25101 = CARTESIAN_POINT ( 'NONE',  ( 92.69370383062498320, 88.66845928578035796, 82.71072916753378479 ) ) ;
#25102 = CARTESIAN_POINT ( 'NONE',  ( 0.000000000000000000, 15.48615015657637883, -39.04073710021327770 ) ) ;
#25103 = DIRECTION ( 'NONE',  ( 0.000000000000000000, 0.2334453638559060296, -0.9723699203976764460 ) ) ;
#25104 = DIRECTION ( 'NONE',  ( 0.000000000000000000, 0.7071067811865486830, -0.7071067811865463515 ) ) ;
#25105 = AXIS2_PLACEMENT_3D ( 'NONE', #2982, #14219, #58610 ) ;
#25106 = DIRECTION ( 'NONE',  ( 0.000000000000000000, 0.000000000000000000, -1.000000000000000000 ) ) ;
#25107 = AXIS2_PLACEMENT_3D ( 'NONE', #18454, #70683, #2700 ) ;
#25108 = CARTESIAN_POINT ( 'NONE',  ( 15.06715634359041900, 0.000000000000000000, 0.000000000000000000 ) ) ;
#25109 = CARTESIAN_POINT ( 'NONE',  ( 4.651285141665000289, 3.088081963278261011, -1.686035282245264444 ) ) ;
#25110 = DIRECTION ( 'NONE',  ( -1.000000000000000000, 0.000000000000000000, 0.000000000000000000 ) ) ;
#25111 = AXIS2_PLACEMENT_3D ( 'NONE', #45308, #45685, #57695 ) ;
#25112 = DIRECTION ( 'NONE',  ( -0.000000000000000000, -0.000000000000000000, 1.000000000000000000 ) ) ;
#25113 = PRODUCT_DEFINITION_CONTEXT ( 'detailed design', #43164, 'design' ) ;
#25114 = EDGE_CURVE ( 'NONE', #5572, #40918, #1890, .T. ) ;
#25115 = DIRECTION ( 'NONE',  ( 0.9918136447140100120, -0.1276937514489704939, 0.000000000000000000 ) ) ;
#25116 = ORIENTED_EDGE ( 'NONE', *, *, #41534, .F. ) ;
#25117 = EDGE_CURVE ( 'NONE', #20003, #3283, #585, .T. ) ;
#25118 = CARTESIAN_POINT ( 'NONE',  ( -95.00000000000002842, 87.33691857156074434, 87.89656250086713385 ) ) ;
#25119 = DIRECTION ( 'NONE',  ( 0.8541291221503275466, -0.5200609990132993854, 0.000000000000000000 ) ) ;
#25120 = ADVANCED_FACE ( 'NONE', ( #1160 ), #58256, .F. ) ;
#25121 = EDGE_CURVE ( 'NONE', #28563, #11928, #42082, .T. ) ;
#25122 = AXIS2_PLACEMENT_3D ( 'NONE', #64753, #1999, #47095 ) ;
#25123 = CARTESIAN_POINT ( 'NONE',  ( -2.410829926157000802E-12, -120.0000000000000000, 127.5000000000000000 ) ) ;
#25124 = ORIENTED_EDGE ( 'NONE', *, *, #6366, .T. ) ;
#25125 = EDGE_CURVE ( 'NONE', #28680, #31033, #4153, .T. ) ;
#25127 = LINE ( 'NONE', #65359, #21043 ) ;
#25126 = VECTOR ( 'NONE', #28309, 1000.000000000000000 ) ;
#25128 = CARTESIAN_POINT ( 'NONE',  ( 10.00000000000000000, 0.000000000000000000, 0.000000000000000000 ) ) ;
#25129 = DIRECTION ( 'NONE',  ( -1.000000000000000000, 0.000000000000000000, 0.000000000000000000 ) ) ;
#25130 = CIRCLE ( 'NONE', #19109, 16.00000000000000000 ) ;
#25131 = AXIS2_PLACEMENT_3D ( 'NONE', #27322, #50258, #21693 ) ;
#25132 = AXIS2_PLACEMENT_3D ( 'NONE', #48308, #14463, #42671 ) ;
#25133 = CARTESIAN_POINT ( 'NONE',  ( 97.30629616937498838, -209.9999999999999716, 81.22906250086715829 ) ) ;
#25134 = AXIS2_PLACEMENT_3D ( 'NONE', #49149, #21298, #2952 ) ;
#25135 = ORIENTED_EDGE ( 'NONE', *, *, #1316, .F. ) ;
#25136 = ORIENTED_EDGE ( 'NONE', *, *, #59449, .T. ) ;
#25137 = EDGE_CURVE ( 'NONE', #40132, #68971, #39806, .T. ) ;
#25138 = EDGE_CURVE ( 'NONE', #59175, #40539, #65382, .T. ) ;
#25139 = PLANE ( 'NONE',  #48811 ) ;
#25140 = ORIENTED_EDGE ( 'NONE', *, *, #52782, .F. ) ;
#25141 = CARTESIAN_POINT ( 'NONE',  ( 10.00000000000000000, -74.65374052328654386, 8.840884882374837161 ) ) ;
#25142 = DIRECTION ( 'NONE',  ( -1.000000000000000000, -0.000000000000000000, 0.000000000000000000 ) ) ;
#25143 = ORIENTED_EDGE ( 'NONE', *, *, #26321, .F. ) ;
#25144 = CARTESIAN_POINT ( 'NONE',  ( 95.00000000000000000, -207.3369185715606307, 79.48281250086715488 ) ) ;
#25145 = VECTOR ( 'NONE', #28498, 1000.000000000000000 ) ;
#25146 = VERTEX_POINT ( 'NONE', #34959 ) ;
#25147 = DIRECTION ( 'NONE',  ( -0.000000000000000000, 0.000000000000000000, 1.000000000000000000 ) ) ;
#25148 = ORIENTED_EDGE ( 'NONE', *, *, #7664, .T. ) ;
#25149 = ORIENTED_EDGE ( 'NONE', *, *, #4899, .T. ) ;
#25150 = CARTESIAN_POINT ( 'NONE',  ( -25.00516449930816876, -111.2255058058861010, -2.500000000000000000 ) ) ;
#25151 = EDGE_CURVE ( 'NONE', #11217, #72850, #48814, .T. ) ;
#25152 = EDGE_CURVE ( 'NONE', #39781, #70065, #23365, .T. ) ;
#25153 = AXIS2_PLACEMENT_3D ( 'NONE', #66857, #15728, #14233 ) ;
#25154 = SHAPE_REPRESENTATION_RELATIONSHIP ( 'NONE' , 'NONE' ,  #49787, #40864 ) ;
#25155 = DIRECTION ( 'NONE',  ( 0.000000000000000000, 0.000000000000000000, 1.000000000000000000 ) ) ;
#25156 = AXIS2_PLACEMENT_3D ( 'NONE', #13307, #11187, #34117 ) ;
#25157 = ORIENTED_EDGE ( 'NONE', *, *, #48042, .F. ) ;
#25158 = CARTESIAN_POINT ( 'NONE',  ( 0.000000000000000000, 0.000000000000000000, -270.0000000000000000 ) ) ;
#25159 = CARTESIAN_POINT ( 'NONE',  ( 96.32499999999998863, -212.2949673200287179, 84.57604166840096127 ) ) ;
#25160 = CARTESIAN_POINT ( 'NONE',  ( 93.67499999999998295, 92.29496732002878900, 86.08416666666666117 ) ) ;
#25161 = VERTEX_POINT ( 'NONE', #66852 ) ;
#25162 = DIRECTION ( 'NONE',  ( -1.000000000000000000, -0.000000000000000000, 0.000000000000000000 ) ) ;
#25163 = LINE ( 'NONE', #69898, #34491 ) ;
#25164 = ORIENTED_EDGE ( 'NONE', *, *, #13890, .T. ) ;
#25165 = EDGE_LOOP ( 'NONE', ( #42822, #44489, #48945, #37122, #37127, #56330 ) ) ;
#25166 = CARTESIAN_POINT ( 'NONE',  ( -92.69370383062505425, 91.33154071421968467, 87.63197916753381378 ) ) ;
#25167 = CARTESIAN_POINT ( 'NONE',  ( 96.15314808468748708, 88.00268892867053694, 81.59947916753381492 ) ) ;
#25168 = ORIENTED_EDGE ( 'NONE', *, *, #21533, .T. ) ;
#25169 = CARTESIAN_POINT ( 'NONE',  ( 93.67499999999998295, 92.29496732002878900, 86.16354166840096696 ) ) ;
#25170 = VERTEX_POINT ( 'NONE', #48446 ) ;
#25171 = CARTESIAN_POINT ( 'NONE',  ( -89.17737905728745318, -39.70432723693717492, -5.500000000000000000 ) ) ;
#25172 = ORIENTED_EDGE ( 'NONE', *, *, #31795, .T. ) ;
#25173 = ORIENTED_EDGE ( 'NONE', *, *, #18379, .T. ) ;
#25174 = ORIENTED_EDGE ( 'NONE', *, *, #28244, .F. ) ;
#25175 = CARTESIAN_POINT ( 'NONE',  ( 15.00000000000000000, 23.49999999999999645, 1.499999999999995337 ) ) ;
#25176 = DIRECTION ( 'NONE',  ( 0.000000000000000000, -0.8660254037844387076, -0.4999999999999998335 ) ) ;
#25177 = CARTESIAN_POINT ( 'NONE',  ( -93.67500000000003979, 92.29496732002878900, 83.43833333333333258 ) ) ;
#25178 = ORIENTED_EDGE ( 'NONE', *, *, #16916, .F. ) ;
#25179 = DIRECTION ( 'NONE',  ( 0.000000000000000000, 0.000000000000000000, -1.000000000000000000 ) ) ;
#25180 = CARTESIAN_POINT ( 'NONE',  ( 10.00000000000000000, 59.03961581697399907, 46.53671651293969802 ) ) ;
#25181 = EDGE_LOOP ( 'NONE', ( #58811, #32714, #22841, #63309 ) ) ;
#25182 = CARTESIAN_POINT ( 'NONE',  ( 11.59999999999999787, 1.420590287010929336E-15, -56.19999999999998863 ) ) ;
#25183 = CARTESIAN_POINT ( 'NONE',  ( -97.30629616937497417, -208.6684592857803011, 81.96989583420048575 ) ) ;
#25184 = ORIENTED_EDGE ( 'NONE', *, *, #13259, .F. ) ;
#25185 = AXIS2_PLACEMENT_3D ( 'NONE', #37579, #8995, #3379 ) ;
#25186 = CARTESIAN_POINT ( 'NONE',  ( -92.35000000000003695, 90.00000000000004263, 82.69749999999999091 ) ) ;
#25187 = DIRECTION ( 'NONE',  ( 0.000000000000000000, 0.000000000000000000, -1.000000000000000000 ) ) ;
#25188 = DIRECTION ( 'NONE',  ( 0.000000000000000000, 0.000000000000000000, 1.000000000000000000 ) ) ;
#25189 = CARTESIAN_POINT ( 'NONE',  ( -97.30629616937495996, -209.9999999999999716, 89.64281250086713726 ) ) ;
#25190 = EDGE_CURVE ( 'NONE', #20602, #74032, #73784, .T. ) ;
#25191 = VECTOR ( 'NONE', #9493, 1000.000000000000000 ) ;
#25192 = AXIS2_PLACEMENT_3D ( 'NONE', #52757, #35096, #47125 ) ;
#25193 = FACE_OUTER_BOUND ( 'NONE', #47030, .T. ) ;
#25195 = AXIS2_PLACEMENT_3D ( 'NONE', #21953, #12426, #61819 ) ;
#25194 = DIRECTION ( 'NONE',  ( 0.000000000000000000, -1.000000000000000000, 0.000000000000000000 ) ) ;
#25196 = ADVANCED_FACE ( 'NONE', ( #13851 ), #20621, .F. ) ;
#25197 = DIRECTION ( 'NONE',  ( -1.000000000000000000, -1.427937372958405461E-15, -7.962523111839130290E-16 ) ) ;
#25198 = CARTESIAN_POINT ( 'NONE',  ( 5.822613034544236399, -142.8165987265839760, 5.500000000000000000 ) ) ;
#25199 = EDGE_CURVE ( 'NONE', #69818, #13377, #59738, .T. ) ;
#25200 = LINE ( 'NONE', #2303, #33235 ) ;
#25201 = CARTESIAN_POINT ( 'NONE',  ( -97.30629616937501680, 91.33154071421968467, 89.74864583420048803 ) ) ;
#25202 = DIRECTION ( 'NONE',  ( 0.000000000000000000, 0.000000000000000000, -1.000000000000000000 ) ) ;
#25203 = DIRECTION ( 'NONE',  ( -0.9827303690289279636, -0.1850432970638682117, 0.000000000000000000 ) ) ;
#25204 = EDGE_CURVE ( 'NONE', #59498, #17376, #15337, .T. ) ;
#25205 = DIRECTION ( 'NONE',  ( -1.000000000000000000, -0.000000000000000000, -0.000000000000000000 ) ) ;
#25206 = EDGE_CURVE ( 'NONE', #16727, #1777, #46175, .T. ) ;
#25207 = CIRCLE ( 'NONE', #16790, 31.99999999999999289 ) ;
#25208 = AXIS2_PLACEMENT_3D ( 'NONE', #1855, #46568, #19464 ) ;
#25209 = CARTESIAN_POINT ( 'NONE',  ( -96.32499999999996021, -212.2949673200287179, 84.47020833506762472 ) ) ;
#25211 = FACE_OUTER_BOUND ( 'NONE', #44270, .T. ) ;
#25210 = CIRCLE ( 'NONE', #33627, 31.99999999999999289 ) ;
#25212 = AXIS2_PLACEMENT_3D ( 'NONE', #37407, #9557, #2844 ) ;
#25213 = CARTESIAN_POINT ( 'NONE',  ( 97.64999999999993463, -211.5299782133524786, 77.56458333333333144 ) ) ;
#25214 = DIRECTION ( 'NONE',  ( -1.000000000000000000, -0.000000000000000000, -0.000000000000000000 ) ) ;
#25215 = EDGE_CURVE ( 'NONE', #67909, #22221, #59363, .T. ) ;
#25216 = FACE_OUTER_BOUND ( 'NONE', #34801, .T. ) ;
#25217 = CARTESIAN_POINT ( 'NONE',  ( -96.32499999999996021, -212.2949673200287179, 86.93083333333332519 ) ) ;
#25218 = CIRCLE ( 'NONE', #3666, 5.000000000000000888 ) ;
#25219 = VECTOR ( 'NONE', #65725, 1000.000000000000000 ) ;
#25220 = CARTESIAN_POINT ( 'NONE',  ( 10.00000000000000000, -59.03961581697367933, -46.53671651294010303 ) ) ;
#25221 = ORIENTED_EDGE ( 'NONE', *, *, #9424, .F. ) ;
#25222 = ADVANCED_FACE ( 'NONE', ( #66128 ), #71361, .F. ) ;
#25223 = CYLINDRICAL_SURFACE ( 'NONE', #41965, 13.90444123027096879 ) ;
#25224 = DIRECTION ( 'NONE',  ( 1.000000000000000000, -0.000000000000000000, 0.000000000000000000 ) ) ;
#25225 = CARTESIAN_POINT ( 'NONE',  ( 11.99999999999999822, 71.91182617369190666, 28.89263327155770966 ) ) ;
#25226 = VERTEX_POINT ( 'NONE', #42816 ) ;
#25227 = EDGE_CURVE ( 'NONE', #42699, #37771, #64212, .T. ) ;
#25228 = CARTESIAN_POINT ( 'NONE',  ( 4.999999999999999112, -41.81611651403864727, 3.925862922256025289 ) ) ;
#25229 = EDGE_CURVE ( 'NONE', #12729, #32190, #32944, .T. ) ;
#25230 = CARTESIAN_POINT ( 'NONE',  ( 0.000000000000000000, -2.956366410620109519, -75.11725578898472122 ) ) ;
#25231 = ORIENTED_EDGE ( 'NONE', *, *, #10078, .F. ) ;
#25232 = CIRCLE ( 'NONE', #47872, 82.00000000000000000 ) ;
#25233 = CARTESIAN_POINT ( 'NONE',  ( 92.69370383062501162, -211.3315407142195852, 82.71072916753378479 ) ) ;
#25234 = CARTESIAN_POINT ( 'NONE',  ( 10.00000000000000000, 0.000000000000000000, 0.000000000000000000 ) ) ;
#25235 = EDGE_CURVE ( 'NONE', #63232, #53287, #14975, .T. ) ;
#25236 = ORIENTED_EDGE ( 'NONE', *, *, #62246, .T. ) ;
#25237 = CARTESIAN_POINT ( 'NONE',  ( 95.00000000000000000, -212.6630814284392557, 88.69031250086716511 ) ) ;
#25238 = AXIS2_PLACEMENT_3D ( 'NONE', #56171, #51263, #50525 ) ;
#25239 = ORIENTED_EDGE ( 'NONE', *, *, #46423, .F. ) ;
#25240 = CARTESIAN_POINT ( 'NONE',  ( -97.65000000000003411, -211.5299782133524502, 80.52791666666665549 ) ) ;
#25241 = ORIENTED_EDGE ( 'NONE', *, *, #56544, .T. ) ;
#25242 = AXIS2_PLACEMENT_3D ( 'NONE', #50244, #37136, #9663 ) ;
#25243 = CARTESIAN_POINT ( 'NONE',  ( -97.30629616937501680, 91.33154071421968467, 76.41364583420049428 ) ) ;
#25244 = ORIENTED_EDGE ( 'NONE', *, *, #29877, .T. ) ;
#25245 = EDGE_LOOP ( 'NONE', ( #12371, #16875, #36879, #14974 ) ) ;
#25246 = AXIS2_PLACEMENT_3D ( 'NONE', #15353, #9344, #36805 ) ;
#25247 = CARTESIAN_POINT ( 'NONE',  ( 11.99999999999999822, 50.95692526931414790, -58.39081064771693974 ) ) ;
#25248 = ORIENTED_EDGE ( 'NONE', *, *, #50052, .F. ) ;
#25249 = DIRECTION ( 'NONE',  ( 0.000000000000000000, 0.000000000000000000, -1.000000000000000000 ) ) ;
#25250 = DIRECTION ( 'NONE',  ( -1.000000000000000000, 0.000000000000000000, 0.000000000000000000 ) ) ;
#25251 = ORIENTED_EDGE ( 'NONE', *, *, #69707, .F. ) ;
#25252 = LINE ( 'NONE', #18852, #43041 ) ;
#25253 = ORIENTED_EDGE ( 'NONE', *, *, #67536, .F. ) ;
#25254 = DIRECTION ( 'NONE',  ( 0.000000000000000000, 0.7431448254773939111, 0.6691306063588584596 ) ) ;
#25255 = ORIENTED_EDGE ( 'NONE', *, *, #24694, .T. ) ;
#25256 = AXIS2_PLACEMENT_3D ( 'NONE', #54956, #9095, #55329 ) ;
#25257 = ORIENTED_EDGE ( 'NONE', *, *, #45355, .T. ) ;
#25258 = EDGE_LOOP ( 'NONE', ( #16160, #14981, #15744, #16063 ) ) ;
#25259 = AXIS2_PLACEMENT_3D ( 'NONE', #34178, #74020, #16145 ) ;
#25260 = CARTESIAN_POINT ( 'NONE',  ( 92.69370383062501162, -209.9999999999999716, 78.84781250086714977 ) ) ;
#25261 = AXIS2_PLACEMENT_3D ( 'NONE', #19888, #1546, #36811 ) ;
#25262 = CARTESIAN_POINT ( 'NONE',  ( -20.30386590532152979, -102.9045904027214959, 5.500000000000000000 ) ) ;
#25263 = DIRECTION ( 'NONE',  ( 1.000000000000000000, 0.000000000000000000, 0.000000000000000000 ) ) ;
#25264 = ORIENTED_EDGE ( 'NONE', *, *, #15039, .T. ) ;
#25265 = CARTESIAN_POINT ( 'NONE',  ( -97.64999999999994884, -209.9999831677324664, 78.64937441956425346 ) ) ;
#25266 = DIRECTION ( 'NONE',  ( -1.000000000000000000, -0.000000000000000000, 0.000000000000000000 ) ) ;
#25267 = CARTESIAN_POINT ( 'NONE',  ( 10.00000000000000000, 0.000000000000000000, 0.000000000000000000 ) ) ;
#25268 = CYLINDRICAL_SURFACE ( 'NONE', #66107, 77.49899999999999523 ) ;
#25269 = DIRECTION ( 'NONE',  ( 0.000000000000000000, 0.000000000000000000, 1.000000000000000000 ) ) ;
#25270 = CIRCLE ( 'NONE', #67285, 31.99999999999998224 ) ;
#25271 = CARTESIAN_POINT ( 'NONE',  ( -96.15314808468745866, -211.9973110713294489, 82.12864583420046927 ) ) ;
#25272 = CARTESIAN_POINT ( 'NONE',  ( -92.69370383062502583, 91.33154071421968467, 80.01197916753380923 ) ) ;
#25273 = EDGE_CURVE ( 'NONE', #28106, #29672, #10141, .T. ) ;
#25274 = ORIENTED_EDGE ( 'NONE', *, *, #62059, .F. ) ;
#25275 = CARTESIAN_POINT ( 'NONE',  ( 93.84685191531248449, 88.00268892867053694, 79.58864583420047722 ) ) ;
#25276 = EDGE_LOOP ( 'NONE', ( #41520, #72905, #44430, #27436 ) ) ;
#25277 = CARTESIAN_POINT ( 'NONE',  ( 94.99999999999998579, 93.05995642670504253, 78.49062500173430124 ) ) ;
#25278 = CARTESIAN_POINT ( 'NONE',  ( -23.54415474984308787, -120.4156646670583086, 5.500000000000000000 ) ) ;
#25279 = CARTESIAN_POINT ( 'NONE',  ( -93.67499999999998295, -212.2949673200287179, 83.30604166840096525 ) ) ;
#25280 = PLANE ( 'NONE',  #49966 ) ;
#25281 = DIRECTION ( 'NONE',  ( 0.000000000000000000, 0.000000000000000000, 1.000000000000000000 ) ) ;
#25282 = CARTESIAN_POINT ( 'NONE',  ( -97.30629616937497417, -208.6684592857803295, 83.87489583420047268 ) ) ;
#25283 = LINE ( 'NONE', #53845, #39864 ) ;
#25284 = LINE ( 'NONE', #66968, #52302 ) ;
#25285 = DIRECTION ( 'NONE',  ( -1.000000000000000000, 0.000000000000000000, 0.000000000000000000 ) ) ;
#25286 = ORIENTED_EDGE ( 'NONE', *, *, #10864, .T. ) ;
#25287 = EDGE_LOOP ( 'NONE', ( #61846, #22872, #35671, #42833 ) ) ;
#25288 = FACE_OUTER_BOUND ( 'NONE', #1184, .T. ) ;
#25289 = EDGE_CURVE ( 'NONE', #43284, #70987, #24539, .T. ) ;
#25290 = CARTESIAN_POINT ( 'NONE',  ( -95.84368202074679743, 85.30516711421526566, 74.84535815546854565 ) ) ;
#25291 = EDGE_CURVE ( 'NONE', #5465, #20634, #30534, .T. ) ;
#25292 = DIRECTION ( 'NONE',  ( 0.000000000000000000, 0.000000000000000000, 1.000000000000000000 ) ) ;
#25293 = CARTESIAN_POINT ( 'NONE',  ( -93.84685191531254134, 91.99731107132950569, 86.89114583420047211 ) ) ;
#25294 = CARTESIAN_POINT ( 'NONE',  ( -97.51367041768831712, -210.0000000000000284, 74.91808492278045151 ) ) ;
#25295 = CARTESIAN_POINT ( 'NONE',  ( 10.00000000000000000, 21.53537804866126137, -30.80686688396986028 ) ) ;
#25296 = DIRECTION ( 'NONE',  ( -1.000000000000000000, 0.000000000000000000, 0.000000000000000000 ) ) ;
#25297 = EDGE_LOOP ( 'NONE', ( #33471, #25095, #13213, #39976 ) ) ;
#25298 = CARTESIAN_POINT ( 'NONE',  ( -93.84685191531252713, 88.00268892867056536, 75.24947916753380639 ) ) ;
#25299 = EDGE_CURVE ( 'NONE', #5973, #17422, #61227, .T. ) ;
#25300 = EDGE_CURVE ( 'NONE', #71848, #67219, #48084, .T. ) ;
#25301 = AXIS2_PLACEMENT_3D ( 'NONE', #46563, #74012, #4887 ) ;
#25302 = DIRECTION ( 'NONE',  ( 9.814797785686868941E-17, -1.000000000000000000, 0.000000000000000000 ) ) ;
#25303 = FACE_BOUND ( 'NONE', #14566, .T. ) ;
#25304 = CARTESIAN_POINT ( 'NONE',  ( 3.429551818649054340, -146.3199197248623875, -2.500000000000000444 ) ) ;
#25305 = CARTESIAN_POINT ( 'NONE',  ( 0.000000000000000000, 0.000000000000000000, -105.0000000000000000 ) ) ;
#25306 = DIRECTION ( 'NONE',  ( -1.000000000000000000, 0.000000000000000000, -0.000000000000000000 ) ) ;
#25307 = CARTESIAN_POINT ( 'NONE',  ( -92.69370383062498320, -211.3315407142195852, 83.71614583420050337 ) ) ;
#25308 = DIRECTION ( 'NONE',  ( -1.000000000000000000, -0.000000000000000000, -0.000000000000000000 ) ) ;
#25309 =( BOUNDED_CURVE ( )  B_SPLINE_CURVE ( 2, ( #44840, #16627, #68131, #21510, #15135, #72636, #38821 ),
 .UNSPECIFIED., .F., .F. ) 
 B_SPLINE_CURVE_WITH_KNOTS ( ( 3, 2, 2, 3 ),
 ( 0.7916666666666669627, 0.7986111111111114935, 0.8055555555555558023, 0.8125000000000002220 ),
 .UNSPECIFIED. ) 
 CURVE ( )  GEOMETRIC_REPRESENTATION_ITEM ( )  RATIONAL_B_SPLINE_CURVE ( ( 0.9999999999999935607, 0.8660254037844451469, 1.000000000000000000, 0.8660254037844387076, 1.000000000000000000, 0.8660254037844343777, 1.000000000000004219 ) ) 
 REPRESENTATION_ITEM ( '' )  );
#25310 = EDGE_CURVE ( 'NONE', #26473, #46616, #54830, .T. ) ;
#25311 = CARTESIAN_POINT ( 'NONE',  ( 12.00000000000000355, 2.571758278209441661E-15, -21.00000000000000000 ) ) ;
#25312 = CARTESIAN_POINT ( 'NONE',  ( -97.30629616937495996, -209.9999999999999716, 75.83156250086716454 ) ) ;
#25313 = CIRCLE ( 'NONE', #133, 12.50000000000000000 ) ;
#25314 = ORIENTED_EDGE ( 'NONE', *, *, #7165, .T. ) ;
#25315 = FACE_OUTER_BOUND ( 'NONE', #49360, .T. ) ;
#25316 = CARTESIAN_POINT ( 'NONE',  ( 0.000000000000000000, 0.000000000000000000, 0.000000000000000000 ) ) ;
#25317 = CYLINDRICAL_SURFACE ( 'NONE', #49810, 82.00000000000000000 ) ;
#25318 = VECTOR ( 'NONE', #35532, 1000.000000000000000 ) ;
#25319 = AXIS2_PLACEMENT_3D ( 'NONE', #49943, #10852, #56732 ) ;
#25320 = VECTOR ( 'NONE', #52950, 1000.000000000000000 ) ;
#25321 = CYLINDRICAL_SURFACE ( 'NONE', #33690, 42.00000000000000000 ) ;
#25322 = CARTESIAN_POINT ( 'NONE',  ( 96.15314808468748708, -208.0026889286704943, 74.82614583420047438 ) ) ;
#25323 = VERTEX_POINT ( 'NONE', #42447 ) ;
#25324 = ADVANCED_FACE ( 'NONE', ( #26248 ), #21338, .T. ) ;
#25325 = EDGE_CURVE ( 'NONE', #44494, #52144, #47486, .T. ) ;
#25326 = DIRECTION ( 'NONE',  ( -1.000000000000000000, 0.000000000000000000, 0.000000000000000000 ) ) ;
#25327 = FILL_AREA_STYLE ('',( #59915 ) ) ;
#25328 = VERTEX_POINT ( 'NONE', #62727 ) ;
#25329 = DIRECTION ( 'NONE',  ( 0.000000000000000000, 0.000000000000000000, 1.000000000000000000 ) ) ;
#25330 = EDGE_CURVE ( 'NONE', #67207, #33925, #39401, .T. ) ;
#25331 = ORIENTED_EDGE ( 'NONE', *, *, #57576, .F. ) ;
#25332 = DIRECTION ( 'NONE',  ( 0.000000000000000000, 0.7071067811865489050, -0.7071067811865462405 ) ) ;
#25333 = VERTEX_POINT ( 'NONE', #4842 ) ;
#25334 = ORIENTED_EDGE ( 'NONE', *, *, #24955, .T. ) ;
#25335 = ORIENTED_EDGE ( 'NONE', *, *, #34857, .F. ) ;
#25336 = FACE_OUTER_BOUND ( 'NONE', #62435, .T. ) ;
#25337 = ORIENTED_EDGE ( 'NONE', *, *, #4705, .F. ) ;
#25338 = PRODUCT_DEFINITION_SHAPE ( 'NONE', 'NONE',  #74343 ) ;
#25339 = EDGE_LOOP ( 'NONE', ( #8466, #9796, #51353, #24312 ) ) ;
#25340 = CARTESIAN_POINT ( 'NONE',  ( 97.30629616937498838, 91.33154071421968467, 81.28197916753381946 ) ) ;
#25341 = FACE_BOUND ( 'NONE', #19211, .T. ) ;
#25342 = CARTESIAN_POINT ( 'NONE',  ( -95.00000000000002842, 86.94004357329504273, 85.07875000000001364 ) ) ;
#25343 = ORIENTED_EDGE ( 'NONE', *, *, #54013, .T. ) ;
#25344 = ORIENTED_EDGE ( 'NONE', *, *, #47763, .T. ) ;
#25345 = AXIS2_PLACEMENT_3D ( 'NONE', #44635, #28059, #33706 ) ;
#25346 = VECTOR ( 'NONE', #9174, 1000.000000000000000 ) ;
#25347 = ORIENTED_EDGE ( 'NONE', *, *, #45618, .F. ) ;
#25348 = DIRECTION ( 'NONE',  ( -0.9580045777625456616, -0.2867529058022021404, 0.000000000000000000 ) ) ;
#25349 = EDGE_LOOP ( 'NONE', ( #22963, #67230, #57829, #36537 ) ) ;
#25350 = DIRECTION ( 'NONE',  ( 0.000000000000000000, 0.000000000000000000, 0.9999999999999998890 ) ) ;
#25351 = CARTESIAN_POINT ( 'NONE',  ( 0.000000000000000000, -80.55351364060578589, -15.33399622253568673 ) ) ;
#25352 = CARTESIAN_POINT ( 'NONE',  ( -94.70223316839030758, 92.36156954995054491, 74.83035915144986916 ) ) ;
#25353 = FACE_OUTER_BOUND ( 'NONE', #32700, .T. ) ;
#25354 = FACE_OUTER_BOUND ( 'NONE', #34458, .T. ) ;
#25355 = CARTESIAN_POINT ( 'NONE',  ( -35.37301231164799731, -123.0000000000000142, 2.500000000000000000 ) ) ;
#25356 = LINE ( 'NONE', #3557, #32406 ) ;
#25357 = CARTESIAN_POINT ( 'NONE',  ( -97.64999999999994884, -211.5299782133524502, 74.89229166840097207 ) ) ;
#25358 = CARTESIAN_POINT ( 'NONE',  ( -97.30629616937501680, 91.33154071421968467, 88.47864583420047779 ) ) ;
#25359 =( REPRESENTATION_RELATIONSHIP ('NONE','NONE', #31117, #42128 ) REPRESENTATION_RELATIONSHIP_WITH_TRANSFORMATION ( #33468 )SHAPE_REPRESENTATION_RELATIONSHIP( ) );
#25360 = ADVANCED_FACE ( 'NONE', ( #73594 ), #22482, .T. ) ;
#25362 = CARTESIAN_POINT ( 'NONE',  ( -93.67500000000003979, 87.70503267997129626, 76.95604166840095672 ) ) ;
#25361 = CARTESIAN_POINT ( 'NONE',  ( 92.34999999999999432, 91.52997821335252127, 75.42145833506764063 ) ) ;
#25363 = ORIENTED_EDGE ( 'NONE', *, *, #72624, .T. ) ;
#25364 = CARTESIAN_POINT ( 'NONE',  ( 96.15314808468748708, 91.99731107132950569, 76.88989583420048746 ) ) ;
#25365 = FACE_OUTER_BOUND ( 'NONE', #30633, .T. ) ;
#25366 = FACE_OUTER_BOUND ( 'NONE', #28378, .T. ) ;
#25367 = FACE_OUTER_BOUND ( 'NONE', #11632, .T. ) ;
#25368 = DIRECTION ( 'NONE',  ( 1.000000000000000000, -0.000000000000000000, -0.000000000000000000 ) ) ;
#25369 = AXIS2_PLACEMENT_3D ( 'NONE', #10869, #6349, #39443 ) ;
#25370 = CARTESIAN_POINT ( 'NONE',  ( 0.000000000000000000, 0.000000000000000000, 0.000000000000000000 ) ) ;
#25371 = ORIENTED_EDGE ( 'NONE', *, *, #37881, .T. ) ;
#25372 = DIRECTION ( 'NONE',  ( 0.000000000000000000, -0.5877852522924624790, -0.8090169943749552228 ) ) ;
#25373 = AXIS2_PLACEMENT_3D ( 'NONE', #24535, #3113, #26007 ) ;
#25374 = DIRECTION ( 'NONE',  ( 0.000000000000000000, 0.000000000000000000, -1.000000000000000000 ) ) ;
#25375 = ORIENTED_EDGE ( 'NONE', *, *, #3955, .T. ) ;
#25376 = ADVANCED_FACE ( 'NONE', ( #68351 ), #56848, .T. ) ;
#25377 = AXIS2_PLACEMENT_3D ( 'NONE', #41633, #64571, #52173 ) ;
#25378 = ORIENTED_EDGE ( 'NONE', *, *, #72649, .F. ) ;
#25379 = CIRCLE ( 'NONE', #67380, 12.79999999999999893 ) ;
#25380 = EDGE_CURVE ( 'NONE', #69749, #52333, #5399, .T. ) ;
#25381 = DIRECTION ( 'NONE',  ( 0.1276937514489679681, 0.9918136447140103451, 0.000000000000000000 ) ) ;
#25382 = CARTESIAN_POINT ( 'NONE',  ( -3.000000000000000000, -1.278221433540502217, 26.51162292216071847 ) ) ;
#25383 = FACE_OUTER_BOUND ( 'NONE', #34417, .T. ) ;
#25384 = DIRECTION ( 'NONE',  ( 0.000000000000000000, 0.000000000000000000, 1.000000000000000000 ) ) ;
#25385 = DIRECTION ( 'NONE',  ( 0.000000000000000000, 0.000000000000000000, 1.000000000000000000 ) ) ;
#25386 = CARTESIAN_POINT ( 'NONE',  ( 10.00000000000000000, 3.894527615419054456, -81.90746397400386059 ) ) ;
#25387 = ORIENTED_EDGE ( 'NONE', *, *, #15339, .T. ) ;
#25388 = ADVANCED_FACE ( 'NONE', ( #45045 ), #32998, .F. ) ;
#25389 = CYLINDRICAL_SURFACE ( 'NONE', #24716, 12.50000000000022560 ) ;
#25390 = LINE ( 'NONE', #14087, #64296 ) ;
#25391 = CARTESIAN_POINT ( 'NONE',  ( -7.572224309238338336, -145.4393675041377492, -5.500000000000000000 ) ) ;
#25392 = CARTESIAN_POINT ( 'NONE',  ( 10.00000000000000000, 49.70050353004977239, -59.46389618801908483 ) ) ;
#25393 = CARTESIAN_POINT ( 'NONE',  ( 10.00000000000000000, 63.97538442413425486, 51.29473840253247374 ) ) ;
#25394 = DIRECTION ( 'NONE',  ( -1.000000000000000000, 0.000000000000000000, -0.000000000000000000 ) ) ;
#25395 = DIRECTION ( 'NONE',  ( 0.000000000000000000, 0.000000000000000000, 1.000000000000000000 ) ) ;
#25396 = CARTESIAN_POINT ( 'NONE',  ( 15.00000000000000000, -1.278221433540507546, -26.51162292216071492 ) ) ;
#25397 = ADVANCED_FACE ( 'NONE', ( #40140 ), #22862, .F. ) ;
#25398 = ADVANCED_FACE ( 'NONE', ( #5207 ), #26986, .T. ) ;
#25399 = CARTESIAN_POINT ( 'NONE',  ( 96.15314808468748708, 88.00268892867053694, 85.56822916753381492 ) ) ;
#25400 = CARTESIAN_POINT ( 'NONE',  ( -96.15314808468747287, -208.0026889286704943, 86.52072916753382970 ) ) ;
#25401 = CARTESIAN_POINT ( 'NONE',  ( 96.32499999999998863, -212.2949673200287179, 83.94104166840097037 ) ) ;
#25402 = VERTEX_POINT ( 'NONE', #63095 ) ;
#25403 = CARTESIAN_POINT ( 'NONE',  ( 0.000000000000000000, -77.49459641780886443, -0.8261519478439277586 ) ) ;
#25404 = AXIS2_PLACEMENT_3D ( 'NONE', #32007, #13973, #7611 ) ;
#25405 = CARTESIAN_POINT ( 'NONE',  ( -93.67499999999998295, -212.2949673200287179, 82.59166666666665435 ) ) ;
#25406 = CARTESIAN_POINT ( 'NONE',  ( -97.30629616937501680, 88.66845928578038638, 76.36072916753381890 ) ) ;
#25407 = EDGE_CURVE ( 'NONE', #23895, #57460, #72838, .T. ) ;
#25408 = VECTOR ( 'NONE', #18891, 1000.000000000000000 ) ;
#25409 = CARTESIAN_POINT ( 'NONE',  ( 97.30629616937498838, -208.6684592857803011, 84.29822916753380468 ) ) ;
#25410 = ORIENTED_EDGE ( 'NONE', *, *, #18307, .F. ) ;
#25411 = AXIS2_PLACEMENT_3D ( 'NONE', #8150, #65677, #31813 ) ;
#25412 = EDGE_CURVE ( 'NONE', #10397, #3672, #47401, .T. ) ;
#25413 = SURFACE_STYLE_USAGE ( .BOTH. , #34552 ) ;
#25414 = EDGE_LOOP ( 'NONE', ( #52041, #445, #24242, #15328 ) ) ;
#25415 = EDGE_CURVE ( 'NONE', #55326, #49491, #5576, .T. ) ;
#25416 = EDGE_LOOP ( 'NONE', ( #54400, #14687, #7788, #13766 ) ) ;
#25417 = CIRCLE ( 'NONE', #38628, 16.00000000000000000 ) ;
#25418 = CARTESIAN_POINT ( 'NONE',  ( 10.00000000000000000, 33.17418723428333749, -17.67226234102790272 ) ) ;
#25419 = CIRCLE ( 'NONE', #12204, 14.09999999999999964 ) ;
#25420 = AXIS2_PLACEMENT_3D ( 'NONE', #69689, #19290, #41485 ) ;
#25421 = ORIENTED_EDGE ( 'NONE', *, *, #69178, .F. ) ;
#25422 = DIRECTION ( 'NONE',  ( -1.000000000000000000, 0.000000000000000000, -0.000000000000000000 ) ) ;
#25423 = CARTESIAN_POINT ( 'NONE',  ( 93.84685191531249870, -208.0026889286704943, 78.26572916753382003 ) ) ;
#25424 = CARTESIAN_POINT ( 'NONE',  ( 10.00000000000000000, -59.03961581697367933, -46.53671651294010303 ) ) ;
#25425 = DIRECTION ( 'NONE',  ( -0.000000000000000000, -0.000000000000000000, 1.000000000000000000 ) ) ;
#25426 = CARTESIAN_POINT ( 'NONE',  ( 92.35000000000000853, -209.9999999999999716, 80.47499999999999432 ) ) ;
#25427 = DIRECTION ( 'NONE',  ( -1.000000000000000000, -0.000000000000000000, -0.000000000000000000 ) ) ;
#25428 = CYLINDRICAL_SURFACE ( 'NONE', #21319, 32.00000000000000000 ) ;
#25429 = CARTESIAN_POINT ( 'NONE',  ( 93.67500000000001137, -207.7050326799711968, 82.90916666666666401 ) ) ;
#25430 = ORIENTED_EDGE ( 'NONE', *, *, #53726, .T. ) ;
#25431 = VERTEX_POINT ( 'NONE', #15724 ) ;
#25432 = VERTEX_POINT ( 'NONE', #73224 ) ;
#25433 = VERTEX_POINT ( 'NONE', #61591 ) ;
#25434 = CARTESIAN_POINT ( 'NONE',  ( -97.30629616937501680, 91.33154071421968467, 83.39864583420050792 ) ) ;
#25435 = CARTESIAN_POINT ( 'NONE',  ( -92.34999999999999432, -209.9999999999999716, 76.98250000000000171 ) ) ;
#25436 = DIRECTION ( 'NONE',  ( 0.000000000000000000, 0.000000000000000000, 1.000000000000000000 ) ) ;
#25437 = CARTESIAN_POINT ( 'NONE',  ( 96.32499999999997442, 92.29496732002878900, 76.45333333333333314 ) ) ;
#25438 = VERTEX_POINT ( 'NONE', #10075 ) ;
#25439 = CARTESIAN_POINT ( 'NONE',  ( -94.99999999999997158, -206.9400435732949575, 84.84062500173429555 ) ) ;
#25440 = ORIENTED_EDGE ( 'NONE', *, *, #68708, .T. ) ;
#25441 = CARTESIAN_POINT ( 'NONE',  ( -2.977765906491215642, 0.000000000000000000, 0.000000000000000000 ) ) ;
#25442 = ORIENTED_EDGE ( 'NONE', *, *, #62559, .T. ) ;
#25443 = CARTESIAN_POINT ( 'NONE',  ( -97.65000000000001990, 90.00000000000004263, 86.90437500173429441 ) ) ;
#25444 = CARTESIAN_POINT ( 'NONE',  ( 96.15314808468748708, 91.99731107132950569, 87.68489583420048916 ) ) ;
#25445 = DIRECTION ( 'NONE',  ( -1.000000000000000000, 0.000000000000000000, 0.000000000000000000 ) ) ;
#25446 = DIRECTION ( 'NONE',  ( -1.000000000000000000, 0.000000000000000000, -0.000000000000000000 ) ) ;
#25447 = CARTESIAN_POINT ( 'NONE',  ( -92.34999999999999432, -208.4700217866474645, 78.38479166840096468 ) ) ;
#25448 = COLOUR_RGB ( '', 0.08235294, 0.09019608, 0.10196078) ;
#25449 = CIRCLE ( 'NONE', #39846, 31.99999999999998579 ) ;
#25450 = EDGE_CURVE ( 'NONE', #58350, #47426, #3795, .T. ) ;
#25451 = DIRECTION ( 'NONE',  ( 0.000000000000000000, 0.000000000000000000, 1.000000000000000000 ) ) ;
#25452 = ORIENTED_EDGE ( 'NONE', *, *, #29175, .T. ) ;
#25453 = CARTESIAN_POINT ( 'NONE',  ( 11.99999999999999822, -73.73191006444582740, 14.66109333815435889 ) ) ;
#25454 = DIRECTION ( 'NONE',  ( 1.000000000000000000, 0.000000000000000000, -0.000000000000000000 ) ) ;
#25455 = ORIENTED_EDGE ( 'NONE', *, *, #3032, .F. ) ;
#25456 = EDGE_CURVE ( 'NONE', #51709, #39121, #11925, .T. ) ;
#25457 = AXIS2_PLACEMENT_3D ( 'NONE', #28604, #63591, #103 ) ;
#25458 = ORIENTED_EDGE ( 'NONE', *, *, #40224, .T. ) ;
#25459 = CYLINDRICAL_SURFACE ( 'NONE', #22968, 77.49899999999999523 ) ;
#25460 = EDGE_CURVE ( 'NONE', #17976, #2629, #6309, .T. ) ;
#25461 = VECTOR ( 'NONE', #66343, 1000.000000000000000 ) ;
#25462 = CARTESIAN_POINT ( 'NONE',  ( 2.499999999999979572, -90.00000000000000000, -310.0000000000000000 ) ) ;
#25463 = DIRECTION ( 'NONE',  ( 0.9435911131814398445, -0.3311129884571295534, 0.000000000000000000 ) ) ;
#25464 = ADVANCED_FACE ( 'NONE', ( #7409 ), #58530, .T. ) ;
#25465 = CARTESIAN_POINT ( 'NONE',  ( -92.69370383062498320, -209.9999999999999716, 83.13406250086715943 ) ) ;
#25466 = ORIENTED_EDGE ( 'NONE', *, *, #39404, .F. ) ;
#25467 = CARTESIAN_POINT ( 'NONE',  ( 10.00000000000000000, 4.992566952384984269, 37.16516213103279398 ) ) ;
#25468 = ORIENTED_EDGE ( 'NONE', *, *, #32503, .T. ) ;
#25469 = ORIENTED_EDGE ( 'NONE', *, *, #71716, .T. ) ;
#25470 = DIRECTION ( 'NONE',  ( -1.000000000000000000, -0.000000000000000000, 0.000000000000000000 ) ) ;
#25471 = AXIS2_PLACEMENT_3D ( 'NONE', #69072, #52139, #6653 ) ;
#25472 = VECTOR ( 'NONE', #60255, 1000.000000000000000 ) ;
#25473 = CARTESIAN_POINT ( 'NONE',  ( -3.000000000000000000, 6.762365576493643893, -25.66652317338391853 ) ) ;
#25474 = CARTESIAN_POINT ( 'NONE',  ( 93.84685191531248449, 91.99731107132950569, 82.55197916753380127 ) ) ;
#25475 = CARTESIAN_POINT ( 'NONE',  ( 5.000000000000000000, -71.21200624218768382, -40.65526001592689909 ) ) ;
#25476 = LINE ( 'NONE', #69488, #18045 ) ;
#25477 = CARTESIAN_POINT ( 'NONE',  ( 11.99999999999999822, 0.000000000000000000, 0.000000000000000000 ) ) ;
#25478 = LINE ( 'NONE', #48773, #25587 ) ;
#25479 = CARTESIAN_POINT ( 'NONE',  ( 5.000000000000000000, 2.886751345948134428, -2.080000000000000071 ) ) ;
#25480 = CARTESIAN_POINT ( 'NONE',  ( 0.000000000000000000, -15.33399622253424432, -80.55351364060604169 ) ) ;
#25481 = CARTESIAN_POINT ( 'NONE',  ( 0.000000000000000000, -31.47745569255092235, -68.26794271651296242 ) ) ;
#25482 = VERTEX_POINT ( 'NONE', #46516 ) ;
#25483 = CARTESIAN_POINT ( 'NONE',  ( -95.00000000000002842, 92.66308142843932671, 87.57906250086713840 ) ) ;
#25484 = EDGE_CURVE ( 'NONE', #48015, #65118, #66557, .T. ) ;
#25485 = EDGE_CURVE ( 'NONE', #31522, #37710, #1775, .T. ) ;
#25486 = CARTESIAN_POINT ( 'NONE',  ( -15.44521549751111422, -137.7748507232956001, -5.500000000000000000 ) ) ;
#25487 = CARTESIAN_POINT ( 'NONE',  ( 15.00000000000000000, -0.9646360437372099028, 23.52805723605590771 ) ) ;
#25488 = ADVANCED_FACE ( 'NONE', ( #35967 ), #12664, .F. ) ;
#25489 = VERTEX_POINT ( 'NONE', #58167 ) ;
#25490 = CARTESIAN_POINT ( 'NONE',  ( -3.000000000000000000, -10.45096189432344147, 21.10159698893426494 ) ) ;
#25491 = CARTESIAN_POINT ( 'NONE',  ( 26.49955575014745079, 0.001194404164630089764, -64.00000000000000000 ) ) ;
#25492 = LINE ( 'NONE', #19840, #62346 ) ;
#25493 = COLOUR_RGB ( '', 0.66274510, 0.83137255, 0.94901961) ;
#25494 = CARTESIAN_POINT ( 'NONE',  ( 97.30629616937498838, -209.9999999999999716, 80.59406250086715318 ) ) ;
#25495 = EDGE_LOOP ( 'NONE', ( #22110, #48078, #47725, #18392 ) ) ;
#25496 = ORIENTED_EDGE ( 'NONE', *, *, #13291, .T. ) ;
#25497 = AXIS2_PLACEMENT_3D ( 'NONE', #31373, #9189, #3577 ) ;
#25498 = DIRECTION ( 'NONE',  ( 0.000000000000000000, 0.8526401643540935105, -0.5224985647159466895 ) ) ;
#25499 = ORIENTED_EDGE ( 'NONE', *, *, #46860, .T. ) ;
#25500 = CYLINDRICAL_SURFACE ( 'NONE', #38949, 3.299999999999969624 ) ;
#25501 = CIRCLE ( 'NONE', #51918, 82.00000000000000000 ) ;
#25502 =( BOUNDED_CURVE ( )  B_SPLINE_CURVE ( 2, ( #35851, #1697, #46408, #34759, #69334, #24226, #953 ),
 .UNSPECIFIED., .F., .F. ) 
 B_SPLINE_CURVE_WITH_KNOTS ( ( 3, 2, 2, 3 ),
 ( 0.6773535682752291898, 0.6844092574655884498, 0.6914650230064715020, 0.6985206468843497829 ),
 .UNSPECIFIED. ) 
 CURVE ( )  GEOMETRIC_REPRESENTATION_ITEM ( )  RATIONAL_B_SPLINE_CURVE ( ( 0.9999971005499384002, 0.8660268535251571809, 1.000000000000000000, 0.8660254037844387076, 1.000000000000000000, 0.8660280936759529036, 0.9999946203249847620 ) ) 
 REPRESENTATION_ITEM ( '' )  );
#25503 = CYLINDRICAL_SURFACE ( 'NONE', #49587, 42.00000000000000000 ) ;
#25504 = ORIENTED_EDGE ( 'NONE', *, *, #58392, .F. ) ;
#25505 = CARTESIAN_POINT ( 'NONE',  ( 95.00000000000000000, -207.3369185715606307, 75.03781250086714749 ) ) ;
#25506 = ORIENTED_EDGE ( 'NONE', *, *, #1737, .F. ) ;
#25507 = LINE ( 'NONE', #36785, #19088 ) ;
#25508 = ORIENTED_EDGE ( 'NONE', *, *, #21821, .F. ) ;
#25509 = CIRCLE ( 'NONE', #29159, 23.50000000000489919 ) ;
#25510 = EDGE_LOOP ( 'NONE', ( #5425, #5752, #17678, #10387 ) ) ;
#25511 = LINE ( 'NONE', #72475, #14171 ) ;
#25512 = AXIS2_PLACEMENT_3D ( 'NONE', #50043, #43338, #72970 ) ;
#25513 = FACE_OUTER_BOUND ( 'NONE', #38261, .T. ) ;
#25514 = ORIENTED_EDGE ( 'NONE', *, *, #7654, .F. ) ;
#25515 = DIRECTION ( 'NONE',  ( 0.000000000000000000, -0.3090169943749349057, -0.9510565162951577500 ) ) ;
#25516 = CARTESIAN_POINT ( 'NONE',  ( 97.64999999999999147, -209.9999999999999716, 82.77687500173431090 ) ) ;
#25517 = CARTESIAN_POINT ( 'NONE',  ( 92.34999999999999432, 91.52997821335252127, 83.59708333333334451 ) ) ;
#25518 = ORIENTED_EDGE ( 'NONE', *, *, #19841, .T. ) ;
#25519 = CARTESIAN_POINT ( 'NONE',  ( 10.00000000000000000, 62.50884508063427347, 41.76106447765511831 ) ) ;
#25520 = DIRECTION ( 'NONE',  ( 0.000000000000000000, 0.000000000000000000, 1.000000000000000000 ) ) ;
#25521 = VERTEX_POINT ( 'NONE', #52150 ) ;
#25522 = ORIENTED_EDGE ( 'NONE', *, *, #46939, .F. ) ;
#25523 = CARTESIAN_POINT ( 'NONE',  ( -97.30629616937501680, 90.00000000000004263, 86.62656250086715204 ) ) ;
#25524 = CARTESIAN_POINT ( 'NONE',  ( 97.30629616937498838, 90.00000000000002842, 81.07031250086714635 ) ) ;
#25525 = VERTEX_POINT ( 'NONE', #24328 ) ;
#25526 = CARTESIAN_POINT ( 'NONE',  ( 96.32499999999998863, 87.70503267997126784, 83.94104166840097037 ) ) ;
#25527 = EDGE_CURVE ( 'NONE', #12032, #33095, #73842, .T. ) ;
#25528 = CARTESIAN_POINT ( 'NONE',  ( 0.000000000000000000, -76.69515212745996280, -29.01471420065644580 ) ) ;
#25529 = ORIENTED_EDGE ( 'NONE', *, *, #3955, .F. ) ;
#25530 = CARTESIAN_POINT ( 'NONE',  ( 92.35000000030107969, -209.9999754409356854, 87.53856274002261273 ) ) ;
#25531 = ORIENTED_EDGE ( 'NONE', *, *, #32943, .F. ) ;
#25532 = ORIENTED_EDGE ( 'NONE', *, *, #52710, .T. ) ;
#25533 = ADVANCED_FACE ( 'NONE', ( #36336 ), #6665, .F. ) ;
#25534 = ORIENTED_EDGE ( 'NONE', *, *, #33712, .T. ) ;
#25535 = CARTESIAN_POINT ( 'NONE',  ( -92.35000000000003695, 90.00000000000004263, 85.87249999999998806 ) ) ;
#25536 = DIRECTION ( 'NONE',  ( 0.000000000000000000, -0.8910065241883627918, -0.4539904997395568520 ) ) ;
#25537 = EDGE_CURVE ( 'NONE', #42721, #2983, #66614, .T. ) ;
#25538 = CARTESIAN_POINT ( 'NONE',  ( -97.65000000000001990, 91.52997821335253548, 83.59708333333334451 ) ) ;
#25539 = ORIENTED_EDGE ( 'NONE', *, *, #36584, .T. ) ;
#25540 = CARTESIAN_POINT ( 'NONE',  ( 97.30629616937497417, 90.27617560457109391, 74.79348190356854786 ) ) ;
#25541 = CARTESIAN_POINT ( 'NONE',  ( 10.00000000000000000, 51.29473840253317718, -63.97538442413367932 ) ) ;
#25542 = EDGE_LOOP ( 'NONE', ( #15268, #23153, #38275, #54543 ) ) ;
#25543 = DIRECTION ( 'NONE',  ( -1.000000000000000000, -0.000000000000000000, 0.000000000000000000 ) ) ;
#25544 = CARTESIAN_POINT ( 'NONE',  ( -92.69370383062498320, -211.3315407142195852, 78.47739583420047893 ) ) ;
#25546 = ORIENTED_EDGE ( 'NONE', *, *, #4441, .F. ) ;
#25545 = EDGE_CURVE ( 'NONE', #68971, #73338, #11455, .T. ) ;
#25547 = DIRECTION ( 'NONE',  ( 0.000000000000000000, 0.000000000000000000, 1.000000000000000000 ) ) ;
#25548 = CARTESIAN_POINT ( 'NONE',  ( 11.99999999999999822, -77.32052557432837148, -5.256550761633681290 ) ) ;
#25549 = DIRECTION ( 'NONE',  ( 0.000000000000000000, 0.000000000000000000, 1.000000000000000000 ) ) ;
#25550 = CARTESIAN_POINT ( 'NONE',  ( 10.00000000000000000, 81.50828551894240093, -8.966570791699799869 ) ) ;
#25551 = LINE ( 'NONE', #65426, #28361 ) ;
#25552 = CIRCLE ( 'NONE', #54374, 26.50000000000552092 ) ;
#25553 = CARTESIAN_POINT ( 'NONE',  ( 4.999999999999999112, 41.81611651403861885, 3.925862922256313503 ) ) ;
#25554 = CARTESIAN_POINT ( 'NONE',  ( 0.000000000000000000, -36.72794159290197769, -65.59268652807249111 ) ) ;
#25555 = CARTESIAN_POINT ( 'NONE',  ( 35.50000000000000711, -120.0000000000000000, 2.500000000000000000 ) ) ;
#25556 = DIRECTION ( 'NONE',  ( 1.000000000000000000, 0.000000000000000000, 0.000000000000000000 ) ) ;
#25557 = EDGE_CURVE ( 'NONE', #45793, #1974, #65441, .T. ) ;
#25558 = CARTESIAN_POINT ( 'NONE',  ( 97.65000000000000568, 88.47002178664752137, 86.53395833506763779 ) ) ;
#25559 = ADVANCED_FACE ( 'NONE', ( #57806 ), #695, .F. ) ;
#25560 = CARTESIAN_POINT ( 'NONE',  ( -96.15314808468751551, 88.00268892867056536, 76.41364583420048007 ) ) ;
#25561 = CARTESIAN_POINT ( 'NONE',  ( 10.00000000000000000, -37.22597642581153821, -5.202137450156795850 ) ) ;
#25562 = CYLINDRICAL_SURFACE ( 'NONE', #35060, 37.49900000000000233 ) ;
#25563 = AXIS2_PLACEMENT_3D ( 'NONE', #28460, #29558, #52496 ) ;
#25564 = LINE ( 'NONE', #25931, #21150 ) ;
#25565 = UNCERTAINTY_MEASURE_WITH_UNIT (LENGTH_MEASURE( 1.000000000000000082E-05 ), #13293, 'distance_accuracy_value', 'NONE');
#25566 = DIRECTION ( 'NONE',  ( -1.000000000000000000, 0.000000000000000000, 0.000000000000000000 ) ) ;
#25567 = AXIS2_PLACEMENT_3D ( 'NONE', #33599, #39258, #62186 ) ;
#25568 = CARTESIAN_POINT ( 'NONE',  ( 0.000000000000000000, 77.19088730480532945, -6.903761155836932062 ) ) ;
#25569 = CARTESIAN_POINT ( 'NONE',  ( 94.99999999999998579, 92.66308142843932671, 89.00781250086716057 ) ) ;
#25570 = EDGE_CURVE ( 'NONE', #6148, #50088, #17945, .T. ) ;
#25572 = EDGE_CURVE ( 'NONE', #6029, #7101, #18308, .T. ) ;
#25571 = AXIS2_PLACEMENT_3D ( 'NONE', #13076, #19823, #26580 ) ;
#25573 = CYLINDRICAL_SURFACE ( 'NONE', #56315, 82.00000000000000000 ) ;
#25574 = DIRECTION ( 'NONE',  ( -1.000000000000000000, 0.000000000000000000, -0.000000000000000000 ) ) ;
#25575 = CARTESIAN_POINT ( 'NONE',  ( 97.64999999999999147, 90.00000000000002842, 86.50750000000000739 ) ) ;
#25576 = CARTESIAN_POINT ( 'NONE',  ( -92.34999999999999432, -209.9999999999999716, 87.77749999999998920 ) ) ;
#25577 = DIRECTION ( 'NONE',  ( -1.000000000000000000, 0.000000000000000000, 0.000000000000000000 ) ) ;
#25578 = ORIENTED_EDGE ( 'NONE', *, *, #34830, .T. ) ;
#25579 = CARTESIAN_POINT ( 'NONE',  ( 11.99999999999999822, 0.000000000000000000, 0.000000000000000000 ) ) ;
#25580 = DIRECTION ( 'NONE',  ( 0.000000000000000000, 0.000000000000000000, 1.000000000000000000 ) ) ;
#25581 =( LENGTH_UNIT ( ) NAMED_UNIT ( * ) SI_UNIT ( .MILLI., .METRE. ) );
#25582 = CARTESIAN_POINT ( 'NONE',  ( -93.67500000000003979, 92.29496732002878900, 84.70833333333332860 ) ) ;
#25583 = EDGE_LOOP ( 'NONE', ( #2279, #43858, #29037, #54963, #61403 ) ) ;
#25584 = DIRECTION ( 'NONE',  ( -1.000000000000000000, -0.000000000000000000, -0.000000000000000000 ) ) ;
#25585 = CARTESIAN_POINT ( 'NONE',  ( -2.500000000000015543, -73.00000000000001421, -255.0000000000000000 ) ) ;
#25586 = ORIENTED_EDGE ( 'NONE', *, *, #6333, .F. ) ;
#25587 = VECTOR ( 'NONE', #24372, 1000.000000000000000 ) ;
#25588 = CARTESIAN_POINT ( 'NONE',  ( 92.69370383062501162, -211.3315407142195852, 82.07572916753382231 ) ) ;
#25589 = CARTESIAN_POINT ( 'NONE',  ( 97.30629616937498838, -209.9999999999999716, 89.48406250086715374 ) ) ;
#25590 = VERTEX_POINT ( 'NONE', #43111 ) ;
#25591 = DIRECTION ( 'NONE',  ( 0.000000000000000000, 0.000000000000000000, 1.000000000000000000 ) ) ;
#25592 = PRODUCT_DEFINITION_FORMATION_WITH_SPECIFIED_SOURCE ( 'ANY', '', #62027, .NOT_KNOWN. ) ;
#25593 = VERTEX_POINT ( 'NONE', #37471 ) ;
#25594 = DIRECTION ( 'NONE',  ( 1.000000000000000000, 0.000000000000000000, 0.000000000000000000 ) ) ;
#25595 = ORIENTED_EDGE ( 'NONE', *, *, #40910, .T. ) ;
#25596 = CARTESIAN_POINT ( 'NONE',  ( -93.84685191531254134, 91.99731107132950569, 75.61989583420049144 ) ) ;
#25597 = ORIENTED_EDGE ( 'NONE', *, *, #73348, .T. ) ;
#25598 = ORIENTED_EDGE ( 'NONE', *, *, #1742, .T. ) ;
#25599 = CARTESIAN_POINT ( 'NONE',  ( -23.97194136764370498, -131.3950000906648938, 5.500000000000000000 ) ) ;
#25600 = VERTEX_POINT ( 'NONE', #48003 ) ;
#25601 = CARTESIAN_POINT ( 'NONE',  ( 0.000000000000000000, -16.65560815589439159, 38.55633173627004595 ) ) ;
#25602 = CARTESIAN_POINT ( 'NONE',  ( 0.000000000000000000, -55.20638768913797634, 51.02545421589302777 ) ) ;
#25603 = ADVANCED_FACE ( 'NONE', ( #9246 ), #60402, .T. ) ;
#25604 = VERTEX_POINT ( 'NONE', #48363 ) ;
#25605 = FACE_OUTER_BOUND ( 'NONE', #5239, .T. ) ;
#25606 = ADVANCED_FACE ( 'NONE', ( #60765 ), #42728, .T. ) ;
#25607 = CIRCLE ( 'NONE', #67647, 77.49899999999999523 ) ;
#25608 = ORIENTED_EDGE ( 'NONE', *, *, #35330, .T. ) ;
#25609 = FACE_OUTER_BOUND ( 'NONE', #42269, .T. ) ;
#25610 = CIRCLE ( 'NONE', #37647, 31.99999999999999289 ) ;
#25611 = EDGE_LOOP ( 'NONE', ( #72421, #53523, #32363, #600 ) ) ;
#25612 = EDGE_CURVE ( 'NONE', #23472, #2062, #31436, .T. ) ;
#25613 = ORIENTED_EDGE ( 'NONE', *, *, #14407, .T. ) ;
#25614 = AXIS2_PLACEMENT_3D ( 'NONE', #18345, #41291, #52939 ) ;
#25615 = ORIENTED_EDGE ( 'NONE', *, *, #6771, .T. ) ;
#25616 = CARTESIAN_POINT ( 'NONE',  ( 96.15314808468748708, -208.0026889286704943, 78.00114583420048575 ) ) ;
#25617 = CIRCLE ( 'NONE', #56870, 42.00000000000000000 ) ;
#25618 = CARTESIAN_POINT ( 'NONE',  ( -93.67500000000003979, 92.29496732002878900, 83.43833333333333258 ) ) ;
#25619 = CIRCLE ( 'NONE', #53265, 31.99999999999999645 ) ;
#25620 = CONTEXT_DEPENDENT_SHAPE_REPRESENTATION ( #36866, #25338 ) ;
#25621 = CARTESIAN_POINT ( 'NONE',  ( 15.00000000000000000, -11.95096189432345746, -23.69967320028757030 ) ) ;
#25622 = ORIENTED_EDGE ( 'NONE', *, *, #26207, .T. ) ;
#25623 = CARTESIAN_POINT ( 'NONE',  ( -97.64999999989191792, -209.9999848944890175, 78.64888723590522090 ) ) ;
#25624 = EDGE_LOOP ( 'NONE', ( #37453, #40106, #43574, #57244 ) ) ;
#25625 = DIRECTION ( 'NONE',  ( 1.000000000000000000, 0.000000000000000000, 0.000000000000000000 ) ) ;
#25626 = ADVANCED_FACE ( 'NONE', ( #37088 ), #2556, .F. ) ;
#25627 = DIRECTION ( 'NONE',  ( 1.000000000000000000, 0.000000000000000000, 0.000000000000000000 ) ) ;
#25628 = DIRECTION ( 'NONE',  ( -1.000000000000000000, -0.000000000000000000, -0.000000000000000000 ) ) ;
#25629 = CARTESIAN_POINT ( 'NONE',  ( -97.51367041768835975, 89.99999999999990052, 74.91808492278043730 ) ) ;
#25630 = CARTESIAN_POINT ( 'NONE',  ( -96.15314808468745866, -211.9973110713294489, 79.58864583420047722 ) ) ;
#25631 = CARTESIAN_POINT ( 'NONE',  ( -96.15314808468752972, 91.99731107132950569, 80.17072916753382117 ) ) ;
#25632 = ORIENTED_EDGE ( 'NONE', *, *, #68449, .F. ) ;
#25633 = CARTESIAN_POINT ( 'NONE',  ( 93.84685191531248449, 88.00268892867053694, 80.85864583420047325 ) ) ;
#25634 = ORIENTED_EDGE ( 'NONE', *, *, #48798, .F. ) ;
#25635 = DIRECTION ( 'NONE',  ( 0.000000000000000000, 0.000000000000000000, 1.000000000000000000 ) ) ;
#25636 = CARTESIAN_POINT ( 'NONE',  ( 0.000000000000000000, 2.946379043147425492, -75.11764819372145041 ) ) ;
#25637 = EDGE_CURVE ( 'NONE', #68597, #65643, #57066, .T. ) ;
#25638 = CARTESIAN_POINT ( 'NONE',  ( -19.90058851926621131, -132.5883508287165853, 5.500000000000000000 ) ) ;
#25639 = DIRECTION ( 'NONE',  ( 0.000000000000000000, 0.000000000000000000, 1.000000000000000000 ) ) ;
#25640 = CARTESIAN_POINT ( 'NONE',  ( -5.000000000000000000, 2.886751345948137981, -5.553418012614792509 ) ) ;
#25641 = CARTESIAN_POINT ( 'NONE',  ( -92.69370383062498320, -208.6684592857803295, 81.75822916753381264 ) ) ;
#25642 = CIRCLE ( 'NONE', #32868, 82.00000000000000000 ) ;
#25643 = CARTESIAN_POINT ( 'NONE',  ( 15.00000000000000000, -22.67460108101774452, 6.353146135318220367 ) ) ;
#25644 = PLANE ( 'NONE',  #3127 ) ;
#25645 = CARTESIAN_POINT ( 'NONE',  ( -95.00000000002617639, -209.9999999999999432, -64.99999999999349143 ) ) ;
#25646 = VERTEX_POINT ( 'NONE', #2174 ) ;
#25647 = EDGE_LOOP ( 'NONE', ( #54095, #576 ) ) ;
#25648 = LINE ( 'NONE', #7989, #37283 ) ;
#25649 = CARTESIAN_POINT ( 'NONE',  ( -97.65000000000001990, 90.00000000000004263, 75.39499999999999602 ) ) ;
#25650 = EDGE_CURVE ( 'NONE', #973, #64962, #19414, .T. ) ;
#25651 = DIRECTION ( 'NONE',  ( -0.000000000000000000, -0.000000000000000000, 1.000000000000000000 ) ) ;
#25652 = EDGE_CURVE ( 'NONE', #31534, #14320, #35424, .T. ) ;
#25653 = CARTESIAN_POINT ( 'NONE',  ( -92.69370383062502583, 91.33154071421968467, 83.66322916753379957 ) ) ;
#25654 = CARTESIAN_POINT ( 'NONE',  ( 11.99999999999999822, 70.53064760720278059, 26.01480285779964774 ) ) ;
#25655 = CARTESIAN_POINT ( 'NONE',  ( -13.05994868825747446, -139.5943292883446532, -5.500000000000000000 ) ) ;
#25656 = DIRECTION ( 'NONE',  ( -1.000000000000000000, -0.000000000000000000, -0.000000000000000000 ) ) ;
#25657 = ORIENTED_EDGE ( 'NONE', *, *, #25114, .T. ) ;
#25658 = LINE ( 'NONE', #58391, #26023 ) ;
#25659 = CIRCLE ( 'NONE', #35271, 42.00000000000000000 ) ;
#25660 = PRODUCT_DEFINITION_FORMATION_WITH_SPECIFIED_SOURCE ( 'ANY', '', #37971, .NOT_KNOWN. ) ;
#25661 = DIRECTION ( 'NONE',  ( -1.000000000000000000, -0.000000000000000000, 0.000000000000000000 ) ) ;
#25662 = AXIS2_PLACEMENT_3D ( 'NONE', #15985, #21623, #16360 ) ;
#25663 = CYLINDRICAL_SURFACE ( 'NONE', #26237, 42.00000000000000000 ) ;
#25664 = CARTESIAN_POINT ( 'NONE',  ( -2.260257450329326456, 4.468542444510766209, -0.5197061503823194872 ) ) ;
#25665 = CARTESIAN_POINT ( 'NONE',  ( 5.000000000000002665, -81.90746397400393164, 3.894527615417586741 ) ) ;
#25666 = DIRECTION ( 'NONE',  ( 0.000000000000000000, 0.5224985647159500202, -0.8526401643540916231 ) ) ;
#25667 = CARTESIAN_POINT ( 'NONE',  ( -92.69370383062498320, -211.3315407142195852, 81.17614583420048291 ) ) ;
#25668 =( NAMED_UNIT ( * ) PLANE_ANGLE_UNIT ( ) SI_UNIT ( $, .RADIAN. ) );
#25669 = CARTESIAN_POINT ( 'NONE',  ( 2.499999999999984457, -73.00000000000001421, -204.9999999999999716 ) ) ;
#25670 = AXIS2_PLACEMENT_3D ( 'NONE', #37996, #44764, #60930 ) ;
#25671 = CIRCLE ( 'NONE', #4125, 82.00000000000000000 ) ;
#25672 = CARTESIAN_POINT ( 'NONE',  ( 5.000000000000000000, 32.34446384430010113, -26.79245525562679831 ) ) ;
#25673 = CARTESIAN_POINT ( 'NONE',  ( 0.000000000000000000, 0.000000000000000000, 0.000000000000000000 ) ) ;
#25674 = CARTESIAN_POINT ( 'NONE',  ( -97.64999999999993463, 88.47002178664749295, 88.78291666666667936 ) ) ;
#25675 = VERTEX_POINT ( 'NONE', #72024 ) ;
#25676 = CARTESIAN_POINT ( 'NONE',  ( 11.99999999999999822, -79.10210256391353312, -21.60688246758669706 ) ) ;
#25677 = CARTESIAN_POINT ( 'NONE',  ( 0.000000000000000000, 0.000000000000000000, 0.000000000000000000 ) ) ;
#25678 = LINE ( 'NONE', #55356, #27005 ) ;
#25679 = CIRCLE ( 'NONE', #56933, 82.00000000000000000 ) ;
#25680 = FACE_OUTER_BOUND ( 'NONE', #20527, .T. ) ;
#25681 = CARTESIAN_POINT ( 'NONE',  ( 97.30629616937497417, -210.9303297190751891, 74.68334033237940162 ) ) ;
#25682 = ORIENTED_EDGE ( 'NONE', *, *, #63826, .T. ) ;
#25683 = ADVANCED_FACE ( 'NONE', ( #7773 ), #20900, .T. ) ;
#25684 = CYLINDRICAL_SURFACE ( 'NONE', #2512, 77.49899999999999523 ) ;
#25685 = LINE ( 'NONE', #71904, #7874 ) ;
#25686 = ORIENTED_EDGE ( 'NONE', *, *, #57295, .T. ) ;
#25687 = DIRECTION ( 'NONE',  ( -1.000000000000000000, 0.000000000000000000, 0.000000000000000000 ) ) ;
#25688 = ORIENTED_EDGE ( 'NONE', *, *, #22533, .T. ) ;
#25689 = CIRCLE ( 'NONE', #4143, 77.49900000000000944 ) ;
#25690 = CARTESIAN_POINT ( 'NONE',  ( 0.000000000000000000, -35.38097989696520074, 12.42422080174625520 ) ) ;
#25691 = ORIENTED_EDGE ( 'NONE', *, *, #38020, .F. ) ;
#25692 = ORIENTED_EDGE ( 'NONE', *, *, #24141, .F. ) ;
#25693 = EDGE_CURVE ( 'NONE', #24127, #55748, #13771, .T. ) ;
#25694 = ORIENTED_EDGE ( 'NONE', *, *, #57747, .F. ) ;
#25695 = VERTEX_POINT ( 'NONE', #25061 ) ;
#25696 = DIRECTION ( 'NONE',  ( -1.000000000000000000, 0.000000000000000000, 0.000000000000000000 ) ) ;
#25697 = EDGE_CURVE ( 'NONE', #7952, #14616, #43490, .T. ) ;
#25698 = ORIENTED_EDGE ( 'NONE', *, *, #46373, .F. ) ;
#25699 = CIRCLE ( 'NONE', #42505, 42.00000000000000000 ) ;
#25700 = ORIENTED_EDGE ( 'NONE', *, *, #25325, .F. ) ;
#25701 = CARTESIAN_POINT ( 'NONE',  ( 94.99999999999998579, 87.33691857156068750, 79.16531250086715943 ) ) ;
#25702 = DIRECTION ( 'NONE',  ( -1.000000000000000000, 0.000000000000000000, -0.000000000000000000 ) ) ;
#25703 = DIRECTION ( 'NONE',  ( 1.000000000000000000, 0.000000000000000000, 0.000000000000000000 ) ) ;
#25704 = ORIENTED_EDGE ( 'NONE', *, *, #3499, .T. ) ;
#25705 = EDGE_CURVE ( 'NONE', #31131, #49474, #66411, .T. ) ;
#25706 = VERTEX_POINT ( 'NONE', #14137 ) ;
#25707 = VERTEX_POINT ( 'NONE', #48729 ) ;
#25708 = DIRECTION ( 'NONE',  ( 0.000000000000000000, 0.000000000000000000, 1.000000000000000000 ) ) ;
#25709 = ORIENTED_EDGE ( 'NONE', *, *, #44665, .F. ) ;
#25710 = CIRCLE ( 'NONE', #49685, 77.49899999999999523 ) ;
#25711 = DIRECTION ( 'NONE',  ( 1.000000000000000000, 0.000000000000000000, 0.000000000000000000 ) ) ;
#25712 = CYLINDRICAL_SURFACE ( 'NONE', #29465, 16.00000000000000000 ) ;
#25713 = CARTESIAN_POINT ( 'NONE',  ( -97.42291288542705274, 90.60195399605305511, 74.90604073465185309 ) ) ;
#25714 = DIRECTION ( 'NONE',  ( 0.000000000000000000, 0.000000000000000000, 1.000000000000000000 ) ) ;
#25715 = CARTESIAN_POINT ( 'NONE',  ( -96.32499999999996021, -207.7050326799711968, 84.25854166840096582 ) ) ;
#25716 = DIRECTION ( 'NONE',  ( -1.000000000000000000, 0.000000000000000000, 0.000000000000000000 ) ) ;
#25717 = DIRECTION ( 'NONE',  ( -1.000000000000000000, -0.000000000000000000, 0.000000000000000000 ) ) ;
#25718 = CARTESIAN_POINT ( 'NONE',  ( -92.34999999999999432, -211.5299782133524502, 77.00895833506763211 ) ) ;
#25719 = CARTESIAN_POINT ( 'NONE',  ( -92.69370383062504004, 90.00000000000004263, 89.48406250086715374 ) ) ;
#25721 = CARTESIAN_POINT ( 'NONE',  ( -96.15314808468751551, 88.00268892867056536, 89.11364583420048291 ) ) ;
#25720 = CARTESIAN_POINT ( 'NONE',  ( 97.64999999999999147, 90.00000000000002842, 75.15687500173430635 ) ) ;
#25722 = VECTOR ( 'NONE', #56322, 1000.000000000000000 ) ;
#25723 = ORIENTED_EDGE ( 'NONE', *, *, #50731, .T. ) ;
#25724 = CARTESIAN_POINT ( 'NONE',  ( 97.30629616937498838, 90.00000000000002842, 75.51406250086715488 ) ) ;
#25725 = EDGE_CURVE ( 'NONE', #20797, #43637, #67850, .T. ) ;
#25726 = CARTESIAN_POINT ( 'NONE',  ( 50.00005079999999680, 12.24744871391588852, 2.500000000000003553 ) ) ;
#25727 = DIRECTION ( 'NONE',  ( -1.000000000000000000, 0.000000000000000000, 0.000000000000000000 ) ) ;
#25728 = CARTESIAN_POINT ( 'NONE',  ( 11.99999999999999822, 0.000000000000000000, 0.000000000000000000 ) ) ;
#25729 = DIRECTION ( 'NONE',  ( -1.000000000000000000, 0.000000000000000000, -0.000000000000000000 ) ) ;
#25730 = CARTESIAN_POINT ( 'NONE',  ( 5.000000000000000888, 0.000000000000000000, -6.000000000000000000 ) ) ;
#25731 = ORIENTED_EDGE ( 'NONE', *, *, #20696, .T. ) ;
#25733 = CARTESIAN_POINT ( 'NONE',  ( -92.35000000000000853, -211.5299782133524218, 80.10458333333330927 ) ) ;
#25732 = AXIS2_PLACEMENT_3D ( 'NONE', #71602, #37425, #43061 ) ;
#25734 = CIRCLE ( 'NONE', #73749, 31.99999999999999289 ) ;
#25735 = CARTESIAN_POINT ( 'NONE',  ( 0.000000000000000000, 0.000000000000000000, 0.000000000000000000 ) ) ;
#25736 = EDGE_LOOP ( 'NONE', ( #37661, #66761, #14455, #328 ) ) ;
#25737 = ORIENTED_EDGE ( 'NONE', *, *, #23709, .T. ) ;
#25738 = ADVANCED_FACE ( 'NONE', ( #66766 ), #36707, .T. ) ;
#25739 = FACE_OUTER_BOUND ( 'NONE', #28548, .T. ) ;
#25740 = EDGE_CURVE ( 'NONE', #11281, #58611, #16214, .T. ) ;
#25741 = CARTESIAN_POINT ( 'NONE',  ( -26.50000000000333600, -119.9999999999998010, -48.99999999999928946 ) ) ;
#25742 = DIRECTION ( 'NONE',  ( -0.000000000000000000, -0.000000000000000000, -1.000000000000000000 ) ) ;
#25743 = CIRCLE ( 'NONE', #44965, 12.49999999999999645 ) ;
#25744 = CARTESIAN_POINT ( 'NONE',  ( -20.63749999999999574, -2.946905753440916183E-14, -1.643265707205091412E-14 ) ) ;
#25745 = DIRECTION ( 'NONE',  ( 0.000000000000000000, -0.7604059656000226042, -0.6494480483301934282 ) ) ;
#25746 = CARTESIAN_POINT ( 'NONE',  ( -94.99999999999997158, -212.6630814284392557, 75.35531250086715715 ) ) ;
#25747 =( BOUNDED_CURVE ( )  B_SPLINE_CURVE ( 2, ( #46107, #17525, #51361, #67927, #22816, #62680, #5528 ),
 .UNSPECIFIED., .F., .F. ) 
 B_SPLINE_CURVE_WITH_KNOTS ( ( 3, 2, 2, 3 ),
 ( 0.7408554641864709689, 0.7479111473335299243, 0.7549669128744133095, 0.7620226289464456793 ),
 .UNSPECIFIED. ) 
 CURVE ( )  GEOMETRIC_REPRESENTATION_ITEM ( )  RATIONAL_B_SPLINE_CURVE ( ( 0.9999968710551943030, 0.8660269682751109421, 1.000000000000000000, 0.8660254037844387076, 1.000000000000000000, 0.8660263430970207565, 0.9999981213880071440 ) ) 
 REPRESENTATION_ITEM ( '' )  );
#25748 = EDGE_CURVE ( 'NONE', #16527, #14919, #41435, .T. ) ;
#25749 = ORIENTED_EDGE ( 'NONE', *, *, #19287, .T. ) ;
#25750 = VECTOR ( 'NONE', #23054, 1000.000000000000000 ) ;
#25751 = DIRECTION ( 'NONE',  ( -1.000000000000000000, -0.000000000000000000, 0.000000000000000000 ) ) ;
#25752 = DIRECTION ( 'NONE',  ( 3.035766082959412415E-16, 1.000000000000000000, 0.000000000000000000 ) ) ;
#25753 = DIRECTION ( 'NONE',  ( -1.000000000000000000, 0.000000000000000000, -0.000000000000000000 ) ) ;
#25754 = FACE_OUTER_BOUND ( 'NONE', #33309, .T. ) ;
#25755 = LINE ( 'NONE', #48317, #42525 ) ;
#25756 = CARTESIAN_POINT ( 'NONE',  ( 0.000000000000000000, -38.55633173627022359, 16.65560815589396526 ) ) ;
#25757 = UNCERTAINTY_MEASURE_WITH_UNIT (LENGTH_MEASURE( 1.000000000000000082E-05 ), #33274, 'distance_accuracy_value', 'NONE');
#25758 = FILL_AREA_STYLE_COLOUR ( '', #16978 ) ;
#25759 = CARTESIAN_POINT ( 'NONE',  ( 0.000000000000000000, -2.956366410620109519, -75.11725578898472122 ) ) ;
#25760 = DIRECTION ( 'NONE',  ( 0.000000000000000000, 0.9876883405951383255, -0.1564344650402277048 ) ) ;
#25761 = CARTESIAN_POINT ( 'NONE',  ( 94.99999999999998579, 87.33691857156068750, 84.24531250086717193 ) ) ;
#25762 = CARTESIAN_POINT ( 'NONE',  ( -93.84685191531247028, -211.9973110713294489, 84.29822916753381890 ) ) ;
#25763 = FACE_OUTER_BOUND ( 'NONE', #4720, .T. ) ;
#25764 = EDGE_LOOP ( 'NONE', ( #73745, #15597 ) ) ;
#25765 = DIRECTION ( 'NONE',  ( 0.000000000000000000, 0.000000000000000000, 1.000000000000000000 ) ) ;
#25766 = CARTESIAN_POINT ( 'NONE',  ( -96.32499999999996021, -212.2949673200287179, 79.31083333333333485 ) ) ;
#25767 = DIRECTION ( 'NONE',  ( 0.000000000000000000, 0.000000000000000000, 1.000000000000000000 ) ) ;
#25768 = AXIS2_PLACEMENT_3D ( 'NONE', #36792, #54457, #3723 ) ;
#25769 = CARTESIAN_POINT ( 'NONE',  ( 97.30629616937498838, -211.3315407142195852, 84.82739583420045903 ) ) ;
#25770 = ORIENTED_EDGE ( 'NONE', *, *, #56745, .T. ) ;
#25771 = B_SPLINE_CURVE_WITH_KNOTS ( 'NONE', 3,
 ( #28947, #45894, #34966, #6043, #69182, #40607, #40984, #7135, #30048, #5668, #52999, #1536, #24418, #70259 ),
 .UNSPECIFIED., .F., .F.,
 ( 4, 2, 2, 2, 2, 2, 4 ),
 ( 0.01481111731982464805, 0.01564725794959783214, 0.01648339857937101624, 0.01690146889425760829, 0.01731953920914420034, 0.01773760952403079239, 0.01815567983891738443 ),
 .UNSPECIFIED. ) ;
#25772 = LINE ( 'NONE', #18007, #9481 ) ;
#25773 = ORIENTED_EDGE ( 'NONE', *, *, #16403, .T. ) ;
#25774 = AXIS2_PLACEMENT_3D ( 'NONE', #3785, #27424, #33434 ) ;
#25775 = AXIS2_PLACEMENT_3D ( 'NONE', #26450, #15544, #20810 ) ;
#25776 = ORIENTED_EDGE ( 'NONE', *, *, #38167, .F. ) ;
#25777 = ADVANCED_FACE ( 'NONE', ( #38191 ), #16755, .T. ) ;
#25778 = DIRECTION ( 'NONE',  ( 1.000000000000000000, 0.000000000000000000, -0.000000000000000000 ) ) ;
#25779 = EDGE_CURVE ( 'NONE', #67855, #11835, #36599, .T. ) ;
#25780 = ORIENTED_EDGE ( 'NONE', *, *, #52053, .T. ) ;
#25781 = LINE ( 'NONE', #48712, #34791 ) ;
#25782 = CARTESIAN_POINT ( 'NONE',  ( 93.84685191531249870, -208.0026889286704943, 79.53572916753381605 ) ) ;
#25783 = ADVANCED_FACE ( 'NONE', ( #28015 ), #44958, .F. ) ;
#25784 = DIRECTION ( 'NONE',  ( 0.000000000000000000, 0.000000000000000000, -1.000000000000000000 ) ) ;
#25786 = CARTESIAN_POINT ( 'NONE',  ( 5.000000000000000000, 59.75363087400153006, -56.15606465354897381 ) ) ;
#25785 = AXIS2_PLACEMENT_3D ( 'NONE', #57993, #11380, #11737 ) ;
#25787 = CARTESIAN_POINT ( 'NONE',  ( 10.00000000000000000, -76.66974797899844418, 11.30684508768314522 ) ) ;
#25788 = DIRECTION ( 'NONE',  ( 1.000000000000000000, -0.000000000000000000, 0.000000000000000000 ) ) ;
#25789 = DIRECTION ( 'NONE',  ( -1.000000000000000000, 0.000000000000000000, 0.000000000000000000 ) ) ;
#25790 = CARTESIAN_POINT ( 'NONE',  ( 92.35000000000000853, -209.9999999999999716, 79.83999999999998920 ) ) ;
#25791 = ORIENTED_EDGE ( 'NONE', *, *, #25485, .F. ) ;
#25792 = ADVANCED_FACE ( 'NONE', ( #49834 ), #5117, .T. ) ;
#25793 = ORIENTED_EDGE ( 'NONE', *, *, #19841, .F. ) ;
#25794 = ORIENTED_EDGE ( 'NONE', *, *, #51850, .T. ) ;
#25795 = ORIENTED_EDGE ( 'NONE', *, *, #42799, .F. ) ;
#25796 = CARTESIAN_POINT ( 'NONE',  ( -34.02017708624681092, -130.1428571428571388, 102.9091629284897493 ) ) ;
#25797 = CARTESIAN_POINT ( 'NONE',  ( -96.15314808468752972, 91.99731107132950569, 82.71072916753381321 ) ) ;
#25798 = CARTESIAN_POINT ( 'NONE',  ( 96.32499999999998863, 87.70503267997126784, 88.38604166840097776 ) ) ;
#25799 = DIRECTION ( 'NONE',  ( 0.000000000000000000, 0.000000000000000000, -1.000000000000000000 ) ) ;
#25800 = CARTESIAN_POINT ( 'NONE',  ( -7.500000000000016875, -80.00000000000001421, -189.9999999999999147 ) ) ;
#25801 = LINE ( 'NONE', #72397, #23584 ) ;
#25802 = VERTEX_POINT ( 'NONE', #22774 ) ;
#25803 = CARTESIAN_POINT ( 'NONE',  ( -92.34999999999999432, -211.5299782133524502, 85.26395833506762756 ) ) ;
#25804 = ORIENTED_EDGE ( 'NONE', *, *, #53945, .T. ) ;
#25805 = LINE ( 'NONE', #20544, #14623 ) ;
#25806 = EDGE_CURVE ( 'NONE', #12200, #41007, #18620, .T. ) ;
#25807 = ORIENTED_EDGE ( 'NONE', *, *, #16442, .T. ) ;
#25808 = CARTESIAN_POINT ( 'NONE',  ( -97.65000000000001990, 90.00000000000004263, 84.99937500173429328 ) ) ;
#25809 = ORIENTED_EDGE ( 'NONE', *, *, #41926, .T. ) ;
#25810 = CARTESIAN_POINT ( 'NONE',  ( 94.99999999999998579, 87.33691857156068750, 86.78531250086716398 ) ) ;
#25811 = EDGE_CURVE ( 'NONE', #63004, #55103, #67510, .T. ) ;
#25812 = ADVANCED_FACE ( 'NONE', ( #56232 ), #11108, .T. ) ;
#25813 = DIRECTION ( 'NONE',  ( 0.000000000000000000, 0.7071067811865439090, 0.7071067811865512365 ) ) ;
#25814 = CARTESIAN_POINT ( 'NONE',  ( 5.000000000000000000, 22.48208911017551870, -35.47612816024499693 ) ) ;
#25815 = CARTESIAN_POINT ( 'NONE',  ( 10.00000000000000000, 0.000000000000000000, 0.000000000000000000 ) ) ;
#25816 = DIRECTION ( 'NONE',  ( -0.000000000000000000, -0.000000000000000000, 1.000000000000000000 ) ) ;
#25817 = ORIENTED_EDGE ( 'NONE', *, *, #57754, .F. ) ;
#25818 = LINE ( 'NONE', #48016, #67540 ) ;
#25819 = CARTESIAN_POINT ( 'NONE',  ( 11.99999999999999822, 0.000000000000000000, 0.000000000000000000 ) ) ;
#25820 = EDGE_LOOP ( 'NONE', ( #30061, #13694, #10541, #43010 ) ) ;
#25821 = ORIENTED_EDGE ( 'NONE', *, *, #37684, .T. ) ;
#25822 = DIRECTION ( 'NONE',  ( 0.000000000000000000, 0.000000000000000000, 1.000000000000000000 ) ) ;
#25823 = ADVANCED_FACE ( 'NONE', ( #68638 ), #34033, .T. ) ;
#25824 = DIRECTION ( 'NONE',  ( 0.000000000000000000, 0.000000000000000000, 1.000000000000000000 ) ) ;
#25825 = EDGE_CURVE ( 'NONE', #1781, #17454, #61879, .T. ) ;
#25826 = CARTESIAN_POINT ( 'NONE',  ( 11.99999999999999822, -2.946379043145784582, -75.11764819372150725 ) ) ;
#25827 = CARTESIAN_POINT ( 'NONE',  ( -97.30629616937495996, -209.9999999999999716, 85.35656250086715602 ) ) ;
#25828 = ORIENTED_EDGE ( 'NONE', *, *, #22956, .F. ) ;
#25829 = VECTOR ( 'NONE', #29185, 1000.000000000000000 ) ;
#25830 = FILL_AREA_STYLE_COLOUR ( '', #40536 ) ;
#25831 = VECTOR ( 'NONE', #24424, 1000.000000000000114 ) ;
#25832 = ORIENTED_EDGE ( 'NONE', *, *, #12247, .T. ) ;
#25833 = CARTESIAN_POINT ( 'NONE',  ( -92.34999999999999432, -209.9999999999999716, 90.00000000000000000 ) ) ;
#25834 = DIRECTION ( 'NONE',  ( -1.000000000000000000, 0.000000000000000000, -0.000000000000000000 ) ) ;
#25835 = CYLINDRICAL_SURFACE ( 'NONE', #74182, 31.99999999999999289 ) ;
#25836 = CARTESIAN_POINT ( 'NONE',  ( 94.99999999999998579, 92.66308142843932671, 79.32406250086714294 ) ) ;
#25837 = CARTESIAN_POINT ( 'NONE',  ( 0.000000000000000000, 0.000000000000000000, 0.000000000000000000 ) ) ;
#25838 = DIRECTION ( 'NONE',  ( -1.000000000000000000, 0.000000000000000000, -0.000000000000000000 ) ) ;
#25839 = CIRCLE ( 'NONE', #17423, 31.99999999999999289 ) ;
#25840 = CARTESIAN_POINT ( 'NONE',  ( -31.74999999999995737, 0.000000000000000000, 0.000000000000000000 ) ) ;
#25841 = CARTESIAN_POINT ( 'NONE',  ( 92.57708711457300410, 90.60195399605306932, 74.90604073465190993 ) ) ;
#25842 = CARTESIAN_POINT ( 'NONE',  ( -10.00000000000000000, 0.000000000000000000, 0.000000000000000000 ) ) ;
#25843 = DIRECTION ( 'NONE',  ( 0.000000000000000000, 0.000000000000000000, 1.000000000000000000 ) ) ;
#25844 = DIRECTION ( 'NONE',  ( 1.343011723336882952E-16, -1.000000000000000000, 0.000000000000000000 ) ) ;
#25845 = PRODUCT_DEFINITION_CONTEXT ( 'detailed design', #1897, 'design' ) ;
#25846 = VECTOR ( 'NONE', #10754, 1000.000000000000000 ) ;
#25847 = CYLINDRICAL_SURFACE ( 'NONE', #72154, 31.99999999999998579 ) ;
#25848 = ORIENTED_EDGE ( 'NONE', *, *, #33882, .T. ) ;
#25849 = CARTESIAN_POINT ( 'NONE',  ( -92.69370383062505425, 88.66845928578038638, 82.28739583420048120 ) ) ;
#25850 = DIRECTION ( 'NONE',  ( 1.343011723336883198E-16, -1.000000000000000000, 0.000000000000000000 ) ) ;
#25851 = AXIS2_PLACEMENT_3D ( 'NONE', #9573, #3221, #43442 ) ;
#25852 = DIRECTION ( 'NONE',  ( 0.000000000000000000, 0.000000000000000000, 1.000000000000000000 ) ) ;
#25853 = VERTEX_POINT ( 'NONE', #74254 ) ;
#25854 = LINE ( 'NONE', #71708, #69109 ) ;
#25855 = DIRECTION ( 'NONE',  ( -1.000000000000000000, 0.000000000000000000, 0.000000000000000000 ) ) ;
#25856 = FACE_OUTER_BOUND ( 'NONE', #32047, .T. ) ;
#25857 = EDGE_CURVE ( 'NONE', #10249, #51767, #47449, .T. ) ;
#25858 = AXIS2_PLACEMENT_3D ( 'NONE', #1718, #18589, #58827 ) ;
#25859 = CARTESIAN_POINT ( 'NONE',  ( 97.30629616937498838, -211.3315407142195852, 79.27114583420048177 ) ) ;
#25860 = ADVANCED_FACE ( 'NONE', ( #67883 ), #15639, .F. ) ;
#25861 = EDGE_CURVE ( 'NONE', #1858, #15332, #55824, .T. ) ;
#25862 = VERTEX_POINT ( 'NONE', #9986 ) ;
#25863 = EDGE_CURVE ( 'NONE', #71285, #38604, #10201, .T. ) ;
#25864 = EDGE_LOOP ( 'NONE', ( #26166, #16725 ) ) ;
#25865 = CARTESIAN_POINT ( 'NONE',  ( 4.574237413256328308E-15, 3.992474787516289480E-15, 42.00000000000001421 ) ) ;
#25866 = DIRECTION ( 'NONE',  ( 0.3853207896976523772, -0.9227826878668550226, 0.000000000000000000 ) ) ;
#25867 = ADVANCED_FACE ( 'NONE', ( #45715 ), #10738, .T. ) ;
#25868 = DIRECTION ( 'NONE',  ( 0.000000000000000000, 0.000000000000000000, 1.000000000000000000 ) ) ;
#25869 = EDGE_LOOP ( 'NONE', ( #2845, #27163, #49557, #14885 ) ) ;
#25870 = VECTOR ( 'NONE', #45350, 1000.000000000000000 ) ;
#25871 = CARTESIAN_POINT ( 'NONE',  ( -8.000000000000000000, 1.298024359000872731E-13, 13.10000000000022879 ) ) ;
#25872 = CARTESIAN_POINT ( 'NONE',  ( 97.30629616937498838, -208.6684592857803011, 75.56697916753383026 ) ) ;
#25873 = EDGE_CURVE ( 'NONE', #63717, #2629, #5340, .T. ) ;
#25874 = ORIENTED_EDGE ( 'NONE', *, *, #24768, .T. ) ;
#25875 = DIRECTION ( 'NONE',  ( 0.000000000000000000, -0.7604059656000369261, 0.6494480483301767748 ) ) ;
#25876 = ORIENTED_EDGE ( 'NONE', *, *, #22061, .T. ) ;
#25877 = AXIS2_PLACEMENT_3D ( 'NONE', #63360, #46809, #58439 ) ;
#25878 = ORIENTED_EDGE ( 'NONE', *, *, #48063, .T. ) ;
#25879 = CARTESIAN_POINT ( 'NONE',  ( -3.000000000000000000, -0.9646360437375307573, 23.52805723605590060 ) ) ;
#25880 = SURFACE_STYLE_USAGE ( .BOTH. , #37913 ) ;
#25881 = CARTESIAN_POINT ( 'NONE',  ( -12.49999999999999645, 0.000000000000000000, -43.79999999999998295 ) ) ;
#25882 = VECTOR ( 'NONE', #20931, 1000.000000000000000 ) ;
#25883 = ORIENTED_EDGE ( 'NONE', *, *, #1253, .T. ) ;
#25884 = DIRECTION ( 'NONE',  ( 1.000000000000000000, 0.000000000000000000, 0.000000000000000000 ) ) ;
#25885 = CARTESIAN_POINT ( 'NONE',  ( 96.32499999999998863, -207.7050326799711968, 83.51770833506763836 ) ) ;
#25886 = CARTESIAN_POINT ( 'NONE',  ( 94.99999999999998579, 93.05995642670504253, 86.66624999999999091 ) ) ;
#25887 = ORIENTED_EDGE ( 'NONE', *, *, #59928, .T. ) ;
#25888 = LINE ( 'NONE', #66132, #43090 ) ;
#25889 = CARTESIAN_POINT ( 'NONE',  ( -94.99999999999997158, -213.0599564267049857, 88.96812500173430749 ) ) ;
#25890 = CIRCLE ( 'NONE', #34323, 82.00000000000000000 ) ;
#25891 = VERTEX_POINT ( 'NONE', #63011 ) ;
#25892 = AXIS2_PLACEMENT_3D ( 'NONE', #37677, #9831, #21095 ) ;
#25893 = ORIENTED_EDGE ( 'NONE', *, *, #1512, .F. ) ;
#25894 = CARTESIAN_POINT ( 'NONE',  ( -95.00000000000002842, 92.66308142843932671, 87.73781250086715033 ) ) ;
#25895 = CARTESIAN_POINT ( 'NONE',  ( 97.30629616937498838, 88.66845928578037217, 82.28739583420048120 ) ) ;
#25896 = ADVANCED_FACE ( 'NONE', ( #34400 ), #68998, .T. ) ;
#25897 = EDGE_LOOP ( 'NONE', ( #23773, #51283, #56161, #19837 ) ) ;
#25898 = CARTESIAN_POINT ( 'NONE',  ( 97.64999999999999147, 90.00000000000002842, 84.04687500173430692 ) ) ;
#25899 = DIRECTION ( 'NONE',  ( -1.000000000000000000, 0.000000000000000000, 0.000000000000000000 ) ) ;
#25900 = ORIENTED_EDGE ( 'NONE', *, *, #54992, .T. ) ;
#25901 = CARTESIAN_POINT ( 'NONE',  ( -20.63750000000001350, -2.447635064697195611E-13, -20.20000000000038298 ) ) ;
#25902 = EDGE_CURVE ( 'NONE', #21235, #7032, #71468, .T. ) ;
#25903 = EDGE_CURVE ( 'NONE', #47350, #23224, #54695, .T. ) ;
#25904 = VERTEX_POINT ( 'NONE', #23871 ) ;
#25905 = ORIENTED_EDGE ( 'NONE', *, *, #4426, .T. ) ;
#25906 = ORIENTED_EDGE ( 'NONE', *, *, #48196, .T. ) ;
#25907 = DIRECTION ( 'NONE',  ( -1.000000000000000000, -0.000000000000000000, 0.000000000000000000 ) ) ;
#25908 = DIRECTION ( 'NONE',  ( -0.5200609990132993854, -0.8541291221503275466, 0.000000000000000000 ) ) ;
#25909 = CARTESIAN_POINT ( 'NONE',  ( -92.35000000000005116, 88.47002178664754979, 83.91458333333333997 ) ) ;
#25910 = ORIENTED_EDGE ( 'NONE', *, *, #44102, .F. ) ;
#25911 = EDGE_CURVE ( 'NONE', #70942, #73391, #34781, .T. ) ;
#25912 = CARTESIAN_POINT ( 'NONE',  ( 4.250000000000000000, -13.95926121303099343, 0.000000000000000000 ) ) ;
#25913 = CARTESIAN_POINT ( 'NONE',  ( 92.34999999999999432, 90.00000000000002842, 88.80937500173430976 ) ) ;
#25914 = ORIENTED_EDGE ( 'NONE', *, *, #34296, .F. ) ;
#25915 = FACE_OUTER_BOUND ( 'NONE', #23594, .T. ) ;
#25916 = CARTESIAN_POINT ( 'NONE',  ( -97.30629616937495996, -209.9999999999999716, 80.11781250086713158 ) ) ;
#25917 = ORIENTED_EDGE ( 'NONE', *, *, #63957, .F. ) ;
#25918 = CARTESIAN_POINT ( 'NONE',  ( -0.0004442498525516064278, 0.001194404164626844313, -85.59999999999999432 ) ) ;
#25919 = DIRECTION ( 'NONE',  ( -1.000000000000000000, 0.000000000000000000, 0.000000000000000000 ) ) ;
#25920 = DIRECTION ( 'NONE',  ( -1.000000000000000000, -0.000000000000000000, -0.000000000000000000 ) ) ;
#25921 = DIRECTION ( 'NONE',  ( -1.000000000000000000, 0.000000000000000000, 0.000000000000000000 ) ) ;
#25922 = DIRECTION ( 'NONE',  ( -1.000000000000000000, -0.000000000000000000, -0.000000000000000000 ) ) ;
#25923 = CARTESIAN_POINT ( 'NONE',  ( -92.34999999999999432, -209.9999999999999716, 90.00000000000000000 ) ) ;
#25924 = CARTESIAN_POINT ( 'NONE',  ( 97.30629616937498838, 88.66845928578035796, 89.27239583420048064 ) ) ;
#25925 = DIRECTION ( 'NONE',  ( 0.000000000000000000, -0.2334453638559126909, 0.9723699203976748917 ) ) ;
#25926 = CARTESIAN_POINT ( 'NONE',  ( -92.35000000000000853, 88.47002178664753558, 87.08958333333333712 ) ) ;
#25927 = DIRECTION ( 'NONE',  ( -1.000000000000000000, 0.000000000000000000, -0.000000000000000000 ) ) ;
#25928 = CARTESIAN_POINT ( 'NONE',  ( -92.69370383062502583, 89.06967028092473981, 74.68334033237941583 ) ) ;
#25929 = LINE ( 'NONE', #65794, #5833 ) ;
#25930 = LINE ( 'NONE', #48858, #13431 ) ;
#25931 = CARTESIAN_POINT ( 'NONE',  ( 3.000000000000000000, -2.935248768560059673, 2.602085213965210642E-15 ) ) ;
#25932 = VECTOR ( 'NONE', #45996, 1000.000000000000114 ) ;
#25933 = CARTESIAN_POINT ( 'NONE',  ( -3.000000000000000000, -19.89357724625003598, 12.59942793731059574 ) ) ;
#25935 = FACE_OUTER_BOUND ( 'NONE', #1786, .T. ) ;
#25934 = AXIS2_PLACEMENT_3D ( 'NONE', #28293, #63276, #28665 ) ;
#25936 = FACE_OUTER_BOUND ( 'NONE', #68836, .T. ) ;
#25937 = CARTESIAN_POINT ( 'NONE',  ( -23.25244084006223133, -132.7111759872722416, 2.500000000000000000 ) ) ;
#25938 = AXIS2_PLACEMENT_3D ( 'NONE', #6462, #63975, #52680 ) ;
#25939 = DIRECTION ( 'NONE',  ( 0.000000000000000000, 0.000000000000000000, 1.000000000000000000 ) ) ;
#25940 = CARTESIAN_POINT ( 'NONE',  ( -93.67499999999998295, -207.7050326799711968, 88.51833333333333087 ) ) ;
#25941 = CARTESIAN_POINT ( 'NONE',  ( -3.000000000000000000, -13.04903810567675038, 19.60159698893425428 ) ) ;
#25942 = PRODUCT_DEFINITION_SHAPE ( 'NONE', 'NONE',  #49042 ) ;
#25943 = CIRCLE ( 'NONE', #57199, 0.2999999999999999334 ) ;
#25944 = VECTOR ( 'NONE', #31553, 1000.000000000000000 ) ;
#25945 =( BOUNDED_CURVE ( )  B_SPLINE_CURVE ( 2, ( #72340, #56554, #73447, #66711, #21952, #4315, #56165 ),
 .UNSPECIFIED., .F., .F. ) 
 B_SPLINE_CURVE_WITH_KNOTS ( ( 3, 2, 2, 3 ),
 ( 0.9166666666666662966, 0.9236111111111108274, 0.9305555555555551361, 0.9374999999999995559 ),
 .UNSPECIFIED. ) 
 CURVE ( )  GEOMETRIC_REPRESENTATION_ITEM ( )  RATIONAL_B_SPLINE_CURVE ( ( 1.000000000000006439, 0.8660254037844322683, 1.000000000000000000, 0.8660254037844387076, 1.000000000000000000, 0.8660254037844472563, 0.9999999999999914513 ) ) 
 REPRESENTATION_ITEM ( '' )  );
#25946 = ORIENTED_EDGE ( 'NONE', *, *, #50756, .F. ) ;
#25947 = LINE ( 'NONE', #56003, #38355 ) ;
#25948 = CARTESIAN_POINT ( 'NONE',  ( 14.59956846177685996, -138.4757300459248484, 5.500000000000000000 ) ) ;
#25949 = CARTESIAN_POINT ( 'NONE',  ( 0.000000000000000000, 34.44570377933695227, -69.42325613327405165 ) ) ;
#25950 = LINE ( 'NONE', #19564, #31727 ) ;
#25951 = EDGE_CURVE ( 'NONE', #57324, #2620, #67908, .T. ) ;
#25952 = EDGE_CURVE ( 'NONE', #59706, #12127, #58084, .T. ) ;
#25953 = AXIS2_PLACEMENT_3D ( 'NONE', #18828, #64714, #13196 ) ;
#25954 = ADVANCED_FACE ( 'NONE', ( #12941 ), #606, .T. ) ;
#25955 = ORIENTED_EDGE ( 'NONE', *, *, #36644, .T. ) ;
#25956 = EDGE_CURVE ( 'NONE', #9715, #14143, #44180, .T. ) ;
#25957 = CARTESIAN_POINT ( 'NONE',  ( 11.99999999999999822, -75.11725578898466438, -2.956366410621452001 ) ) ;
#25958 = DIRECTION ( 'NONE',  ( 0.000000000000000000, 0.000000000000000000, -1.000000000000000000 ) ) ;
#25959 = ORIENTED_EDGE ( 'NONE', *, *, #10383, .F. ) ;
#25960 = CARTESIAN_POINT ( 'NONE',  ( 97.30629616937498838, -208.6684592857803295, 81.75822916753381264 ) ) ;
#25961 = CYLINDRICAL_SURFACE ( 'NONE', #5935, 77.49899999999999523 ) ;
#25962 = ORIENTED_EDGE ( 'NONE', *, *, #39888, .F. ) ;
#25963 = CARTESIAN_POINT ( 'NONE',  ( 95.00000000000000000, -212.6630814284392557, 86.78531250086716398 ) ) ;
#25964 = ORIENTED_EDGE ( 'NONE', *, *, #42422, .T. ) ;
#25965 = DIRECTION ( 'NONE',  ( 0.000000000000000000, 0.000000000000000000, -1.000000000000000000 ) ) ;
#25966 = ORIENTED_EDGE ( 'NONE', *, *, #35127, .F. ) ;
#25967 = CARTESIAN_POINT ( 'NONE',  ( -96.15314808468751551, 88.00268892867056536, 77.20739583420048291 ) ) ;
#25968 = ORIENTED_EDGE ( 'NONE', *, *, #1330, .F. ) ;
#25969 = ORIENTED_EDGE ( 'NONE', *, *, #34957, .F. ) ;
#25970 = CARTESIAN_POINT ( 'NONE',  ( 0.000000000000000000, 17.80606268964540106, 33.00180498840052934 ) ) ;
#25971 = VERTEX_POINT ( 'NONE', #47174 ) ;
#25972 = DIRECTION ( 'NONE',  ( -0.6575728627325957421, 0.7533909544171994987, 0.000000000000000000 ) ) ;
#25973 = CARTESIAN_POINT ( 'NONE',  ( 96.32499999999998863, -212.2949673200287179, 79.41666666666665719 ) ) ;
#25974 = EDGE_CURVE ( 'NONE', #64000, #25226, #53454, .T. ) ;
#25975 = ORIENTED_EDGE ( 'NONE', *, *, #7550, .T. ) ;
#25976 = DIRECTION ( 'NONE',  ( 1.000000000000000000, 0.000000000000000000, 0.000000000000000000 ) ) ;
#25977 = VERTEX_POINT ( 'NONE', #41166 ) ;
#25978 = CARTESIAN_POINT ( 'NONE',  ( 10.00000000000000000, 0.000000000000000000, 0.000000000000000000 ) ) ;
#25979 = VECTOR ( 'NONE', #39147, 1000.000000000000000 ) ;
#25980 = VERTEX_POINT ( 'NONE', #12583 ) ;
#25981 = ORIENTED_EDGE ( 'NONE', *, *, #17808, .F. ) ;
#25982 = EDGE_LOOP ( 'NONE', ( #32653, #12639, #20215, #68453 ) ) ;
#25983 = CARTESIAN_POINT ( 'NONE',  ( 95.00000000000000000, -207.3369185715606307, 79.32406250086714294 ) ) ;
#25985 = EDGE_CURVE ( 'NONE', #6755, #38459, #36657, .T. ) ;
#25984 = LINE ( 'NONE', #7596, #65270 ) ;
#25986 = EDGE_CURVE ( 'NONE', #71078, #58524, #35480, .T. ) ;
#25987 = CARTESIAN_POINT ( 'NONE',  ( -20.63749999999998863, 1.408645127833826896E-13, 15.80000000000026539 ) ) ;
#25988 = VERTEX_POINT ( 'NONE', #35876 ) ;
#25989 = EDGE_LOOP ( 'NONE', ( #71181, #44969, #53087, #59662 ) ) ;
#25990 = CIRCLE ( 'NONE', #7960, 16.00000000000000711 ) ;
#25991 = FACE_OUTER_BOUND ( 'NONE', #59644, .T. ) ;
#25992 = VERTEX_POINT ( 'NONE', #30243 ) ;
#25993 = AXIS2_PLACEMENT_3D ( 'NONE', #32168, #38575, #72754 ) ;
#25994 = DIRECTION ( 'NONE',  ( -1.000000000000000000, 0.000000000000000000, -0.000000000000000000 ) ) ;
#25995 = DIRECTION ( 'NONE',  ( 0.8774505977381978905, 0.4796670183876304283, -0.000000000000000000 ) ) ;
#25996 = CARTESIAN_POINT ( 'NONE',  ( -93.84685191531254134, 91.99731107132950569, 78.79489583420048859 ) ) ;
#25997 = ORIENTED_EDGE ( 'NONE', *, *, #51187, .T. ) ;
#25998 = AXIS2_PLACEMENT_3D ( 'NONE', #62394, #27789, #73270 ) ;
#25999 = CARTESIAN_POINT ( 'NONE',  ( 97.30629616937498838, 91.33154071421968467, 77.94822916753381037 ) ) ;
#26000 = VERTEX_POINT ( 'NONE', #53182 ) ;
#26001 = FACE_OUTER_BOUND ( 'NONE', #54630, .T. ) ;
#26002 = DIRECTION ( 'NONE',  ( -1.000000000000000000, -0.000000000000000000, -0.000000000000000000 ) ) ;
#26003 = DIRECTION ( 'NONE',  ( 1.000000000000000000, -7.571541139944063212E-15, -2.603472992745718826E-14 ) ) ;
#26004 = CARTESIAN_POINT ( 'NONE',  ( 0.000000000000000000, 0.000000000000000000, 0.000000000000000000 ) ) ;
#26005 = DIRECTION ( 'NONE',  ( -0.000000000000000000, 0.9510565162951539753, -0.3090169943749460635 ) ) ;
#26006 = CARTESIAN_POINT ( 'NONE',  ( -97.30629616937495996, -209.9999999999999716, 83.92781250086714806 ) ) ;
#26007 = DIRECTION ( 'NONE',  ( 0.000000000000000000, 0.000000000000000000, 1.000000000000000000 ) ) ;
#26008 = CARTESIAN_POINT ( 'NONE',  ( 0.000000000000000000, -81.96053171279901051, -2.543863470249259962 ) ) ;
#26009 = DIRECTION ( 'NONE',  ( -1.000000000000000000, 0.000000000000000000, 0.000000000000000000 ) ) ;
#26010 = ORIENTED_EDGE ( 'NONE', *, *, #34623, .T. ) ;
#26011 = CIRCLE ( 'NONE', #12804, 82.00000000000000000 ) ;
#26012 = ORIENTED_EDGE ( 'NONE', *, *, #13435, .T. ) ;
#26013 = CARTESIAN_POINT ( 'NONE',  ( 12.75000000000000000, -120.0000000000000000, -80.00000000000001421 ) ) ;
#26014 = CARTESIAN_POINT ( 'NONE',  ( 10.00000000000000000, 0.000000000000000000, 0.000000000000000000 ) ) ;
#26015 = CARTESIAN_POINT ( 'NONE',  ( 11.99999999999999822, -75.16055320797016748, -18.89407956138335365 ) ) ;
#26016 = CARTESIAN_POINT ( 'NONE',  ( -96.15314808468752972, 91.99731107132950569, 85.09197916753380753 ) ) ;
#26017 = CARTESIAN_POINT ( 'NONE',  ( 3.000000000000000000, 2.201436576420041202, -1.271000000000003016 ) ) ;
#26018 = CARTESIAN_POINT ( 'NONE',  ( 97.64999999999999147, -209.9999999999999716, 82.69749999999999091 ) ) ;
#26019 = LINE ( 'NONE', #15766, #48096 ) ;
#26020 = VERTEX_POINT ( 'NONE', #51703 ) ;
#26021 = FACE_OUTER_BOUND ( 'NONE', #16355, .T. ) ;
#26022 = DIRECTION ( 'NONE',  ( -1.000000000000000000, -0.000000000000000000, 0.000000000000000000 ) ) ;
#26023 = VECTOR ( 'NONE', #58774, 1000.000000000000000 ) ;
#26024 = CARTESIAN_POINT ( 'NONE',  ( 10.00000000000000000, -6.555932627142676772, 37.01155633439056203 ) ) ;
#26025 = CARTESIAN_POINT ( 'NONE',  ( -4.282125186551308360, 3.301216562737181892, -1.327869168827478408 ) ) ;
#26026 = DIRECTION ( 'NONE',  ( 0.000000000000000000, 0.9969173337331276308, 0.07845909572784873220 ) ) ;
#26027 = CARTESIAN_POINT ( 'NONE',  ( -100.0000000000260059, -214.9999999999999716, -74.99999999999349143 ) ) ;
#26028 = CARTESIAN_POINT ( 'NONE',  ( -97.30629616937497417, -211.3315407142195852, 82.23447916753383424 ) ) ;
#26029 = CARTESIAN_POINT ( 'NONE',  ( 97.64999999999601243, 89.99999541993086893, 76.42687486206342840 ) ) ;
#26030 = DIRECTION ( 'NONE',  ( 0.000000000000000000, -0.8910065241883722287, 0.4539904997395382003 ) ) ;
#26031 = PRODUCT_RELATED_PRODUCT_CATEGORY ( 'part', '', ( #55381 ) ) ;
#26032 = ADVANCED_FACE ( 'NONE', ( #251, #46066, #40414 ), #11828, .T. ) ;
#26033 = CARTESIAN_POINT ( 'NONE',  ( -6.170112525937321735, 10.87104923258428180, -44.99999999999998579 ) ) ;
#26034 = DIRECTION ( 'NONE',  ( -1.000000000000000000, 0.000000000000000000, 0.000000000000000000 ) ) ;
#26035 = ORIENTED_EDGE ( 'NONE', *, *, #30626, .F. ) ;
#26036 = DIRECTION ( 'NONE',  ( 0.02332147558787822997, 0.9997280174009349762, 0.000000000000000000 ) ) ;
#26037 = CARTESIAN_POINT ( 'NONE',  ( 0.000000000000000000, -13.04903810567675038, 19.60159698893425428 ) ) ;
#26038 = FACE_OUTER_BOUND ( 'NONE', #50658, .T. ) ;
#26039 = VECTOR ( 'NONE', #51986, 1000.000000000000000 ) ;
#26040 = EDGE_CURVE ( 'NONE', #7975, #23684, #45103, .T. ) ;
#26041 = AXIS2_PLACEMENT_3D ( 'NONE', #22016, #57723, #11111 ) ;
#26042 = CARTESIAN_POINT ( 'NONE',  ( 0.000000000000000000, 0.000000000000000000, 0.000000000000000000 ) ) ;
#26043 = ORIENTED_EDGE ( 'NONE', *, *, #33424, .T. ) ;
#26044 = EDGE_CURVE ( 'NONE', #70238, #60373, #22279, .T. ) ;
#26045 = DIRECTION ( 'NONE',  ( 0.000000000000000000, 0.000000000000000000, 1.000000000000000000 ) ) ;
#26046 = CIRCLE ( 'NONE', #35649, 31.99999999999999645 ) ;
#26047 = DIRECTION ( 'NONE',  ( 1.000000000000000000, 0.000000000000000000, 0.000000000000000000 ) ) ;
#26049 = VERTEX_POINT ( 'NONE', #26453 ) ;
#26048 = AXIS2_PLACEMENT_3D ( 'NONE', #63606, #45195, #16988 ) ;
#26050 = EDGE_CURVE ( 'NONE', #60033, #56046, #63092, .T. ) ;
#26051 = CARTESIAN_POINT ( 'NONE',  ( 10.00000000000000000, 68.27212725128275395, -31.46837873495001503 ) ) ;
#26052 = VERTEX_POINT ( 'NONE', #36255 ) ;
#26053 = CARTESIAN_POINT ( 'NONE',  ( 10.00000000000000000, 17.28742895386084655, 75.54627589209950145 ) ) ;
#26054 = AXIS2_PLACEMENT_3D ( 'NONE', #29933, #57789, #57416 ) ;
#26055 = ORIENTED_EDGE ( 'NONE', *, *, #33361, .T. ) ;
#26056 = ORIENTED_EDGE ( 'NONE', *, *, #63614, .F. ) ;
#26057 = VERTEX_POINT ( 'NONE', #65957 ) ;
#26058 = ORIENTED_EDGE ( 'NONE', *, *, #49748, .F. ) ;
#26059 = CARTESIAN_POINT ( 'NONE',  ( -20.63750000000001350, -2.799353718898444395E-13, -23.50000000000043698 ) ) ;
#26060 = EDGE_CURVE ( 'NONE', #69330, #27263, #48991, .T. ) ;
#26061 = CIRCLE ( 'NONE', #36854, 82.00000000000000000 ) ;
#26062 = EDGE_CURVE ( 'NONE', #68933, #54089, #37386, .T. ) ;
#26063 = ORIENTED_EDGE ( 'NONE', *, *, #5621, .T. ) ;
#26064 = ORIENTED_EDGE ( 'NONE', *, *, #30691, .F. ) ;
#26065 = CARTESIAN_POINT ( 'NONE',  ( 92.69370383062498320, 88.66845928578037217, 75.24947916753383481 ) ) ;
#26066 = DIRECTION ( 'NONE',  ( 0.000000000000000000, 0.000000000000000000, 1.000000000000000000 ) ) ;
#26067 = DIRECTION ( 'NONE',  ( -0.000000000000000000, -0.000000000000000000, -1.000000000000000000 ) ) ;
#26068 = EDGE_LOOP ( 'NONE', ( #49362, #41417, #8184, #67520 ) ) ;
#26069 = ORIENTED_EDGE ( 'NONE', *, *, #46678, .F. ) ;
#26070 = ORIENTED_EDGE ( 'NONE', *, *, #35648, .T. ) ;
#26071 = DIRECTION ( 'NONE',  ( -0.000000000000000000, -0.000000000000000000, 1.000000000000000000 ) ) ;
#26072 = EDGE_LOOP ( 'NONE', ( #67258, #45221, #34382, #21918 ) ) ;
#26073 = CARTESIAN_POINT ( 'NONE',  ( 92.69370383062501162, -208.6684592857803011, 87.04989583420048405 ) ) ;
#26074 = ADVANCED_FACE ( 'NONE', ( #2087 ), #59950, .T. ) ;
#26075 = DIRECTION ( 'NONE',  ( 0.9237280213470682178, 0.3830490080632377725, 0.000000000000000000 ) ) ;
#26076 = CARTESIAN_POINT ( 'NONE',  ( 12.49999999999999822, -120.0000000000000000, 125.0000000000000000 ) ) ;
#26077 = CARTESIAN_POINT ( 'NONE',  ( 10.00000000000000000, 33.00180498840072829, -17.80606268964504935 ) ) ;
#26078 = CARTESIAN_POINT ( 'NONE',  ( -12.00000000000000000, 0.000000000000000000, 0.000000000000000000 ) ) ;
#26079 = CARTESIAN_POINT ( 'NONE',  ( 8.700667342345820288, -98.11853780484867116, 5.500000000000000000 ) ) ;
#26080 = DIRECTION ( 'NONE',  ( -1.000000000000000000, 3.469446951953614189E-15, 0.000000000000000000 ) ) ;
#26081 = CARTESIAN_POINT ( 'NONE',  ( 11.99999999999999822, 2.946379043147425492, -75.11764819372145041 ) ) ;
#26082 = CARTESIAN_POINT ( 'NONE',  ( -94.99999999999997158, -206.9400435732949575, 76.58562500173430010 ) ) ;
#26083 = CARTESIAN_POINT ( 'NONE',  ( -93.84685191531254134, 91.99731107132950569, 88.95489583420049939 ) ) ;
#26084 = ORIENTED_EDGE ( 'NONE', *, *, #4247, .T. ) ;
#26086 = CARTESIAN_POINT ( 'NONE',  ( -93.84685191531254134, 91.99731107132950569, 88.79614583420047325 ) ) ;
#26085 = CARTESIAN_POINT ( 'NONE',  ( 94.99999999999998579, 93.05995642670504253, 74.68062500173429896 ) ) ;
#26087 = VERTEX_POINT ( 'NONE', #47908 ) ;
#26088 = CARTESIAN_POINT ( 'NONE',  ( 94.99999999999998579, 92.66308142843935514, 75.03781250086714749 ) ) ;
#26089 = AXIS2_PLACEMENT_3D ( 'NONE', #37500, #32939, #49863 ) ;
#26090 = CARTESIAN_POINT ( 'NONE',  ( 0.000000000000000000, -21.32104025579135964, 30.84782396557210760 ) ) ;
#26091 = FACE_OUTER_BOUND ( 'NONE', #18040, .T. ) ;
#26092 = CARTESIAN_POINT ( 'NONE',  ( 5.999999999999999112, 33.71516098798741012, 74.74816331893441657 ) ) ;
#26093 = AXIS2_PLACEMENT_3D ( 'NONE', #16178, #21820, #27829 ) ;
#26094 = CARTESIAN_POINT ( 'NONE',  ( 0.000000000000000000, -3.948201729842038432, -23.21447184625298021 ) ) ;
#26095 = CARTESIAN_POINT ( 'NONE',  ( -97.64999999999997726, -211.5299782133524502, 79.89291666666666458 ) ) ;
#26096 = DIRECTION ( 'NONE',  ( -1.000000000000000000, 0.000000000000000000, -0.000000000000000000 ) ) ;
#26097 = VERTEX_POINT ( 'NONE', #19328 ) ;
#26098 = AXIS2_PLACEMENT_3D ( 'NONE', #33485, #73341, #15461 ) ;
#26099 = ORIENTED_EDGE ( 'NONE', *, *, #18154, .F. ) ;
#26100 = VECTOR ( 'NONE', #64056, 1000.000000000000000 ) ;
#26101 = DIRECTION ( 'NONE',  ( -0.000000000000000000, -1.000000000000000000, -0.000000000000000000 ) ) ;
#26102 = LINE ( 'NONE', #9188, #30921 ) ;
#26103 = CARTESIAN_POINT ( 'NONE',  ( -92.35000000000005116, 91.52997821335253548, 86.00479166840096923 ) ) ;
#26104 = CARTESIAN_POINT ( 'NONE',  ( 2.499999999999984457, -73.00000000000001421, -204.9999999999999716 ) ) ;
#26105 = CARTESIAN_POINT ( 'NONE',  ( 0.000000000000000000, 16.83928648764945279, -16.46020748918028076 ) ) ;
#26106 = CARTESIAN_POINT ( 'NONE',  ( 97.64999999999999147, -209.9999999999999716, 89.04749999999999943 ) ) ;
#26107 = EDGE_LOOP ( 'NONE', ( #60759, #74188, #11103, #56239 ) ) ;
#26108 = CARTESIAN_POINT ( 'NONE',  ( -92.69370383062502583, 88.66845928578038638, 82.92239583420045790 ) ) ;
#26109 = EDGE_CURVE ( 'NONE', #52121, #16273, #52279, .T. ) ;
#26110 = CARTESIAN_POINT ( 'NONE',  ( 5.000000000000002665, 81.34940948281351325, -10.30890764327296161 ) ) ;
#26111 = CARTESIAN_POINT ( 'NONE',  ( 10.00000000000000000, 74.65374052328648702, 8.840884882375350529 ) ) ;
#26112 = AXIS2_PLACEMENT_3D ( 'NONE', #50654, #61952, #11542 ) ;
#26113 = FILL_AREA_STYLE_COLOUR ( '', #47830 ) ;
#26114 = CARTESIAN_POINT ( 'NONE',  ( 14.59956846177685996, -138.4757300459248484, 5.500000000000000000 ) ) ;
#26115 = DIRECTION ( 'NONE',  ( 1.000000000000000000, 0.000000000000000000, 0.000000000000000000 ) ) ;
#26116 = LINE ( 'NONE', #26496, #43088 ) ;
#26117 = ADVANCED_FACE ( 'NONE', ( #25354 ), #41490, .F. ) ;
#26118 = CARTESIAN_POINT ( 'NONE',  ( -89.99999999999998579, -124.0000000000000142, -40.00000000000002132 ) ) ;
#26119 = DIRECTION ( 'NONE',  ( 0.000000000000000000, 0.4999999999999929501, 0.8660254037844427044 ) ) ;
#26121 = EDGE_CURVE ( 'NONE', #14707, #16927, #1868, .T. ) ;
#26120 = CIRCLE ( 'NONE', #65730, 82.00000000000000000 ) ;
#26122 = DIRECTION ( 'NONE',  ( 0.000000000000000000, -0.9781476007338070211, 0.2079116908177525425 ) ) ;
#26123 = CARTESIAN_POINT ( 'NONE',  ( 97.30629616937498838, 88.66845928578035796, 84.35114583420050849 ) ) ;
#26124 = EDGE_CURVE ( 'NONE', #67331, #21642, #65212, .T. ) ;
#26125 = CARTESIAN_POINT ( 'NONE',  ( -94.99999999999997158, -207.3369185715606307, 83.29281250086715715 ) ) ;
#26126 = FACE_OUTER_BOUND ( 'NONE', #35617, .T. ) ;
#26127 = ORIENTED_EDGE ( 'NONE', *, *, #44908, .F. ) ;
#26128 = CARTESIAN_POINT ( 'NONE',  ( -96.32499999999996021, -207.7050326799711968, 78.46416666666667084 ) ) ;
#26129 = DIRECTION ( 'NONE',  ( 0.000000000000000000, 0.000000000000000000, 1.000000000000000000 ) ) ;
#26130 = CARTESIAN_POINT ( 'NONE',  ( 93.84685191531249870, -208.0026889286704943, 82.55197916753380127 ) ) ;
#26131 = EDGE_LOOP ( 'NONE', ( #69269, #14037, #9135, #58446 ) ) ;
#26132 = LINE ( 'NONE', #32878, #56296 ) ;
#26133 = EDGE_LOOP ( 'NONE', ( #28478, #25508, #55373, #29321 ) ) ;
#26134 = EDGE_CURVE ( 'NONE', #34322, #19874, #72642, .T. ) ;
#26135 = VECTOR ( 'NONE', #11191, 1000.000000000000000 ) ;
#26136 = DIRECTION ( 'NONE',  ( -1.000000000000000000, -0.000000000000000000, 0.000000000000000000 ) ) ;
#26137 = ORIENTED_EDGE ( 'NONE', *, *, #68326, .F. ) ;
#26138 = CARTESIAN_POINT ( 'NONE',  ( 92.34999999999998010, -208.4700217866474929, 84.23208333333334963 ) ) ;
#26139 = CIRCLE ( 'NONE', #2150, 77.49899999999999523 ) ;
#26140 = VERTEX_POINT ( 'NONE', #19695 ) ;
#26141 = CARTESIAN_POINT ( 'NONE',  ( 96.15314808468748708, -208.0026889286704943, 76.88989583420048746 ) ) ;
#26142 = EDGE_CURVE ( 'NONE', #62606, #7429, #48681, .T. ) ;
#26143 = CARTESIAN_POINT ( 'NONE',  ( -92.34999999999999432, -209.9999999999999716, 80.79249999999998977 ) ) ;
#26144 = EDGE_CURVE ( 'NONE', #47974, #12189, #66328, .T. ) ;
#26145 = DIRECTION ( 'NONE',  ( 0.000000000000000000, 0.000000000000000000, 1.000000000000000000 ) ) ;
#26146 =( BOUNDED_CURVE ( )  B_SPLINE_CURVE ( 2, ( #68122, #4988, #44457, #44829, #15126, #38438, #27891, #50816, #32412 ),
 .UNSPECIFIED., .F., .F. ) 
 B_SPLINE_CURVE_WITH_KNOTS ( ( 3, 2, 2, 2, 3 ),
 ( 0.8043570860654228882, 0.8043572716605900119, 0.8114130372014725090, 0.8184688027423547840, 0.8255245790564498254 ),
 .UNSPECIFIED. ) 
 CURVE ( )  GEOMETRIC_REPRESENTATION_ITEM ( )  RATIONAL_B_SPLINE_CURVE ( ( 0.9999929520380519410, 0.9999964759263285652, 1.000000000000000000, 0.8660254037844387076, 1.000000000000000000, 0.8660254037844387076, 1.000000000000000000, 0.8660254037844387076, 1.000000000000000000 ) ) 
 REPRESENTATION_ITEM ( '' )  );
#26147 = CARTESIAN_POINT ( 'NONE',  ( 10.00000000000000000, -72.35432306680469594, -20.40083707022958848 ) ) ;
#26148 = CARTESIAN_POINT ( 'NONE',  ( -16.06301359042743115, -102.7814171781257357, 5.500000000000000000 ) ) ;
#26149 = ADVANCED_FACE ( 'NONE', ( #65583 ), #36998, .F. ) ;
#26150 = CARTESIAN_POINT ( 'NONE',  ( 0.000000000000000000, 0.000000000000000000, 0.000000000000000000 ) ) ;
#26151 = CARTESIAN_POINT ( 'NONE',  ( 95.00000000000000000, -213.0599564267049857, 81.26874999999999716 ) ) ;
#26152 = EDGE_LOOP ( 'NONE', ( #64775, #68533, #36739, #35500 ) ) ;
#26153 = ORIENTED_EDGE ( 'NONE', *, *, #7795, .T. ) ;
#26154 = VERTEX_POINT ( 'NONE', #20064 ) ;
#26155 = ORIENTED_EDGE ( 'NONE', *, *, #71795, .F. ) ;
#26156 = DIRECTION ( 'NONE',  ( -1.000000000000000000, 0.000000000000000000, -0.000000000000000000 ) ) ;
#26157 = AXIS2_PLACEMENT_3D ( 'NONE', #58519, #63443, #35221 ) ;
#26158 = CARTESIAN_POINT ( 'NONE',  ( -95.00000000000002842, 87.33691857156074434, 83.61031250086716682 ) ) ;
#26159 = CARTESIAN_POINT ( 'NONE',  ( 11.99999999999999822, 75.16055320797030959, 18.89407956138283851 ) ) ;
#26160 = VECTOR ( 'NONE', #5590, 1000.000000000000000 ) ;
#26161 = DIRECTION ( 'NONE',  ( 1.000000000000000000, 0.000000000000000000, 0.000000000000000000 ) ) ;
#26162 = CARTESIAN_POINT ( 'NONE',  ( 97.64999999999999147, 90.00000000000002842, 75.71250000000000568 ) ) ;
#26163 = CIRCLE ( 'NONE', #43165, 15.99999999999999645 ) ;
#26164 = DIRECTION ( 'NONE',  ( -1.000000000000000000, 0.000000000000000000, 0.000000000000000000 ) ) ;
#26165 = VECTOR ( 'NONE', #19277, 1000.000000000000000 ) ;
#26166 = ORIENTED_EDGE ( 'NONE', *, *, #11360, .T. ) ;
#26167 = CARTESIAN_POINT ( 'NONE',  ( -94.99999999999997158, -206.9400435732949575, 86.74562500173429669 ) ) ;
#26168 = VERTEX_POINT ( 'NONE', #5404 ) ;
#26169 = CARTESIAN_POINT ( 'NONE',  ( 0.000000000000000000, 63.97538442413426907, 51.29473840253247374 ) ) ;
#26170 = ORIENTED_EDGE ( 'NONE', *, *, #17094, .T. ) ;
#26171 = CARTESIAN_POINT ( 'NONE',  ( -96.32500000000001705, 92.29496732002878900, 82.35354166840096468 ) ) ;
#26172 = AXIS2_PLACEMENT_3D ( 'NONE', #59433, #12083, #19202 ) ;
#26173 = ORIENTED_EDGE ( 'NONE', *, *, #45018, .T. ) ;
#26174 = CARTESIAN_POINT ( 'NONE',  ( 92.69370383062498320, 90.00000000000002842, 87.89656250086714806 ) ) ;
#26175 = PLANE ( 'NONE',  #63431 ) ;
#26176 = DIRECTION ( 'NONE',  ( -0.000000000000000000, -0.9135454576426006446, 0.4067366430758008744 ) ) ;
#26177 = CARTESIAN_POINT ( 'NONE',  ( -95.00000000000002842, 86.94004357329504273, 83.88812500173429498 ) ) ;
#26178 = DIRECTION ( 'NONE',  ( 0.000000000000000000, 0.000000000000000000, 1.000000000000000000 ) ) ;
#26179 = DIRECTION ( 'NONE',  ( -1.000000000000000000, 0.000000000000000000, 0.000000000000000000 ) ) ;
#26180 = VERTEX_POINT ( 'NONE', #39229 ) ;
#26181 = CYLINDRICAL_SURFACE ( 'NONE', #32685, 16.00000000000000000 ) ;
#26182 = LINE ( 'NONE', #37489, #21540 ) ;
#26183 = ORIENTED_EDGE ( 'NONE', *, *, #49381, .F. ) ;
#26184 = VERTEX_POINT ( 'NONE', #49385 ) ;
#26185 = DIRECTION ( 'NONE',  ( -1.000000000000000000, 3.061616997868382648E-16, 0.000000000000000000 ) ) ;
#26186 = DIRECTION ( 'NONE',  ( -0.000000000000000000, -0.000000000000000000, 1.000000000000000000 ) ) ;
#26187 = DIRECTION ( 'NONE',  ( -0.000000000000000000, 0.5000000000000004441, 0.8660254037844383745 ) ) ;
#26188 = CARTESIAN_POINT ( 'NONE',  ( -93.84685191531247028, -211.9973110713294489, 85.56822916753381492 ) ) ;
#26189 = EDGE_LOOP ( 'NONE', ( #66950, #72950, #65321, #48706 ) ) ;
#26190 = FACE_OUTER_BOUND ( 'NONE', #45080, .T. ) ;
#26191 = ORIENTED_EDGE ( 'NONE', *, *, #36589, .F. ) ;
#26192 = CIRCLE ( 'NONE', #68230, 31.99999999999999289 ) ;
#26193 = CIRCLE ( 'NONE', #72980, 2.500000000000000444 ) ;
#26194 = ADVANCED_FACE ( 'NONE', ( #16663 ), #9902, .T. ) ;
#26195 = DIRECTION ( 'NONE',  ( -1.000000000000000000, 0.000000000000000000, -0.000000000000000000 ) ) ;
#26196 = CYLINDRICAL_SURFACE ( 'NONE', #29910, 31.99999999999998579 ) ;
#26197 = VECTOR ( 'NONE', #65892, 1000.000000000000000 ) ;
#26198 = DIRECTION ( 'NONE',  ( -1.000000000000000000, 0.000000000000000000, 0.000000000000000000 ) ) ;
#26199 = CARTESIAN_POINT ( 'NONE',  ( 93.84685191531248449, 88.00268892867053694, 79.58864583420047722 ) ) ;
#26200 = CIRCLE ( 'NONE', #35808, 12.49999999999999822 ) ;
#26201 = DIRECTION ( 'NONE',  ( -1.000000000000000000, 0.000000000000000000, 0.000000000000000000 ) ) ;
#26202 = CARTESIAN_POINT ( 'NONE',  ( 97.65000000000000568, 91.52997821335252127, 86.63979166840096013 ) ) ;
#26203 = EDGE_CURVE ( 'NONE', #70758, #8427, #19842, .T. ) ;
#26204 = LINE ( 'NONE', #31844, #44565 ) ;
#26205 = DIRECTION ( 'NONE',  ( 0.000000000000000000, 0.8910065241883688980, -0.4539904997395447506 ) ) ;
#26206 = CARTESIAN_POINT ( 'NONE',  ( 0.000000000000000000, -70.52718814184277107, 26.02418014898285037 ) ) ;
#26207 = EDGE_CURVE ( 'NONE', #17536, #66848, #46277, .T. ) ;
#26208 = DIRECTION ( 'NONE',  ( -1.000000000000000000, 0.000000000000000000, 0.000000000000000000 ) ) ;
#26209 = CARTESIAN_POINT ( 'NONE',  ( 0.000000000000000000, -29.81001611431024045, 22.74946021919122430 ) ) ;
#26210 = EDGE_CURVE ( 'NONE', #60556, #30694, #15168, .T. ) ;
#26211 = CARTESIAN_POINT ( 'NONE',  ( -96.32500000000001705, 87.70503267997129626, 78.12020833506763040 ) ) ;
#26212 = CIRCLE ( 'NONE', #49024, 82.00000000000000000 ) ;
#26213 = ORIENTED_EDGE ( 'NONE', *, *, #28341, .T. ) ;
#26214 = CARTESIAN_POINT ( 'NONE',  ( -96.15314808468752972, 91.99731107132950569, 81.91697916753381037 ) ) ;
#26215 = CARTESIAN_POINT ( 'NONE',  ( -15.44521549751111422, -137.7748507232956001, 2.500000000000000000 ) ) ;
#26216 = AXIS2_PLACEMENT_3D ( 'NONE', #50384, #54922, #4182 ) ;
#26217 = VECTOR ( 'NONE', #40066, 1000.000000000000114 ) ;
#26218 = CIRCLE ( 'NONE', #65837, 77.49900000000000944 ) ;
#26219 = AXIS2_PLACEMENT_3D ( 'NONE', #36473, #64326, #13177 ) ;
#26220 = DIRECTION ( 'NONE',  ( -1.000000000000000000, -0.000000000000000000, -0.000000000000000000 ) ) ;
#26221 = ORIENTED_EDGE ( 'NONE', *, *, #26567, .F. ) ;
#26222 = AXIS2_PLACEMENT_3D ( 'NONE', #60908, #26682, #71427 ) ;
#26223 = CARTESIAN_POINT ( 'NONE',  ( 0.000000000000000000, 30.80686688397010542, 21.53537804866092387 ) ) ;
#26224 = CARTESIAN_POINT ( 'NONE',  ( 0.000000000000000000, 0.000000000000000000, 0.000000000000000000 ) ) ;
#26225 = ADVANCED_FACE ( 'NONE', ( #61792 ), #45245, .T. ) ;
#26226 = PLANE ( 'NONE',  #46719 ) ;
#26227 = DIRECTION ( 'NONE',  ( 0.000000000000000000, 0.000000000000000000, 1.000000000000000000 ) ) ;
#26228 = CARTESIAN_POINT ( 'NONE',  ( 95.00000000000000000, -212.6630814284392557, 79.80031250086715033 ) ) ;
#26229 = VERTEX_POINT ( 'NONE', #20813 ) ;
#26230 = ORIENTED_EDGE ( 'NONE', *, *, #60093, .F. ) ;
#26231 = ADVANCED_FACE ( 'NONE', ( #10645 ), #56895, .F. ) ;
#26232 = DIRECTION ( 'NONE',  ( 0.000000000000000000, 0.000000000000000000, 1.000000000000000000 ) ) ;
#26233 = EDGE_CURVE ( 'NONE', #49041, #28732, #45220, .T. ) ;
#26234 = CARTESIAN_POINT ( 'NONE',  ( 0.000000000000000000, -68.55367621811110723, -44.99326035066126650 ) ) ;
#26235 = DIRECTION ( 'NONE',  ( -4.476705744456276711E-17, 1.000000000000000000, -0.000000000000000000 ) ) ;
#26236 = CARTESIAN_POINT ( 'NONE',  ( 93.84685191531249870, -208.0026889286704943, 76.99572916753382401 ) ) ;
#26237 = AXIS2_PLACEMENT_3D ( 'NONE', #13634, #2411, #54608 ) ;
#26238 = AXIS2_PLACEMENT_3D ( 'NONE', #37429, #37793, #65623 ) ;
#26239 = ORIENTED_EDGE ( 'NONE', *, *, #3087, .T. ) ;
#26240 = DIRECTION ( 'NONE',  ( 0.000000000000000000, 0.000000000000000000, 1.000000000000000000 ) ) ;
#26241 = VERTEX_POINT ( 'NONE', #10274 ) ;
#26242 = EDGE_LOOP ( 'NONE', ( #36360, #40407 ) ) ;
#26243 = DIRECTION ( 'NONE',  ( 0.000000000000000000, -0.9781476007338040235, -0.2079116908177671419 ) ) ;
#26244 = AXIS2_PLACEMENT_3D ( 'NONE', #69580, #58300, #28603 ) ;
#26245 = CARTESIAN_POINT ( 'NONE',  ( 10.00000000000000000, 10.74501242461333028, -35.92658777277499382 ) ) ;
#26246 = AXIS2_PLACEMENT_3D ( 'NONE', #25948, #8289, #19562 ) ;
#26247 = EDGE_LOOP ( 'NONE', ( #70159, #45882, #28265, #52836 ) ) ;
#26248 = FACE_OUTER_BOUND ( 'NONE', #32902, .T. ) ;
#26249 = CARTESIAN_POINT ( 'NONE',  ( 95.00000000000000000, -206.9400435732949575, 81.03062500173430749 ) ) ;
#26250 = CARTESIAN_POINT ( 'NONE',  ( 96.32499999999997442, 92.29496732002878900, 85.97833333333332462 ) ) ;
#26251 = ORIENTED_EDGE ( 'NONE', *, *, #1176, .F. ) ;
#26252 = CARTESIAN_POINT ( 'NONE',  ( 10.00000000000000000, 0.000000000000000000, 0.000000000000000000 ) ) ;
#26253 = CARTESIAN_POINT ( 'NONE',  ( 10.00000000000000000, -26.79245525562738095, 32.34446384429961796 ) ) ;
#26254 = ORIENTED_EDGE ( 'NONE', *, *, #72617, .F. ) ;
#26255 = DIRECTION ( 'NONE',  ( 0.000000000000000000, 0.000000000000000000, 1.000000000000000000 ) ) ;
#26256 = CARTESIAN_POINT ( 'NONE',  ( -95.00000000000002842, 92.66308142843932671, 88.37281250086715545 ) ) ;
#26257 = CARTESIAN_POINT ( 'NONE',  ( 92.69370383062498320, 88.66845928578037217, 80.17072916753379275 ) ) ;
#26258 = VERTEX_POINT ( 'NONE', #49743 ) ;
#26259 = VECTOR ( 'NONE', #39249, 1000.000000000000114 ) ;
#26260 = AXIS2_PLACEMENT_3D ( 'NONE', #2662, #36087, #59767 ) ;
#26261 = LINE ( 'NONE', #66142, #14397 ) ;
#26262 = EDGE_LOOP ( 'NONE', ( #48076, #44551, #41257, #40395, #52796, #9709 ) ) ;
#26263 = CARTESIAN_POINT ( 'NONE',  ( -0.2999999999999947153, 0.000000000000000000, 0.000000000000000000 ) ) ;
#26264 = VERTEX_POINT ( 'NONE', #66684 ) ;
#26265 = AXIS2_PLACEMENT_3D ( 'NONE', #7130, #19141, #30776 ) ;
#26266 = ORIENTED_EDGE ( 'NONE', *, *, #12454, .F. ) ;
#26267 = ORIENTED_EDGE ( 'NONE', *, *, #12038, .F. ) ;
#26268 = CARTESIAN_POINT ( 'NONE',  ( 92.34999999999999432, 90.00000000000002842, 75.47437500173430180 ) ) ;
#26269 = AXIS2_PLACEMENT_3D ( 'NONE', #73673, #27818, #67307 ) ;
#26270 = CIRCLE ( 'NONE', #32277, 1.000000000000000888 ) ;
#26271 = ORIENTED_EDGE ( 'NONE', *, *, #51021, .T. ) ;
#26272 = DIRECTION ( 'NONE',  ( -1.000000000000000000, -0.000000000000000000, -0.000000000000000000 ) ) ;
#26273 = ADVANCED_FACE ( 'NONE', ( #38105 ), #50106, .F. ) ;
#26274 = CIRCLE ( 'NONE', #58700, 77.49899999999999523 ) ;
#26275 = DIRECTION ( 'NONE',  ( -1.000000000000000000, 0.000000000000000000, 0.000000000000000000 ) ) ;
#26276 = ORIENTED_EDGE ( 'NONE', *, *, #54328, .T. ) ;
#26277 = FACE_OUTER_BOUND ( 'NONE', #52222, .T. ) ;
#26278 = CARTESIAN_POINT ( 'NONE',  ( -97.30629616937497417, -208.6684592857803011, 80.69989583420048973 ) ) ;
#26279 = ORIENTED_EDGE ( 'NONE', *, *, #69758, .F. ) ;
#26280 = CARTESIAN_POINT ( 'NONE',  ( 0.000000000000000000, 75.11764819372142199, 2.946379043147685728 ) ) ;
#26281 = CARTESIAN_POINT ( 'NONE',  ( 10.00000000000000000, -21.32104025579091910, -30.84782396557241313 ) ) ;
#26282 = CARTESIAN_POINT ( 'NONE',  ( 0.000000000000000000, 0.000000000000000000, 0.000000000000000000 ) ) ;
#26283 = CYLINDRICAL_SURFACE ( 'NONE', #53152, 2.649999999999985700 ) ;
#26284 = ADVANCED_FACE ( 'NONE', ( #44872 ), #5030, .T. ) ;
#26285 = CARTESIAN_POINT ( 'NONE',  ( 5.000000000000002665, -79.10210256391383155, 21.60688246758557796 ) ) ;
#26286 = B_SPLINE_CURVE_WITH_KNOTS ( 'NONE', 3,
 ( #32635, #54835, #49559, #66858, #20988, #67233, #49927, #60855 ),
 .UNSPECIFIED., .F., .F.,
 ( 4, 2, 2, 4 ),
 ( 0.001653806717455033820, 0.002539064216007439964, 0.002981692965283634471, 0.003424321714559829845 ),
 .UNSPECIFIED. ) ;
#26287 = EDGE_CURVE ( 'NONE', #11557, #11811, #66788, .T. ) ;
#26288 = LINE ( 'NONE', #38322, #22915 ) ;
#26289 = CARTESIAN_POINT ( 'NONE',  ( 96.15314808468748708, 91.99731107132950569, 86.89114583420047211 ) ) ;
#26290 = CARTESIAN_POINT ( 'NONE',  ( 97.30629616937497417, -209.9999999999998863, 74.79348190356849102 ) ) ;
#26291 = DIRECTION ( 'NONE',  ( 2.628368902995175337E-16, 1.000000000000000000, 0.000000000000000000 ) ) ;
#26292 = ADVANCED_FACE ( 'NONE', ( #38850 ), #39600, .T. ) ;
#26293 =( BOUNDED_CURVE ( )  B_SPLINE_CURVE ( 2, ( #11688, #70305, #24112, #41389, #64694 ),
 .UNSPECIFIED., .F., .F. ) 
 B_SPLINE_CURVE_WITH_KNOTS ( ( 3, 2, 3 ),
 ( 0.9525283480321509177, 0.9595841135600021721, 0.9629953541049911525 ),
 .UNSPECIFIED. ) 
 CURVE ( )  GEOMETRIC_REPRESENTATION_ITEM ( )  RATIONAL_B_SPLINE_CURVE ( ( 1.000000000000000000, 0.8660254037844387076, 1.000000000000000000, 0.9352274998423648622, 0.9330859296547732162 ) ) 
 REPRESENTATION_ITEM ( '' )  );
#26294 = CARTESIAN_POINT ( 'NONE',  ( 95.39412261730187481, -212.6434372237805803, 75.00000000000001421 ) ) ;
#26295 = CARTESIAN_POINT ( 'NONE',  ( 11.99999999999999822, -59.03961581697367933, -46.53671651294010303 ) ) ;
#26296 = AXIS2_PLACEMENT_3D ( 'NONE', #7603, #30516, #69645 ) ;
#26297 = DIRECTION ( 'NONE',  ( 0.000000000000000000, 0.9135454576426010886, -0.4067366430757998752 ) ) ;
#26298 = CARTESIAN_POINT ( 'NONE',  ( 0.000000000000000000, 18.84667830672579925, 18.68964196561269020 ) ) ;
#26299 =( GEOMETRIC_REPRESENTATION_CONTEXT ( 3 ) GLOBAL_UNCERTAINTY_ASSIGNED_CONTEXT ( ( #43771 ) ) GLOBAL_UNIT_ASSIGNED_CONTEXT ( ( #4204, #50028, #27096 ) ) REPRESENTATION_CONTEXT ( 'NONE', 'WORKASPACE' ) );
#26300 = LINE ( 'NONE', #21392, #37653 ) ;
#26301 = CIRCLE ( 'NONE', #40697, 16.00000000000000000 ) ;
#26302 = CIRCLE ( 'NONE', #21465, 31.99999999999999645 ) ;
#26303 = EDGE_CURVE ( 'NONE', #24118, #43739, #43984, .T. ) ;
#26304 = VECTOR ( 'NONE', #6327, 1000.000000000000000 ) ;
#26305 = DIRECTION ( 'NONE',  ( 0.000000000000000000, 0.9135454576426005335, -0.4067366430758009299 ) ) ;
#26306 = CARTESIAN_POINT ( 'NONE',  ( 97.30629616937498838, 88.66845928578035796, 89.43114583420049257 ) ) ;
#26308 = VECTOR ( 'NONE', #58578, 1000.000000000000000 ) ;
#26307 = DIRECTION ( 'NONE',  ( -1.000000000000000000, -0.000000000000000000, -0.000000000000000000 ) ) ;
#26309 = DIRECTION ( 'NONE',  ( 0.000000000000000000, 0.4539904997395477482, -0.8910065241883673437 ) ) ;
#26310 = CARTESIAN_POINT ( 'NONE',  ( -92.34999999999999432, -211.5299782133524502, 87.72458333333332803 ) ) ;
#26311 = AXIS2_PLACEMENT_3D ( 'NONE', #21401, #11609, #47324 ) ;
#26312 = DIRECTION ( 'NONE',  ( 2.889240119132116694E-16, -1.000000000000000000, 0.000000000000000000 ) ) ;
#26313 = EDGE_CURVE ( 'NONE', #1516, #63719, #6787, .T. ) ;
#26314 = ORIENTED_EDGE ( 'NONE', *, *, #23881, .F. ) ;
#26315 = FACE_OUTER_BOUND ( 'NONE', #41350, .T. ) ;
#26316 = ADVANCED_FACE ( 'NONE', ( #27563 ), #67795, .T. ) ;
#26317 = CARTESIAN_POINT ( 'NONE',  ( 97.64999999981932888, -210.0000309431867436, 78.33187387208516839 ) ) ;
#26318 = CARTESIAN_POINT ( 'NONE',  ( 92.35000000006145626, -209.9999881787626919, 81.82400613091914465 ) ) ;
#26319 = DIRECTION ( 'NONE',  ( -0.000000000000000000, 0.000000000000000000, 1.000000000000000000 ) ) ;
#26320 = VECTOR ( 'NONE', #64662, 1000.000000000000000 ) ;
#26321 = EDGE_CURVE ( 'NONE', #2397, #26241, #68163, .T. ) ;
#26322 = CIRCLE ( 'NONE', #1155, 15.39727592589476579 ) ;
#26323 = VECTOR ( 'NONE', #3661, 1000.000000000000000 ) ;
#26324 = ORIENTED_EDGE ( 'NONE', *, *, #25415, .F. ) ;
#26325 = VECTOR ( 'NONE', #30763, 1000.000000000000000 ) ;
#26326 = ORIENTED_EDGE ( 'NONE', *, *, #72376, .F. ) ;
#26327 = CIRCLE ( 'NONE', #35938, 77.49899999999999523 ) ;
#26328 = DIRECTION ( 'NONE',  ( -1.000000000000000000, 0.000000000000000000, -0.000000000000000000 ) ) ;
#26329 = EDGE_CURVE ( 'NONE', #24236, #69181, #70355, .T. ) ;
#26330 = CARTESIAN_POINT ( 'NONE',  ( 1.233757462863572574, -119.1468631277289347, -2.500000000000000000 ) ) ;
#26331 = VERTEX_POINT ( 'NONE', #51976 ) ;
#26332 = APPLICATION_CONTEXT ( 'automotive_design' ) ;
#26333 = CARTESIAN_POINT ( 'NONE',  ( 92.69370383062501162, -208.6684592857803295, 82.60489583420049087 ) ) ;
#26334 = CARTESIAN_POINT ( 'NONE',  ( 96.15314808468750130, -211.9973110713294489, 86.83822916753382515 ) ) ;
#26335 = ORIENTED_EDGE ( 'NONE', *, *, #58978, .F. ) ;
#26336 = CARTESIAN_POINT ( 'NONE',  ( 92.69370383062501162, -209.9999999999999716, 85.35656250086715602 ) ) ;
#26337 = EDGE_CURVE ( 'NONE', #25004, #14607, #18736, .T. ) ;
#26338 = ORIENTED_EDGE ( 'NONE', *, *, #42625, .F. ) ;
#26339 = CARTESIAN_POINT ( 'NONE',  ( -0.8815729230226008184, -93.47222532549339746, -5.500000000000000000 ) ) ;
#26340 = ORIENTED_EDGE ( 'NONE', *, *, #11280, .T. ) ;
#26341 = CARTESIAN_POINT ( 'NONE',  ( -97.30629616937501680, 88.66845928578038638, 77.15447916753382174 ) ) ;
#26342 = VERTEX_POINT ( 'NONE', #45627 ) ;
#26343 = VERTEX_POINT ( 'NONE', #12854 ) ;
#26344 = CARTESIAN_POINT ( 'NONE',  ( 11.99999999999999822, 59.03961581697399907, 46.53671651293969802 ) ) ;
#26345 = EDGE_LOOP ( 'NONE', ( #66226, #50681, #43439, #8944 ) ) ;
#26346 = DIRECTION ( 'NONE',  ( 0.000000000000000000, 0.9510565162951523099, 0.3090169943749514481 ) ) ;
#26347 = DIRECTION ( 'NONE',  ( -1.000000000000000000, 0.000000000000000000, -0.000000000000000000 ) ) ;
#26348 = VERTEX_POINT ( 'NONE', #58357 ) ;
#26349 = DIRECTION ( 'NONE',  ( 0.000000000000000000, 0.000000000000000000, 1.000000000000000000 ) ) ;
#26350 = ORIENTED_EDGE ( 'NONE', *, *, #66313, .T. ) ;
#26351 = DIRECTION ( 'NONE',  ( -0.000000000000000000, -0.000000000000000000, 1.000000000000000000 ) ) ;
#26352 = AXIS2_PLACEMENT_3D ( 'NONE', #46267, #40254, #63202 ) ;
#26353 = EDGE_LOOP ( 'NONE', ( #6639, #30957, #9399, #40618 ) ) ;
#26354 = AXIS2_PLACEMENT_3D ( 'NONE', #60242, #9449, #37670 ) ;
#26355 = ORIENTED_EDGE ( 'NONE', *, *, #19503, .F. ) ;
#26356 = ORIENTED_EDGE ( 'NONE', *, *, #55503, .F. ) ;
#26357 = CARTESIAN_POINT ( 'NONE',  ( 92.69370383062501162, -211.3315407142195852, 80.17072916753379275 ) ) ;
#26358 = ITEM_DEFINED_TRANSFORMATION ( 'NONE', 'NONE', #37586,  #43395 ) ;
#26359 = CARTESIAN_POINT ( 'NONE',  ( 5.000000000000002665, -78.73519480814938731, -22.90783923731713756 ) ) ;
#26360 = EDGE_LOOP ( 'NONE', ( #61115, #55014, #4924, #26425 ) ) ;
#26361 = VERTEX_POINT ( 'NONE', #29044 ) ;
#26362 = AXIS2_PLACEMENT_3D ( 'NONE', #10052, #5553, #51022 ) ;
#26363 = ORIENTED_EDGE ( 'NONE', *, *, #58415, .T. ) ;
#26364 = CARTESIAN_POINT ( 'NONE',  ( -11.99999999999999645, 0.000000000000000000, 12.85999999999999943 ) ) ;
#26365 = CARTESIAN_POINT ( 'NONE',  ( 10.00000000000000000, -16.65972982744992592, 80.28980883073749908 ) ) ;
#26366 = CARTESIAN_POINT ( 'NONE',  ( -93.84685191531252713, 88.00268892867056536, 77.94822916753382458 ) ) ;
#26367 = ORIENTED_EDGE ( 'NONE', *, *, #69987, .F. ) ;
#26368 = CARTESIAN_POINT ( 'NONE',  ( 93.84685191531248449, 91.99731107132950569, 78.74197916753381321 ) ) ;
#26369 = VERTEX_POINT ( 'NONE', #18139 ) ;
#26370 = FACE_OUTER_BOUND ( 'NONE', #32247, .T. ) ;
#26371 = DIRECTION ( 'NONE',  ( -1.000000000000000000, -0.000000000000000000, -0.000000000000000000 ) ) ;
#26372 = DIRECTION ( 'NONE',  ( 0.3311129884571304971, 0.9435911131814395114, -0.000000000000000000 ) ) ;
#26373 = DIRECTION ( 'NONE',  ( 0.000000000000000000, 0.000000000000000000, 1.000000000000000000 ) ) ;
#26374 = DIRECTION ( 'NONE',  ( -1.000000000000000000, -0.000000000000000000, -0.000000000000000000 ) ) ;
#26375 = CARTESIAN_POINT ( 'NONE',  ( -97.30629616937495996, -209.9999999999999716, 78.21281250086714465 ) ) ;
#26376 = AXIS2_PLACEMENT_3D ( 'NONE', #16029, #68287, #10764 ) ;
#26377 = EDGE_CURVE ( 'NONE', #29550, #10929, #51862, .T. ) ;
#26378 = DIRECTION ( 'NONE',  ( -1.000000000000000000, 0.000000000000000000, -0.000000000000000000 ) ) ;
#26379 = CARTESIAN_POINT ( 'NONE',  ( 0.000000000000000000, 11.30684508768339569, 76.66974797899841576 ) ) ;
#26380 = CARTESIAN_POINT ( 'NONE',  ( 10.00000000000000000, 27.75498641678786527, -31.52238457039571173 ) ) ;
#26381 = ORIENTED_EDGE ( 'NONE', *, *, #33077, .F. ) ;
#26382 = VECTOR ( 'NONE', #17121, 1000.000000000000000 ) ;
#26383 = ADVANCED_FACE ( 'NONE', ( #35063 ), #11739, .F. ) ;
#26384 = ORIENTED_EDGE ( 'NONE', *, *, #70452, .F. ) ;
#26385 = FACE_BOUND ( 'NONE', #29466, .T. ) ;
#26386 = VECTOR ( 'NONE', #73959, 1000.000000000000000 ) ;
#26387 = EDGE_CURVE ( 'NONE', #70060, #28874, #59603, .T. ) ;
#26388 = AXIS2_PLACEMENT_3D ( 'NONE', #26224, #61194, #14204 ) ;
#26389 = EDGE_CURVE ( 'NONE', #9978, #57786, #23779, .T. ) ;
#26390 = CARTESIAN_POINT ( 'NONE',  ( 0.000000000000000000, 0.000000000000000000, 0.000000000000000000 ) ) ;
#26391 = CARTESIAN_POINT ( 'NONE',  ( -43.60332556124591008, -123.0000000000000142, 2.500000000000002220 ) ) ;
#26392 = CARTESIAN_POINT ( 'NONE',  ( -92.69370383062502583, 88.66845928578038638, 85.46239583420047836 ) ) ;
#26393 = DIRECTION ( 'NONE',  ( -0.000000000000000000, -0.000000000000000000, 1.000000000000000000 ) ) ;
#26394 = DIRECTION ( 'NONE',  ( -1.000000000000000000, -0.000000000000000000, -0.000000000000000000 ) ) ;
#26395 =( BOUNDED_CURVE ( )  B_SPLINE_CURVE ( 2, ( #27190, #9914, #66697, #72679, #14815, #43780, #56540 ),
 .UNSPECIFIED., .F., .F. ) 
 B_SPLINE_CURVE_WITH_KNOTS ( ( 3, 2, 2, 3 ),
 ( 0.4656806970056960315, 0.4727362912391188110, 0.4797920567800011971, 0.4868478063929146393 ),
 .UNSPECIFIED. ) 
 CURVE ( )  GEOMETRIC_REPRESENTATION_ITEM ( )  RATIONAL_B_SPLINE_CURVE ( ( 0.9999934945994508606, 0.8660286565636877709, 1.000000000000000000, 0.8660254037844387076, 1.000000000000000000, 0.8660254037844387076, 1.000000000000000000 ) ) 
 REPRESENTATION_ITEM ( '' )  );
#26396 = ORIENTED_EDGE ( 'NONE', *, *, #64755, .F. ) ;
#26397 = CARTESIAN_POINT ( 'NONE',  ( 0.000000000000000000, -65.64334221924882229, -41.19522573413803457 ) ) ;
#26398 = DIRECTION ( 'NONE',  ( -1.000000000000000000, 0.000000000000000000, 0.000000000000000000 ) ) ;
#26399 = CARTESIAN_POINT ( 'NONE',  ( -32.50000000000000000, -120.0000000000000000, 2.500000000000000000 ) ) ;
#26400 = DIRECTION ( 'NONE',  ( 1.000000000000000000, 0.000000000000000000, 0.000000000000000000 ) ) ;
#26401 = CARTESIAN_POINT ( 'NONE',  ( -1.898848305348268983, 4.677202111653171457, -0.6020238742160447520 ) ) ;
#26402 = LINE ( 'NONE', #45193, #31734 ) ;
#26403 = CARTESIAN_POINT ( 'NONE',  ( -92.69370383062498320, -208.6684592857803011, 84.45697916753383083 ) ) ;
#26404 = ADVANCED_FACE ( 'NONE', ( #74165 ), #522, .F. ) ;
#26405 = CARTESIAN_POINT ( 'NONE',  ( 94.99999999999998579, 86.94004357329502852, 76.26812500173430465 ) ) ;
#26406 = CIRCLE ( 'NONE', #2476, 77.49899999999999523 ) ;
#26407 = CARTESIAN_POINT ( 'NONE',  ( 11.99999999999999822, -2.956366410621191765, 75.11725578898467859 ) ) ;
#26408 = DIRECTION ( 'NONE',  ( 0.000000000000000000, 0.3826834323650905589, -0.9238795325112864054 ) ) ;
#26409 = PLANE ( 'NONE',  #33351 ) ;
#26410 = ORIENTED_EDGE ( 'NONE', *, *, #28095, .T. ) ;
#26411 = CARTESIAN_POINT ( 'NONE',  ( -93.67499999999998295, -212.2949673200287179, 82.03604166840096923 ) ) ;
#26412 = CARTESIAN_POINT ( 'NONE',  ( 10.00000000000000000, -17.67226234102849958, 33.17418723428301774 ) ) ;
#26413 = AXIS2_PLACEMENT_3D ( 'NONE', #53125, #64047, #40739 ) ;
#26414 = PLANE ( 'NONE',  #5422 ) ;
#26415 = EDGE_CURVE ( 'NONE', #8512, #8585, #22681, .T. ) ;
#26416 = EDGE_CURVE ( 'NONE', #55326, #11224, #63212, .T. ) ;
#26417 = CIRCLE ( 'NONE', #40868, 31.99999999999998934 ) ;
#26418 = LINE ( 'NONE', #39559, #56424 ) ;
#26419 = ORIENTED_EDGE ( 'NONE', *, *, #44761, .F. ) ;
#26420 = CARTESIAN_POINT ( 'NONE',  ( 97.64999999999987779, 91.52997821335259232, 78.30541666666667311 ) ) ;
#26421 = CARTESIAN_POINT ( 'NONE',  ( 0.000000000000000000, -71.91182617369207719, 28.89263327155721228 ) ) ;
#26422 = ORIENTED_EDGE ( 'NONE', *, *, #19362, .T. ) ;
#26423 = CARTESIAN_POINT ( 'NONE',  ( 12.49999999999999645, 1.530808498934191127E-15, -20.00000000000000000 ) ) ;
#26424 = CARTESIAN_POINT ( 'NONE',  ( -96.32499999999996021, -207.7050326799711968, 87.43354166840096298 ) ) ;
#26425 = ORIENTED_EDGE ( 'NONE', *, *, #64193, .F. ) ;
#26426 = DIRECTION ( 'NONE',  ( -1.000000000000000000, -0.000000000000000000, 0.000000000000000000 ) ) ;
#26427 = CIRCLE ( 'NONE', #7223, 31.99999999999999289 ) ;
#26428 = ORIENTED_EDGE ( 'NONE', *, *, #37523, .F. ) ;
#26429 = CARTESIAN_POINT ( 'NONE',  ( 0.000000000000000000, -12.42422080174663712, 35.38097989696507994 ) ) ;
#26430 = CIRCLE ( 'NONE', #48017, 16.00000000000000000 ) ;
#26431 = CIRCLE ( 'NONE', #63646, 3.299999999999983391 ) ;
#26432 = CIRCLE ( 'NONE', #29849, 32.00000000000000000 ) ;
#26433 = ORIENTED_EDGE ( 'NONE', *, *, #15893, .T. ) ;
#26434 = ORIENTED_EDGE ( 'NONE', *, *, #1687, .T. ) ;
#26435 = CIRCLE ( 'NONE', #60068, 22.90000000000041780 ) ;
#26436 = VERTEX_POINT ( 'NONE', #17034 ) ;
#26437 = VERTEX_POINT ( 'NONE', #17763 ) ;
#26438 = CARTESIAN_POINT ( 'NONE',  ( 92.35000000039376289, -209.9999706925934504, 76.74344264317686282 ) ) ;
#26439 = VERTEX_POINT ( 'NONE', #41083 ) ;
#26440 = ORIENTED_EDGE ( 'NONE', *, *, #16445, .T. ) ;
#26441 = CARTESIAN_POINT ( 'NONE',  ( 93.84685191531248449, 91.99731107132950569, 78.26572916753382003 ) ) ;
#26442 = CARTESIAN_POINT ( 'NONE',  ( 11.99999999999999822, 51.29473840253223216, 63.97538442413446091 ) ) ;
#26443 = CARTESIAN_POINT ( 'NONE',  ( -92.35000000000003695, 90.00000000000004263, 85.23749999999999716 ) ) ;
#26444 = ORIENTED_EDGE ( 'NONE', *, *, #40892, .T. ) ;
#26445 = VERTEX_POINT ( 'NONE', #24161 ) ;
#26446 = ORIENTED_EDGE ( 'NONE', *, *, #59343, .T. ) ;
#26447 = ORIENTED_EDGE ( 'NONE', *, *, #64244, .T. ) ;
#26448 = CARTESIAN_POINT ( 'NONE',  ( 95.00000000000000000, -207.3369185715606307, 88.84906250086713442 ) ) ;
#26449 = CARTESIAN_POINT ( 'NONE',  ( 8.500000000000035527, 73.00000000000001421, -205.0000000000000284 ) ) ;
#26450 = CARTESIAN_POINT ( 'NONE',  ( 10.00000000000000000, 0.000000000000000000, 0.000000000000000000 ) ) ;
#26451 = CARTESIAN_POINT ( 'NONE',  ( -97.65000000000001990, 90.00000000000004263, 77.37937500173428873 ) ) ;
#26452 = DIRECTION ( 'NONE',  ( 0.000000000000000000, 0.000000000000000000, 1.000000000000000000 ) ) ;
#26453 = CARTESIAN_POINT ( 'NONE',  ( 21.85433023846371370, -135.0628101570779620, -5.500000000000000000 ) ) ;
#26454 = DIRECTION ( 'NONE',  ( 0.000000000000000000, -1.224646799147353207E-16, 1.000000000000000000 ) ) ;
#26455 = FACE_OUTER_BOUND ( 'NONE', #49706, .T. ) ;
#26456 = CARTESIAN_POINT ( 'NONE',  ( -96.32499999999996021, -212.2949673200287179, 76.21520833506762926 ) ) ;
#26457 = CARTESIAN_POINT ( 'NONE',  ( -92.69370383062502583, 91.33154071421968467, 89.53697916753382913 ) ) ;
#26458 = VERTEX_POINT ( 'NONE', #64016 ) ;
#26460 = CARTESIAN_POINT ( 'NONE',  ( -92.69370383062502583, 91.33154071421968467, 87.47322916753381605 ) ) ;
#26459 = CARTESIAN_POINT ( 'NONE',  ( 93.84685191531248449, 91.99731107132950569, 87.63197916753379957 ) ) ;
#26461 = ORIENTED_EDGE ( 'NONE', *, *, #23459, .F. ) ;
#26462 = DIRECTION ( 'NONE',  ( 0.000000000000000000, 0.9510565162951543083, 0.3090169943749448977 ) ) ;
#26463 = CYLINDRICAL_SURFACE ( 'NONE', #20570, 32.00000000000000000 ) ;
#26464 = CARTESIAN_POINT ( 'NONE',  ( 11.99999999999999822, 63.18004540533030422, 44.88180994100399346 ) ) ;
#26465 = LINE ( 'NONE', #62172, #51578 ) ;
#26466 = DIRECTION ( 'NONE',  ( 0.000000000000000000, 1.000000000000000000, 0.000000000000000000 ) ) ;
#26467 = DIRECTION ( 'NONE',  ( -1.000000000000000000, -0.000000000000000000, 0.000000000000000000 ) ) ;
#26468 = AXIS2_PLACEMENT_3D ( 'NONE', #73635, #29253, #13 ) ;
#26469 = ADVANCED_FACE ( 'NONE', ( #6857 ), #63652, .F. ) ;
#26470 = FACE_OUTER_BOUND ( 'NONE', #64021, .T. ) ;
#26471 = AXIS2_PLACEMENT_3D ( 'NONE', #28809, #57384, #40457 ) ;
#26472 = DIRECTION ( 'NONE',  ( 1.000000000000000000, 0.000000000000000000, 0.000000000000000000 ) ) ;
#26473 = VERTEX_POINT ( 'NONE', #64381 ) ;
#26474 = ADVANCED_FACE ( 'NONE', ( #11382 ), #34316, .T. ) ;
#26475 = ORIENTED_EDGE ( 'NONE', *, *, #32399, .T. ) ;
#26476 = AXIS2_PLACEMENT_3D ( 'NONE', #23980, #17960, #12679 ) ;
#26477 = EDGE_CURVE ( 'NONE', #63620, #47511, #68910, .T. ) ;
#26478 = CARTESIAN_POINT ( 'NONE',  ( -97.65000000000001990, 91.52997821335253548, 81.69208333333332916 ) ) ;
#26479 = CARTESIAN_POINT ( 'NONE',  ( -10.00000000000000000, 0.000000000000000000, 0.000000000000000000 ) ) ;
#26480 = CARTESIAN_POINT ( 'NONE',  ( 97.64999999999999147, -209.9999999999999716, 82.69749999999999091 ) ) ;
#26481 = CARTESIAN_POINT ( 'NONE',  ( 15.00000000000000000, -23.29833615347109088, -3.418703333116486665 ) ) ;
#26482 = DIRECTION ( 'NONE',  ( -1.000000000000000000, -0.000000000000000000, -0.000000000000000000 ) ) ;
#26483 = DIRECTION ( 'NONE',  ( -1.000000000000000000, -0.000000000000000000, -0.000000000000000000 ) ) ;
#26484 = CARTESIAN_POINT ( 'NONE',  ( 0.000000000000000000, -75.11725578898466438, -2.956366410621452001 ) ) ;
#26485 = EDGE_CURVE ( 'NONE', #69892, #6635, #31994, .T. ) ;
#26486 = VERTEX_POINT ( 'NONE', #53826 ) ;
#26487 = CARTESIAN_POINT ( 'NONE',  ( -96.15314808468752972, 91.99731107132950569, 82.55197916753380127 ) ) ;
#26488 = CIRCLE ( 'NONE', #69741, 82.00000000000000000 ) ;
#26489 = CARTESIAN_POINT ( 'NONE',  ( 11.99999999999999822, -34.94270380257692921, 74.18225833017875459 ) ) ;
#26490 = AXIS2_PLACEMENT_3D ( 'NONE', #57176, #28578, #12403 ) ;
#26491 = CARTESIAN_POINT ( 'NONE',  ( -3.000000000000000000, 14.60985201121729737, -18.46759930825687945 ) ) ;
#26492 = AXIS2_PLACEMENT_3D ( 'NONE', #36444, #25176, #43227 ) ;
#26493 = CARTESIAN_POINT ( 'NONE',  ( -92.35000000000005116, 91.52997821335254969, 78.94041666666664980 ) ) ;
#26494 = DIRECTION ( 'NONE',  ( -0.1276937514489679404, -0.9918136447140103451, 0.000000000000000000 ) ) ;
#26495 = DIRECTION ( 'NONE',  ( -1.000000000000000000, 5.236901059551556403E-15, 2.618450529775778123E-14 ) ) ;
#26496 = CARTESIAN_POINT ( 'NONE',  ( 19.12409105625795291, -101.5943176906707919, 5.500000000000000000 ) ) ;
#26497 = CARTESIAN_POINT ( 'NONE',  ( 0.000000000000000000, -4.261787119645322974, 26.19803753235775190 ) ) ;
#26498 = CIRCLE ( 'NONE', #57690, 82.00000000000000000 ) ;
#26499 = DIRECTION ( 'NONE',  ( -1.000000000000000000, 0.000000000000000000, 0.000000000000000000 ) ) ;
#26500 = ADVANCED_FACE ( 'NONE', ( #71474 ), #59852, .T. ) ;
#26501 = EDGE_CURVE ( 'NONE', #4344, #70067, #72057, .T. ) ;
#26502 = CARTESIAN_POINT ( 'NONE',  ( 93.84685191531248449, 88.00268892867053694, 79.11239583420048405 ) ) ;
#26503 = CARTESIAN_POINT ( 'NONE',  ( -96.15314808468745866, -211.9973110713294489, 82.28739583420048120 ) ) ;
#26504 = DIRECTION ( 'NONE',  ( -0.000000000000000000, -0.000000000000000000, 1.000000000000000000 ) ) ;
#26505 = ORIENTED_EDGE ( 'NONE', *, *, #44547, .F. ) ;
#26506 = DIRECTION ( 'NONE',  ( -1.000000000000000000, -0.000000000000000000, -0.000000000000000000 ) ) ;
#26507 = CARTESIAN_POINT ( 'NONE',  ( -96.32499999999996021, -212.2949673200287179, 78.67583333333332973 ) ) ;
#26508 = DIRECTION ( 'NONE',  ( -1.000000000000000000, -0.000000000000000000, 0.000000000000000000 ) ) ;
#26509 = EDGE_CURVE ( 'NONE', #38472, #30664, #7601, .T. ) ;
#26510 = EDGE_CURVE ( 'NONE', #60490, #64515, #40379, .T. ) ;
#26511 = CARTESIAN_POINT ( 'NONE',  ( 96.15314808468750130, -211.9973110713294489, 85.40947916753380298 ) ) ;
#26512 = EDGE_LOOP ( 'NONE', ( #51884, #4777, #70607, #70331 ) ) ;
#26513 = CARTESIAN_POINT ( 'NONE',  ( 10.00000000000000000, -41.76106447765533147, 62.50884508063410294 ) ) ;
#26514 = ORIENTED_EDGE ( 'NONE', *, *, #39505, .F. ) ;
#26515 = CARTESIAN_POINT ( 'NONE',  ( 0.000000000000000000, 0.8828120875905820508, -37.48860685352290290 ) ) ;
#26516 = VERTEX_POINT ( 'NONE', #14345 ) ;
#26517 = AXIS2_PLACEMENT_3D ( 'NONE', #27188, #44883, #33581 ) ;
#26519 = VECTOR ( 'NONE', #58388, 1000.000000000000000 ) ;
#26518 = CARTESIAN_POINT ( 'NONE',  ( -92.35000000000005116, 88.47002178664754979, 79.54895833506762415 ) ) ;
#26520 = CARTESIAN_POINT ( 'NONE',  ( 92.69370383062501162, -209.9999999999999716, 77.10156250086714635 ) ) ;
#26521 = CARTESIAN_POINT ( 'NONE',  ( -10.00000000000000000, 0.000000000000000000, 0.000000000000000000 ) ) ;
#26522 = DIRECTION ( 'NONE',  ( 1.000000000000000000, 0.000000000000000000, -0.000000000000000000 ) ) ;
#26523 = CARTESIAN_POINT ( 'NONE',  ( -95.29566955675987572, 87.37275709988156791, 74.99300273738300859 ) ) ;
#26524 = CARTESIAN_POINT ( 'NONE',  ( 96.15314808468748708, 91.99731107132950569, 85.14489583420048291 ) ) ;
#26525 = CARTESIAN_POINT ( 'NONE',  ( -95.00000000000002842, 90.00000000000004263, 90.00000000000000000 ) ) ;
#26526 = CARTESIAN_POINT ( 'NONE',  ( 97.64999999999997726, -211.5299782133524502, 82.00958333333332462 ) ) ;
#26527 = VERTEX_POINT ( 'NONE', #53461 ) ;
#26528 = VERTEX_POINT ( 'NONE', #48191 ) ;
#26529 = ORIENTED_EDGE ( 'NONE', *, *, #50984, .F. ) ;
#26530 = VERTEX_POINT ( 'NONE', #37294 ) ;
#26531 = CARTESIAN_POINT ( 'NONE',  ( 93.67500000000001137, -207.7050326799711968, 89.25916666666667254 ) ) ;
#26532 = VECTOR ( 'NONE', #4773, 1000.000000000000000 ) ;
#26533 = CIRCLE ( 'NONE', #63802, 17.37152077436032371 ) ;
#26534 = CARTESIAN_POINT ( 'NONE',  ( -95.00000000000002842, 92.66308142843932671, 83.92781250086716227 ) ) ;
#26535 = EDGE_CURVE ( 'NONE', #65205, #21877, #18866, .T. ) ;
#26536 = VECTOR ( 'NONE', #19466, 1000.000000000000000 ) ;
#26537 = DIRECTION ( 'NONE',  ( 0.000000000000000000, 0.7431448254773954654, -0.6691306063588569053 ) ) ;
#26538 = CARTESIAN_POINT ( 'NONE',  ( -9.974659986866640793E-15, -5.773502691896262640, -5.553418012614792509 ) ) ;
#26539 = DIRECTION ( 'NONE',  ( -1.000000000000000000, 0.000000000000000000, -0.000000000000000000 ) ) ;
#26540 = EDGE_CURVE ( 'NONE', #34012, #4061, #41805, .T. ) ;
#26541 = ORIENTED_EDGE ( 'NONE', *, *, #53876, .F. ) ;
#26542 = CARTESIAN_POINT ( 'NONE',  ( -93.67499999999998295, -212.2949673200287179, 87.11604166840096752 ) ) ;
#26543 = VERTEX_POINT ( 'NONE', #8340 ) ;
#26544 = DIRECTION ( 'NONE',  ( -1.000000000000000000, -0.000000000000000000, 0.000000000000000000 ) ) ;
#26546 = VERTEX_POINT ( 'NONE', #19241 ) ;
#26545 = EDGE_CURVE ( 'NONE', #20634, #72495, #64432, .T. ) ;
#26547 = CARTESIAN_POINT ( 'NONE',  ( -96.32500000000001705, 87.70503267997129626, 84.47020833506762472 ) ) ;
#26548 = EDGE_LOOP ( 'NONE', ( #52980, #29871, #43416, #19875 ) ) ;
#26549 = CARTESIAN_POINT ( 'NONE',  ( 97.30629616937498838, 88.66845928578037217, 87.52614583420049144 ) ) ;
#26550 = CARTESIAN_POINT ( 'NONE',  ( 6.000000000000000000, 39.47590169984945163, -71.87247863392373404 ) ) ;
#26551 = CARTESIAN_POINT ( 'NONE',  ( 12.00000000000000000, 22.07842321921480888, -8.187992925817425771 ) ) ;
#26552 = EDGE_CURVE ( 'NONE', #5770, #68267, #25990, .T. ) ;
#26553 = CARTESIAN_POINT ( 'NONE',  ( 10.00000000000000000, -3.925862922255855647, -41.81611651403866858 ) ) ;
#26554 = LINE ( 'NONE', #50216, #59447 ) ;
#26555 = DIRECTION ( 'NONE',  ( -0.2867529058022021404, 0.9580045777625456616, 0.000000000000000000 ) ) ;
#26556 = ORIENTED_EDGE ( 'NONE', *, *, #15510, .F. ) ;
#26557 = CARTESIAN_POINT ( 'NONE',  ( -92.35000000000005116, 91.52997821335253548, 80.92479166840097093 ) ) ;
#26558 = CYLINDRICAL_SURFACE ( 'NONE', #23928, 2.649999999999985700 ) ;
#26559 = ORIENTED_EDGE ( 'NONE', *, *, #22568, .T. ) ;
#26560 = EDGE_CURVE ( 'NONE', #67190, #48030, #62022, .T. ) ;
#26561 = ORIENTED_EDGE ( 'NONE', *, *, #577, .F. ) ;
#26562 = PRODUCT_DEFINITION_SHAPE ( 'NONE', 'NONE',  #30197 ) ;
#26563 = PLANE ( 'NONE',  #50417 ) ;
#26564 = LINE ( 'NONE', #49498, #37733 ) ;
#26565 = CARTESIAN_POINT ( 'NONE',  ( -97.30629616937495996, -209.9999999999999716, 83.45156250086715488 ) ) ;
#26566 = EDGE_LOOP ( 'NONE', ( #13004, #36991, #19773, #46989 ) ) ;
#26567 = EDGE_CURVE ( 'NONE', #70160, #60573, #7963, .T. ) ;
#26568 = CYLINDRICAL_SURFACE ( 'NONE', #41706, 77.49899999999999523 ) ;
#26569 = EDGE_LOOP ( 'NONE', ( #41431, #11357, #58974, #13216 ) ) ;
#26570 = PRESENTATION_LAYER_ASSIGNMENT (  '', '', ( #32576 ) ) ;
#26571 = AXIS2_PLACEMENT_3D ( 'NONE', #68175, #16301, #38116 ) ;
#26572 = LINE ( 'NONE', #49504, #25882 ) ;
#26573 = VECTOR ( 'NONE', #50711, 1000.000000000000000 ) ;
#26574 = CARTESIAN_POINT ( 'NONE',  ( -12.50000000000000000, -132.5000000000000000, 2.500000000000000000 ) ) ;
#26575 = VECTOR ( 'NONE', #36196, 1000.000000000000000 ) ;
#26576 = CARTESIAN_POINT ( 'NONE',  ( 93.84685191531248449, 91.99731107132950569, 78.74197916753381321 ) ) ;
#26577 = DIRECTION ( 'NONE',  ( -1.000000000000000000, 0.000000000000000000, -0.000000000000000000 ) ) ;
#26578 = PLANE ( 'NONE',  #9677 ) ;
#26579 = LINE ( 'NONE', #61179, #24070 ) ;
#26580 = DIRECTION ( 'NONE',  ( 0.000000000000000000, 0.000000000000000000, -1.000000000000000000 ) ) ;
#26581 = LINE ( 'NONE', #3684, #38801 ) ;
#26582 = ADVANCED_FACE ( 'NONE', ( #47453 ), #2740, .F. ) ;
#26583 = CARTESIAN_POINT ( 'NONE',  ( -92.34999999999999432, -209.9999999999999716, 87.14249999999999829 ) ) ;
#26584 = AXIS2_PLACEMENT_3D ( 'NONE', #28033, #74273, #67524 ) ;
#26585 = EDGE_CURVE ( 'NONE', #7032, #15962, #39203, .T. ) ;
#26586 = LINE ( 'NONE', #72799, #56454 ) ;
#26587 = FACE_OUTER_BOUND ( 'NONE', #5468, .T. ) ;
#26588 = ORIENTED_EDGE ( 'NONE', *, *, #71609, .F. ) ;
#26589 = CARTESIAN_POINT ( 'NONE',  ( -92.69370383062505425, 88.66845928578038638, 81.65239583420047609 ) ) ;
#26590 = AXIS2_PLACEMENT_3D ( 'NONE', #21185, #5047, #44138 ) ;
#26591 = FACE_OUTER_BOUND ( 'NONE', #25297, .T. ) ;
#26592 = AXIS2_PLACEMENT_3D ( 'NONE', #28068, #45761, #40105 ) ;
#26593 = CARTESIAN_POINT ( 'NONE',  ( 0.000000000000000000, 0.000000000000000000, 0.000000000000000000 ) ) ;
#26594 = VERTEX_POINT ( 'NONE', #63521 ) ;
#26595 =( BOUNDED_CURVE ( )  B_SPLINE_CURVE ( 2, ( #44083, #14761, #43725, #48247, #48612, #72271, #66646 ),
 .UNSPECIFIED., .F., .F. ) 
 B_SPLINE_CURVE_WITH_KNOTS ( ( 3, 2, 2, 3 ),
 ( 0.6666666666666667407, 0.6736111111111112715, 0.6805555555555555802, 0.6875000000000000000 ),
 .UNSPECIFIED. ) 
 CURVE ( )  GEOMETRIC_REPRESENTATION_ITEM ( )  RATIONAL_B_SPLINE_CURVE ( ( 0.9999999999999978906, 0.8660254037844408170, 1.000000000000000000, 0.8660254037844387076, 1.000000000000000000, 0.8660254037844387076, 1.000000000000000000 ) ) 
 REPRESENTATION_ITEM ( '' )  );
#26596 = DIRECTION ( 'NONE',  ( 0.000000000000000000, 0.000000000000000000, 1.000000000000000000 ) ) ;
#26597 = LINE ( 'NONE', #48423, #2453 ) ;
#26598 = DIRECTION ( 'NONE',  ( -1.000000000000000000, 0.000000000000000000, 0.000000000000000000 ) ) ;
#26599 = CYLINDRICAL_SURFACE ( 'NONE', #54766, 16.00000000000000000 ) ;
#26600 = CARTESIAN_POINT ( 'NONE',  ( 97.30629616937498838, -208.6684592857803011, 77.47197916753381719 ) ) ;
#26601 = VERTEX_POINT ( 'NONE', #52964 ) ;
#26602 = VERTEX_POINT ( 'NONE', #69153 ) ;
#26603 = EDGE_CURVE ( 'NONE', #34276, #45130, #35655, .T. ) ;
#26604 = CARTESIAN_POINT ( 'NONE',  ( -24.50849501662245800, -109.8101191361138831, -5.500000000000000000 ) ) ;
#26605 = CARTESIAN_POINT ( 'NONE',  ( 5.000000000000000000, 74.74816331893477184, -33.71516098798660011 ) ) ;
#26606 = DIRECTION ( 'NONE',  ( 0.000000000000000000, 0.000000000000000000, -1.000000000000000000 ) ) ;
#26607 = CARTESIAN_POINT ( 'NONE',  ( 10.00000000000000000, 0.000000000000000000, 0.000000000000000000 ) ) ;
#26608 = CARTESIAN_POINT ( 'NONE',  ( 10.00000000000000000, -35.95386929396264009, 10.96151621346475658 ) ) ;
#26609 = CARTESIAN_POINT ( 'NONE',  ( 92.69370383062501162, -209.9999999999999716, 77.10156250086714635 ) ) ;
#26610 = MECHANICAL_DESIGN_GEOMETRIC_PRESENTATION_REPRESENTATION (  '', ( #66249 ), #68666 ) ;
#26611 = VECTOR ( 'NONE', #65778, 1000.000000000000000 ) ;
#26612 = VERTEX_POINT ( 'NONE', #69512 ) ;
#26613 = PLANE ( 'NONE',  #41903 ) ;
#26614 = ORIENTED_EDGE ( 'NONE', *, *, #21620, .T. ) ;
#26615 = ORIENTED_EDGE ( 'NONE', *, *, #47198, .T. ) ;
#26616 = DIRECTION ( 'NONE',  ( -1.000000000000000000, -0.000000000000000000, 0.000000000000000000 ) ) ;
#26617 = CIRCLE ( 'NONE', #56656, 31.99999999999998579 ) ;
#26618 = DIRECTION ( 'NONE',  ( -1.000000000000000000, 0.000000000000000000, 0.000000000000000000 ) ) ;
#26619 = EDGE_CURVE ( 'NONE', #63855, #35666, #11996, .T. ) ;
#26620 = ORIENTED_EDGE ( 'NONE', *, *, #24069, .T. ) ;
#26621 = DIRECTION ( 'NONE',  ( 0.000000000000000000, 0.000000000000000000, -1.000000000000000000 ) ) ;
#26622 = CARTESIAN_POINT ( 'NONE',  ( 93.67500000000001137, -212.2949673200287179, 80.66020833506763665 ) ) ;
#26623 = CARTESIAN_POINT ( 'NONE',  ( 94.99999999999998579, 93.05995642670504253, 85.39624999999998067 ) ) ;
#26624 = ADVANCED_FACE ( 'NONE', ( #46958 ), #57871, .F. ) ;
#26625 = ORIENTED_EDGE ( 'NONE', *, *, #37536, .F. ) ;
#26626 = LINE ( 'NONE', #38286, #65902 ) ;
#26627 = VECTOR ( 'NONE', #25921, 1000.000000000000000 ) ;
#26628 = CYLINDRICAL_SURFACE ( 'NONE', #35719, 77.49899999999999523 ) ;
#26629 = ORIENTED_EDGE ( 'NONE', *, *, #44563, .F. ) ;
#26630 = LINE ( 'NONE', #33006, #60818 ) ;
#26631 = CIRCLE ( 'NONE', #23220, 82.00000000000000000 ) ;
#26632 = CARTESIAN_POINT ( 'NONE',  ( -97.30629616937501680, 91.33154071421968467, 84.03364583420049883 ) ) ;
#26633 = CARTESIAN_POINT ( 'NONE',  ( 92.69370383062498320, 88.66845928578037217, 82.07572916753380809 ) ) ;
#26634 = ORIENTED_EDGE ( 'NONE', *, *, #71995, .F. ) ;
#26635 = ADVANCED_FACE ( 'NONE', ( #6374 ), #29278, .T. ) ;
#26636 = EDGE_CURVE ( 'NONE', #29381, #58538, #17273, .T. ) ;
#26637 = DIRECTION ( 'NONE',  ( 0.1276937514489694392, 0.9918136447140102341, -0.000000000000000000 ) ) ;
#26638 = ORIENTED_EDGE ( 'NONE', *, *, #51367, .F. ) ;
#26639 = DIRECTION ( 'NONE',  ( 0.000000000000000000, 0.000000000000000000, 1.000000000000000000 ) ) ;
#26640 = AXIS2_PLACEMENT_3D ( 'NONE', #50418, #45169, #21094 ) ;
#26641 = AXIS2_PLACEMENT_3D ( 'NONE', #2401, #64778, #30539 ) ;
#26642 = ORIENTED_EDGE ( 'NONE', *, *, #70656, .F. ) ;
#26643 = ORIENTED_EDGE ( 'NONE', *, *, #61140, .T. ) ;
#26644 = AXIS2_PLACEMENT_3D ( 'NONE', #48243, #18186, #12539 ) ;
#26645 = DIRECTION ( 'NONE',  ( 0.000000000000000000, -0.9723699203976789995, 0.2334453638558956767 ) ) ;
#26646 = ORIENTED_EDGE ( 'NONE', *, *, #70276, .T. ) ;
#26647 = LINE ( 'NONE', #3019, #62417 ) ;
#26648 = CARTESIAN_POINT ( 'NONE',  ( 97.64999999999999147, 90.00000000000002842, 88.49187500173430010 ) ) ;
#26649 = VERTEX_POINT ( 'NONE', #58596 ) ;
#26650 = DIRECTION ( 'NONE',  ( -3.061616997868383141E-16, -1.000000000000000000, 0.000000000000000000 ) ) ;
#26651 = CARTESIAN_POINT ( 'NONE',  ( -94.99999999999997158, -212.6630814284392557, 80.27656250086714351 ) ) ;
#26652 = EDGE_LOOP ( 'NONE', ( #37636, #43197, #7344, #55793 ) ) ;
#26654 = ADVANCED_FACE ( 'NONE', ( #45867 ), #6013, .T. ) ;
#26653 = LINE ( 'NONE', #33032, #54275 ) ;
#26655 = DIRECTION ( 'NONE',  ( -1.000000000000000000, 0.000000000000000000, 0.000000000000000000 ) ) ;
#26656 = DIRECTION ( 'NONE',  ( 0.000000000000000000, 0.000000000000000000, 1.000000000000000000 ) ) ;
#26657 = DIRECTION ( 'NONE',  ( 0.000000000000000000, 0.7431448254773863615, -0.6691306063588670083 ) ) ;
#26658 = PLANE ( 'NONE',  #6741 ) ;
#26659 = CARTESIAN_POINT ( 'NONE',  ( 5.999999999999999112, 67.80270845531887858, 46.11716303203210288 ) ) ;
#26660 = CARTESIAN_POINT ( 'NONE',  ( 97.30629616937498838, 90.00000000000002842, 86.78531250086714977 ) ) ;
#26661 = DIRECTION ( 'NONE',  ( 0.000000000000000000, 0.000000000000000000, -1.000000000000000000 ) ) ;
#26662 = DIRECTION ( 'NONE',  ( -0.9038112904824846527, 0.4279312458752990711, 0.000000000000000000 ) ) ;
#26663 = CARTESIAN_POINT ( 'NONE',  ( -96.32500000000001705, 92.29496732002878900, 88.70354166840097321 ) ) ;
#26664 = CARTESIAN_POINT ( 'NONE',  ( 0.000000000000000000, 0.000000000000000000, 0.000000000000000000 ) ) ;
#26665 = EDGE_CURVE ( 'NONE', #42918, #70364, #18734, .T. ) ;
#26666 = CARTESIAN_POINT ( 'NONE',  ( 10.00000000000000000, 0.000000000000000000, 0.000000000000000000 ) ) ;
#26667 = CARTESIAN_POINT ( 'NONE',  ( -11.70000000000000107, 0.000000000000000000, 0.000000000000000000 ) ) ;
#26668 = CARTESIAN_POINT ( 'NONE',  ( -8.000000000000007105, 15.80000000000013749, 1.517382266529735144E-13 ) ) ;
#26669 = ADVANCED_FACE ( 'NONE', ( #12360 ), #762, .T. ) ;
#26670 = CARTESIAN_POINT ( 'NONE',  ( 10.00000000000000000, 15.48615015657582283, 39.04073710021349797 ) ) ;
#26671 = COLOUR_RGB ( '', 0.66274510, 0.83137255, 0.94901961) ;
#26672 = CARTESIAN_POINT ( 'NONE',  ( 2.117611129180199558, -93.54218975225703048, 5.500000000000000000 ) ) ;
#26673 = CARTESIAN_POINT ( 'NONE',  ( 100.0010000000000900, 64.99999999999997158, -90.00000000000000000 ) ) ;
#26674 = AXIS2_PLACEMENT_3D ( 'NONE', #18719, #53679, #58964 ) ;
#26675 = CARTESIAN_POINT ( 'NONE',  ( -97.64999999999996305, -209.9999999999999716, 84.92000000000000171 ) ) ;
#26676 = VECTOR ( 'NONE', #7353, 1000.000000000000000 ) ;
#26677 = DIRECTION ( 'NONE',  ( 0.000000000000000000, 0.000000000000000000, -1.000000000000000000 ) ) ;
#26678 = AXIS2_PLACEMENT_3D ( 'NONE', #55877, #4772, #27675 ) ;
#26679 = ORIENTED_EDGE ( 'NONE', *, *, #2089, .F. ) ;
#26680 = FACE_OUTER_BOUND ( 'NONE', #65502, .T. ) ;
#26681 = CARTESIAN_POINT ( 'NONE',  ( 5.999999999999999112, -64.81221759200306565, -50.23322058963418613 ) ) ;
#26682 = DIRECTION ( 'NONE',  ( -1.000000000000000000, 0.000000000000000000, 0.000000000000000000 ) ) ;
#26683 = DIRECTION ( 'NONE',  ( -1.000000000000000000, -0.000000000000000000, -0.000000000000000000 ) ) ;
#26684 = AXIS2_PLACEMENT_3D ( 'NONE', #61950, #26975, #38647 ) ;
#26685 = AXIS2_PLACEMENT_3D ( 'NONE', #7536, #70661, #14273 ) ;
#26686 = VERTEX_POINT ( 'NONE', #35305 ) ;
#26687 = ORIENTED_EDGE ( 'NONE', *, *, #42689, .F. ) ;
#26688 = CARTESIAN_POINT ( 'NONE',  ( -2.499999999999970690, 73.00000000000001421, -255.0000000000000000 ) ) ;
#26689 = CARTESIAN_POINT ( 'NONE',  ( 0.000000000000000000, 34.44570377933693806, -69.42325613327405165 ) ) ;
#26690 = ORIENTED_EDGE ( 'NONE', *, *, #29854, .T. ) ;
#26691 = CARTESIAN_POINT ( 'NONE',  ( 92.69370383062501162, -209.9999999999999716, 82.02281250086714692 ) ) ;
#26692 = CARTESIAN_POINT ( 'NONE',  ( 96.15314808468748708, -208.0026889286704943, 86.41489583420049314 ) ) ;
#26693 = VERTEX_POINT ( 'NONE', #23291 ) ;
#26694 = CARTESIAN_POINT ( 'NONE',  ( 92.69370383062501162, -208.6684592857803011, 86.57364583420047666 ) ) ;
#26695 = EDGE_LOOP ( 'NONE', ( #3807, #44655, #69184, #52615 ) ) ;
#26696 = CYLINDRICAL_SURFACE ( 'NONE', #56291, 31.99999999999998579 ) ;
#26697 = ORIENTED_EDGE ( 'NONE', *, *, #46618, .T. ) ;
#26698 = CARTESIAN_POINT ( 'NONE',  ( -92.69370383062504004, 90.00000000000004263, 78.05406250086716113 ) ) ;
#26699 = VERTEX_POINT ( 'NONE', #28918 ) ;
#26700 = EDGE_LOOP ( 'NONE', ( #24322, #52702, #34141, #30779 ) ) ;
#26701 = CARTESIAN_POINT ( 'NONE',  ( 0.000000000000000000, -1.278221433540501550, 26.51162292216071847 ) ) ;
#26702 = EDGE_CURVE ( 'NONE', #48244, #43660, #30385, .T. ) ;
#26703 = ORIENTED_EDGE ( 'NONE', *, *, #52266, .T. ) ;
#26704 = DIRECTION ( 'NONE',  ( -1.000000000000000000, 0.000000000000000000, 0.000000000000000000 ) ) ;
#26705 = DIRECTION ( 'NONE',  ( 0.000000000000000000, 0.000000000000000000, 1.000000000000000000 ) ) ;
#26706 = EDGE_CURVE ( 'NONE', #25402, #19772, #30014, .T. ) ;
#26707 = VERTEX_POINT ( 'NONE', #68789 ) ;
#26708 = CYLINDRICAL_SURFACE ( 'NONE', #40615, 2.649999999999999467 ) ;
#26709 = ORIENTED_EDGE ( 'NONE', *, *, #73298, .F. ) ;
#26710 = DIRECTION ( 'NONE',  ( 1.000000000000000000, 0.000000000000000000, 0.000000000000000000 ) ) ;
#26711 = ORIENTED_EDGE ( 'NONE', *, *, #41414, .T. ) ;
#26712 = EDGE_CURVE ( 'NONE', #66935, #16641, #24390, .T. ) ;
#26713 = ORIENTED_EDGE ( 'NONE', *, *, #71180, .T. ) ;
#26714 = VERTEX_POINT ( 'NONE', #29639 ) ;
#26715 = CARTESIAN_POINT ( 'NONE',  ( 93.84685191531249870, -208.0026889286704943, 74.93197916753379673 ) ) ;
#26716 = CONTEXT_DEPENDENT_SHAPE_REPRESENTATION ( #14807, #23040 ) ;
#26717 = LINE ( 'NONE', #10178, #9028 ) ;
#26718 = ORIENTED_EDGE ( 'NONE', *, *, #4074, .T. ) ;
#26719 = VECTOR ( 'NONE', #46783, 1000.000000000000000 ) ;
#26720 = VERTEX_POINT ( 'NONE', #17642 ) ;
#26721 = VERTEX_POINT ( 'NONE', #52582 ) ;
#26722 = PLANE ( 'NONE',  #73279 ) ;
#26723 =( BOUNDED_SURFACE ( )  B_SPLINE_SURFACE ( 1, 2, ( 
 ( #49301, #72587, #3466, #43685, #56060, #37307, #66605, #61706, #10189, #32739, #33111, #21088, #55689, #32006, #44046, #50410, #4205, #8722, #15457, #15085, #73337, #31638, #48927, #38027, #27097, #44419, #32374, #50029, #67340, #55317, #21844, #65872, #71850, #20367, #51902, #63203, #50781, #63568, #57922, #22220, #45910, #57183, #33869, #68835, #10945, #17322, #16577, #12045, #5688, #29326, #40629, #46268, #74085, #6063, #62081, #45543, #51152, #22599, #444, #40255, #11665, #62464, #23342, #56815, #34605, #16204, #39895, #45161, #56443, #68467, #34987, #51529, #28222, #6425, #812, #10559, #69199, #57554, #28969, #17692, #52270, #44792, #33481, #16958, #67714, #39143, #11306, #4953, #27853, #73708, #86, #68086, #39521, #5324, #62844, #34239, #28590, #22979, #69563, #12413, #24440, #41368, #36090, #30435, #23700, #12778, #7525, #24088, #65051, #69922, #1922, #53022, #42481, #13526, #24807, #2293, #48112, #53749, #58284, #35706, #35360, #59770, #18422, #63938, #59398, #47737, #58653, #18785, #47378, #7886, #71029, #19529, #65419, #1191, #7154, #30073, #47012, #1554, #30800, #36452, #8255, #70650, #18064, #64305, #70282, #25183, #53385, #41725, #13882, #64667, #41006, #6777, #36821, #13150, #29691, #52641, #59037, #19162, #31180, #54132, #46636, #42114, #15751, #66520, #72863, #61253, #38689, #60515, #15367, #26278, #61620, #31920, #65776, #72507, #14262, #43601, #66877, #26651, #8996, #9361, #25916, #32658, #14635, #10106, #44328, #32284, #14999, #48481, #9738, #37943, #55602, #55226, #60154, #37212, #67257, #66159, #37580, #20651, #4122, #8637, #60876, #31545, #54858, #54490, #42844, #49212, #3380, #33030, #27015, #2665, #3024, #25544, #3750, #21369, #49948, #71396, #72141, #38314, #49578, #19896, #21009, #48842, #43960, #71762, #20270, #43234, #5605, #39434, #62761, #4873, #11580, #68000, #63481, #23254, #11223, #68387, #27385, #63127, #16874, #34516, #34155, #39060, #44711, #46186, #45079, #16495, #73998, #40172, #61998, #39807, #10476, #10857, #73252, #5981, #68752, #28501, #57464, #28887, #40533, #21759, #33785, #51439, #2, #22512, #11958, #17240, #69120, #57101, #51819, #33394, #67627, #22893, #16122, #45830, #365, #50327, #56358, #56737, #73623, #17605, #55972, #4488, #62380, #27773, #50700 ),
 ( #5238, #22136, #28137, #51074, #45456, #65327, #46923, #23617, #40917, #30717, #24358, #19442, #52178, #29602, #69837, #70196, #18337, #23996, #25089, #57840, #41281, #59305, #53664, #1831, #7798, #41637, #30351, #35266, #18703, #2201, #53295, #29239, #64574, #12693, #48027, #728, #6342, #52543, #34900, #35622, #46547, #52928, #6696, #63854, #69475, #29986, #17975, #24723, #13061, #35998, #64219, #58946, #1102, #70939, #12329, #7438, #58193, #58559, #7057, #47653, #19071, #1469, #47292, #70556, #42026, #64957, #13440, #42390, #36364, #9277, #20927, #54777, #66437, #49500, #66077, #71680, #72425, #8548, #37498, #55520, #26188, #43876, #8914, #44240, #25827, #2577, #19807, #9654, #3301, #72781, #31090, #31464, #48760, #49129, #20178, #2936, #4037, #36738, #43142, #38220, #32571, #55140, #61167, #20565, #32194, #14168, #72058, #26933, #3671, #8164, #43523, #14546, #49860, #54044, #59681, #54406, #14918, #66800, #60429, #15286, #26565, #31827, #37864, #60795, #21284, #13794, #25465, #48389, #42758, #71304, #65692, #37121, #60072, #5150, #56262, #16786, #33306, #39723, #38974, #11498, #28048, #51734, #63041, #68663, #22046, #28420, #10019, #67915, #73537, #44989, #74288, #68290, #34067, #10394, #22806, #4785, #57012, #38601, #62280, #44622, #4403, #16408, #34431, #73911, #50609, #57375, #51352, #27686, #21671, #5517, #10767, #33695, #39347, #5886, #45746, #62667, #17152, #56647, #45368, #40083, #50989, #22423, #28797, #61908, #11142, #277, #23170, #67168, #15671, #61538, #32937, #55888, #73166, #27297, #50231, #67541, #16032, #40831, #6610, #6970, #58113, #35179, #36282, #69030, #52457, #70475, #41932, #12970, #18981, #52845, #41554, #46462, #29892, #64871, #64493, #40448, #1385, #23901, #13352, #11860, #17515, #63770, #47203, #53212, #1010, #7356, #35907, #29518, #24276, #70115, #18617, #59221, #1749, #58857, #52094, #7717, #30631, #23527, #30268, #58475, #46840, #24636, #12241, #47569, #17883, #53576, #2119, #46098, #63394, #34813, #69756, #57751, #6255, #18253, #41195, #64134, #29156, #638, #69387, #12608, #35539, #37029, #66355, #70858, #20095, #2497, #36652, #54326, #20842, #31746, #8465, #43797, #55430, #25746, #19360, #43053, #71219, #53958, #25002, #65988, #42312, #20481, #60344, #3216, #14083 ) ),
 .UNSPECIFIED., .F., .F., .F. ) 
 B_SPLINE_SURFACE_WITH_KNOTS ( ( 2, 2 ),
 ( 3, 2, 2, 2, 2, 2, 2, 2, 2, 2, 2, 2, 2, 2, 2, 2, 2, 2, 2, 2, 2, 2, 2, 2, 2, 2, 2, 2, 2, 2, 2, 2, 2, 2, 2, 2, 2, 2, 2, 2, 2, 2, 2, 2, 2, 2, 2, 2, 2, 2, 2, 2, 2, 2, 2, 2, 2, 2, 2, 2, 2, 2, 2, 2, 2, 2, 2, 2, 2, 2, 2, 2, 2, 2, 2, 2, 2, 2, 2, 2, 2, 2, 2, 2, 2, 2, 2, 2, 2, 2, 2, 2, 2, 2, 2, 2, 2, 2, 2, 2, 2, 2, 2, 2, 2, 2, 2, 2, 2, 2, 2, 2, 2, 2, 2, 2, 2, 2, 2, 2, 2, 2, 2, 2, 2, 2, 2, 2, 2, 2, 2, 2, 2, 2, 2, 2, 2, 2, 2, 2, 2, 2, 3 ),
 ( 0.000000000000000000, 1.000000000000000000 ),
 ( 0.000000000000000000, 0.006944444444444444059, 0.01388888888888888812, 0.02083333333333333218, 0.02777777777777777624, 0.03472222222222222376, 0.04166666666666666435, 0.04861111111111111188, 0.05555555555555555247, 0.06250000000000000000, 0.06944444444444444753, 0.07638888888888889506, 0.08333333333333332871, 0.09027777777777777624, 0.09722222222222222376, 0.1041666666666666713, 0.1111111111111111049, 0.1180555555555555525, 0.1250000000000000000, 0.1319444444444444475, 0.1388888888888888951, 0.1458333333333333426, 0.1527777777777777901, 0.1597222222222222099, 0.1666666666666666574, 0.1736111111111111049, 0.1805555555555555525, 0.1875000000000000000, 0.1944444444444444475, 0.2013888888888888951, 0.2083333333333333426, 0.2152777777777777901, 0.2222222222222222099, 0.2291666666666666574, 0.2361111111111111049, 0.2430555555555555525, 0.2500000000000000000, 0.2569444444444444198, 0.2638888888888888951, 0.2708333333333333148, 0.2777777777777777901, 0.2847222222222222099, 0.2916666666666666852, 0.2986111111111111049, 0.3055555555555555802, 0.3125000000000000000, 0.3194444444444444198, 0.3263888888888888951, 0.3333333333333333148, 0.3402777777777777901, 0.3472222222222222099, 0.3541666666666666852, 0.3611111111111111049, 0.3680555555555555802, 0.3750000000000000000, 0.3819444444444444198, 0.3888888888888888951, 0.3958333333333333148, 0.4027777777777777901, 0.4097222222222222099, 0.4166666666666666852, 0.4236111111111111049, 0.4305555555555555802, 0.4375000000000000000, 0.4444444444444444198, 0.4513888888888888951, 0.4583333333333333148, 0.4652777777777777901, 0.4722222222222222099, 0.4791666666666666852, 0.4861111111111111049, 0.4930555555555555802, 0.5000000000000000000, 0.5069444444444444198, 0.5138888888888888395, 0.5208333333333333703, 0.5277777777777777901, 0.5347222222222222099, 0.5416666666666666297, 0.5486111111111111605, 0.5555555555555555802, 0.5625000000000000000, 0.5694444444444444198, 0.5763888888888888395, 0.5833333333333333703, 0.5902777777777777901, 0.5972222222222222099, 0.6041666666666666297, 0.6111111111111111605, 0.6180555555555555802, 0.6250000000000000000, 0.6319444444444444198, 0.6388888888888888395, 0.6458333333333333703, 0.6527777777777777901, 0.6597222222222222099, 0.6666666666666666297, 0.6736111111111111605, 0.6805555555555555802, 0.6875000000000000000, 0.6944444444444444198, 0.7013888888888888395, 0.7083333333333333703, 0.7152777777777777901, 0.7222222222222222099, 0.7291666666666666297, 0.7361111111111111605, 0.7430555555555555802, 0.7500000000000000000, 0.7569444444444444198, 0.7638888888888888395, 0.7708333333333333703, 0.7777777777777777901, 0.7847222222222222099, 0.7916666666666666297, 0.7986111111111111605, 0.8055555555555555802, 0.8125000000000000000, 0.8194444444444444198, 0.8263888888888888395, 0.8333333333333333703, 0.8402777777777777901, 0.8472222222222222099, 0.8541666666666666297, 0.8611111111111111605, 0.8680555555555555802, 0.8750000000000000000, 0.8819444444444444198, 0.8888888888888888395, 0.8958333333333333703, 0.9027777777777777901, 0.9097222222222222099, 0.9166666666666666297, 0.9236111111111111605, 0.9305555555555555802, 0.9375000000000000000, 0.9444444444444444198, 0.9513888888888888395, 0.9583333333333333703, 0.9652777777777777901, 0.9722222222222222099, 0.9791666666666666297, 0.9842227634901432598 ),
 .UNSPECIFIED. ) 
 GEOMETRIC_REPRESENTATION_ITEM ( )  RATIONAL_B_SPLINE_SURFACE ( (
 ( 1.000000000000000000, 0.8660254037844387076, 1.000000000000000000, 0.8660254037844387076, 1.000000000000000000, 0.8660254037844387076, 1.000000000000000000, 0.8660254037844387076, 1.000000000000000000, 0.8660254037844387076, 1.000000000000000000, 0.8660254037844387076, 1.000000000000000000, 0.8660254037844387076, 1.000000000000000000, 0.8660254037844387076, 1.000000000000000000, 0.8660254037844387076, 1.000000000000000000, 0.8660254037844387076, 1.000000000000000000, 0.8660254037844387076, 1.000000000000000000, 0.8660254037844387076, 1.000000000000000000, 0.8660254037844387076, 1.000000000000000000, 0.8660254037844387076, 1.000000000000000000, 0.8660254037844387076, 1.000000000000000000, 0.8660254037844387076, 1.000000000000000000, 0.8660254037844387076, 1.000000000000000000, 0.8660254037844387076, 1.000000000000000000, 0.8660254037844387076, 1.000000000000000000, 0.8660254037844387076, 1.000000000000000000, 0.8660254037844387076, 1.000000000000000000, 0.8660254037844387076, 1.000000000000000000, 0.8660254037844387076, 1.000000000000000000, 0.8660254037844387076, 1.000000000000000000, 0.8660254037844387076, 1.000000000000000000, 0.8660254037844387076, 1.000000000000000000, 0.8660254037844387076, 1.000000000000000000, 0.8660254037844387076, 1.000000000000000000, 0.8660254037844387076, 1.000000000000000000, 0.8660254037844387076, 1.000000000000000000, 0.8660254037844387076, 1.000000000000000000, 0.8660254037844387076, 1.000000000000000000, 0.8660254037844387076, 1.000000000000000000, 0.8660254037844387076, 1.000000000000000000, 0.8660254037844387076, 1.000000000000000000, 0.8660254037844387076, 1.000000000000000000, 0.8660254037844387076, 1.000000000000000000, 0.8660254037844387076, 1.000000000000000000, 0.8660254037844387076, 1.000000000000000000, 0.8660254037844387076, 1.000000000000000000, 0.8660254037844387076, 1.000000000000000000, 0.8660254037844387076, 1.000000000000000000, 0.8660254037844387076, 1.000000000000000000, 0.8660254037844387076, 1.000000000000000000, 0.8660254037844387076, 1.000000000000000000, 0.8660254037844387076, 1.000000000000000000, 0.8660254037844387076, 1.000000000000000000, 0.8660254037844387076, 1.000000000000000000, 0.8660254037844387076, 1.000000000000000000, 0.8660254037844387076, 1.000000000000000000, 0.8660254037844387076, 1.000000000000000000, 0.8660254037844387076, 1.000000000000000000, 0.8660254037844387076, 1.000000000000000000, 0.8660254037844387076, 1.000000000000000000, 0.8660254037844387076, 1.000000000000000000, 0.8660254037844387076, 1.000000000000000000, 0.8660254037844387076, 1.000000000000000000, 0.8660254037844387076, 1.000000000000000000, 0.8660254037844387076, 1.000000000000000000, 0.8660254037844387076, 1.000000000000000000, 0.8660254037844387076, 1.000000000000000000, 0.8660254037844387076, 1.000000000000000000, 0.8660254037844387076, 1.000000000000000000, 0.8660254037844387076, 1.000000000000000000, 0.8660254037844387076, 1.000000000000000000, 0.8660254037844387076, 1.000000000000000000, 0.8660254037844387076, 1.000000000000000000, 0.8660254037844387076, 1.000000000000000000, 0.8660254037844387076, 1.000000000000000000, 0.8660254037844387076, 1.000000000000000000, 0.8660254037844387076, 1.000000000000000000, 0.8660254037844387076, 1.000000000000000000, 0.8660254037844387076, 1.000000000000000000, 0.8660254037844387076, 1.000000000000000000, 0.8660254037844387076, 1.000000000000000000, 0.8660254037844387076, 1.000000000000000000, 0.8660254037844387076, 1.000000000000000000, 0.8660254037844387076, 1.000000000000000000, 0.8660254037844387076, 1.000000000000000000, 0.8660254037844387076, 1.000000000000000000, 0.8660254037844387076, 1.000000000000000000, 0.8660254037844387076, 1.000000000000000000, 0.8660254037844387076, 1.000000000000000000, 0.8660254037844387076, 1.000000000000000000, 0.8660254037844387076, 1.000000000000000000, 0.8660254037844387076, 1.000000000000000000, 0.8660254037844387076, 1.000000000000000000, 0.8660254037844387076, 1.000000000000000000, 0.8660254037844387076, 1.000000000000000000, 0.8660254037844387076, 1.000000000000000000, 0.8660254037844387076, 1.000000000000000000, 0.8660254037844387076, 1.000000000000000000, 0.8660254037844387076, 1.000000000000000000, 0.8660254037844387076, 1.000000000000000000, 0.8660254037844387076, 1.000000000000000000, 0.8660254037844387076, 1.000000000000000000, 0.8660254037844387076, 1.000000000000000000, 0.8660254037844387076, 1.000000000000000000, 0.8660254037844387076, 1.000000000000000000, 0.8660254037844387076, 1.000000000000000000, 0.8660254037844387076, 1.000000000000000000, 0.8660254037844387076, 1.000000000000000000, 0.8660254037844387076, 1.000000000000000000, 0.8660254037844387076, 1.000000000000000000, 0.8660254037844387076, 1.000000000000000000, 0.8660254037844387076, 1.000000000000000000, 0.8660254037844387076, 1.000000000000000000, 0.8660254037844387076, 1.000000000000000000, 0.8660254037844387076, 1.000000000000000000, 0.8660254037844387076, 1.000000000000000000, 0.8660254037844387076, 1.000000000000000000, 0.8660254037844387076, 1.000000000000000000, 0.8660254037844387076, 1.000000000000000000, 0.8660254037844387076, 1.000000000000000000, 0.8660254037844387076, 1.000000000000000000, 0.8660254037844387076, 1.000000000000000000, 0.8660254037844387076, 1.000000000000000000, 0.8660254037844387076, 1.000000000000000000, 0.8660254037844387076, 1.000000000000000000, 0.8660254037844387076, 1.000000000000000000, 0.8660254037844387076, 1.000000000000000000, 0.8660254037844387076, 1.000000000000000000, 0.8660254037844387076, 1.000000000000000000, 0.8660254037844387076, 1.000000000000000000, 0.8660254037844387076, 1.000000000000000000, 0.8660254037844387076, 1.000000000000000000, 0.8660254037844387076, 1.000000000000000000, 0.8660254037844387076, 1.000000000000000000, 0.8660254037844387076, 1.000000000000000000, 0.8660254037844387076, 1.000000000000000000, 0.8660254037844387076, 1.000000000000000000, 0.8660254037844387076, 1.000000000000000000, 0.8660254037844387076, 1.000000000000000000, 0.8660254037844387076, 1.000000000000000000, 0.8660254037844387076, 1.000000000000000000, 0.8660254037844387076, 1.000000000000000000, 0.8660254037844387076, 1.000000000000000000, 0.8660254037844387076, 1.000000000000000000, 0.8660254037844387076, 1.000000000000000000, 0.8660254037844387076, 1.000000000000000000, 0.8660254037844387076, 1.000000000000000000, 0.9024560516293040902, 0.9469512977404621612),
 ( 1.000000000000000000, 0.8660254037844387076, 1.000000000000000000, 0.8660254037844387076, 1.000000000000000000, 0.8660254037844387076, 1.000000000000000000, 0.8660254037844387076, 1.000000000000000000, 0.8660254037844387076, 1.000000000000000000, 0.8660254037844387076, 1.000000000000000000, 0.8660254037844387076, 1.000000000000000000, 0.8660254037844387076, 1.000000000000000000, 0.8660254037844387076, 1.000000000000000000, 0.8660254037844387076, 1.000000000000000000, 0.8660254037844387076, 1.000000000000000000, 0.8660254037844387076, 1.000000000000000000, 0.8660254037844387076, 1.000000000000000000, 0.8660254037844387076, 1.000000000000000000, 0.8660254037844387076, 1.000000000000000000, 0.8660254037844387076, 1.000000000000000000, 0.8660254037844387076, 1.000000000000000000, 0.8660254037844387076, 1.000000000000000000, 0.8660254037844387076, 1.000000000000000000, 0.8660254037844387076, 1.000000000000000000, 0.8660254037844387076, 1.000000000000000000, 0.8660254037844387076, 1.000000000000000000, 0.8660254037844387076, 1.000000000000000000, 0.8660254037844387076, 1.000000000000000000, 0.8660254037844387076, 1.000000000000000000, 0.8660254037844387076, 1.000000000000000000, 0.8660254037844387076, 1.000000000000000000, 0.8660254037844387076, 1.000000000000000000, 0.8660254037844387076, 1.000000000000000000, 0.8660254037844387076, 1.000000000000000000, 0.8660254037844387076, 1.000000000000000000, 0.8660254037844387076, 1.000000000000000000, 0.8660254037844387076, 1.000000000000000000, 0.8660254037844387076, 1.000000000000000000, 0.8660254037844387076, 1.000000000000000000, 0.8660254037844387076, 1.000000000000000000, 0.8660254037844387076, 1.000000000000000000, 0.8660254037844387076, 1.000000000000000000, 0.8660254037844387076, 1.000000000000000000, 0.8660254037844387076, 1.000000000000000000, 0.8660254037844387076, 1.000000000000000000, 0.8660254037844387076, 1.000000000000000000, 0.8660254037844387076, 1.000000000000000000, 0.8660254037844387076, 1.000000000000000000, 0.8660254037844387076, 1.000000000000000000, 0.8660254037844387076, 1.000000000000000000, 0.8660254037844387076, 1.000000000000000000, 0.8660254037844387076, 1.000000000000000000, 0.8660254037844387076, 1.000000000000000000, 0.8660254037844387076, 1.000000000000000000, 0.8660254037844387076, 1.000000000000000000, 0.8660254037844387076, 1.000000000000000000, 0.8660254037844387076, 1.000000000000000000, 0.8660254037844387076, 1.000000000000000000, 0.8660254037844387076, 1.000000000000000000, 0.8660254037844387076, 1.000000000000000000, 0.8660254037844387076, 1.000000000000000000, 0.8660254037844387076, 1.000000000000000000, 0.8660254037844387076, 1.000000000000000000, 0.8660254037844387076, 1.000000000000000000, 0.8660254037844387076, 1.000000000000000000, 0.8660254037844387076, 1.000000000000000000, 0.8660254037844387076, 1.000000000000000000, 0.8660254037844387076, 1.000000000000000000, 0.8660254037844387076, 1.000000000000000000, 0.8660254037844387076, 1.000000000000000000, 0.8660254037844387076, 1.000000000000000000, 0.8660254037844387076, 1.000000000000000000, 0.8660254037844387076, 1.000000000000000000, 0.8660254037844387076, 1.000000000000000000, 0.8660254037844387076, 1.000000000000000000, 0.8660254037844387076, 1.000000000000000000, 0.8660254037844387076, 1.000000000000000000, 0.8660254037844387076, 1.000000000000000000, 0.8660254037844387076, 1.000000000000000000, 0.8660254037844387076, 1.000000000000000000, 0.8660254037844387076, 1.000000000000000000, 0.8660254037844387076, 1.000000000000000000, 0.8660254037844387076, 1.000000000000000000, 0.8660254037844387076, 1.000000000000000000, 0.8660254037844387076, 1.000000000000000000, 0.8660254037844387076, 1.000000000000000000, 0.8660254037844387076, 1.000000000000000000, 0.8660254037844387076, 1.000000000000000000, 0.8660254037844387076, 1.000000000000000000, 0.8660254037844387076, 1.000000000000000000, 0.8660254037844387076, 1.000000000000000000, 0.8660254037844387076, 1.000000000000000000, 0.8660254037844387076, 1.000000000000000000, 0.8660254037844387076, 1.000000000000000000, 0.8660254037844387076, 1.000000000000000000, 0.8660254037844387076, 1.000000000000000000, 0.8660254037844387076, 1.000000000000000000, 0.8660254037844387076, 1.000000000000000000, 0.8660254037844387076, 1.000000000000000000, 0.8660254037844387076, 1.000000000000000000, 0.8660254037844387076, 1.000000000000000000, 0.8660254037844387076, 1.000000000000000000, 0.8660254037844387076, 1.000000000000000000, 0.8660254037844387076, 1.000000000000000000, 0.8660254037844387076, 1.000000000000000000, 0.8660254037844387076, 1.000000000000000000, 0.8660254037844387076, 1.000000000000000000, 0.8660254037844387076, 1.000000000000000000, 0.8660254037844387076, 1.000000000000000000, 0.8660254037844387076, 1.000000000000000000, 0.8660254037844387076, 1.000000000000000000, 0.8660254037844387076, 1.000000000000000000, 0.8660254037844387076, 1.000000000000000000, 0.8660254037844387076, 1.000000000000000000, 0.8660254037844387076, 1.000000000000000000, 0.8660254037844387076, 1.000000000000000000, 0.8660254037844387076, 1.000000000000000000, 0.8660254037844387076, 1.000000000000000000, 0.8660254037844387076, 1.000000000000000000, 0.8660254037844387076, 1.000000000000000000, 0.8660254037844387076, 1.000000000000000000, 0.8660254037844387076, 1.000000000000000000, 0.8660254037844387076, 1.000000000000000000, 0.8660254037844387076, 1.000000000000000000, 0.8660254037844387076, 1.000000000000000000, 0.8660254037844387076, 1.000000000000000000, 0.8660254037844387076, 1.000000000000000000, 0.8660254037844387076, 1.000000000000000000, 0.8660254037844387076, 1.000000000000000000, 0.8660254037844387076, 1.000000000000000000, 0.8660254037844387076, 1.000000000000000000, 0.8660254037844387076, 1.000000000000000000, 0.8660254037844387076, 1.000000000000000000, 0.8660254037844387076, 1.000000000000000000, 0.8660254037844387076, 1.000000000000000000, 0.8660254037844387076, 1.000000000000000000, 0.8660254037844387076, 1.000000000000000000, 0.8660254037844387076, 1.000000000000000000, 0.8660254037844387076, 1.000000000000000000, 0.8660254037844387076, 1.000000000000000000, 0.8660254037844387076, 1.000000000000000000, 0.8660254037844387076, 1.000000000000000000, 0.8660254037844387076, 1.000000000000000000, 0.8660254037844387076, 1.000000000000000000, 0.8660254037844387076, 1.000000000000000000, 0.9024560516293040902, 0.9469512977404621612) ) ) 
 REPRESENTATION_ITEM ( '' )  SURFACE ( )  );
#26724 = DIRECTION ( 'NONE',  ( -0.000000000000000000, -0.000000000000000000, 1.000000000000000000 ) ) ;
#26725 = CARTESIAN_POINT ( 'NONE',  ( -96.15314808468752972, 91.99731107132950569, 75.09072916753380866 ) ) ;
#26726 = AXIS2_PLACEMENT_3D ( 'NONE', #47123, #52755, #68939 ) ;
#26727 = ORIENTED_EDGE ( 'NONE', *, *, #45007, .T. ) ;
#26728 = EDGE_CURVE ( 'NONE', #40918, #74142, #57238, .T. ) ;
#26729 = CARTESIAN_POINT ( 'NONE',  ( 92.69370383062498320, 91.33154071421968467, 78.79489583420047438 ) ) ;
#26730 = AXIS2_PLACEMENT_3D ( 'NONE', #21712, #34108, #62329 ) ;
#26731 = EDGE_LOOP ( 'NONE', ( #42214, #40440, #13955, #25236 ) ) ;
#26732 = FACE_BOUND ( 'NONE', #27768, .T. ) ;
#26733 = DIRECTION ( 'NONE',  ( -1.000000000000000000, 0.000000000000000000, 0.000000000000000000 ) ) ;
#26735 = ADVANCED_FACE ( 'NONE', ( #46583 ), #22931, .T. ) ;
#26734 = CARTESIAN_POINT ( 'NONE',  ( -25.50183398199384754, -112.6408924756582053, 5.500000000000000000 ) ) ;
#26736 = CARTESIAN_POINT ( 'NONE',  ( 10.00000000000000000, -70.52718814184277107, 26.02418014898285037 ) ) ;
#26737 = CARTESIAN_POINT ( 'NONE',  ( 10.00000000000000000, 36.73666225445894185, 65.58780272294090707 ) ) ;
#26738 = EDGE_CURVE ( 'NONE', #48419, #5745, #70226, .T. ) ;
#26739 = CARTESIAN_POINT ( 'NONE',  ( -97.30629616937495996, -209.9999999999999716, 79.48281250086714067 ) ) ;
#26740 = CYLINDRICAL_SURFACE ( 'NONE', #26640, 77.49899999999999523 ) ;
#26741 = LINE ( 'NONE', #32012, #53534 ) ;
#26742 = AXIS2_PLACEMENT_3D ( 'NONE', #32112, #73070, #21955 ) ;
#26743 = EDGE_CURVE ( 'NONE', #68977, #62228, #53331, .T. ) ;
#26744 = CYLINDRICAL_SURFACE ( 'NONE', #63533, 42.00000000000000000 ) ;
#26745 = ORIENTED_EDGE ( 'NONE', *, *, #16555, .T. ) ;
#26746 = AXIS2_PLACEMENT_3D ( 'NONE', #25477, #8179, #64233 ) ;
#26747 = ORIENTED_EDGE ( 'NONE', *, *, #56208, .F. ) ;
#26748 = CARTESIAN_POINT ( 'NONE',  ( 0.000000000000000000, 10.74501242461282757, 35.92658777277515014 ) ) ;
#26749 = DIRECTION ( 'NONE',  ( 0.000000000000000000, 0.000000000000000000, 1.000000000000000000 ) ) ;
#26750 = DIRECTION ( 'NONE',  ( -1.000000000000000000, -0.000000000000000000, 0.000000000000000000 ) ) ;
#26751 = ADVANCED_FACE ( 'NONE', ( #19112 ), #24752, .T. ) ;
#26752 = CARTESIAN_POINT ( 'NONE',  ( -93.84685191531252713, 88.00268892867056536, 81.59947916753381492 ) ) ;
#26753 = DIRECTION ( 'NONE',  ( 1.000000000000000000, 0.000000000000000000, -0.000000000000000000 ) ) ;
#26754 = LINE ( 'NONE', #9844, #11019 ) ;
#26755 = ORIENTED_EDGE ( 'NONE', *, *, #30855, .F. ) ;
#26756 = CARTESIAN_POINT ( 'NONE',  ( 92.34999999999999432, 90.00000000000002842, 81.10999999999999943 ) ) ;
#26757 = CARTESIAN_POINT ( 'NONE',  ( 10.00000000000000000, -30.80686688396994910, -21.53537804866113703 ) ) ;
#26758 = DIRECTION ( 'NONE',  ( -0.000000000000000000, -0.000000000000000000, 1.000000000000000000 ) ) ;
#26759 = CARTESIAN_POINT ( 'NONE',  ( 100.0010000000000190, -123.9999999999999858, -40.00000000000002132 ) ) ;
#26760 = DIRECTION ( 'NONE',  ( 0.1850432970638656582, -0.9827303690289285187, 0.000000000000000000 ) ) ;
#26761 = CARTESIAN_POINT ( 'NONE',  ( -94.99999999999997158, -207.3369185715606307, 82.02281250086714692 ) ) ;
#26762 = DIRECTION ( 'NONE',  ( -1.000000000000000000, 0.000000000000000000, -0.000000000000000000 ) ) ;
#26763 = APPLICATION_CONTEXT ( 'automotive_design' ) ;
#26764 = ORIENTED_EDGE ( 'NONE', *, *, #57740, .F. ) ;
#26765 = DIRECTION ( 'NONE',  ( 0.000000000000000000, 0.000000000000000000, 1.000000000000000000 ) ) ;
#26766 = DIRECTION ( 'NONE',  ( 0.000000000000000000, 0.000000000000000000, 1.000000000000000000 ) ) ;
#26767 = CARTESIAN_POINT ( 'NONE',  ( 10.00000000000000000, 0.000000000000000000, 0.000000000000000000 ) ) ;
#26768 = ORIENTED_EDGE ( 'NONE', *, *, #57980, .T. ) ;
#26769 = AXIS2_PLACEMENT_3D ( 'NONE', #976, #28758, #52811 ) ;
#26770 = CARTESIAN_POINT ( 'NONE',  ( 5.000000000000000000, 79.10210256391368944, 21.60688246758614284 ) ) ;
#26771 = CARTESIAN_POINT ( 'NONE',  ( -97.64999999999996305, -209.9999999999999716, 79.20499999999999829 ) ) ;
#26772 = DIRECTION ( 'NONE',  ( 0.000000000000000000, 0.000000000000000000, 1.000000000000000000 ) ) ;
#26773 = CIRCLE ( 'NONE', #6413, 77.49899999999999523 ) ;
#26774 = CARTESIAN_POINT ( 'NONE',  ( 3.250000000000000444, -13.95926121303099343, -1.199999999999999956 ) ) ;
#26775 = EDGE_LOOP ( 'NONE', ( #44277, #6274, #15055, #10427 ) ) ;
#26776 = LINE ( 'NONE', #50459, #44438 ) ;
#26777 = CARTESIAN_POINT ( 'NONE',  ( 10.00000000000000000, 30.80686688397041451, -21.53537804866048688 ) ) ;
#26778 = VERTEX_POINT ( 'NONE', #43466 ) ;
#26779 = VECTOR ( 'NONE', #60020, 1000.000000000000227 ) ;
#26780 = DIRECTION ( 'NONE',  ( 0.000000000000000000, -6.982962677686266711E-15, 1.000000000000000000 ) ) ;
#26781 = LINE ( 'NONE', #67954, #13542 ) ;
#26782 = VECTOR ( 'NONE', #15116, 1000.000000000000000 ) ;
#26783 = ORIENTED_EDGE ( 'NONE', *, *, #72989, .F. ) ;
#26784 = EDGE_CURVE ( 'NONE', #58261, #73517, #67106, .T. ) ;
#26785 = DIRECTION ( 'NONE',  ( 0.000000000000000000, 0.000000000000000000, 1.000000000000000000 ) ) ;
#26786 = AXIS2_PLACEMENT_3D ( 'NONE', #18953, #63735, #980 ) ;
#26787 = EDGE_LOOP ( 'NONE', ( #61541, #44456, #48028, #60586 ) ) ;
#26788 = CIRCLE ( 'NONE', #60421, 77.49899999999999523 ) ;
#26789 = CARTESIAN_POINT ( 'NONE',  ( 11.99999999999999822, -74.65374052328644439, -8.840884882375878107 ) ) ;
#26790 = AXIS2_PLACEMENT_3D ( 'NONE', #23362, #16595, #22618 ) ;
#26791 = AXIS2_PLACEMENT_3D ( 'NONE', #23632, #5619, #4888 ) ;
#26792 = ADVANCED_FACE ( 'NONE', ( #21231 ), #3978, .T. ) ;
#26793 = EDGE_LOOP ( 'NONE', ( #18374, #17239, #72170, #2205, #32213, #57465, #9882, #36441, #41282, #29794, #6646, #32898, #53803, #28607, #32068, #47072 ) ) ;
#26794 = VERTEX_POINT ( 'NONE', #55464 ) ;
#26795 = EDGE_CURVE ( 'NONE', #69818, #14214, #18793, .T. ) ;
#26797 = ORIENTED_EDGE ( 'NONE', *, *, #15438, .F. ) ;
#26796 = EDGE_CURVE ( 'NONE', #2735, #688, #42060, .T. ) ;
#26798 = ORIENTED_EDGE ( 'NONE', *, *, #30145, .T. ) ;
#26799 = CARTESIAN_POINT ( 'NONE',  ( -2.981742216678212820, 1.885622467846870828E-15, -15.39727592608509177 ) ) ;
#26800 = ORIENTED_EDGE ( 'NONE', *, *, #14373, .F. ) ;
#26802 = EDGE_CURVE ( 'NONE', #58339, #18110, #72727, .T. ) ;
#26801 = EDGE_LOOP ( 'NONE', ( #28645, #71297, #24147, #14256 ) ) ;
#26803 = CARTESIAN_POINT ( 'NONE',  ( 97.30629616937498838, 90.00000000000002842, 75.51406250086715488 ) ) ;
#26804 = CARTESIAN_POINT ( 'NONE',  ( 92.35000000045006630, -210.0000310946952595, 88.81037122969986797 ) ) ;
#26805 = FACE_OUTER_BOUND ( 'NONE', #42379, .T. ) ;
#26806 = ORIENTED_EDGE ( 'NONE', *, *, #58220, .F. ) ;
#26807 = ORIENTED_EDGE ( 'NONE', *, *, #58896, .T. ) ;
#26808 = EDGE_CURVE ( 'NONE', #18566, #51720, #10333, .T. ) ;
#26809 = VERTEX_POINT ( 'NONE', #9961 ) ;
#26810 = CARTESIAN_POINT ( 'NONE',  ( 97.30629616937498838, 90.00000000000002842, 89.32531250086714181 ) ) ;
#26811 = ORIENTED_EDGE ( 'NONE', *, *, #23516, .F. ) ;
#26812 = CARTESIAN_POINT ( 'NONE',  ( 93.84685191531249870, -208.0026889286704943, 85.09197916753380753 ) ) ;
#26813 = APPLICATION_PROTOCOL_DEFINITION ( 'draft international standard', 'automotive_design', 1998, #12386 ) ;
#26814 = DIRECTION ( 'NONE',  ( 0.000000000000000000, 0.000000000000000000, 1.000000000000000000 ) ) ;
#26815 = DIRECTION ( 'NONE',  ( 1.000000000000000000, 0.000000000000000000, 0.000000000000000000 ) ) ;
#26816 = DIRECTION ( 'NONE',  ( -1.000000000000000000, -0.000000000000000000, -0.000000000000000000 ) ) ;
#26817 = DIRECTION ( 'NONE',  ( -1.000000000000000000, -0.000000000000000000, -0.000000000000000000 ) ) ;
#26818 = CARTESIAN_POINT ( 'NONE',  ( 10.00000000000000000, -50.95692526931372157, 58.39081064771733054 ) ) ;
#26819 = CARTESIAN_POINT ( 'NONE',  ( 0.000000000000000000, 0.000000000000000000, 0.000000000000000000 ) ) ;
#26820 = CARTESIAN_POINT ( 'NONE',  ( -92.34999999999999432, -208.4700217866474645, 75.20979166840096752 ) ) ;
#26821 = DIRECTION ( 'NONE',  ( -1.000000000000000000, 0.000000000000000000, 0.000000000000000000 ) ) ;
#26822 = VERTEX_POINT ( 'NONE', #3618 ) ;
#26823 = CIRCLE ( 'NONE', #43642, 77.49899999999999523 ) ;
#26825 = CARTESIAN_POINT ( 'NONE',  ( -93.09170853947344426, 88.16127117233644128, 74.44346887015069569 ) ) ;
#26824 = CARTESIAN_POINT ( 'NONE',  ( 96.15314808468748708, 91.99731107132950569, 88.16114583420046813 ) ) ;
#26826 =( BOUNDED_CURVE ( )  B_SPLINE_CURVE ( 2, ( #9610, #54730, #2889, #19400, #15241, #25046, #20519 ),
 .UNSPECIFIED., .F., .F. ) 
 B_SPLINE_CURVE_WITH_KNOTS ( ( 3, 2, 2, 3 ),
 ( 0.8466920362367552633, 0.8537476304467667143, 0.8608033959876489893, 0.8678591737214811364 ),
 .UNSPECIFIED. ) 
 CURVE ( )  GEOMETRIC_REPRESENTATION_ITEM ( )  RATIONAL_B_SPLINE_CURVE ( ( 0.9999934937104295596, 0.8660286570082199598, 1.000000000000000000, 0.8660254037844387076, 1.000000000000000000, 0.8660254037844387076, 1.000000000000000000 ) ) 
 REPRESENTATION_ITEM ( '' )  );
#26827 = ORIENTED_EDGE ( 'NONE', *, *, #38320, .F. ) ;
#26828 = PLANE ( 'NONE',  #2310 ) ;
#26830 = EDGE_CURVE ( 'NONE', #65939, #23811, #32880, .T. ) ;
#26829 = CYLINDRICAL_SURFACE ( 'NONE', #37376, 77.49899999999999523 ) ;
#26831 = DIRECTION ( 'NONE',  ( -1.000000000000000000, -0.000000000000000000, 0.000000000000000000 ) ) ;
#26832 = DIRECTION ( 'NONE',  ( -0.1045284632676570929, 0.9945218953682730678, 0.000000000000000000 ) ) ;
#26833 = CARTESIAN_POINT ( 'NONE',  ( -97.30629616937495996, -209.9999999999999716, 89.64281250086713726 ) ) ;
#26834 = CARTESIAN_POINT ( 'NONE',  ( 0.000000000000000000, 0.000000000000000000, 0.000000000000000000 ) ) ;
#26835 = ORIENTED_EDGE ( 'NONE', *, *, #72990, .T. ) ;
#26836 = CARTESIAN_POINT ( 'NONE',  ( 0.000000000000000000, -44.99326035066101781, 68.55367621811127776 ) ) ;
#26837 = EDGE_CURVE ( 'NONE', #70257, #5113, #70596, .T. ) ;
#26838 = EDGE_CURVE ( 'NONE', #71076, #23556, #64995, .T. ) ;
#26839 = CARTESIAN_POINT ( 'NONE',  ( 0.000000000000000000, 62.50884508063427347, 41.76106447765511831 ) ) ;
#26840 = VERTEX_POINT ( 'NONE', #21611 ) ;
#26841 = AXIS2_PLACEMENT_3D ( 'NONE', #11178, #57055, #44667 ) ;
#26842 = VERTEX_POINT ( 'NONE', #50171 ) ;
#26843 = CARTESIAN_POINT ( 'NONE',  ( -92.35000000000005116, 91.52997821335253548, 82.75041666666665208 ) ) ;
#26844 = LINE ( 'NONE', #8822, #63164 ) ;
#26845 = EDGE_CURVE ( 'NONE', #58346, #11208, #20678, .T. ) ;
#26846 = DIRECTION ( 'NONE',  ( -1.000000000000000000, 0.000000000000000000, 0.000000000000000000 ) ) ;
#26847 = CARTESIAN_POINT ( 'NONE',  ( -97.64999999999996305, -211.5299782133524218, 76.79729166840095900 ) ) ;
#26848 = DIRECTION ( 'NONE',  ( 1.000000000000000000, -7.677074106448950501E-15, -2.598394312951952234E-14 ) ) ;
#26849 = DIRECTION ( 'NONE',  ( 0.000000000000000000, 0.000000000000000000, 1.000000000000000000 ) ) ;
#26850 = DIRECTION ( 'NONE',  ( -1.000000000000000000, 0.000000000000000000, 0.000000000000000000 ) ) ;
#26851 = VECTOR ( 'NONE', #37611, 1000.000000000000000 ) ;
#26852 = VERTEX_POINT ( 'NONE', #26515 ) ;
#26853 = CARTESIAN_POINT ( 'NONE',  ( -93.84685191531254134, 91.99731107132950569, 80.54114583420046358 ) ) ;
#26854 = CARTESIAN_POINT ( 'NONE',  ( -7.500000000000014211, -69.70000000000003126, -255.0000000000000000 ) ) ;
#26855 = VECTOR ( 'NONE', #48036, 1000.000000000000000 ) ;
#26856 = FACE_OUTER_BOUND ( 'NONE', #5751, .T. ) ;
#26857 = DIRECTION ( 'NONE',  ( 0.000000000000000000, -0.7071067811865388020, -0.7071067811865561215 ) ) ;
#26858 = LINE ( 'NONE', #72702, #60524 ) ;
#26859 = CYLINDRICAL_SURFACE ( 'NONE', #64647, 82.00000000000000000 ) ;
#26860 = FACE_OUTER_BOUND ( 'NONE', #9642, .T. ) ;
#26861 = DIRECTION ( 'NONE',  ( -0.000000000000000000, -0.000000000000000000, -1.000000000000000000 ) ) ;
#26862 = CARTESIAN_POINT ( 'NONE',  ( 94.99999999999998579, 87.33691857156068750, 79.80031250086715033 ) ) ;
#26863 = CIRCLE ( 'NONE', #48502, 31.99999999999998934 ) ;
#26864 = CARTESIAN_POINT ( 'NONE',  ( -94.99999999999997158, -212.6630814284392557, 82.34031250086714238 ) ) ;
#26865 = DIRECTION ( 'NONE',  ( 0.000000000000000000, 0.000000000000000000, 1.000000000000000000 ) ) ;
#26866 = EDGE_LOOP ( 'NONE', ( #66664, #9167, #24510, #8085 ) ) ;
#26867 = CARTESIAN_POINT ( 'NONE',  ( -92.35000000000005116, 88.47002178664754979, 87.16895833506762870 ) ) ;
#26868 = CARTESIAN_POINT ( 'NONE',  ( -94.99999999999997158, -206.9400435732949575, 76.50624999999999432 ) ) ;
#26869 = DIRECTION ( 'NONE',  ( 0.000000000000000000, 0.000000000000000000, 1.000000000000000000 ) ) ;
#26870 = CARTESIAN_POINT ( 'NONE',  ( -92.69370383062505425, 88.66845928578038638, 76.73114583420048973 ) ) ;
#26871 = CARTESIAN_POINT ( 'NONE',  ( 92.69370383062501162, -211.3315407142195852, 83.98072916753380923 ) ) ;
#26872 = VERTEX_POINT ( 'NONE', #36397 ) ;
#26873 = AXIS2_PLACEMENT_3D ( 'NONE', #49788, #26119, #60358 ) ;
#26874 = DIRECTION ( 'NONE',  ( -1.000000000000000000, -0.000000000000000000, -0.000000000000000000 ) ) ;
#26875 = VERTEX_POINT ( 'NONE', #14864 ) ;
#26876 = DIRECTION ( 'NONE',  ( 1.000000000000000000, 0.000000000000000000, -0.000000000000000000 ) ) ;
#26877 = ORIENTED_EDGE ( 'NONE', *, *, #27240, .T. ) ;
#26878 = AXIS2_PLACEMENT_3D ( 'NONE', #70040, #1675, #30559 ) ;
#26879 = LINE ( 'NONE', #34008, #23757 ) ;
#26880 = AXIS2_PLACEMENT_3D ( 'NONE', #18484, #64730, #46696 ) ;
#26881 = ADVANCED_FACE ( 'NONE', ( #61850 ), #47686, .T. ) ;
#26882 = ORIENTED_EDGE ( 'NONE', *, *, #9136, .T. ) ;
#26883 = EDGE_LOOP ( 'NONE', ( #4453, #55914, #65318, #59276 ) ) ;
#26884 = EDGE_CURVE ( 'NONE', #26649, #22283, #72003, .T. ) ;
#26885 = CYLINDRICAL_SURFACE ( 'NONE', #37104, 31.99999999999998579 ) ;
#26886 = LINE ( 'NONE', #49816, #42925 ) ;
#26887 = DIRECTION ( 'NONE',  ( -1.000000000000000000, 0.000000000000000000, 0.000000000000000000 ) ) ;
#26888 = AXIS2_PLACEMENT_3D ( 'NONE', #58253, #2633, #24055 ) ;
#26889 = CARTESIAN_POINT ( 'NONE',  ( -96.53982248244427922, 87.90457393955784937, 74.96680960279263672 ) ) ;
#26890 = CARTESIAN_POINT ( 'NONE',  ( 96.15314808468748708, 91.99731107132950569, 87.04989583420048405 ) ) ;
#26891 = AXIS2_PLACEMENT_3D ( 'NONE', #48694, #26506, #60733 ) ;
#26892 = DIRECTION ( 'NONE',  ( 0.000000000000000000, -0.4999999999999920064, 0.8660254037844432595 ) ) ;
#26893 = CARTESIAN_POINT ( 'NONE',  ( 92.35000000000002274, -208.4700217866474645, 81.05708333333333826 ) ) ;
#26894 = ORIENTED_EDGE ( 'NONE', *, *, #21526, .T. ) ;
#26895 = ORIENTED_EDGE ( 'NONE', *, *, #73653, .T. ) ;
#26896 = VERTEX_POINT ( 'NONE', #66747 ) ;
#26897 = VERTEX_POINT ( 'NONE', #15233 ) ;
#26898 = LINE ( 'NONE', #32538, #70606 ) ;
#26899 = CIRCLE ( 'NONE', #68950, 15.80000000000028315 ) ;
#26900 =( NAMED_UNIT ( * ) SI_UNIT ( $, .STERADIAN. ) SOLID_ANGLE_UNIT ( ) );
#26901 = CYLINDRICAL_SURFACE ( 'NONE', #41503, 42.00000000000000000 ) ;
#26902 = CARTESIAN_POINT ( 'NONE',  ( -97.65000000000001990, 90.00000000000004263, 81.82437500173429612 ) ) ;
#26903 = DIRECTION ( 'NONE',  ( 0.000000000000000000, 0.000000000000000000, 1.000000000000000000 ) ) ;
#26904 = CYLINDRICAL_SURFACE ( 'NONE', #32384, 31.99999999999998579 ) ;
#26905 = EDGE_CURVE ( 'NONE', #52144, #30123, #12985, .T. ) ;
#26906 = DIRECTION ( 'NONE',  ( 0.000000000000000000, 0.000000000000000000, -1.000000000000000000 ) ) ;
#26907 = ORIENTED_EDGE ( 'NONE', *, *, #13761, .F. ) ;
#26908 = CARTESIAN_POINT ( 'NONE',  ( -97.64999999999996305, -209.9999999999999716, 85.63437500173431260 ) ) ;
#26909 = EDGE_LOOP ( 'NONE', ( #796, #3198, #2805, #27320 ) ) ;
#26910 = EDGE_CURVE ( 'NONE', #56201, #42329, #5417, .T. ) ;
#26911 = DIRECTION ( 'NONE',  ( -0.000000000000000000, -0.000000000000000000, 1.000000000000000000 ) ) ;
#26912 = AXIS2_PLACEMENT_3D ( 'NONE', #62558, #11400, #45999 ) ;
#26913 = VERTEX_POINT ( 'NONE', #69289 ) ;
#26914 = CARTESIAN_POINT ( 'NONE',  ( -92.35000000000005116, 88.47002178664754979, 81.45395833506763950 ) ) ;
#26915 = ORIENTED_EDGE ( 'NONE', *, *, #49563, .F. ) ;
#26916 = CARTESIAN_POINT ( 'NONE',  ( 92.69370383062498320, 90.00000000000002842, 82.18156250086715886 ) ) ;
#26917 = CARTESIAN_POINT ( 'NONE',  ( -95.00000000000002842, 86.94004357329504273, 76.18874999999999886 ) ) ;
#26918 = DIRECTION ( 'NONE',  ( 0.000000000000000000, 0.000000000000000000, 1.000000000000000000 ) ) ;
#26919 = DIRECTION ( 'NONE',  ( -0.000000000000000000, -0.000000000000000000, 1.000000000000000000 ) ) ;
#26920 = LINE ( 'NONE', #14157, #46248 ) ;
#26921 = DIRECTION ( 'NONE',  ( -1.000000000000000000, 0.000000000000000000, 0.000000000000000000 ) ) ;
#26922 = ORIENTED_EDGE ( 'NONE', *, *, #53546, .T. ) ;
#26923 = CYLINDRICAL_SURFACE ( 'NONE', #59119, 42.00000000000000000 ) ;
#26924 = EDGE_CURVE ( 'NONE', #17282, #26612, #906, .T. ) ;
#26925 = ADVANCED_FACE ( 'NONE', ( #40347 ), #28684, .F. ) ;
#26926 = CARTESIAN_POINT ( 'NONE',  ( 5.000000000000000000, 77.16300072079700101, -27.74655509720590629 ) ) ;
#26927 = ORIENTED_EDGE ( 'NONE', *, *, #59410, .T. ) ;
#26928 = ORIENTED_EDGE ( 'NONE', *, *, #4675, .T. ) ;
#26929 = DIRECTION ( 'NONE',  ( 0.000000000000000000, 0.000000000000000000, 1.000000000000000000 ) ) ;
#26930 = AXIS2_PLACEMENT_3D ( 'NONE', #54043, #71303, #21282 ) ;
#26931 = CARTESIAN_POINT ( 'NONE',  ( 15.00000000000000000, -20.55727247249748402, -16.78983467731284307 ) ) ;
#26932 = FACE_OUTER_BOUND ( 'NONE', #14464, .T. ) ;
#26933 = CARTESIAN_POINT ( 'NONE',  ( -97.30629616937497417, -211.3315407142195852, 84.13947916753383538 ) ) ;
#26934 = VERTEX_POINT ( 'NONE', #62556 ) ;
#26935 = CARTESIAN_POINT ( 'NONE',  ( 93.67500000000001137, -212.2949673200287179, 81.21583333333333599 ) ) ;
#26936 = ORIENTED_EDGE ( 'NONE', *, *, #23800, .T. ) ;
#26937 = CYLINDRICAL_SURFACE ( 'NONE', #45117, 30.50000000000000000 ) ;
#26938 = VECTOR ( 'NONE', #60124, 1000.000000000000114 ) ;
#26939 = CYLINDRICAL_SURFACE ( 'NONE', #49133, 82.00000000000000000 ) ;
#26940 = CARTESIAN_POINT ( 'NONE',  ( 92.35000000000000853, -208.4700217866474645, 83.04145833506764518 ) ) ;
#26941 = CARTESIAN_POINT ( 'NONE',  ( 96.15314808468748708, 88.00268892867053694, 79.05947916753380866 ) ) ;
#26942 = CARTESIAN_POINT ( 'NONE',  ( 23.50000000000708411, -120.0000000000001705, -49.00000000000058265 ) ) ;
#26943 = CARTESIAN_POINT ( 'NONE',  ( 10.00000000000000000, -27.75498641678720446, -31.52238457039628727 ) ) ;
#26944 = DIRECTION ( 'NONE',  ( -2.628368902995164490E-16, -1.000000000000000000, 0.000000000000000000 ) ) ;
#26945 = CARTESIAN_POINT ( 'NONE',  ( -0.8179331680533066251, -5.301268757141566645, -5.826062401966622062 ) ) ;
#26946 = CARTESIAN_POINT ( 'NONE',  ( 10.00000000000000000, -37.58145647212455032, 16.68533520207890319 ) ) ;
#26947 = CARTESIAN_POINT ( 'NONE',  ( 0.000000000000000000, -3.894527615418457600, 81.90746397400387480 ) ) ;
#26948 = AXIS2_PLACEMENT_3D ( 'NONE', #694, #12295, #13028 ) ;
#26949 = CIRCLE ( 'NONE', #8930, 16.00000000000000355 ) ;
#26950 = CARTESIAN_POINT ( 'NONE',  ( -18.24502636017238899, -100.7225776329765665, 5.500000000000000000 ) ) ;
#26951 = CARTESIAN_POINT ( 'NONE',  ( 11.99999999999999822, 36.72794159290334903, -65.59268652807170952 ) ) ;
#26952 = ORIENTED_EDGE ( 'NONE', *, *, #15778, .F. ) ;
#26953 = AXIS2_PLACEMENT_3D ( 'NONE', #57947, #111, #29354 ) ;
#26954 = CARTESIAN_POINT ( 'NONE',  ( -96.15314808468751551, 88.00268892867056536, 84.66864583420047552 ) ) ;
#26955 = AXIS2_PLACEMENT_3D ( 'NONE', #9384, #9017, #31940 ) ;
#26956 = DIRECTION ( 'NONE',  ( 1.000000000000000000, -3.061616997868382648E-16, -0.000000000000000000 ) ) ;
#26957 = FACE_OUTER_BOUND ( 'NONE', #42723, .T. ) ;
#26958 = VECTOR ( 'NONE', #62804, 1000.000000000000114 ) ;
#26959 = EDGE_LOOP ( 'NONE', ( #66384, #62223, #53020, #34147 ) ) ;
#26960 = DIRECTION ( 'NONE',  ( -0.000000000000000000, -0.000000000000000000, 1.000000000000000000 ) ) ;
#26961 = CYLINDRICAL_SURFACE ( 'NONE', #61230, 16.00000000000000000 ) ;
#26962 = DIRECTION ( 'NONE',  ( -1.000000000000000000, 0.000000000000000000, -0.000000000000000000 ) ) ;
#26963 = PRODUCT_RELATED_PRODUCT_CATEGORY ( 'part', '', ( #48755 ) ) ;
#26964 = VECTOR ( 'NONE', #25266, 1000.000000000000000 ) ;
#26965 = EDGE_CURVE ( 'NONE', #23740, #56929, #534, .T. ) ;
#26966 = DIRECTION ( 'NONE',  ( 0.000000000000000000, 0.000000000000000000, 1.000000000000000000 ) ) ;
#26967 = CARTESIAN_POINT ( 'NONE',  ( 92.69370383062501162, -208.6684592857803011, 77.04864583420048518 ) ) ;
#26968 = EDGE_CURVE ( 'NONE', #15280, #67382, #34422, .T. ) ;
#26969 = ORIENTED_EDGE ( 'NONE', *, *, #33242, .T. ) ;
#26970 = VERTEX_POINT ( 'NONE', #16676 ) ;
#26971 = EDGE_CURVE ( 'NONE', #31889, #52806, #23547, .T. ) ;
#26972 = CARTESIAN_POINT ( 'NONE',  ( 0.000000000000000000, -69.42325613327466272, 34.44570377933573724 ) ) ;
#26973 = DIRECTION ( 'NONE',  ( 0.000000000000000000, 0.000000000000000000, 1.000000000000000000 ) ) ;
#26974 = FACE_OUTER_BOUND ( 'NONE', #4587, .T. ) ;
#26975 = DIRECTION ( 'NONE',  ( -1.000000000000000000, 0.000000000000000000, -0.000000000000000000 ) ) ;
#26976 = EDGE_CURVE ( 'NONE', #11203, #32827, #70408, .T. ) ;
#26977 = DIRECTION ( 'NONE',  ( -1.000000000000000000, -0.000000000000000000, 0.000000000000000000 ) ) ;
#26978 = CARTESIAN_POINT ( 'NONE',  ( 95.00000000000000000, -212.6630814284392557, 75.35531250086715715 ) ) ;
#26979 = ORIENTED_EDGE ( 'NONE', *, *, #71614, .F. ) ;
#26980 = DIRECTION ( 'NONE',  ( -0.000000000000000000, -0.000000000000000000, -1.000000000000000000 ) ) ;
#26981 = ORIENTED_EDGE ( 'NONE', *, *, #42204, .T. ) ;
#26982 = VERTEX_POINT ( 'NONE', #29059 ) ;
#26983 = DIRECTION ( 'NONE',  ( -1.000000000000000000, 0.000000000000000000, 0.000000000000000000 ) ) ;
#26984 = LINE ( 'NONE', #37553, #22133 ) ;
#26985 = ORIENTED_EDGE ( 'NONE', *, *, #29943, .T. ) ;
#26986 = PLANE ( 'NONE',  #60614 ) ;
#26987 = CARTESIAN_POINT ( 'NONE',  ( 92.35000000000000853, -209.9999999999999716, 79.28437500173430408 ) ) ;
#26988 = CARTESIAN_POINT ( 'NONE',  ( 92.34999999999999432, 90.00000000000002842, 82.37999999999999545 ) ) ;
#26989 = ADVANCED_FACE ( 'NONE', ( #23430 ), #177, .F. ) ;
#26990 = ORIENTED_EDGE ( 'NONE', *, *, #19522, .T. ) ;
#26991 = CARTESIAN_POINT ( 'NONE',  ( -5.000000000000000000, -4.846777557549235459E-18, -0.5080592402122449114 ) ) ;
#26992 = VERTEX_POINT ( 'NONE', #33962 ) ;
#26993 = EDGE_CURVE ( 'NONE', #45152, #15229, #12134, .T. ) ;
#26994 = DIRECTION ( 'NONE',  ( -0.000000000000000000, -0.000000000000000000, -1.000000000000000000 ) ) ;
#26995 = ORIENTED_EDGE ( 'NONE', *, *, #2529, .F. ) ;
#26996 = CARTESIAN_POINT ( 'NONE',  ( 0.000000000000000000, 37.01155633439059756, 6.555932627142549762 ) ) ;
#26997 = CARTESIAN_POINT ( 'NONE',  ( -92.69370383062505425, 91.33154071421968467, 83.18697916753382060 ) ) ;
#26998 = AXIS2_PLACEMENT_3D ( 'NONE', #17272, #63151, #57502 ) ;
#26999 = CARTESIAN_POINT ( 'NONE',  ( 93.84685191531248449, 91.99731107132950569, 80.01197916753380923 ) ) ;
#27000 = ORIENTED_EDGE ( 'NONE', *, *, #54552, .F. ) ;
#27001 = CARTESIAN_POINT ( 'NONE',  ( 1.560000000000000053, 0.8660254037844389297, -1.500000000000000000 ) ) ;
#27002 = DIRECTION ( 'NONE',  ( 0.000000000000000000, 0.000000000000000000, 1.000000000000000000 ) ) ;
#27003 = ORIENTED_EDGE ( 'NONE', *, *, #74059, .T. ) ;
#27004 = CARTESIAN_POINT ( 'NONE',  ( 2.047646702416564768, -96.54137380445985173, 5.500000000000000000 ) ) ;
#27005 = VECTOR ( 'NONE', #66286, 1000.000000000000000 ) ;
#27006 = CARTESIAN_POINT ( 'NONE',  ( -97.30629616937495996, -209.9999999999999716, 82.02281250086714692 ) ) ;
#27007 = VERTEX_POINT ( 'NONE', #68560 ) ;
#27008 = EDGE_LOOP ( 'NONE', ( #63288, #14780, #19431, #64485 ) ) ;
#27010 = CARTESIAN_POINT ( 'NONE',  ( 92.34999999999993747, 91.52997821335250705, 79.15208333333333712 ) ) ;
#27009 = AXIS2_PLACEMENT_3D ( 'NONE', #39814, #57108, #67266 ) ;
#27011 = ORIENTED_EDGE ( 'NONE', *, *, #29050, .T. ) ;
#27012 = CARTESIAN_POINT ( 'NONE',  ( -97.64999999947046661, -209.9999663481462164, 81.18829462297327382 ) ) ;
#27013 = LINE ( 'NONE', #65773, #23921 ) ;
#27014 = ORIENTED_EDGE ( 'NONE', *, *, #50938, .T. ) ;
#27015 = CARTESIAN_POINT ( 'NONE',  ( -93.84685191531248449, -208.0026889286704943, 78.63614583420047666 ) ) ;
#27016 = ORIENTED_EDGE ( 'NONE', *, *, #28207, .F. ) ;
#27017 = CARTESIAN_POINT ( 'NONE',  ( 0.000000000000000000, 22.74946021919175720, -29.81001611430984255 ) ) ;
#27018 = CARTESIAN_POINT ( 'NONE',  ( 10.00000000000000000, -20.40083707022829174, -72.35432306680507963 ) ) ;
#27019 = CARTESIAN_POINT ( 'NONE',  ( 0.000000000000000000, 0.000000000000000000, -1.466666666666671670 ) ) ;
#27020 = DIRECTION ( 'NONE',  ( 0.000000000000000000, 0.7604059656000276002, 0.6494480483301876550 ) ) ;
#27021 = AXIS2_PLACEMENT_3D ( 'NONE', #70546, #1456, #19059 ) ;
#27022 = CARTESIAN_POINT ( 'NONE',  ( 10.00000000000000000, 6.736453364083557105, 36.88895765772635826 ) ) ;
#27023 = CIRCLE ( 'NONE', #52258, 31.99999999999999645 ) ;
#27024 = CARTESIAN_POINT ( 'NONE',  ( 95.00000000000000000, -206.9400435732949575, 82.30062500173427509 ) ) ;
#27025 = CARTESIAN_POINT ( 'NONE',  ( 97.30629616937498838, 91.33154071421968467, 88.10822916753380696 ) ) ;
#27026 = FACE_OUTER_BOUND ( 'NONE', #72267, .T. ) ;
#27027 = CARTESIAN_POINT ( 'NONE',  ( 0.000000000000000000, 21.60688246758585507, 79.10210256391376049 ) ) ;
#27028 = CARTESIAN_POINT ( 'NONE',  ( -92.35000000005469190, 89.99998298270445218, 88.49187441316097136 ) ) ;
#27029 = DIRECTION ( 'NONE',  ( 0.000000000000000000, -0.9781476007338070211, 0.2079116908177525425 ) ) ;
#27030 = CARTESIAN_POINT ( 'NONE',  ( 10.00000000000000000, 73.44644590900094272, -24.73286445877628026 ) ) ;
#27031 = CYLINDRICAL_SURFACE ( 'NONE', #65074, 42.00000000000000000 ) ;
#27032 =( BOUNDED_SURFACE ( )  B_SPLINE_SURFACE ( 1, 2, ( 
 ( #58385, #73913, #7263, #62670, #59136, #18889, #29800, #64042, #44991, #30177, #12516, #53121, #1297, #33697, #39349, #41834, #39725, #12146, #69668, #50991, #24186, #50611, #67918, #22426, #1660, #64780, #35453, #24543, #35092, #58017, #47481, #70385, #47121, #70021, #13262, #16410, #36194, #918, #18526, #41467, #62283, #45370, #10769, #68293, #64407, #16788, #6522, #29426, #23806, #46747, #18166, #41109, #25293, #66261, #32022, #14374, #30909, #71871, #2403, #8739, #59882, #49315, #20386, #14735, #72246, #20749, #48221, #48940, #60619, #2026, #36930, #71132, #70766, #37686, #31652, #8370, #31286, #54959, #3482, #26392, #43699, #66621, #7992, #15103, #42957, #9100, #26016, #43341, #37320, #60257, #65891, #24910, #38045, #54599, #60973, #3124, #13624, #19267, #30541, #19634, #42579, #48589, #36553, #53489, #47841, #42223, #59505, #65155, #53855, #65518, #13990, #54240, #2767, #25653, #71500, #19999, #16219, #45560, #32392, #33886, #10207, #27871, #39162, #39534, #38420, #21107, #55333, #62096, #56831, #55707, #3851, #72601, #33130, #27114, #10958, #4221, #45178, #5336, #67732, #9842, #50796, #50047, #10571, #38789, #28234, #73722, #68102, #51169, #74100, #72972, #22237, #62483, #26752, #15857, #21478, #49677, #16590, #33499, #61722, #56077, #22612, #68484, #16972, #39912, #9466, #61356, #44060, #21862, #66977, #4968, #15477, #56464, #32756, #44441, #67354, #27496, #4593, #50433, #73353, #44806, #11320, #63954, #35001, #35722, #62861, #47027, #51547, #12429, #11678, #69214, #47394, #41381, #30089, #45926, #1571, #52285, #58667, #69936, #68853, #46283, #18439, #34620, #57936, #40269, #17337, #34251, #101, #29342, #52654, #35373, #17704, #69579, #57571, #64318, #461, #70295, #53034, #6080, #28602, #24101, #41019, #40640, #63589, #12794, #7172, #24456, #18801, #57196, #63217, #5704, #830, #22991, #58299, #6794, #46648, #29707, #28981, #1207, #6439, #51915, #23356, #12063, #18082, #23716, #54148, #71043, #31563, #41742, #37228, #30452, #25560, #42133, #2306, #43252, #8650, #48856, #24824, #20284, #13897, #3039, #14278, #47751, #30819, #60171, #65065, #19544, #70665, #19181, #13170, #53399, #65432, #42863, #48497, #53764, #31197, #13539, #54509, #59413, #66175, #71779, #8269, #36838, #36107, #25928, #59789 ),
 ( #48131, #25201, #64683, #42494, #59049, #7539, #1937, #36466, #7898, #2679, #71409, #65793, #19908, #70164, #333, #53266, #34486, #63449, #69440, #12662, #693, #47620, #69083, #57803, #1441, #24326, #57429, #29949, #18667, #46514, #11922, #29210, #1802, #12293, #58165, #24688, #47261, #52899, #41609, #1066, #35592, #64549, #35232, #5944, #6663, #29568, #46896, #64929, #28853, #17568, #70529, #19040, #30322, #35964, #63820, #13027, #51784, #52510, #40884, #23960, #58916, #58528, #7407, #52148, #41993, #17943, #23227, #46152, #69805, #7023, #18305, #41248, #40502, #64188, #34867, #6307, #23580, #20898, #37085, #60036, #20146, #7771, #14890, #37832, #55108, #36334, #60763, #14133, #31797, #43108, #43488, #42361, #25059, #59279, #66040, #9242, #59648, #30685, #2172, #8520, #31058, #32162, #8132, #49096, #3635, #71650, #13769, #54742, #54015, #14513, #42725, #26534, #3267, #72020, #49467, #72391, #2553, #26158, #66409, #53630, #19778, #25434, #48000, #20533, #37469, #65659, #31434, #43848, #13405, #70912, #19412, #65299, #36705, #48361, #25797, #71274, #8881, #54375, #60400, #2906, #48727, #47429, #52322, #12832, #23396, #52697, #51951, #13572, #36506, #12469, #18477, #70709, #42168, #24860, #40687, #63632, #13207, #70334, #63990, #58708, #1609, #30125, #1972, #59087, #69972, #36140, #35408, #1245, #58337, #41418, #502, #7207, #24495, #18120, #18840, #23751, #19217, #64358, #6830, #69249, #59453, #47789, #41780, #53074, #64724, #865, #35757, #46321, #24142, #17738, #7937, #12100, #29741, #7577, #65102, #35039, #57972, #6479, #29382, #30493, #53436, #47070, #46692, #69621, #41058, #55286, #37992, #48894, #15054, #65831, #31600, #14318, #20329, #53800, #37634, #54911, #71448, #3435, #2714, #49628, #43288, #15421, #26698, #32342, #60206, #66575, #48169, #54545, #37269, #8688, #60925, #31969, #72193, #48533, #9414, #42906, #20701, #2348, #25967, #26341, #3073, #71818, #38367, #66212, #3804, #43651, #72556, #61308, #14686, #60571, #9048, #49269, #21061, #25243, #44011, #66926, #30854, #59824, #71077, #19580, #19949, #42529, #65472, #54188, #13936, #36876, #8313, #31238, #25596, #21813, #38742, #4544, #51496, #62050, #33451, #56, #74051, #5293, #16930, #50750, #62436, #45510, #10526, #55653, #56413 ) ),
 .UNSPECIFIED., .F., .F., .F. ) 
 B_SPLINE_SURFACE_WITH_KNOTS ( ( 2, 2 ),
 ( 3, 2, 2, 2, 2, 2, 2, 2, 2, 2, 2, 2, 2, 2, 2, 2, 2, 2, 2, 2, 2, 2, 2, 2, 2, 2, 2, 2, 2, 2, 2, 2, 2, 2, 2, 2, 2, 2, 2, 2, 2, 2, 2, 2, 2, 2, 2, 2, 2, 2, 2, 2, 2, 2, 2, 2, 2, 2, 2, 2, 2, 2, 2, 2, 2, 2, 2, 2, 2, 2, 2, 2, 2, 2, 2, 2, 2, 2, 2, 2, 2, 2, 2, 2, 2, 2, 2, 2, 2, 2, 2, 2, 2, 2, 2, 2, 2, 2, 2, 2, 2, 2, 2, 2, 2, 2, 2, 2, 2, 2, 2, 2, 2, 2, 2, 2, 2, 2, 2, 2, 2, 2, 2, 2, 2, 2, 2, 2, 2, 2, 2, 2, 2, 2, 2, 2, 2, 2, 2, 2, 2, 2, 3 ),
 ( 0.000000000000000000, 1.000000000000000000 ),
 ( 0.000000000000000000, 0.006944444444444444059, 0.01388888888888888812, 0.02083333333333333218, 0.02777777777777777624, 0.03472222222222222376, 0.04166666666666666435, 0.04861111111111111188, 0.05555555555555555247, 0.06250000000000000000, 0.06944444444444444753, 0.07638888888888889506, 0.08333333333333332871, 0.09027777777777777624, 0.09722222222222222376, 0.1041666666666666713, 0.1111111111111111049, 0.1180555555555555525, 0.1250000000000000000, 0.1319444444444444475, 0.1388888888888888951, 0.1458333333333333426, 0.1527777777777777901, 0.1597222222222222099, 0.1666666666666666574, 0.1736111111111111049, 0.1805555555555555525, 0.1875000000000000000, 0.1944444444444444475, 0.2013888888888888951, 0.2083333333333333426, 0.2152777777777777901, 0.2222222222222222099, 0.2291666666666666574, 0.2361111111111111049, 0.2430555555555555525, 0.2500000000000000000, 0.2569444444444444198, 0.2638888888888888951, 0.2708333333333333148, 0.2777777777777777901, 0.2847222222222222099, 0.2916666666666666852, 0.2986111111111111049, 0.3055555555555555802, 0.3125000000000000000, 0.3194444444444444198, 0.3263888888888888951, 0.3333333333333333148, 0.3402777777777777901, 0.3472222222222222099, 0.3541666666666666852, 0.3611111111111111049, 0.3680555555555555802, 0.3750000000000000000, 0.3819444444444444198, 0.3888888888888888951, 0.3958333333333333148, 0.4027777777777777901, 0.4097222222222222099, 0.4166666666666666852, 0.4236111111111111049, 0.4305555555555555802, 0.4375000000000000000, 0.4444444444444444198, 0.4513888888888888951, 0.4583333333333333148, 0.4652777777777777901, 0.4722222222222222099, 0.4791666666666666852, 0.4861111111111111049, 0.4930555555555555802, 0.5000000000000000000, 0.5069444444444444198, 0.5138888888888888395, 0.5208333333333333703, 0.5277777777777777901, 0.5347222222222222099, 0.5416666666666666297, 0.5486111111111111605, 0.5555555555555555802, 0.5625000000000000000, 0.5694444444444444198, 0.5763888888888888395, 0.5833333333333333703, 0.5902777777777777901, 0.5972222222222222099, 0.6041666666666666297, 0.6111111111111111605, 0.6180555555555555802, 0.6250000000000000000, 0.6319444444444444198, 0.6388888888888888395, 0.6458333333333333703, 0.6527777777777777901, 0.6597222222222222099, 0.6666666666666666297, 0.6736111111111111605, 0.6805555555555555802, 0.6875000000000000000, 0.6944444444444444198, 0.7013888888888888395, 0.7083333333333333703, 0.7152777777777777901, 0.7222222222222222099, 0.7291666666666666297, 0.7361111111111111605, 0.7430555555555555802, 0.7500000000000000000, 0.7569444444444444198, 0.7638888888888888395, 0.7708333333333333703, 0.7777777777777777901, 0.7847222222222222099, 0.7916666666666666297, 0.7986111111111111605, 0.8055555555555555802, 0.8125000000000000000, 0.8194444444444444198, 0.8263888888888888395, 0.8333333333333333703, 0.8402777777777777901, 0.8472222222222222099, 0.8541666666666666297, 0.8611111111111111605, 0.8680555555555555802, 0.8750000000000000000, 0.8819444444444444198, 0.8888888888888888395, 0.8958333333333333703, 0.9027777777777777901, 0.9097222222222222099, 0.9166666666666666297, 0.9236111111111111605, 0.9305555555555555802, 0.9375000000000000000, 0.9444444444444444198, 0.9513888888888888395, 0.9583333333333333703, 0.9652777777777777901, 0.9722222222222222099, 0.9791666666666666297, 0.9842227634901433708 ),
 .UNSPECIFIED. ) 
 GEOMETRIC_REPRESENTATION_ITEM ( )  RATIONAL_B_SPLINE_SURFACE ( (
 ( 1.000000000000000000, 0.8660254037844387076, 1.000000000000000000, 0.8660254037844387076, 1.000000000000000000, 0.8660254037844387076, 1.000000000000000000, 0.8660254037844387076, 1.000000000000000000, 0.8660254037844387076, 1.000000000000000000, 0.8660254037844387076, 1.000000000000000000, 0.8660254037844387076, 1.000000000000000000, 0.8660254037844387076, 1.000000000000000000, 0.8660254037844387076, 1.000000000000000000, 0.8660254037844387076, 1.000000000000000000, 0.8660254037844387076, 1.000000000000000000, 0.8660254037844387076, 1.000000000000000000, 0.8660254037844387076, 1.000000000000000000, 0.8660254037844387076, 1.000000000000000000, 0.8660254037844387076, 1.000000000000000000, 0.8660254037844387076, 1.000000000000000000, 0.8660254037844387076, 1.000000000000000000, 0.8660254037844387076, 1.000000000000000000, 0.8660254037844387076, 1.000000000000000000, 0.8660254037844387076, 1.000000000000000000, 0.8660254037844387076, 1.000000000000000000, 0.8660254037844387076, 1.000000000000000000, 0.8660254037844387076, 1.000000000000000000, 0.8660254037844387076, 1.000000000000000000, 0.8660254037844387076, 1.000000000000000000, 0.8660254037844387076, 1.000000000000000000, 0.8660254037844387076, 1.000000000000000000, 0.8660254037844387076, 1.000000000000000000, 0.8660254037844387076, 1.000000000000000000, 0.8660254037844387076, 1.000000000000000000, 0.8660254037844387076, 1.000000000000000000, 0.8660254037844387076, 1.000000000000000000, 0.8660254037844387076, 1.000000000000000000, 0.8660254037844387076, 1.000000000000000000, 0.8660254037844387076, 1.000000000000000000, 0.8660254037844387076, 1.000000000000000000, 0.8660254037844387076, 1.000000000000000000, 0.8660254037844387076, 1.000000000000000000, 0.8660254037844387076, 1.000000000000000000, 0.8660254037844387076, 1.000000000000000000, 0.8660254037844387076, 1.000000000000000000, 0.8660254037844387076, 1.000000000000000000, 0.8660254037844387076, 1.000000000000000000, 0.8660254037844387076, 1.000000000000000000, 0.8660254037844387076, 1.000000000000000000, 0.8660254037844387076, 1.000000000000000000, 0.8660254037844387076, 1.000000000000000000, 0.8660254037844387076, 1.000000000000000000, 0.8660254037844387076, 1.000000000000000000, 0.8660254037844387076, 1.000000000000000000, 0.8660254037844387076, 1.000000000000000000, 0.8660254037844387076, 1.000000000000000000, 0.8660254037844387076, 1.000000000000000000, 0.8660254037844387076, 1.000000000000000000, 0.8660254037844387076, 1.000000000000000000, 0.8660254037844387076, 1.000000000000000000, 0.8660254037844387076, 1.000000000000000000, 0.8660254037844387076, 1.000000000000000000, 0.8660254037844387076, 1.000000000000000000, 0.8660254037844387076, 1.000000000000000000, 0.8660254037844387076, 1.000000000000000000, 0.8660254037844387076, 1.000000000000000000, 0.8660254037844387076, 1.000000000000000000, 0.8660254037844387076, 1.000000000000000000, 0.8660254037844387076, 1.000000000000000000, 0.8660254037844387076, 1.000000000000000000, 0.8660254037844387076, 1.000000000000000000, 0.8660254037844387076, 1.000000000000000000, 0.8660254037844387076, 1.000000000000000000, 0.8660254037844387076, 1.000000000000000000, 0.8660254037844387076, 1.000000000000000000, 0.8660254037844387076, 1.000000000000000000, 0.8660254037844387076, 1.000000000000000000, 0.8660254037844387076, 1.000000000000000000, 0.8660254037844387076, 1.000000000000000000, 0.8660254037844387076, 1.000000000000000000, 0.8660254037844387076, 1.000000000000000000, 0.8660254037844387076, 1.000000000000000000, 0.8660254037844387076, 1.000000000000000000, 0.8660254037844387076, 1.000000000000000000, 0.8660254037844387076, 1.000000000000000000, 0.8660254037844387076, 1.000000000000000000, 0.8660254037844387076, 1.000000000000000000, 0.8660254037844387076, 1.000000000000000000, 0.8660254037844387076, 1.000000000000000000, 0.8660254037844387076, 1.000000000000000000, 0.8660254037844387076, 1.000000000000000000, 0.8660254037844387076, 1.000000000000000000, 0.8660254037844387076, 1.000000000000000000, 0.8660254037844387076, 1.000000000000000000, 0.8660254037844387076, 1.000000000000000000, 0.8660254037844387076, 1.000000000000000000, 0.8660254037844387076, 1.000000000000000000, 0.8660254037844387076, 1.000000000000000000, 0.8660254037844387076, 1.000000000000000000, 0.8660254037844387076, 1.000000000000000000, 0.8660254037844387076, 1.000000000000000000, 0.8660254037844387076, 1.000000000000000000, 0.8660254037844387076, 1.000000000000000000, 0.8660254037844387076, 1.000000000000000000, 0.8660254037844387076, 1.000000000000000000, 0.8660254037844387076, 1.000000000000000000, 0.8660254037844387076, 1.000000000000000000, 0.8660254037844387076, 1.000000000000000000, 0.8660254037844387076, 1.000000000000000000, 0.8660254037844387076, 1.000000000000000000, 0.8660254037844387076, 1.000000000000000000, 0.8660254037844387076, 1.000000000000000000, 0.8660254037844387076, 1.000000000000000000, 0.8660254037844387076, 1.000000000000000000, 0.8660254037844387076, 1.000000000000000000, 0.8660254037844387076, 1.000000000000000000, 0.8660254037844387076, 1.000000000000000000, 0.8660254037844387076, 1.000000000000000000, 0.8660254037844387076, 1.000000000000000000, 0.8660254037844387076, 1.000000000000000000, 0.8660254037844387076, 1.000000000000000000, 0.8660254037844387076, 1.000000000000000000, 0.8660254037844387076, 1.000000000000000000, 0.8660254037844387076, 1.000000000000000000, 0.8660254037844387076, 1.000000000000000000, 0.8660254037844387076, 1.000000000000000000, 0.8660254037844387076, 1.000000000000000000, 0.8660254037844387076, 1.000000000000000000, 0.8660254037844387076, 1.000000000000000000, 0.8660254037844387076, 1.000000000000000000, 0.8660254037844387076, 1.000000000000000000, 0.8660254037844387076, 1.000000000000000000, 0.8660254037844387076, 1.000000000000000000, 0.8660254037844387076, 1.000000000000000000, 0.8660254037844387076, 1.000000000000000000, 0.8660254037844387076, 1.000000000000000000, 0.8660254037844387076, 1.000000000000000000, 0.8660254037844387076, 1.000000000000000000, 0.8660254037844387076, 1.000000000000000000, 0.8660254037844387076, 1.000000000000000000, 0.8660254037844387076, 1.000000000000000000, 0.8660254037844387076, 1.000000000000000000, 0.8660254037844387076, 1.000000000000000000, 0.8660254037844387076, 1.000000000000000000, 0.8660254037844387076, 1.000000000000000000, 0.9024560516293018697, 0.9469512977404641596),
 ( 1.000000000000000000, 0.8660254037844387076, 1.000000000000000000, 0.8660254037844387076, 1.000000000000000000, 0.8660254037844387076, 1.000000000000000000, 0.8660254037844387076, 1.000000000000000000, 0.8660254037844387076, 1.000000000000000000, 0.8660254037844387076, 1.000000000000000000, 0.8660254037844387076, 1.000000000000000000, 0.8660254037844387076, 1.000000000000000000, 0.8660254037844387076, 1.000000000000000000, 0.8660254037844387076, 1.000000000000000000, 0.8660254037844387076, 1.000000000000000000, 0.8660254037844387076, 1.000000000000000000, 0.8660254037844387076, 1.000000000000000000, 0.8660254037844387076, 1.000000000000000000, 0.8660254037844387076, 1.000000000000000000, 0.8660254037844387076, 1.000000000000000000, 0.8660254037844387076, 1.000000000000000000, 0.8660254037844387076, 1.000000000000000000, 0.8660254037844387076, 1.000000000000000000, 0.8660254037844387076, 1.000000000000000000, 0.8660254037844387076, 1.000000000000000000, 0.8660254037844387076, 1.000000000000000000, 0.8660254037844387076, 1.000000000000000000, 0.8660254037844387076, 1.000000000000000000, 0.8660254037844387076, 1.000000000000000000, 0.8660254037844387076, 1.000000000000000000, 0.8660254037844387076, 1.000000000000000000, 0.8660254037844387076, 1.000000000000000000, 0.8660254037844387076, 1.000000000000000000, 0.8660254037844387076, 1.000000000000000000, 0.8660254037844387076, 1.000000000000000000, 0.8660254037844387076, 1.000000000000000000, 0.8660254037844387076, 1.000000000000000000, 0.8660254037844387076, 1.000000000000000000, 0.8660254037844387076, 1.000000000000000000, 0.8660254037844387076, 1.000000000000000000, 0.8660254037844387076, 1.000000000000000000, 0.8660254037844387076, 1.000000000000000000, 0.8660254037844387076, 1.000000000000000000, 0.8660254037844387076, 1.000000000000000000, 0.8660254037844387076, 1.000000000000000000, 0.8660254037844387076, 1.000000000000000000, 0.8660254037844387076, 1.000000000000000000, 0.8660254037844387076, 1.000000000000000000, 0.8660254037844387076, 1.000000000000000000, 0.8660254037844387076, 1.000000000000000000, 0.8660254037844387076, 1.000000000000000000, 0.8660254037844387076, 1.000000000000000000, 0.8660254037844387076, 1.000000000000000000, 0.8660254037844387076, 1.000000000000000000, 0.8660254037844387076, 1.000000000000000000, 0.8660254037844387076, 1.000000000000000000, 0.8660254037844387076, 1.000000000000000000, 0.8660254037844387076, 1.000000000000000000, 0.8660254037844387076, 1.000000000000000000, 0.8660254037844387076, 1.000000000000000000, 0.8660254037844387076, 1.000000000000000000, 0.8660254037844387076, 1.000000000000000000, 0.8660254037844387076, 1.000000000000000000, 0.8660254037844387076, 1.000000000000000000, 0.8660254037844387076, 1.000000000000000000, 0.8660254037844387076, 1.000000000000000000, 0.8660254037844387076, 1.000000000000000000, 0.8660254037844387076, 1.000000000000000000, 0.8660254037844387076, 1.000000000000000000, 0.8660254037844387076, 1.000000000000000000, 0.8660254037844387076, 1.000000000000000000, 0.8660254037844387076, 1.000000000000000000, 0.8660254037844387076, 1.000000000000000000, 0.8660254037844387076, 1.000000000000000000, 0.8660254037844387076, 1.000000000000000000, 0.8660254037844387076, 1.000000000000000000, 0.8660254037844387076, 1.000000000000000000, 0.8660254037844387076, 1.000000000000000000, 0.8660254037844387076, 1.000000000000000000, 0.8660254037844387076, 1.000000000000000000, 0.8660254037844387076, 1.000000000000000000, 0.8660254037844387076, 1.000000000000000000, 0.8660254037844387076, 1.000000000000000000, 0.8660254037844387076, 1.000000000000000000, 0.8660254037844387076, 1.000000000000000000, 0.8660254037844387076, 1.000000000000000000, 0.8660254037844387076, 1.000000000000000000, 0.8660254037844387076, 1.000000000000000000, 0.8660254037844387076, 1.000000000000000000, 0.8660254037844387076, 1.000000000000000000, 0.8660254037844387076, 1.000000000000000000, 0.8660254037844387076, 1.000000000000000000, 0.8660254037844387076, 1.000000000000000000, 0.8660254037844387076, 1.000000000000000000, 0.8660254037844387076, 1.000000000000000000, 0.8660254037844387076, 1.000000000000000000, 0.8660254037844387076, 1.000000000000000000, 0.8660254037844387076, 1.000000000000000000, 0.8660254037844387076, 1.000000000000000000, 0.8660254037844387076, 1.000000000000000000, 0.8660254037844387076, 1.000000000000000000, 0.8660254037844387076, 1.000000000000000000, 0.8660254037844387076, 1.000000000000000000, 0.8660254037844387076, 1.000000000000000000, 0.8660254037844387076, 1.000000000000000000, 0.8660254037844387076, 1.000000000000000000, 0.8660254037844387076, 1.000000000000000000, 0.8660254037844387076, 1.000000000000000000, 0.8660254037844387076, 1.000000000000000000, 0.8660254037844387076, 1.000000000000000000, 0.8660254037844387076, 1.000000000000000000, 0.8660254037844387076, 1.000000000000000000, 0.8660254037844387076, 1.000000000000000000, 0.8660254037844387076, 1.000000000000000000, 0.8660254037844387076, 1.000000000000000000, 0.8660254037844387076, 1.000000000000000000, 0.8660254037844387076, 1.000000000000000000, 0.8660254037844387076, 1.000000000000000000, 0.8660254037844387076, 1.000000000000000000, 0.8660254037844387076, 1.000000000000000000, 0.8660254037844387076, 1.000000000000000000, 0.8660254037844387076, 1.000000000000000000, 0.8660254037844387076, 1.000000000000000000, 0.8660254037844387076, 1.000000000000000000, 0.8660254037844387076, 1.000000000000000000, 0.8660254037844387076, 1.000000000000000000, 0.8660254037844387076, 1.000000000000000000, 0.8660254037844387076, 1.000000000000000000, 0.8660254037844387076, 1.000000000000000000, 0.8660254037844387076, 1.000000000000000000, 0.8660254037844387076, 1.000000000000000000, 0.8660254037844387076, 1.000000000000000000, 0.8660254037844387076, 1.000000000000000000, 0.8660254037844387076, 1.000000000000000000, 0.8660254037844387076, 1.000000000000000000, 0.8660254037844387076, 1.000000000000000000, 0.8660254037844387076, 1.000000000000000000, 0.8660254037844387076, 1.000000000000000000, 0.8660254037844387076, 1.000000000000000000, 0.8660254037844387076, 1.000000000000000000, 0.8660254037844387076, 1.000000000000000000, 0.8660254037844387076, 1.000000000000000000, 0.8660254037844387076, 1.000000000000000000, 0.8660254037844387076, 1.000000000000000000, 0.8660254037844387076, 1.000000000000000000, 0.9024560516293018697, 0.9469512977404641596) ) ) 
 REPRESENTATION_ITEM ( '' )  SURFACE ( )  );
#27033 = CYLINDRICAL_SURFACE ( 'NONE', #52345, 2.649999999999985700 ) ;
#27034 = CARTESIAN_POINT ( 'NONE',  ( 97.65000000000000568, 91.52997821335252127, 75.84479166840098685 ) ) ;
#27035 = EDGE_CURVE ( 'NONE', #17023, #52404, #17048, .T. ) ;
#27036 = CARTESIAN_POINT ( 'NONE',  ( 15.00000000000000000, -13.04903810567646971, 19.60159698893442481 ) ) ;
#27037 = AXIS2_PLACEMENT_3D ( 'NONE', #23143, #46812, #46431 ) ;
#27038 = DIRECTION ( 'NONE',  ( -0.000000000000000000, -0.000000000000000000, 1.000000000000000000 ) ) ;
#27039 = CARTESIAN_POINT ( 'NONE',  ( -97.64999999999996305, -209.9999999999999716, 84.28499999999999659 ) ) ;
#27040 = EDGE_CURVE ( 'NONE', #49118, #37730, #39983, .T. ) ;
#27041 = EDGE_CURVE ( 'NONE', #71124, #12034, #45997, .T. ) ;
#27042 = CARTESIAN_POINT ( 'NONE',  ( 0.000000000000000000, 0.000000000000000000, 53.20000000000001705 ) ) ;
#27043 = CIRCLE ( 'NONE', #60667, 16.00000000000000000 ) ;
#27044 = FACE_OUTER_BOUND ( 'NONE', #57839, .T. ) ;
#27045 = CIRCLE ( 'NONE', #19854, 31.99999999999999289 ) ;
#27046 = CARTESIAN_POINT ( 'NONE',  ( 10.00000000000000000, 18.89407956138362010, -75.16055320797013906 ) ) ;
#27047 = DIRECTION ( 'NONE',  ( -1.000000000000000000, -0.000000000000000000, -0.000000000000000000 ) ) ;
#27048 = EDGE_CURVE ( 'NONE', #17672, #68345, #51723, .T. ) ;
#27049 = CARTESIAN_POINT ( 'NONE',  ( 0.000000000000000000, 0.000000000000000000, -4.400000000000001243 ) ) ;
#27050 = CIRCLE ( 'NONE', #57090, 37.49900000000000944 ) ;
#27051 = CARTESIAN_POINT ( 'NONE',  ( 92.69370383062501162, -209.9999999999999716, 87.89656250086714806 ) ) ;
#27052 = VERTEX_POINT ( 'NONE', #48576 ) ;
#27053 = EDGE_LOOP ( 'NONE', ( #4251, #32061 ) ) ;
#27054 = B_SPLINE_CURVE_WITH_KNOTS ( 'NONE', 3,
 ( #67582, #50274, #33739, #4075, #73950, #22463 ),
 .UNSPECIFIED., .F., .F.,
 ( 4, 2, 4 ),
 ( 0.000000000000000000, 0.0008269033587271741939, 0.001653806717454348388 ),
 .UNSPECIFIED. ) ;
#27055 = DIRECTION ( 'NONE',  ( 0.000000000000000000, -0.9510565162951566398, 0.3090169943749380144 ) ) ;
#27056 = FACE_OUTER_BOUND ( 'NONE', #35807, .T. ) ;
#27057 = EDGE_LOOP ( 'NONE', ( #72757, #14369, #48368, #17219 ) ) ;
#27058 = AXIS2_PLACEMENT_3D ( 'NONE', #6158, #29063, #14914 ) ;
#27059 = CARTESIAN_POINT ( 'NONE',  ( 95.00000000000000000, -212.6630814284392557, 79.00656250086714749 ) ) ;
#27060 = CARTESIAN_POINT ( 'NONE',  ( 96.15314808468748708, -208.0026889286704943, 83.87489583420048689 ) ) ;
#27061 = EDGE_CURVE ( 'NONE', #39027, #66404, #24817, .T. ) ;
#27062 = EDGE_LOOP ( 'NONE', ( #42665, #24853, #39563, #30422 ) ) ;
#27063 = VECTOR ( 'NONE', #12869, 1000.000000000000000 ) ;
#27064 = CARTESIAN_POINT ( 'NONE',  ( 95.00000000000000000, -207.3369185715606307, 86.46781250086716852 ) ) ;
#27065 = ORIENTED_EDGE ( 'NONE', *, *, #44136, .T. ) ;
#27066 = CARTESIAN_POINT ( 'NONE',  ( 11.99999999999999822, -20.40083707022935400, 72.35432306680478121 ) ) ;
#27067 = ORIENTED_EDGE ( 'NONE', *, *, #35635, .T. ) ;
#27068 = EDGE_LOOP ( 'NONE', ( #44966, #53832, #63416, #2095 ) ) ;
#27069 = AXIS2_PLACEMENT_3D ( 'NONE', #26777, #50076, #61004 ) ;
#27070 = EDGE_LOOP ( 'NONE', ( #22137, #1975, #42229, #24588 ) ) ;
#27071 = DIRECTION ( 'NONE',  ( 0.000000000000000000, 0.000000000000000000, 1.000000000000000000 ) ) ;
#27072 = ORIENTED_EDGE ( 'NONE', *, *, #43047, .T. ) ;
#27073 = CARTESIAN_POINT ( 'NONE',  ( 0.000000000000000000, 0.000000000000000000, 0.000000000000000000 ) ) ;
#27074 = LINE ( 'NONE', #20707, #29624 ) ;
#27075 = EDGE_CURVE ( 'NONE', #16641, #28106, #66834, .T. ) ;
#27076 = EDGE_LOOP ( 'NONE', ( #58003, #50583, #17234, #40727 ) ) ;
#27077 = CYLINDRICAL_SURFACE ( 'NONE', #68254, 77.49899999999999523 ) ;
#27078 = ADVANCED_FACE ( 'NONE', ( #3111 ), #65876, .T. ) ;
#27079 = VERTEX_POINT ( 'NONE', #8354 ) ;
#27080 = CARTESIAN_POINT ( 'NONE',  ( 0.000000000000000000, 0.000000000000000000, 0.000000000000000000 ) ) ;
#27081 = ADVANCED_FACE ( 'NONE', ( #8725 ), #47106, .T. ) ;
#27082 = ORIENTED_EDGE ( 'NONE', *, *, #48658, .T. ) ;
#27083 = ORIENTED_EDGE ( 'NONE', *, *, #25825, .T. ) ;
#27084 = ORIENTED_EDGE ( 'NONE', *, *, #40302, .T. ) ;
#27085 = DIRECTION ( 'NONE',  ( -1.000000000000000000, 0.000000000000000000, -0.000000000000000000 ) ) ;
#27086 = DIRECTION ( 'NONE',  ( -1.000000000000000000, -0.000000000000000000, 0.000000000000000000 ) ) ;
#27087 = VERTEX_POINT ( 'NONE', #19988 ) ;
#27088 = ORIENTED_EDGE ( 'NONE', *, *, #5812, .F. ) ;
#27089 = ORIENTED_EDGE ( 'NONE', *, *, #656, .T. ) ;
#27090 = CARTESIAN_POINT ( 'NONE',  ( 2.047646702416564768, -96.54137380445985173, 2.500000000000000000 ) ) ;
#27091 = CARTESIAN_POINT ( 'NONE',  ( 11.99999999999999822, -40.65526001592663619, 71.21200624218782593 ) ) ;
#27092 = CARTESIAN_POINT ( 'NONE',  ( -93.84685191531252713, 88.00268892867056536, 77.31322916753381946 ) ) ;
#27093 = ORIENTED_EDGE ( 'NONE', *, *, #50560, .F. ) ;
#27094 = CARTESIAN_POINT ( 'NONE',  ( 97.30629616937498838, 90.00000000000002842, 79.16531250086714522 ) ) ;
#27095 = EDGE_LOOP ( 'NONE', ( #65715, #26183, #28952, #15973 ) ) ;
#27096 =( NAMED_UNIT ( * ) SI_UNIT ( $, .STERADIAN. ) SOLID_ANGLE_UNIT ( ) );
#27097 = CARTESIAN_POINT ( 'NONE',  ( -97.30629616937495996, -209.9999999999999716, 88.37281250086715545 ) ) ;
#27098 = EDGE_LOOP ( 'NONE', ( #28662, #12501, #38181, #72273 ) ) ;
#27099 = CARTESIAN_POINT ( 'NONE',  ( 0.3487148583350060949, -5.572172074566128508, -1.686035282245279765 ) ) ;
#27100 = DIRECTION ( 'NONE',  ( 0.000000000000000000, 0.000000000000000000, 1.000000000000000000 ) ) ;
#27101 = CARTESIAN_POINT ( 'NONE',  ( 12.50000000000000000, -132.5000000000000000, 2.500000000000000000 ) ) ;
#27102 = CARTESIAN_POINT ( 'NONE',  ( -92.69370383062498320, -211.3315407142195852, 78.47739583420047893 ) ) ;
#27103 = LINE ( 'NONE', #15092, #27820 ) ;
#27104 = DIRECTION ( 'NONE',  ( -1.000000000000000000, -0.000000000000000000, -0.000000000000000000 ) ) ;
#27105 = CIRCLE ( 'NONE', #16278, 77.49899999999999523 ) ;
#27106 = LINE ( 'NONE', #27862, #71924 ) ;
#27107 = VERTEX_POINT ( 'NONE', #42943 ) ;
#27108 = AXIS2_PLACEMENT_3D ( 'NONE', #23019, #851, #45948 ) ;
#27109 = VERTEX_POINT ( 'NONE', #31641 ) ;
#27110 = CYLINDRICAL_SURFACE ( 'NONE', #58860, 77.49899999999999523 ) ;
#27111 = AXIS2_PLACEMENT_3D ( 'NONE', #33228, #16323, #21203 ) ;
#27112 = DIRECTION ( 'NONE',  ( 0.000000000000000000, 0.4539904997395413644, 0.8910065241883706744 ) ) ;
#27113 = CARTESIAN_POINT ( 'NONE',  ( 92.54662210827909519, -209.5154774236565061, 74.90854212414865287 ) ) ;
#27114 = CARTESIAN_POINT ( 'NONE',  ( -97.30629616937501680, 91.33154071421968467, 82.60489583420047666 ) ) ;
#27115 = CARTESIAN_POINT ( 'NONE',  ( 10.00000000000000000, -2.663952781845854378, -41.91543099594820632 ) ) ;
#27116 = DIRECTION ( 'NONE',  ( -1.000000000000000000, -0.000000000000000000, 0.000000000000000000 ) ) ;
#27117 = CIRCLE ( 'NONE', #69162, 15.99999999999999645 ) ;
#27118 = EDGE_LOOP ( 'NONE', ( #51133, #31465, #13299, #73770 ) ) ;
#27119 = FACE_OUTER_BOUND ( 'NONE', #59875, .T. ) ;
#27120 = EDGE_CURVE ( 'NONE', #15096, #5732, #4437, .T. ) ;
#27121 = LINE ( 'NONE', #38795, #35291 ) ;
#27122 = CARTESIAN_POINT ( 'NONE',  ( 11.59999999999999787, 1.420590287010929336E-15, -54.99999999999998579 ) ) ;
#27123 = FACE_OUTER_BOUND ( 'NONE', #52408, .T. ) ;
#27124 = AXIS2_PLACEMENT_3D ( 'NONE', #56108, #50825, #67764 ) ;
#27125 = DIRECTION ( 'NONE',  ( -1.000000000000000000, -0.000000000000000000, -0.000000000000000000 ) ) ;
#27126 = CARTESIAN_POINT ( 'NONE',  ( -93.84685191531247028, -211.9973110713294489, 79.21822916753382060 ) ) ;
#27127 = ADVANCED_FACE ( 'NONE', ( #36919 ), #70011, .T. ) ;
#27128 = ADVANCED_FACE ( 'NONE', ( #59867 ), #18513, .F. ) ;
#27129 = CARTESIAN_POINT ( 'NONE',  ( -93.67499999999998295, -212.2949673200287179, 87.11604166840096752 ) ) ;
#27130 = ORIENTED_EDGE ( 'NONE', *, *, #55576, .T. ) ;
#27131 = CARTESIAN_POINT ( 'NONE',  ( -4.250000000000000000, -13.95926121303099343, 0.000000000000000000 ) ) ;
#27132 = CARTESIAN_POINT ( 'NONE',  ( -93.33864827736698544, -211.6008015735577033, 74.79754476654878204 ) ) ;
#27133 = CARTESIAN_POINT ( 'NONE',  ( 10.00000000000000000, -39.47590169984793818, -71.87247863392455827 ) ) ;
#27134 = ORIENTED_EDGE ( 'NONE', *, *, #65043, .T. ) ;
#27135 = EDGE_CURVE ( 'NONE', #47166, #39507, #12867, .T. ) ;
#27136 = CARTESIAN_POINT ( 'NONE',  ( -10.00000000000000000, 0.000000000000000000, 0.000000000000000000 ) ) ;
#27137 = CARTESIAN_POINT ( 'NONE',  ( 0.000000000000000000, -10.41901085202107247, 40.68715046381925049 ) ) ;
#27138 = UNCERTAINTY_MEASURE_WITH_UNIT (LENGTH_MEASURE( 1.000000000000000082E-05 ), #37042, 'distance_accuracy_value', 'NONE');
#27139 = DIRECTION ( 'NONE',  ( -1.000000000000000000, 0.000000000000000000, 0.000000000000000000 ) ) ;
#27140 = VERTEX_POINT ( 'NONE', #70374 ) ;
#27141 = DIRECTION ( 'NONE',  ( 0.000000000000000000, 0.5877852522924742473, -0.8090169943749466741 ) ) ;
#27142 = FILL_AREA_STYLE_COLOUR ( '', #53503 ) ;
#27143 = ORIENTED_EDGE ( 'NONE', *, *, #55222, .F. ) ;
#27144 = DIRECTION ( 'NONE',  ( 0.000000000000000000, 0.000000000000000000, 1.000000000000000000 ) ) ;
#27145 = CARTESIAN_POINT ( 'NONE',  ( 10.00000000000000000, -26.01480285779885904, 70.53064760720306481 ) ) ;
#27146 = EDGE_CURVE ( 'NONE', #56502, #61671, #65142, .T. ) ;
#27147 = ORIENTED_EDGE ( 'NONE', *, *, #38614, .T. ) ;
#27148 = PLANE ( 'NONE',  #18630 ) ;
#27149 = ORIENTED_EDGE ( 'NONE', *, *, #49690, .T. ) ;
#27150 = CARTESIAN_POINT ( 'NONE',  ( 10.00000000000000000, -46.53671651293907274, -59.03961581697448935 ) ) ;
#27151 = CARTESIAN_POINT ( 'NONE',  ( 10.00000000000000000, -33.80338159004296017, 16.23288003029484727 ) ) ;
#27152 = ORIENTED_EDGE ( 'NONE', *, *, #66151, .F. ) ;
#27153 = ORIENTED_EDGE ( 'NONE', *, *, #11069, .F. ) ;
#27154 = AXIS2_PLACEMENT_3D ( 'NONE', #67648, #61639, #10126 ) ;
#27155 = ORIENTED_EDGE ( 'NONE', *, *, #26321, .T. ) ;
#27156 = CARTESIAN_POINT ( 'NONE',  ( 10.00000000000000000, 33.80338159004307386, -16.23288003029461279 ) ) ;
#27157 = EDGE_CURVE ( 'NONE', #59771, #12130, #33231, .T. ) ;
#27158 = ORIENTED_EDGE ( 'NONE', *, *, #22611, .F. ) ;
#27159 = PRODUCT ( 'big gear_ISO - Spur gear 2M 80T 20PA 10FW ---S80A75H50L20.0N', 'big gear_ISO - Spur gear 2M 80T 20PA 10FW ---S80A75H50L20.0N', '', ( #12850 ) ) ;
#27160 = EDGE_CURVE ( 'NONE', #33095, #16927, #1646, .T. ) ;
#27161 = AXIS2_PLACEMENT_3D ( 'NONE', #53854, #37685, #25292 ) ;
#27162 = AXIS2_PLACEMENT_3D ( 'NONE', #821, #35713, #24094 ) ;
#27163 = ORIENTED_EDGE ( 'NONE', *, *, #37337, .F. ) ;
#27164 = CARTESIAN_POINT ( 'NONE',  ( 93.84685191531248449, 88.00268892867053694, 77.84239583420048803 ) ) ;
#27165 = DIRECTION ( 'NONE',  ( 0.000000000000000000, 0.000000000000000000, 1.000000000000000000 ) ) ;
#27166 = CARTESIAN_POINT ( 'NONE',  ( -3.000000000000000000, -14.54903810567676636, 22.19967320028755964 ) ) ;
#27167 = VERTEX_POINT ( 'NONE', #71118 ) ;
#27168 = ORIENTED_EDGE ( 'NONE', *, *, #73476, .F. ) ;
#27169 = VERTEX_POINT ( 'NONE', #53477 ) ;
#27170 = CARTESIAN_POINT ( 'NONE',  ( 93.84685191531248449, 91.99731107132950569, 88.90197916753380980 ) ) ;
#27171 = ORIENTED_EDGE ( 'NONE', *, *, #65347, .T. ) ;
#27172 = CARTESIAN_POINT ( 'NONE',  ( 93.84685191531249870, -208.0026889286704943, 86.36197916753381776 ) ) ;
#27173 = DIRECTION ( 'NONE',  ( -5.551115123125782702E-17, 0.000000000000000000, -1.000000000000000000 ) ) ;
#27174 = CYLINDRICAL_SURFACE ( 'NONE', #19914, 2.649999999999999467 ) ;
#27175 = AXIS2_PLACEMENT_3D ( 'NONE', #8588, #43187, #31502 ) ;
#27176 = DIRECTION ( 'NONE',  ( -1.000000000000000000, 0.000000000000000000, 0.000000000000000000 ) ) ;
#27177 = DIRECTION ( 'NONE',  ( 0.000000000000000000, -0.6494480483301903195, 0.7604059656000251577 ) ) ;
#27178 = DIRECTION ( 'NONE',  ( 0.000000000000000000, 0.000000000000000000, 1.000000000000000000 ) ) ;
#27179 = DIRECTION ( 'NONE',  ( -0.000000000000000000, -0.000000000000000000, 1.000000000000000000 ) ) ;
#27180 = DIRECTION ( 'NONE',  ( -1.000000000000000000, 0.000000000000000000, 0.000000000000000000 ) ) ;
#27181 = CARTESIAN_POINT ( 'NONE',  ( -92.69370383062498320, -208.6684592857803011, 89.37822916753381719 ) ) ;
#27182 = CARTESIAN_POINT ( 'NONE',  ( -93.84685191531252713, 88.00268892867056536, 84.93322916753382401 ) ) ;
#27183 = EDGE_LOOP ( 'NONE', ( #14811, #44495, #16521, #7143 ) ) ;
#27185 = CARTESIAN_POINT ( 'NONE',  ( -92.69370383062502583, 91.33154071421968467, 86.83822916753381094 ) ) ;
#27184 = CARTESIAN_POINT ( 'NONE',  ( 94.99999999999998579, 92.66308142843935514, 88.21406250086714351 ) ) ;
#27186 = ORIENTED_EDGE ( 'NONE', *, *, #10059, .F. ) ;
#27187 = DIRECTION ( 'NONE',  ( -1.000000000000000000, -0.000000000000000000, -0.000000000000000000 ) ) ;
#27188 = CARTESIAN_POINT ( 'NONE',  ( 0.000000000000000000, 0.000000000000000000, 0.000000000000000000 ) ) ;
#27189 = CARTESIAN_POINT ( 'NONE',  ( -94.99999999999997158, -209.9999999999999716, 90.00000000000000000 ) ) ;
#27190 = CARTESIAN_POINT ( 'NONE',  ( 92.35000000039362078, 90.00002930319625705, 82.45844277051448046 ) ) ;
#27191 = CARTESIAN_POINT ( 'NONE',  ( -3.000000000000000000, -4.261787119645322974, 26.19803753235774835 ) ) ;
#27192 = LINE ( 'NONE', #62175, #53497 ) ;
#27193 = CARTESIAN_POINT ( 'NONE',  ( 92.35000000039362078, 90.00002930319625705, 82.45844277051448046 ) ) ;
#27194 = DIRECTION ( 'NONE',  ( -1.000000000000000000, 0.000000000000000000, -0.000000000000000000 ) ) ;
#27195 = ORIENTED_EDGE ( 'NONE', *, *, #18019, .F. ) ;
#27196 = ORIENTED_EDGE ( 'NONE', *, *, #7709, .T. ) ;
#27197 = CARTESIAN_POINT ( 'NONE',  ( -96.32500000000001705, 87.70503267997129626, 81.21583333333333599 ) ) ;
#27198 = CYLINDRICAL_SURFACE ( 'NONE', #5536, 77.49899999999999523 ) ;
#27199 = CARTESIAN_POINT ( 'NONE',  ( 0.000000000000000000, 81.90746397400387480, 3.894527615418187150 ) ) ;
#27200 = DIRECTION ( 'NONE',  ( -0.000000000000000000, -0.000000000000000000, -1.000000000000000000 ) ) ;
#27201 = FACE_BOUND ( 'NONE', #61304, .T. ) ;
#27202 = LINE ( 'NONE', #66713, #49548 ) ;
#27203 = ADVANCED_FACE ( 'NONE', ( #47468 ), #7613, .T. ) ;
#27204 = CARTESIAN_POINT ( 'NONE',  ( 10.00000000000000000, -71.21200624218766961, -40.65526001592689909 ) ) ;
#27205 = DIRECTION ( 'NONE',  ( 0.000000000000000000, 0.000000000000000000, 1.000000000000000000 ) ) ;
#27206 = AXIS2_PLACEMENT_3D ( 'NONE', #44331, #60880, #3383 ) ;
#27207 = ORIENTED_EDGE ( 'NONE', *, *, #32233, .T. ) ;
#27208 = CARTESIAN_POINT ( 'NONE',  ( -93.84685191531252713, 88.00268892867056536, 81.59947916753381492 ) ) ;
#27209 = EDGE_CURVE ( 'NONE', #16098, #64851, #70749, .T. ) ;
#27210 = MECHANICAL_DESIGN_GEOMETRIC_PRESENTATION_REPRESENTATION (  '', ( #65653 ), #70462 ) ;
#27211 = DIRECTION ( 'NONE',  ( 1.000000000000000000, -3.061616997868382648E-16, -0.000000000000000000 ) ) ;
#27212 = CARTESIAN_POINT ( 'NONE',  ( -100.0000000000260485, 95.00000000000001421, -65.00000000000001421 ) ) ;
#27213 = EDGE_CURVE ( 'NONE', #16746, #51113, #867, .T. ) ;
#27214 = CYLINDRICAL_SURFACE ( 'NONE', #29786, 77.49899999999999523 ) ;
#27215 = VECTOR ( 'NONE', #5779, 999.9999999999998863 ) ;
#27216 = FACE_OUTER_BOUND ( 'NONE', #16975, .T. ) ;
#27217 = CARTESIAN_POINT ( 'NONE',  ( 10.00000000000000000, 33.80338159004283938, 16.23288003029508886 ) ) ;
#27218 = CARTESIAN_POINT ( 'NONE',  ( -97.30629616937497417, -208.6684592857803011, 88.47864583420047779 ) ) ;
#27219 = AXIS2_PLACEMENT_3D ( 'NONE', #70449, #7688, #41531 ) ;
#27220 = EDGE_CURVE ( 'NONE', #48336, #13922, #19622, .T. ) ;
#27221 = LINE ( 'NONE', #3962, #16048 ) ;
#27222 = CIRCLE ( 'NONE', #69261, 16.00000000000000000 ) ;
#27223 = CARTESIAN_POINT ( 'NONE',  ( 92.69370383062498320, 91.33154071421968467, 78.95364583420045790 ) ) ;
#27224 = CARTESIAN_POINT ( 'NONE',  ( -97.30629616937497417, -208.6684592857803295, 84.03364583420049883 ) ) ;
#27225 = PLANE ( 'NONE',  #31370 ) ;
#27226 = ORIENTED_EDGE ( 'NONE', *, *, #22959, .T. ) ;
#27227 = EDGE_CURVE ( 'NONE', #3283, #10069, #9825, .T. ) ;
#27228 = DIRECTION ( 'NONE',  ( 0.000000000000000000, 0.000000000000000000, 1.000000000000000000 ) ) ;
#27229 = CARTESIAN_POINT ( 'NONE',  ( -97.64999999999996305, -209.9999999999999716, 76.66499999999999204 ) ) ;
#27230 = CARTESIAN_POINT ( 'NONE',  ( 97.64999999999999147, -209.9999999999999716, 78.25249999999999773 ) ) ;
#27231 = AXIS2_PLACEMENT_3D ( 'NONE', #42347, #48344, #13393 ) ;
#27232 = CARTESIAN_POINT ( 'NONE',  ( -92.69370383062504004, 90.00000000000004263, 79.95906250086714806 ) ) ;
#27233 = CARTESIAN_POINT ( 'NONE',  ( 92.69370383062501162, -209.9999999999999716, 82.02281250086714692 ) ) ;
#27234 = EDGE_LOOP ( 'NONE', ( #44027, #24499, #35475, #35858 ) ) ;
#27235 = AXIS2_PLACEMENT_3D ( 'NONE', #3524, #13749, #16256 ) ;
#27236 = CARTESIAN_POINT ( 'NONE',  ( 6.000000000000001776, 0.000000000000000000, 0.000000000000000000 ) ) ;
#27237 = EDGE_CURVE ( 'NONE', #46924, #48813, #9453, .T. ) ;
#27238 = ORIENTED_EDGE ( 'NONE', *, *, #17510, .T. ) ;
#27239 = DIRECTION ( 'NONE',  ( -0.9827303690289279636, -0.1850432970638682117, 0.000000000000000000 ) ) ;
#27240 = EDGE_CURVE ( 'NONE', #61698, #27755, #62119, .T. ) ;
#27241 = VERTEX_POINT ( 'NONE', #10563 ) ;
#27242 = DIRECTION ( 'NONE',  ( 0.000000000000000000, 0.000000000000000000, -1.000000000000000000 ) ) ;
#27243 = ADVANCED_FACE ( 'NONE', ( #72230 ), #18901, .T. ) ;
#27244 = ADVANCED_FACE ( 'NONE', ( #50415 ), #44796, .F. ) ;
#27245 = ORIENTED_EDGE ( 'NONE', *, *, #4042, .F. ) ;
#27246 = ORIENTED_EDGE ( 'NONE', *, *, #39501, .T. ) ;
#27247 = ORIENTED_EDGE ( 'NONE', *, *, #45196, .F. ) ;
#27248 = DIRECTION ( 'NONE',  ( -0.000000000000000000, -0.000000000000000000, 1.000000000000000000 ) ) ;
#27249 = EDGE_CURVE ( 'NONE', #61202, #44676, #44423, .T. ) ;
#27250 = VERTEX_POINT ( 'NONE', #55694 ) ;
#27251 = DIRECTION ( 'NONE',  ( 0.000000000000000000, -0.6494480483301738882, -0.7604059656000392575 ) ) ;
#27252 = CARTESIAN_POINT ( 'NONE',  ( 0.000000000000000000, 59.03961581697399907, 46.53671651293969802 ) ) ;
#27253 =( BOUNDED_CURVE ( )  B_SPLINE_CURVE ( 2, ( #43033, #49022, #2838, #31731, #48666, #54676, #65975, #71953, #43421 ),
 .UNSPECIFIED., .F., .F. ) 
 B_SPLINE_CURVE_WITH_KNOTS ( ( 3, 2, 2, 2, 3 ),
 ( 0.7196881748034551496, 0.7267438507108833212, 0.7337996162517648191, 0.7408553817926464280, 0.7408554641864648627 ),
 .UNSPECIFIED. ) 
 CURVE ( )  GEOMETRIC_REPRESENTATION_ITEM ( )  RATIONAL_B_SPLINE_CURVE ( ( 0.9999965961303247663, 0.8660271057408972517, 1.000000000000000000, 0.8660254037844387076, 1.000000000000000000, 0.8660254037844387076, 1.000000000000000000, 0.9999984355094434507, 0.9999968710554256734 ) ) 
 REPRESENTATION_ITEM ( '' )  );
#27254 = CARTESIAN_POINT ( 'NONE',  ( 94.99999999999998579, 92.66308142843935514, 86.46781250086716852 ) ) ;
#27255 = AXIS2_PLACEMENT_3D ( 'NONE', #65422, #44714, #55975 ) ;
#27256 = DIRECTION ( 'NONE',  ( 0.000000000000000000, 0.000000000000000000, -1.000000000000000000 ) ) ;
#27257 = CARTESIAN_POINT ( 'NONE',  ( 93.67500000000001137, -212.2949673200287179, 76.77083333333332860 ) ) ;
#27258 = CIRCLE ( 'NONE', #36872, 37.49900000000000944 ) ;
#27259 = ORIENTED_EDGE ( 'NONE', *, *, #59238, .F. ) ;
#27260 = EDGE_CURVE ( 'NONE', #18206, #40286, #62087, .T. ) ;
#27261 = ORIENTED_EDGE ( 'NONE', *, *, #58930, .F. ) ;
#27262 = EDGE_LOOP ( 'NONE', ( #21409, #34678, #71917, #9674 ) ) ;
#27263 = VERTEX_POINT ( 'NONE', #4581 ) ;
#27264 = CARTESIAN_POINT ( 'NONE',  ( 1.560000000000000053, -0.8660254037844384856, -1.500000000000000000 ) ) ;
#27265 = VECTOR ( 'NONE', #41373, 1000.000000000000000 ) ;
#27266 = CARTESIAN_POINT ( 'NONE',  ( 0.000000000000000000, 80.28980883073781172, -16.65972982744850839 ) ) ;
#27267 = CIRCLE ( 'NONE', #12897, 77.49900000000000944 ) ;
#27268 = DIRECTION ( 'NONE',  ( 0.000000000000000000, 0.000000000000000000, 1.000000000000000000 ) ) ;
#27269 = CARTESIAN_POINT ( 'NONE',  ( -92.35000982493194499, -211.5299838857795862, 88.43895794268827615 ) ) ;
#27270 = CARTESIAN_POINT ( 'NONE',  ( 0.000000000000000000, -37.58145647212455032, 0.6853352020789044152 ) ) ;
#27271 = VERTEX_POINT ( 'NONE', #67344 ) ;
#27272 = CARTESIAN_POINT ( 'NONE',  ( -96.32499999999996021, -212.2949673200287179, 81.29520833506762756 ) ) ;
#27273 = ORIENTED_EDGE ( 'NONE', *, *, #5233, .F. ) ;
#27274 = DIRECTION ( 'NONE',  ( 1.000000000000000000, 0.000000000000000000, 0.000000000000000000 ) ) ;
#27275 = AXIS2_PLACEMENT_3D ( 'NONE', #5717, #73738, #28621 ) ;
#27276 = EDGE_LOOP ( 'NONE', ( #21535, #12002, #34405, #4863 ) ) ;
#27278 = CARTESIAN_POINT ( 'NONE',  ( -95.00000000000002842, 93.05995642670501411, 82.93562500173429441 ) ) ;
#27277 = CARTESIAN_POINT ( 'NONE',  ( 93.67499999999998295, 92.29496732002878900, 84.25854166840096582 ) ) ;
#27279 = ORIENTED_EDGE ( 'NONE', *, *, #13132, .F. ) ;
#27280 = CARTESIAN_POINT ( 'NONE',  ( 97.30629616937498838, 88.66845928578037217, 84.98614583420047097 ) ) ;
#27281 = DIRECTION ( 'NONE',  ( -1.000000000000000000, -0.000000000000000000, 0.000000000000000000 ) ) ;
#27282 = CARTESIAN_POINT ( 'NONE',  ( 11.99999999999999822, 0.000000000000000000, 0.000000000000000000 ) ) ;
#27283 = CARTESIAN_POINT ( 'NONE',  ( -10.00000000000000000, 0.000000000000000000, 0.000000000000000000 ) ) ;
#27284 = LINE ( 'NONE', #43507, #4240 ) ;
#27285 = CYLINDRICAL_SURFACE ( 'NONE', #56488, 31.99999999999998579 ) ;
#27286 = ORIENTED_EDGE ( 'NONE', *, *, #26387, .F. ) ;
#27287 = DIRECTION ( 'NONE',  ( 0.000000000000000000, 0.000000000000000000, 1.000000000000000000 ) ) ;
#27288 = CARTESIAN_POINT ( 'NONE',  ( 11.99999999999999822, 75.11764819372149304, -2.946379043146603482 ) ) ;
#27289 = CARTESIAN_POINT ( 'NONE',  ( 0.000000000000000000, 0.000000000000000000, 0.000000000000000000 ) ) ;
#27290 = ORIENTED_EDGE ( 'NONE', *, *, #31759, .T. ) ;
#27291 = COLOUR_RGB ( '', 0.31764706, 0.68627451, 0.89019608) ;
#27292 = VERTEX_POINT ( 'NONE', #27480 ) ;
#27293 = CIRCLE ( 'NONE', #52517, 31.99999999999998579 ) ;
#27294 = FACE_OUTER_BOUND ( 'NONE', #26801, .T. ) ;
#27295 = CARTESIAN_POINT ( 'NONE',  ( -97.65000000000001990, 90.00002373248484844, 79.91937418090955703 ) ) ;
#27296 = DIRECTION ( 'NONE',  ( -0.000000000000000000, -0.000000000000000000, -1.000000000000000000 ) ) ;
#27297 = CARTESIAN_POINT ( 'NONE',  ( -97.30629616937497417, -208.6684592857803011, 79.58864583420047722 ) ) ;
#27298 = ORIENTED_EDGE ( 'NONE', *, *, #32239, .F. ) ;
#27299 = DIRECTION ( 'NONE',  ( -1.000000000000000000, -0.000000000000000000, -0.000000000000000000 ) ) ;
#27300 = ORIENTED_EDGE ( 'NONE', *, *, #24460, .F. ) ;
#27301 = ADVANCED_FACE ( 'NONE', ( #50033 ), #55320, .T. ) ;
#27302 = DIRECTION ( 'NONE',  ( 0.9135454576426059736, -0.4067366430757887730, 0.000000000000000000 ) ) ;
#27303 = FACE_BOUND ( 'NONE', #3304, .T. ) ;
#27304 = EDGE_CURVE ( 'NONE', #67853, #15222, #10484, .T. ) ;
#27305 = DIRECTION ( 'NONE',  ( -1.000000000000000000, 0.000000000000000000, -0.000000000000000000 ) ) ;
#27306 = CARTESIAN_POINT ( 'NONE',  ( 92.69370383062498320, 91.33154071421968467, 77.52489583420046415 ) ) ;
#27307 = DIRECTION ( 'NONE',  ( -1.000000000000000000, 0.000000000000000000, 0.000000000000000000 ) ) ;
#27308 = DIRECTION ( 'NONE',  ( 0.000000000000000000, 1.000000000000000000, -9.787530781167596740E-16 ) ) ;
#27309 = CYLINDRICAL_SURFACE ( 'NONE', #21690, 2.649999999999985700 ) ;
#27310 = DIRECTION ( 'NONE',  ( -1.000000000000000000, 0.000000000000000000, 0.000000000000000000 ) ) ;
#27311 = EDGE_CURVE ( 'NONE', #1450, #11217, #45331, .T. ) ;
#27313 = EDGE_CURVE ( 'NONE', #50235, #14882, #47675, .T. ) ;
#27312 = LINE ( 'NONE', #55535, #65219 ) ;
#27314 = CARTESIAN_POINT ( 'NONE',  ( 0.000000000000000000, 55.38113227695858143, -54.21277698773617715 ) ) ;
#27315 = AXIS2_PLACEMENT_3D ( 'NONE', #37866, #21286, #43879 ) ;
#27316 = CARTESIAN_POINT ( 'NONE',  ( 97.64999999999999147, -209.9999999999999716, 83.33250000000001023 ) ) ;
#27317 = AXIS2_PLACEMENT_3D ( 'NONE', #38610, #66085, #2945 ) ;
#27318 = CARTESIAN_POINT ( 'NONE',  ( 3.000000000000000000, 2.935248768560057897, -3.252606517456513302E-15 ) ) ;
#27319 = DIRECTION ( 'NONE',  ( 0.000000000000000000, 0.000000000000000000, 1.000000000000000000 ) ) ;
#27320 = ORIENTED_EDGE ( 'NONE', *, *, #73652, .T. ) ;
#27321 = CARTESIAN_POINT ( 'NONE',  ( -97.30629616937501680, 90.00000000000004263, 83.92781250086714806 ) ) ;
#27322 = CARTESIAN_POINT ( 'NONE',  ( 11.99999999999999822, -31.47745569255092235, -68.26794271651296242 ) ) ;
#27323 = VECTOR ( 'NONE', #60881, 1000.000000000000114 ) ;
#27324 = EDGE_CURVE ( 'NONE', #70648, #18411, #16208, .T. ) ;
#27325 = AXIS2_PLACEMENT_3D ( 'NONE', #16984, #27508, #11329 ) ;
#27326 = EDGE_CURVE ( 'NONE', #68748, #4061, #43688, .T. ) ;
#27327 = DIRECTION ( 'NONE',  ( -1.000000000000000000, 0.000000000000000000, 0.000000000000000000 ) ) ;
#27328 = ORIENTED_EDGE ( 'NONE', *, *, #54836, .T. ) ;
#27329 = FACE_OUTER_BOUND ( 'NONE', #4170, .T. ) ;
#27330 = CARTESIAN_POINT ( 'NONE',  ( 0.000000000000000000, 0.000000000000000000, 0.000000000000000000 ) ) ;
#27331 = FACE_OUTER_BOUND ( 'NONE', #2900, .T. ) ;
#27332 = DIRECTION ( 'NONE',  ( -1.000000000000000000, -0.000000000000000000, -0.000000000000000000 ) ) ;
#27333 = EDGE_CURVE ( 'NONE', #48627, #2059, #33276, .T. ) ;
#27334 = EDGE_CURVE ( 'NONE', #26778, #61936, #6894, .T. ) ;
#27335 = CARTESIAN_POINT ( 'NONE',  ( 95.00000000000000000, -207.3369185715606307, 80.11781250086714579 ) ) ;
#27336 = VECTOR ( 'NONE', #14502, 1000.000000000000000 ) ;
#27337 = AXIS2_PLACEMENT_3D ( 'NONE', #54930, #27756, #50303 ) ;
#27338 = EDGE_LOOP ( 'NONE', ( #60924, #2809 ) ) ;
#27339 = ORIENTED_EDGE ( 'NONE', *, *, #44564, .F. ) ;
#27340 = CIRCLE ( 'NONE', #69383, 77.49900000000002365 ) ;
#27341 = VECTOR ( 'NONE', #4975, 1000.000000000000000 ) ;
#27342 = LINE ( 'NONE', #21324, #42878 ) ;
#27343 = DIRECTION ( 'NONE',  ( 0.000000000000000000, -0.8090169943749403458, -0.5877852522924830181 ) ) ;
#27344 = AXIS2_PLACEMENT_3D ( 'NONE', #18456, #70316, #849 ) ;
#27345 = DIRECTION ( 'NONE',  ( -1.000000000000000000, 7.955419762439749020E-15, 2.563413034563919251E-14 ) ) ;
#27346 = CARTESIAN_POINT ( 'NONE',  ( 10.00000000000000000, 0.000000000000000000, 0.000000000000000000 ) ) ;
#27347 = LINE ( 'NONE', #16830, #40501 ) ;
#27348 = CARTESIAN_POINT ( 'NONE',  ( 93.67500000000001137, -212.2949673200287179, 86.93083333333332519 ) ) ;
#27349 = ORIENTED_EDGE ( 'NONE', *, *, #68828, .F. ) ;
#27350 = CARTESIAN_POINT ( 'NONE',  ( 0.000000000000000000, -30.00120703465189465, -22.64427369931201639 ) ) ;
#27351 = ORIENTED_EDGE ( 'NONE', *, *, #71864, .T. ) ;
#27352 = ORIENTED_EDGE ( 'NONE', *, *, #15714, .F. ) ;
#27353 = CARTESIAN_POINT ( 'NONE',  ( 12.00000000000000000, 14.60985201121703980, -18.46759930825707841 ) ) ;
#27354 = CARTESIAN_POINT ( 'NONE',  ( 0.000000000000000000, 6.736453364083555329, 36.88895765772635116 ) ) ;
#27355 = ORIENTED_EDGE ( 'NONE', *, *, #16228, .F. ) ;
#27356 = CARTESIAN_POINT ( 'NONE',  ( 4.755015822784811164, -4.336808689942017736E-16, 0.000000000000000000 ) ) ;
#27357 = CARTESIAN_POINT ( 'NONE',  ( 92.35000000000002274, -208.4700217866474645, 78.59645833506763779 ) ) ;
#27358 = CARTESIAN_POINT ( 'NONE',  ( 92.34999999999999432, 91.52997821335252127, 82.96208333333333940 ) ) ;
#27359 = ORIENTED_EDGE ( 'NONE', *, *, #57148, .T. ) ;
#27360 = DIRECTION ( 'NONE',  ( 0.000000000000000000, 0.000000000000000000, 1.000000000000000000 ) ) ;
#27361 = ORIENTED_EDGE ( 'NONE', *, *, #34225, .T. ) ;
#27362 = CARTESIAN_POINT ( 'NONE',  ( 97.65000000000000568, 91.52997821335252127, 80.92479166840097093 ) ) ;
#27363 = ORIENTED_EDGE ( 'NONE', *, *, #52567, .T. ) ;
#27364 = DIRECTION ( 'NONE',  ( -1.000000000000000000, -0.000000000000000000, 0.000000000000000000 ) ) ;
#27365 = CARTESIAN_POINT ( 'NONE',  ( -92.69370383062505425, 91.33154071421968467, 84.45697916753383083 ) ) ;
#27366 = AXIS2_PLACEMENT_3D ( 'NONE', #69533, #34954, #28939 ) ;
#27367 = CARTESIAN_POINT ( 'NONE',  ( 92.69370383062498320, 90.00000000000002842, 77.57781250086713953 ) ) ;
#27368 = ORIENTED_EDGE ( 'NONE', *, *, #55071, .T. ) ;
#27369 = LINE ( 'NONE', #40155, #54984 ) ;
#27370 = VECTOR ( 'NONE', #25014, 1000.000000000000000 ) ;
#27371 = CYLINDRICAL_SURFACE ( 'NONE', #38899, 2.649999999999985700 ) ;
#27372 = DIRECTION ( 'NONE',  ( 0.000000000000000000, 0.4539904997395412534, 0.8910065241883706744 ) ) ;
#27373 = CARTESIAN_POINT ( 'NONE',  ( 3.000000000000000000, 0.000000000000000000, 0.000000000000000000 ) ) ;
#27374 = ORIENTED_EDGE ( 'NONE', *, *, #11806, .F. ) ;
#27375 = CARTESIAN_POINT ( 'NONE',  ( 15.00000000000000000, -14.54903810567644484, 22.19967320028775504 ) ) ;
#27376 = CARTESIAN_POINT ( 'NONE',  ( -96.15314808468747287, -208.0026889286704943, 81.28197916753380525 ) ) ;
#27377 = ORIENTED_EDGE ( 'NONE', *, *, #16476, .T. ) ;
#27378 = CIRCLE ( 'NONE', #14179, 42.00000000000000000 ) ;
#27379 = ORIENTED_EDGE ( 'NONE', *, *, #73856, .T. ) ;
#27380 = DIRECTION ( 'NONE',  ( 0.000000000000000000, 0.000000000000000000, -1.000000000000000000 ) ) ;
#27381 = VERTEX_POINT ( 'NONE', #49666 ) ;
#27382 = CARTESIAN_POINT ( 'NONE',  ( 0.000000000000000000, -44.88180994100421373, 63.18004540533011948 ) ) ;
#27383 = CARTESIAN_POINT ( 'NONE',  ( 92.34999999999999432, 88.47002178664753558, 88.86229166840097093 ) ) ;
#27384 = ORIENTED_EDGE ( 'NONE', *, *, #61277, .T. ) ;
#27385 = CARTESIAN_POINT ( 'NONE',  ( -93.84685191531247028, -211.9973110713294489, 77.15447916753380753 ) ) ;
#27386 = ORIENTED_EDGE ( 'NONE', *, *, #70430, .T. ) ;
#27387 = CARTESIAN_POINT ( 'NONE',  ( 11.99999999999999822, -20.41045688087876897, 72.35160999960810102 ) ) ;
#27388 = DIRECTION ( 'NONE',  ( -1.000000000000000000, 0.000000000000000000, 0.000000000000000000 ) ) ;
#27389 = DIRECTION ( 'NONE',  ( -0.000000000000000000, -0.000000000000000000, 1.000000000000000000 ) ) ;
#27390 = DIRECTION ( 'NONE',  ( 0.000000000000000000, 0.6691306063588670083, 0.7431448254773863615 ) ) ;
#27391 = EDGE_CURVE ( 'NONE', #18937, #11372, #65718, .T. ) ;
#27392 = ADVANCED_FACE ( 'NONE', ( #44049 ), #32009, .T. ) ;
#27393 = CARTESIAN_POINT ( 'NONE',  ( -92.35000000000000853, 88.47002178664759242, 81.37458333333333371 ) ) ;
#27394 = CIRCLE ( 'NONE', #45464, 3.000000000000000000 ) ;
#27395 = ADVANCED_FACE ( 'NONE', ( #39525 ), #5692, .T. ) ;
#27396 = LINE ( 'NONE', #26659, #51718 ) ;
#27398 = CIRCLE ( 'NONE', #33404, 16.00000000000000000 ) ;
#27397 = CARTESIAN_POINT ( 'NONE',  ( 93.84685191531248449, 88.00268892867053694, 88.47864583420047779 ) ) ;
#27399 = DIRECTION ( 'NONE',  ( 1.000000000000000000, 0.000000000000000000, 0.000000000000000000 ) ) ;
#27400 = CARTESIAN_POINT ( 'NONE',  ( -8.826826895187510402, -94.96827758698185562, 5.500000000000000000 ) ) ;
#27401 = FACE_OUTER_BOUND ( 'NONE', #17782, .T. ) ;
#27402 = AXIS2_PLACEMENT_3D ( 'NONE', #4635, #72641, #4260 ) ;
#27403 = CARTESIAN_POINT ( 'NONE',  ( -92.35000000000002274, 89.99999149135206267, 88.49187470744952577 ) ) ;
#27404 = VECTOR ( 'NONE', #56285, 1000.000000000000000 ) ;
#27406 = EDGE_CURVE ( 'NONE', #3895, #26473, #64529, .T. ) ;
#27405 = FACE_OUTER_BOUND ( 'NONE', #46259, .T. ) ;
#27407 = DIRECTION ( 'NONE',  ( 1.000000000000000000, 0.000000000000000000, 0.000000000000000000 ) ) ;
#27408 = FACE_OUTER_BOUND ( 'NONE', #59181, .T. ) ;
#27409 = LINE ( 'NONE', #50343, #1997 ) ;
#27410 = EDGE_CURVE ( 'NONE', #55837, #42834, #69651, .T. ) ;
#27411 = CARTESIAN_POINT ( 'NONE',  ( 0.000000000000000000, 65.64334221924966073, -41.19522573413664190 ) ) ;
#27412 = DIRECTION ( 'NONE',  ( -1.000000000000000000, 0.000000000000000000, 0.000000000000000000 ) ) ;
#27413 = FACE_OUTER_BOUND ( 'NONE', #44783, .T. ) ;
#27414 = DIRECTION ( 'NONE',  ( 0.000000000000000000, 0.8526401643540897357, 0.5224985647159531288 ) ) ;
#27415 = CARTESIAN_POINT ( 'NONE',  ( -92.34999999999999432, -209.9999999999999716, 85.87249999999998806 ) ) ;
#27416 = ADVANCED_FACE ( 'NONE', ( #28594 ), #16582, .T. ) ;
#27417 = FACE_OUTER_BOUND ( 'NONE', #11184, .T. ) ;
#27418 = EDGE_CURVE ( 'NONE', #34394, #53435, #50785, .T. ) ;
#27419 = CIRCLE ( 'NONE', #12986, 16.00000000000000000 ) ;
#27420 = CARTESIAN_POINT ( 'NONE',  ( 11.99999999999999822, -72.35160999960801576, -20.41045688087902121 ) ) ;
#27421 = CARTESIAN_POINT ( 'NONE',  ( 0.000000000000000000, -30.41916302227164337, 71.27951684758015460 ) ) ;
#27422 = DIRECTION ( 'NONE',  ( -1.000000000000000000, -0.000000000000000000, -0.000000000000000000 ) ) ;
#27423 = AXIS2_PLACEMENT_3D ( 'NONE', #45937, #68861, #17347 ) ;
#27424 = DIRECTION ( 'NONE',  ( 1.000000000000000000, 0.000000000000000000, -0.000000000000000000 ) ) ;
#27425 = EDGE_CURVE ( 'NONE', #1988, #2136, #51156, .T. ) ;
#27426 = EDGE_CURVE ( 'NONE', #32014, #18969, #68124, .T. ) ;
#27427 = CARTESIAN_POINT ( 'NONE',  ( 93.84685191531251292, -211.9973110713294489, 89.27239583420049485 ) ) ;
#27428 = AXIS2_PLACEMENT_3D ( 'NONE', #10959, #51916, #63955 ) ;
#27429 = AXIS2_PLACEMENT_3D ( 'NONE', #12082, #35021, #6812 ) ;
#27430 = ORIENTED_EDGE ( 'NONE', *, *, #72816, .F. ) ;
#27431 = VERTEX_POINT ( 'NONE', #34243 ) ;
#27432 = CARTESIAN_POINT ( 'NONE',  ( 0.000000000000000000, 49.70050353004889132, 59.46389618801982380 ) ) ;
#27433 = VERTEX_POINT ( 'NONE', #68840 ) ;
#27434 = CARTESIAN_POINT ( 'NONE',  ( 0.000000000000000000, 0.000000000000000000, -4.400000000000001243 ) ) ;
#27435 = CARTESIAN_POINT ( 'NONE',  ( 97.30629616937498838, -209.9999999999999716, 78.53031250086714010 ) ) ;
#27436 = ORIENTED_EDGE ( 'NONE', *, *, #44507, .T. ) ;
#27437 = CARTESIAN_POINT ( 'NONE',  ( 92.69370383062501162, -208.6684592857803011, 87.20864583420049598 ) ) ;
#27438 = VECTOR ( 'NONE', #53881, 1000.000000000000000 ) ;
#27439 = ORIENTED_EDGE ( 'NONE', *, *, #12589, .F. ) ;
#27440 = LINE ( 'NONE', #9791, #64658 ) ;
#27441 = EDGE_LOOP ( 'NONE', ( #65547, #9064, #51471, #19870 ) ) ;
#27442 = LINE ( 'NONE', #50377, #4537 ) ;
#27443 = AXIS2_PLACEMENT_3D ( 'NONE', #11282, #33845, #51134 ) ;
#27444 = EDGE_LOOP ( 'NONE', ( #42949, #61254, #60660, #31066 ) ) ;
#27445 = CARTESIAN_POINT ( 'NONE',  ( 119.3426274441929280, -132.5434155921172419, -5.500000000000000000 ) ) ;
#27446 = ORIENTED_EDGE ( 'NONE', *, *, #27984, .F. ) ;
#27447 = DIRECTION ( 'NONE',  ( -1.000000000000000000, 0.000000000000000000, -0.000000000000000000 ) ) ;
#27448 = DIRECTION ( 'NONE',  ( 0.000000000000000000, 0.000000000000000000, -1.000000000000000000 ) ) ;
#27449 = AXIS2_PLACEMENT_3D ( 'NONE', #67369, #9116, #26765 ) ;
#27450 = EDGE_LOOP ( 'NONE', ( #65464, #67125, #55278, #53565 ) ) ;
#27451 = FACE_OUTER_BOUND ( 'NONE', #45457, .T. ) ;
#27452 = ORIENTED_EDGE ( 'NONE', *, *, #1973, .F. ) ;
#27453 = AXIS2_PLACEMENT_3D ( 'NONE', #17456, #73848, #62982 ) ;
#27454 = LINE ( 'NONE', #9805, #19194 ) ;
#27455 = EDGE_LOOP ( 'NONE', ( #71185, #52376, #46497, #47253 ) ) ;
#27456 = VERTEX_POINT ( 'NONE', #46640 ) ;
#27457 = VERTEX_POINT ( 'NONE', #91 ) ;
#27458 = CARTESIAN_POINT ( 'NONE',  ( -5.000000000000000000, -2.886751345948137981, -5.553418012614792509 ) ) ;
#27459 = CARTESIAN_POINT ( 'NONE',  ( 11.99999999999999822, 14.66109333815460225, 73.73191006444577056 ) ) ;
#27460 = ORIENTED_EDGE ( 'NONE', *, *, #59773, .F. ) ;
#27461 = VERTEX_POINT ( 'NONE', #63573 ) ;
#27463 = EDGE_CURVE ( 'NONE', #33591, #28018, #56820, .T. ) ;
#27462 = ORIENTED_EDGE ( 'NONE', *, *, #40178, .F. ) ;
#27464 = CYLINDRICAL_SURFACE ( 'NONE', #9644, 2.649999999999985700 ) ;
#27465 = CARTESIAN_POINT ( 'NONE',  ( 10.00000000000000000, 46.21855187248629449, 62.20884554314036308 ) ) ;
#27466 = EDGE_CURVE ( 'NONE', #4529, #30100, #11669, .T. ) ;
#27468 = CARTESIAN_POINT ( 'NONE',  ( -93.84685191531254134, 91.99731107132950569, 76.25489583420049655 ) ) ;
#27467 = VECTOR ( 'NONE', #31266, 1000.000000000000000 ) ;
#27469 = EDGE_LOOP ( 'NONE', ( #23035, #69582, #34581, #19946 ) ) ;
#27470 = CARTESIAN_POINT ( 'NONE',  ( 92.69370383062498320, 88.66845928578037217, 76.99572916753380980 ) ) ;
#27471 = EDGE_CURVE ( 'NONE', #55116, #13677, #45549, .T. ) ;
#27472 =( BOUNDED_CURVE ( )  B_SPLINE_CURVE ( 2, ( #70778, #19281, #42235, #65165, #4607, #3866, #61368 ),
 .UNSPECIFIED., .F., .F. ) 
 B_SPLINE_CURVE_WITH_KNOTS ( ( 3, 2, 2, 3 ),
 ( 0.6773535682785479795, 0.6844092574689497610, 0.6914650230098673411, 0.6985206468877303010 ),
 .UNSPECIFIED. ) 
 CURVE ( )  GEOMETRIC_REPRESENTATION_ITEM ( )  RATIONAL_B_SPLINE_CURVE ( ( 0.9999971005502381605, 0.8660268535250073008, 1.000000000000000000, 0.8660254037844387076, 1.000000000000000000, 0.8660280936769018112, 0.9999946203230871689 ) ) 
 REPRESENTATION_ITEM ( '' )  );
#27473 = ORIENTED_EDGE ( 'NONE', *, *, #29887, .F. ) ;
#27474 = DIRECTION ( 'NONE',  ( -0.000000000000000000, -0.000000000000000000, 1.000000000000000000 ) ) ;
#27475 = CARTESIAN_POINT ( 'NONE',  ( 10.00000000000000000, 0.000000000000000000, 0.000000000000000000 ) ) ;
#27476 = ORIENTED_EDGE ( 'NONE', *, *, #66313, .F. ) ;
#27477 = CIRCLE ( 'NONE', #28654, 82.00000000000000000 ) ;
#27478 = CARTESIAN_POINT ( 'NONE',  ( 3.675296855064185575, -3.651569063273171434, -0.8655517945778166133 ) ) ;
#27479 = CARTESIAN_POINT ( 'NONE',  ( 0.000000000000000000, 0.000000000000000000, 0.000000000000000000 ) ) ;
#27480 = CARTESIAN_POINT ( 'NONE',  ( 0.000000000000000000, -40.65526001592564853, -71.21200624218839437 ) ) ;
#27481 = CARTESIAN_POINT ( 'NONE',  ( -94.99999999999997158, -207.3369185715606307, 78.68906250086713783 ) ) ;
#27482 = VECTOR ( 'NONE', #31696, 1000.000000000000000 ) ;
#27483 = AXIS2_PLACEMENT_3D ( 'NONE', #16149, #26307, #4901 ) ;
#27484 = EDGE_CURVE ( 'NONE', #51707, #39053, #5328, .T. ) ;
#27485 = DIRECTION ( 'NONE',  ( -1.000000000000000000, 0.000000000000000000, 0.000000000000000000 ) ) ;
#27486 = CARTESIAN_POINT ( 'NONE',  ( 5.999999999999999112, -79.10210256391353312, -21.60688246758669351 ) ) ;
#27487 = CARTESIAN_POINT ( 'NONE',  ( -96.32499999999996021, -212.2949673200287179, 79.31083333333333485 ) ) ;
#27488 = VERTEX_POINT ( 'NONE', #818 ) ;
#27489 = VECTOR ( 'NONE', #64594, 1000.000000000000000 ) ;
#27491 = ORIENTED_EDGE ( 'NONE', *, *, #19082, .T. ) ;
#27490 = EDGE_CURVE ( 'NONE', #45343, #423, #41754, .T. ) ;
#27492 = CARTESIAN_POINT ( 'NONE',  ( -10.00000000000000000, 0.000000000000000000, 0.000000000000000000 ) ) ;
#27493 = AXIS2_PLACEMENT_3D ( 'NONE', #23287, #46217, #759 ) ;
#27494 = DIRECTION ( 'NONE',  ( -1.000000000000000000, 0.000000000000000000, -0.000000000000000000 ) ) ;
#27495 = PLANE ( 'NONE',  #6739 ) ;
#27496 = CARTESIAN_POINT ( 'NONE',  ( -92.69370383062502583, 88.66845928578038638, 80.38239583420049428 ) ) ;
#27497 = CARTESIAN_POINT ( 'NONE',  ( 0.000000000000000000, 0.000000000000000000, 0.000000000000000000 ) ) ;
#27498 = CARTESIAN_POINT ( 'NONE',  ( 0.000000000000000000, 2.956366410620650420, 75.11725578898469280 ) ) ;
#27499 = EDGE_CURVE ( 'NONE', #17107, #24230, #6068, .T. ) ;
#27500 = ORIENTED_EDGE ( 'NONE', *, *, #67826, .T. ) ;
#27501 = LINE ( 'NONE', #72978, #36571 ) ;
#27502 = CIRCLE ( 'NONE', #37125, 26.50000000000000355 ) ;
#27503 = VECTOR ( 'NONE', #18419, 1000.000000000000000 ) ;
#27504 = CARTESIAN_POINT ( 'NONE',  ( 10.00000000000000000, -50.95692526931372157, 58.39081064771733054 ) ) ;
#27505 = CARTESIAN_POINT ( 'NONE',  ( 5.000000000000002665, -81.34940948281344220, 10.30890764327356557 ) ) ;
#27506 = CIRCLE ( 'NONE', #56346, 16.00000000000000000 ) ;
#27507 = DIRECTION ( 'NONE',  ( 0.000000000000000000, 0.000000000000000000, 1.000000000000000000 ) ) ;
#27508 = DIRECTION ( 'NONE',  ( -1.000000000000000000, 0.000000000000000000, 0.000000000000000000 ) ) ;
#27509 = CARTESIAN_POINT ( 'NONE',  ( 95.00000000000000000, -206.9400435732949575, 88.65062500173428361 ) ) ;
#27510 = CARTESIAN_POINT ( 'NONE',  ( -96.15314808468745866, -211.9973110713294489, 79.11239583420048405 ) ) ;
#27511 = AXIS2_PLACEMENT_3D ( 'NONE', #27350, #38653, #15330 ) ;
#27512 = EDGE_CURVE ( 'NONE', #25600, #54039, #53686, .T. ) ;
#27513 = DIRECTION ( 'NONE',  ( 0.000000000000000000, 0.000000000000000000, 1.000000000000000000 ) ) ;
#27514 = ADVANCED_FACE ( 'NONE', ( #16962 ), #39899, .T. ) ;
#27515 = AXIS2_PLACEMENT_3D ( 'NONE', #6640, #46490, #57781 ) ;
#27516 = ORIENTED_EDGE ( 'NONE', *, *, #24273, .T. ) ;
#27517 = DIRECTION ( 'NONE',  ( 1.000000000000000000, 0.000000000000000000, 0.000000000000000000 ) ) ;
#27518 = CARTESIAN_POINT ( 'NONE',  ( 11.99999999999999822, 77.19088730480524418, 6.903761155838049390 ) ) ;
#27519 = CARTESIAN_POINT ( 'NONE',  ( 11.99999999999999822, 8.966570791701867549, -81.50828551894218776 ) ) ;
#27520 = ORIENTED_EDGE ( 'NONE', *, *, #52982, .T. ) ;
#27521 = DIRECTION ( 'NONE',  ( 0.000000000000000000, 0.4067366430758000417, -0.9135454576426009776 ) ) ;
#27522 = CARTESIAN_POINT ( 'NONE',  ( 0.000000000000000000, -73.72996012237429397, -14.67089635893794508 ) ) ;
#27523 = CARTESIAN_POINT ( 'NONE',  ( 4.999999999999999112, -41.81611651403859042, -3.925862922256606602 ) ) ;
#27524 = ORIENTED_EDGE ( 'NONE', *, *, #67022, .T. ) ;
#27525 = CARTESIAN_POINT ( 'NONE',  ( 94.99999999999998579, 93.05995642670504253, 78.41125000000000966 ) ) ;
#27526 = CARTESIAN_POINT ( 'NONE',  ( -12.74999999999990941, -119.9999999999999005, -70.59999999999966747 ) ) ;
#27527 = VERTEX_POINT ( 'NONE', #47383 ) ;
#27528 = CIRCLE ( 'NONE', #13091, 82.00000000000000000 ) ;
#27529 = CARTESIAN_POINT ( 'NONE',  ( 97.30629616937498838, -211.3315407142195852, 88.63739583420047552 ) ) ;
#27530 = CARTESIAN_POINT ( 'NONE',  ( 0.000000000000000000, -68.67312586195022561, 35.91791733033449674 ) ) ;
#27531 = ORIENTED_EDGE ( 'NONE', *, *, #38464, .T. ) ;
#27532 = CIRCLE ( 'NONE', #32305, 31.99999999999998224 ) ;
#27533 = DIRECTION ( 'NONE',  ( 0.7273375899149802093, -0.6862798483830544471, 0.000000000000000000 ) ) ;
#27534 = CIRCLE ( 'NONE', #21516, 31.99999999999999645 ) ;
#27535 = ORIENTED_EDGE ( 'NONE', *, *, #5362, .T. ) ;
#27536 = CARTESIAN_POINT ( 'NONE',  ( 22.75000000000000000, 0.000000000000000000, 2.055000000000000160 ) ) ;
#27537 = VERTEX_POINT ( 'NONE', #1196 ) ;
#27538 = DIRECTION ( 'NONE',  ( 0.000000000000000000, 0.000000000000000000, 1.000000000000000000 ) ) ;
#27539 = VERTEX_POINT ( 'NONE', #42849 ) ;
#27540 = ORIENTED_EDGE ( 'NONE', *, *, #69841, .F. ) ;
#27541 = CIRCLE ( 'NONE', #6007, 31.99999999999998224 ) ;
#27542 = ORIENTED_EDGE ( 'NONE', *, *, #30735, .T. ) ;
#27543 = DIRECTION ( 'NONE',  ( -1.000000000000000000, 0.000000000000000000, 0.000000000000000000 ) ) ;
#27544 = EDGE_CURVE ( 'NONE', #2465, #57048, #8260, .T. ) ;
#27545 = EDGE_LOOP ( 'NONE', ( #3149, #10353, #8491, #55655 ) ) ;
#27546 = VERTEX_POINT ( 'NONE', #48485 ) ;
#27547 = CARTESIAN_POINT ( 'NONE',  ( 97.30629616937498838, 90.00000000000002842, 77.41906250086715602 ) ) ;
#27548 = CARTESIAN_POINT ( 'NONE',  ( 1.433254160131044044E-14, 1.918465386552270249E-13, 18.00000000000031974 ) ) ;
#27549 = LINE ( 'NONE', #38471, #17702 ) ;
#27550 = ORIENTED_EDGE ( 'NONE', *, *, #24875, .F. ) ;
#27552 = ORIENTED_EDGE ( 'NONE', *, *, #51865, .T. ) ;
#27551 = VECTOR ( 'NONE', #32654, 1000.000000000000000 ) ;
#27553 = ORIENTED_EDGE ( 'NONE', *, *, #28207, .T. ) ;
#27554 = CARTESIAN_POINT ( 'NONE',  ( 92.69370383062498320, 90.00000000000002842, 87.73781250086713612 ) ) ;
#27555 = ORIENTED_EDGE ( 'NONE', *, *, #13428, .F. ) ;
#27556 = CARTESIAN_POINT ( 'NONE',  ( 95.00000000000000000, -212.6630814284392557, 85.99156250086714692 ) ) ;
#27557 = AXIS2_PLACEMENT_3D ( 'NONE', #25355, #49009, #59951 ) ;
#27558 = VECTOR ( 'NONE', #8456, 1000.000000000000227 ) ;
#27559 = PRODUCT_CONTEXT ( 'NONE', #26763, 'mechanical' ) ;
#27560 = CARTESIAN_POINT ( 'NONE',  ( 0.000000000000000000, 0.000000000000000000, 0.000000000000000000 ) ) ;
#27561 = CARTESIAN_POINT ( 'NONE',  ( 11.99999999999999822, -72.35432306680469594, -20.40083707022958848 ) ) ;
#27562 = DIRECTION ( 'NONE',  ( -1.000000000000000000, -0.000000000000000000, -0.000000000000000000 ) ) ;
#27563 = FACE_OUTER_BOUND ( 'NONE', #63542, .T. ) ;
#27564 = ADVANCED_FACE ( 'NONE', ( #71034 ), #13156, .T. ) ;
#27565 = FACE_OUTER_BOUND ( 'NONE', #55308, .T. ) ;
#27566 = CIRCLE ( 'NONE', #9541, 3.300000000000000711 ) ;
#27567 = CARTESIAN_POINT ( 'NONE',  ( 92.35000000049316782, -210.0000320386632495, 83.73041644179299681 ) ) ;
#27568 = AXIS2_PLACEMENT_3D ( 'NONE', #50640, #57041, #56298 ) ;
#27569 = CARTESIAN_POINT ( 'NONE',  ( -94.99999999999997158, -207.3369185715606307, 86.94406250086714749 ) ) ;
#27570 = EDGE_CURVE ( 'NONE', #32656, #20380, #71400, .T. ) ;
#27571 = CARTESIAN_POINT ( 'NONE',  ( -96.15314808468752972, 91.99731107132950569, 85.88572916753381037 ) ) ;
#27572 = EDGE_LOOP ( 'NONE', ( #14308, #19409, #59065, #39154 ) ) ;
#27574 = CARTESIAN_POINT ( 'NONE',  ( -93.84685191531252713, 88.00268892867056536, 84.77447916753381207 ) ) ;
#27573 = CARTESIAN_POINT ( 'NONE',  ( 96.15314808468748708, 91.99731107132950569, 87.52614583420047722 ) ) ;
#27575 = VERTEX_POINT ( 'NONE', #35710 ) ;
#27576 = LINE ( 'NONE', #67053, #46705 ) ;
#27577 = CARTESIAN_POINT ( 'NONE',  ( -96.32499999999996021, -212.2949673200287179, 80.66020833506763665 ) ) ;
#27578 = FACE_OUTER_BOUND ( 'NONE', #66233, .T. ) ;
#27579 = CYLINDRICAL_SURFACE ( 'NONE', #2422, 2.649999999999985700 ) ;
#27580 = CARTESIAN_POINT ( 'NONE',  ( -94.99999999999997158, -207.3369185715606307, 89.48406250086713953 ) ) ;
#27581 = DIRECTION ( 'NONE',  ( 1.000000000000000000, 0.000000000000000000, 0.000000000000000000 ) ) ;
#27582 = EDGE_CURVE ( 'NONE', #32702, #70313, #51272, .T. ) ;
#27583 = EDGE_CURVE ( 'NONE', #70347, #20087, #60887, .T. ) ;
#27584 = CARTESIAN_POINT ( 'NONE',  ( 5.000000000000002665, 15.33399622253600292, -80.55351364060572905 ) ) ;
#27585 = CARTESIAN_POINT ( 'NONE',  ( 10.00000000000000000, -33.80338159004296017, 16.23288003029484727 ) ) ;
#27586 = PLANE ( 'NONE',  #32266 ) ;
#27587 = ORIENTED_EDGE ( 'NONE', *, *, #47187, .T. ) ;
#27588 = ORIENTED_EDGE ( 'NONE', *, *, #5627, .T. ) ;
#27589 = CARTESIAN_POINT ( 'NONE',  ( -96.32500000000001705, 92.29496732002878900, 81.00416666666666288 ) ) ;
#27590 = CARTESIAN_POINT ( 'NONE',  ( -95.00000000000002842, 90.00000000000004263, 90.00000000000000000 ) ) ;
#27591 = DIRECTION ( 'NONE',  ( -1.000000000000000000, 0.000000000000000000, 0.000000000000000000 ) ) ;
#27592 = FACE_OUTER_BOUND ( 'NONE', #69179, .T. ) ;
#27593 = DIRECTION ( 'NONE',  ( 2.603472992745699578E-14, -2.546204323184531851E-14, 1.000000000000000000 ) ) ;
#27594 = CARTESIAN_POINT ( 'NONE',  ( 10.00000000000000000, 30.84782396557248418, -21.32104025579081252 ) ) ;
#27595 = CARTESIAN_POINT ( 'NONE',  ( 0.000000000000000000, -35.92658777277502935, -10.74501242461320594 ) ) ;
#27596 = CARTESIAN_POINT ( 'NONE',  ( 10.00000000000000000, 0.000000000000000000, 0.000000000000000000 ) ) ;
#27597 = AXIS2_PLACEMENT_3D ( 'NONE', #5512, #21008, #22416 ) ;
#27598 = ADVANCED_FACE ( 'NONE', ( #36094 ), #14267, .T. ) ;
#27599 = VERTEX_POINT ( 'NONE', #53026 ) ;
#27600 = CARTESIAN_POINT ( 'NONE',  ( -93.84685191531252713, 88.00268892867056536, 80.32947916753380468 ) ) ;
#27601 = AXIS2_PLACEMENT_3D ( 'NONE', #38444, #10603, #3880 ) ;
#27602 = DIRECTION ( 'NONE',  ( 0.000000000000000000, 0.000000000000000000, 1.000000000000000000 ) ) ;
#27603 = CARTESIAN_POINT ( 'NONE',  ( -97.65000000000001990, 90.00000000000004263, 88.73000000000000398 ) ) ;
#27604 = CYLINDRICAL_SURFACE ( 'NONE', #39416, 20.20000000000036522 ) ;
#27605 = CARTESIAN_POINT ( 'NONE',  ( 5.000000000000002665, -34.94270380257693631, 74.18225833017875459 ) ) ;
#27606 = FACE_OUTER_BOUND ( 'NONE', #209, .T. ) ;
#27607 = CARTESIAN_POINT ( 'NONE',  ( -96.15314808468745866, -211.9973110713294489, 88.00239583420048461 ) ) ;
#27608 = ADVANCED_FACE ( 'NONE', ( #36457, #69926 ), #47016, .F. ) ;
#27609 = ADVANCED_FACE ( 'NONE', ( #48116 ), #42119, .T. ) ;
#27610 = EDGE_CURVE ( 'NONE', #27765, #68607, #14071, .T. ) ;
#27611 = CARTESIAN_POINT ( 'NONE',  ( 92.69370383062498320, 88.66845928578035796, 81.59947916753382913 ) ) ;
#27612 = CARTESIAN_POINT ( 'NONE',  ( -97.30629616937497417, -208.6684592857803295, 81.49364583420049257 ) ) ;
#27613 = LINE ( 'NONE', #208, #11051 ) ;
#27614 = CIRCLE ( 'NONE', #69633, 42.00000000000000000 ) ;
#27615 = ORIENTED_EDGE ( 'NONE', *, *, #23272, .F. ) ;
#27616 = DIRECTION ( 'NONE',  ( -1.000000000000000000, -0.000000000000000000, -0.000000000000000000 ) ) ;
#27617 = CARTESIAN_POINT ( 'NONE',  ( -96.32499999999996021, -212.2949673200287179, 76.13583333333333769 ) ) ;
#27618 = CARTESIAN_POINT ( 'NONE',  ( 92.35000000000000853, 89.99996406754245015, 85.63437624451401575 ) ) ;
#27619 = AXIS2_PLACEMENT_3D ( 'NONE', #39362, #46763, #10789 ) ;
#27620 = AXIS2_PLACEMENT_3D ( 'NONE', #41084, #51236, #74166 ) ;
#27621 = VECTOR ( 'NONE', #73809, 1000.000000000000000 ) ;
#27622 = AXIS2_PLACEMENT_3D ( 'NONE', #62058, #10922, #56793 ) ;
#27623 = VECTOR ( 'NONE', #14401, 1000.000000000000114 ) ;
#27624 = CARTESIAN_POINT ( 'NONE',  ( -96.15314808468752972, 91.99731107132950569, 79.53572916753381605 ) ) ;
#27625 = CARTESIAN_POINT ( 'NONE',  ( 92.69370383062501162, -211.3315407142195852, 80.80572916753382628 ) ) ;
#27626 = VERTEX_POINT ( 'NONE', #47741 ) ;
#27627 = DIRECTION ( 'NONE',  ( 2.603472992746261562E-14, 2.546204323184492723E-14, -1.000000000000000000 ) ) ;
#27628 = ORIENTED_EDGE ( 'NONE', *, *, #8325, .T. ) ;
#27629 = CARTESIAN_POINT ( 'NONE',  ( 10.00000000000000000, -41.76106447765443619, -62.50884508063471401 ) ) ;
#27630 = ORIENTED_EDGE ( 'NONE', *, *, #4434, .T. ) ;
#27631 = AXIS2_PLACEMENT_3D ( 'NONE', #12717, #13089, #1862 ) ;
#27632 = PLANE ( 'NONE',  #21382 ) ;
#27633 = VERTEX_POINT ( 'NONE', #31185 ) ;
#27634 = ORIENTED_EDGE ( 'NONE', *, *, #9695, .T. ) ;
#27635 = VERTEX_POINT ( 'NONE', #70654 ) ;
#27636 = LINE ( 'NONE', #50562, #20293 ) ;
#27637 = ORIENTED_EDGE ( 'NONE', *, *, #3615, .F. ) ;
#27638 = DIRECTION ( 'NONE',  ( 1.000000000000000000, 0.000000000000000000, 0.000000000000000000 ) ) ;
#27639 = EDGE_CURVE ( 'NONE', #10014, #30392, #58288, .T. ) ;
#27640 = LINE ( 'NONE', #73866, #2884 ) ;
#27641 = CARTESIAN_POINT ( 'NONE',  ( 94.99999999999998579, 92.66308142843935514, 85.83281250086714920 ) ) ;
#27642 = PLANE ( 'NONE',  #65784 ) ;
#27643 = CARTESIAN_POINT ( 'NONE',  ( 92.35000000000002274, -211.5299782133524502, 77.98791666666664923 ) ) ;
#27644 = ORIENTED_EDGE ( 'NONE', *, *, #6967, .F. ) ;
#27645 = VERTEX_POINT ( 'NONE', #7159 ) ;
#27646 = ORIENTED_EDGE ( 'NONE', *, *, #29927, .F. ) ;
#27647 = EDGE_LOOP ( 'NONE', ( #44598, #59599, #53817, #66859 ) ) ;
#27648 = LINE ( 'NONE', #49466, #23790 ) ;
#27649 = AXIS2_PLACEMENT_3D ( 'NONE', #30278, #71978, #20852 ) ;
#27650 = ADVANCED_FACE ( 'NONE', ( #64309 ), #54136, .T. ) ;
#27651 = CARTESIAN_POINT ( 'NONE',  ( 0.000000000000000000, 0.000000000000000000, 0.000000000000000000 ) ) ;
#27652 = DIRECTION ( 'NONE',  ( 1.000000000000000000, -0.000000000000000000, 0.000000000000000000 ) ) ;
#27653 = AXIS2_PLACEMENT_3D ( 'NONE', #38297, #61242, #9725 ) ;
#27654 = CARTESIAN_POINT ( 'NONE',  ( 97.64999999997404245, -210.0000117261773198, 82.77687459617033028 ) ) ;
#27655 = EDGE_CURVE ( 'NONE', #59589, #67219, #46592, .T. ) ;
#27656 = CYLINDRICAL_SURFACE ( 'NONE', #21539, 16.00000000000000000 ) ;
#27657 = CARTESIAN_POINT ( 'NONE',  ( 3.000000000000000000, 1.467624384280025174, -2.542000000000001592 ) ) ;
#27658 = EDGE_LOOP ( 'NONE', ( #41148, #44853, #21707, #11895 ) ) ;
#27659 = CARTESIAN_POINT ( 'NONE',  ( -94.99999999999997158, -213.0599564267049857, 83.25312500173430408 ) ) ;
#27660 = VERTEX_POINT ( 'NONE', #49217 ) ;
#27661 = FACE_OUTER_BOUND ( 'NONE', #66232, .T. ) ;
#27662 = VERTEX_POINT ( 'NONE', #37584 ) ;
#27664 = CARTESIAN_POINT ( 'NONE',  ( -93.67500000000003979, 87.70503267997129626, 84.57604166840096127 ) ) ;
#27663 = CARTESIAN_POINT ( 'NONE',  ( 97.64999999999997726, 88.47002178664753558, 82.08895833506764461 ) ) ;
#27665 = ORIENTED_EDGE ( 'NONE', *, *, #23272, .T. ) ;
#27666 = CARTESIAN_POINT ( 'NONE',  ( 97.30629616937498838, 91.33154071421968467, 82.55197916753382970 ) ) ;
#27667 = CARTESIAN_POINT ( 'NONE',  ( 5.999999999999999112, -56.15606465354916566, -59.75363087400133111 ) ) ;
#27668 = CARTESIAN_POINT ( 'NONE',  ( 0.000000000000000000, -75.11764819372149304, 2.946379043146075905 ) ) ;
#27669 = DIRECTION ( 'NONE',  ( -1.000000000000000000, -0.000000000000000000, -0.000000000000000000 ) ) ;
#27670 = CIRCLE ( 'NONE', #66106, 31.99999999999999289 ) ;
#27671 = CARTESIAN_POINT ( 'NONE',  ( 92.48632958231164025, 89.99999999999990052, 74.91808492278045151 ) ) ;
#27672 = EDGE_CURVE ( 'NONE', #18650, #19207, #32288, .T. ) ;
#27673 = FACE_OUTER_BOUND ( 'NONE', #25276, .T. ) ;
#27674 = ORIENTED_EDGE ( 'NONE', *, *, #41665, .T. ) ;
#27675 = DIRECTION ( 'NONE',  ( 0.000000000000000000, 0.9945218953682731788, 0.1045284632676559550 ) ) ;
#27676 = CARTESIAN_POINT ( 'NONE',  ( -96.32500000000001705, 87.70503267997129626, 82.56520833506762358 ) ) ;
#27677 = CIRCLE ( 'NONE', #22918, 32.00000000000000000 ) ;
#27678 = CARTESIAN_POINT ( 'NONE',  ( 94.99999999999998579, 90.00000000000002842, 90.00000000000000000 ) ) ;
#27679 = ORIENTED_EDGE ( 'NONE', *, *, #72624, .F. ) ;
#27680 = ORIENTED_EDGE ( 'NONE', *, *, #52136, .F. ) ;
#27681 = VECTOR ( 'NONE', #24574, 1000.000000000000000 ) ;
#27682 = LINE ( 'NONE', #67537, #71987 ) ;
#27683 = EDGE_CURVE ( 'NONE', #23039, #11760, #60983, .T. ) ;
#27684 = CARTESIAN_POINT ( 'NONE',  ( 10.00000000000000000, -12.26510123303234501, -35.53030884539098366 ) ) ;
#27685 = DIRECTION ( 'NONE',  ( -1.000000000000000000, -0.000000000000000000, 0.000000000000000000 ) ) ;
#27686 = CARTESIAN_POINT ( 'NONE',  ( -97.30629616937497417, -211.3315407142195852, 80.96447916753382401 ) ) ;
#27687 = ORIENTED_EDGE ( 'NONE', *, *, #65305, .T. ) ;
#27688 = CARTESIAN_POINT ( 'NONE',  ( -10.43921258969510824, -98.89258801967538659, -2.500000000000000000 ) ) ;
#27689 = EDGE_CURVE ( 'NONE', #68126, #12127, #53736, .T. ) ;
#27690 = ORIENTED_EDGE ( 'NONE', *, *, #5904, .F. ) ;
#27691 = CYLINDRICAL_SURFACE ( 'NONE', #55900, 77.49899999999999523 ) ;
#27692 = EDGE_CURVE ( 'NONE', #23688, #29022, #72146, .T. ) ;
#27693 = FACE_BOUND ( 'NONE', #17791, .T. ) ;
#27694 = DIRECTION ( 'NONE',  ( 1.000000000000000000, 0.000000000000000000, 0.000000000000000000 ) ) ;
#27695 = DIRECTION ( 'NONE',  ( -1.000000000000000000, -0.000000000000000000, 0.000000000000000000 ) ) ;
#27696 = CARTESIAN_POINT ( 'NONE',  ( -12.40464318976454727, 10.41032311384371667, -45.00000000000000000 ) ) ;
#27697 = LINE ( 'NONE', #50621, #7271 ) ;
#27698 = LINE ( 'NONE', #50622, #31293 ) ;
#27699 = CARTESIAN_POINT ( 'NONE',  ( 2.750000000000000000, 0.000000000000000000, 0.000000000000000000 ) ) ;
#27700 = CYLINDRICAL_SURFACE ( 'NONE', #9971, 31.99999999999998579 ) ;
#27701 = CARTESIAN_POINT ( 'NONE',  ( 10.00000000000000000, -0.8261519478436571973, 77.49459641780886443 ) ) ;
#27702 = EDGE_CURVE ( 'NONE', #69267, #40399, #71750, .T. ) ;
#27703 = CARTESIAN_POINT ( 'NONE',  ( 11.99999999999999822, -36.73666225445940370, 65.58780272294062286 ) ) ;
#27704 = CARTESIAN_POINT ( 'NONE',  ( 11.99999999999999822, 31.47745569255237896, -68.26794271651228030 ) ) ;
#27705 = DIRECTION ( 'NONE',  ( -0.8090169943749504489, 0.5877852522924689183, 0.000000000000000000 ) ) ;
#27706 = LINE ( 'NONE', #46116, #13387 ) ;
#27707 = ORIENTED_EDGE ( 'NONE', *, *, #14094, .T. ) ;
#27708 = VECTOR ( 'NONE', #73923, 1000.000000000000000 ) ;
#27709 = DIRECTION ( 'NONE',  ( 0.000000000000000000, 0.000000000000000000, 1.000000000000000000 ) ) ;
#27710 = CARTESIAN_POINT ( 'NONE',  ( -93.84685191531254134, 91.99731107132950569, 80.54114583420046358 ) ) ;
#27711 = AXIS2_PLACEMENT_3D ( 'NONE', #4690, #10675, #61450 ) ;
#27712 = CARTESIAN_POINT ( 'NONE',  ( 92.69370383062501162, -208.6684592857803011, 89.58989583420047609 ) ) ;
#27713 = ORIENTED_EDGE ( 'NONE', *, *, #37078, .F. ) ;
#27714 =( BOUNDED_CURVE ( )  B_SPLINE_CURVE ( 2, ( #62768, #34526, #45465, #68761, #50708, #22522, #39818, #63864, #23265 ),
 .UNSPECIFIED., .F., .F. ) 
 B_SPLINE_CURVE_WITH_KNOTS ( ( 3, 2, 2, 2, 3 ),
 ( 0.2116728463006670169, 0.2116729662264711653, 0.2187287317673535236, 0.2257844973082358264, 0.2328402629019980796 ),
 .UNSPECIFIED. ) 
 CURVE ( )  GEOMETRIC_REPRESENTATION_ITEM ( )  RATIONAL_B_SPLINE_CURVE ( ( 0.9999954457845842137, 0.9999977228535877893, 1.000000000000000000, 0.8660254037844387076, 1.000000000000000000, 0.8660254037844387076, 1.000000000000000000, 0.8660254037844387076, 1.000000000000000000 ) ) 
 REPRESENTATION_ITEM ( '' )  );
#27715 = CARTESIAN_POINT ( 'NONE',  ( 35.50000000000000711, -120.0000000000000000, 2.500000000000000000 ) ) ;
#27716 = CARTESIAN_POINT ( 'NONE',  ( 11.99999999999999822, -17.28742895386137945, 75.54627589209938776 ) ) ;
#27717 = DIRECTION ( 'NONE',  ( -1.000000000000000000, 0.000000000000000000, -0.000000000000000000 ) ) ;
#27718 = VECTOR ( 'NONE', #11968, 1000.000000000000000 ) ;
#27719 = AXIS2_PLACEMENT_3D ( 'NONE', #54479, #68656, #8628 ) ;
#27720 = LINE ( 'NONE', #62320, #50323 ) ;
#27721 = CARTESIAN_POINT ( 'NONE',  ( 93.84685191531251292, -211.9973110713294489, 75.93739583420048689 ) ) ;
#27722 = VECTOR ( 'NONE', #24432, 1000.000000000000000 ) ;
#27723 = ORIENTED_EDGE ( 'NONE', *, *, #47020, .F. ) ;
#27724 = CIRCLE ( 'NONE', #49346, 77.49900000000000944 ) ;
#27725 = ORIENTED_EDGE ( 'NONE', *, *, #793, .T. ) ;
#27726 = DIRECTION ( 'NONE',  ( -1.000000000000000000, -0.000000000000000000, 0.000000000000000000 ) ) ;
#27727 = FACE_OUTER_BOUND ( 'NONE', #4469, .T. ) ;
#27728 = CARTESIAN_POINT ( 'NONE',  ( -94.99999999999997158, -206.9400435732949575, 85.47562500173430067 ) ) ;
#27729 = DIRECTION ( 'NONE',  ( -1.000000000000000000, 0.000000000000000000, 0.000000000000000000 ) ) ;
#27730 = CARTESIAN_POINT ( 'NONE',  ( -11.59999999999999787, 0.000000000000000000, -54.99999999999998579 ) ) ;
#27731 = CARTESIAN_POINT ( 'NONE',  ( 92.35000000000000853, -209.9999999999999716, 88.73000000000000398 ) ) ;
#27732 = ADVANCED_FACE ( 'NONE', ( #15755 ), #38318, .T. ) ;
#27733 = ORIENTED_EDGE ( 'NONE', *, *, #4809, .F. ) ;
#27734 = ADVANCED_FACE ( 'NONE', ( #9742 ), #43605, .F. ) ;
#27735 = CARTESIAN_POINT ( 'NONE',  ( 0.000000000000000000, 0.000000000000000000, 0.000000000000000000 ) ) ;
#27736 = ORIENTED_EDGE ( 'NONE', *, *, #59261, .F. ) ;
#27737 = ORIENTED_EDGE ( 'NONE', *, *, #63076, .F. ) ;
#27738 = DIRECTION ( 'NONE',  ( -0.5687579148473765889, 0.8225049752423776450, 0.000000000000000000 ) ) ;
#27739 = ADVANCED_FACE ( 'NONE', ( #9001 ), #4545, .F. ) ;
#27740 = FACE_OUTER_BOUND ( 'NONE', #42533, .T. ) ;
#27741 = ORIENTED_EDGE ( 'NONE', *, *, #69088, .T. ) ;
#27742 = CARTESIAN_POINT ( 'NONE',  ( -10.00000000000000000, 0.000000000000000000, 0.000000000000000000 ) ) ;
#27743 = CARTESIAN_POINT ( 'NONE',  ( 92.35000000000000853, -209.9999999999999716, 81.18937500173430521 ) ) ;
#27744 = EDGE_CURVE ( 'NONE', #26721, #71482, #48949, .T. ) ;
#27745 = CARTESIAN_POINT ( 'NONE',  ( 94.99999999999998579, 93.05995642670504253, 83.49125000000000796 ) ) ;
#27746 = ORIENTED_EDGE ( 'NONE', *, *, #58555, .F. ) ;
#27747 = DIRECTION ( 'NONE',  ( -0.000000000000000000, -0.000000000000000000, 1.000000000000000000 ) ) ;
#27748 = ORIENTED_EDGE ( 'NONE', *, *, #36054, .T. ) ;
#27749 = CARTESIAN_POINT ( 'NONE',  ( 10.00000000000000000, 8.966570791700695153, 81.50828551894228724 ) ) ;
#27750 = ORIENTED_EDGE ( 'NONE', *, *, #73389, .T. ) ;
#27751 = CARTESIAN_POINT ( 'NONE',  ( 12.50000000000000000, -107.5000000000000000, -2.500000000000000000 ) ) ;
#27752 = ADVANCED_FACE ( 'NONE', ( #20274 ), #66164, .F. ) ;
#27753 = CARTESIAN_POINT ( 'NONE',  ( -92.69370383062505425, 88.66845928578038638, 84.35114583420050849 ) ) ;
#27754 = CARTESIAN_POINT ( 'NONE',  ( 94.99999999999998579, 87.33691857156068750, 78.37156250086714238 ) ) ;
#27755 = VERTEX_POINT ( 'NONE', #66525 ) ;
#27756 = DIRECTION ( 'NONE',  ( 1.000000000000000000, -3.061616997868382648E-16, -0.000000000000000000 ) ) ;
#27757 = DIRECTION ( 'NONE',  ( -0.000000000000000000, -0.000000000000000000, 1.000000000000000000 ) ) ;
#27758 = CYLINDRICAL_SURFACE ( 'NONE', #23391, 16.00000000000000000 ) ;
#27759 = AXIS2_PLACEMENT_3D ( 'NONE', #15561, #22314, #4302 ) ;
#27760 = CARTESIAN_POINT ( 'NONE',  ( 0.000000000000000000, 36.72794159290334903, -65.59268652807170952 ) ) ;
#27761 = VERTEX_POINT ( 'NONE', #10111 ) ;
#27762 = CARTESIAN_POINT ( 'NONE',  ( 97.64999999999999147, 90.00000000000002842, 75.07749999999998636 ) ) ;
#27763 = VECTOR ( 'NONE', #54054, 1000.000000000000000 ) ;
#27764 = CARTESIAN_POINT ( 'NONE',  ( -93.84685191531248449, -208.0026889286704943, 76.09614583420047040 ) ) ;
#27765 = VERTEX_POINT ( 'NONE', #4493 ) ;
#27766 = EDGE_LOOP ( 'NONE', ( #59642, #38185, #29839, #27460, #56844, #51487, #26010 ) ) ;
#27767 = DIRECTION ( 'NONE',  ( 0.000000000000000000, 0.1564344650402244852, 0.9876883405951387696 ) ) ;
#27768 = EDGE_LOOP ( 'NONE', ( #19813, #63355 ) ) ;
#27769 = FACE_OUTER_BOUND ( 'NONE', #15526, .T. ) ;
#27770 =( REPRESENTATION_RELATIONSHIP ('NONE','NONE', #31117, #67135 ) REPRESENTATION_RELATIONSHIP_WITH_TRANSFORMATION ( #24881 )SHAPE_REPRESENTATION_RELATIONSHIP( ) );
#27771 = CARTESIAN_POINT ( 'NONE',  ( -92.34999999999986642, -211.5299782133523649, 78.19958333333332234 ) ) ;
#27772 = VERTEX_POINT ( 'NONE', #33034 ) ;
#27773 = CARTESIAN_POINT ( 'NONE',  ( -92.69370383062499741, -210.9303297190751891, 74.68334033237940162 ) ) ;
#27774 = ORIENTED_EDGE ( 'NONE', *, *, #67586, .T. ) ;
#27775 = CARTESIAN_POINT ( 'NONE',  ( 10.00000000000000000, -29.01471420065617224, 76.69515212746006227 ) ) ;
#27776 = LINE ( 'NONE', #55230, #34462 ) ;
#27777 = CARTESIAN_POINT ( 'NONE',  ( 10.00000000000000000, -30.00120703465189465, -22.64427369931201639 ) ) ;
#27778 = CARTESIAN_POINT ( 'NONE',  ( -97.64999999999996305, -208.4700217866474645, 89.39145833506763950 ) ) ;
#27779 = DIRECTION ( 'NONE',  ( -0.6575728627325955200, 0.7533909544171997208, 0.000000000000000000 ) ) ;
#27780 = EDGE_CURVE ( 'NONE', #48813, #53009, #37948, .T. ) ;
#27781 = ADVANCED_FACE ( 'NONE', ( #21763 ), #31924, .F. ) ;
#27782 = VECTOR ( 'NONE', #56547, 1000.000000000000114 ) ;
#27783 =( NAMED_UNIT ( * ) PLANE_ANGLE_UNIT ( ) SI_UNIT ( $, .RADIAN. ) );
#27784 = CARTESIAN_POINT ( 'NONE',  ( 93.84685191531248449, 91.99731107132950569, 83.82197916753381151 ) ) ;
#27785 = CARTESIAN_POINT ( 'NONE',  ( 92.34999999999999432, 90.00000000000002842, 90.00000000000000000 ) ) ;
#27786 = VECTOR ( 'NONE', #35929, 1000.000000000000000 ) ;
#27787 = CARTESIAN_POINT ( 'NONE',  ( -7.499999999999969802, 73.00000000000001421, -255.0000000000000000 ) ) ;
#27788 = CARTESIAN_POINT ( 'NONE',  ( 10.00000000000000000, 0.000000000000000000, 0.000000000000000000 ) ) ;
#27789 = DIRECTION ( 'NONE',  ( 1.000000000000000000, 0.000000000000000000, 0.000000000000000000 ) ) ;
#27790 = DIRECTION ( 'NONE',  ( 0.000000000000000000, 0.000000000000000000, 1.000000000000000000 ) ) ;
#27791 = FACE_OUTER_BOUND ( 'NONE', #4454, .T. ) ;
#27792 = EDGE_CURVE ( 'NONE', #590, #5835, #43964, .T. ) ;
#27793 = CARTESIAN_POINT ( 'NONE',  ( 11.99999999999999822, 44.88180994100376608, 63.18004540533043922 ) ) ;
#27794 = CARTESIAN_POINT ( 'NONE',  ( 10.00000000000000000, 10.96151621346487914, 35.95386929396260456 ) ) ;
#27795 = DIRECTION ( 'NONE',  ( 0.000000000000000000, 0.000000000000000000, 1.000000000000000000 ) ) ;
#27796 = LINE ( 'NONE', #72889, #52087 ) ;
#27797 = CARTESIAN_POINT ( 'NONE',  ( 0.000000000000000000, 4.992566952385522505, -37.16516213103271582 ) ) ;
#27798 = CARTESIAN_POINT ( 'NONE',  ( -92.34999999999999432, -209.9999999999999716, 85.23749999999999716 ) ) ;
#27799 = CARTESIAN_POINT ( 'NONE',  ( 97.64999999999999147, 90.00000000000002842, 85.87249999999998806 ) ) ;
#27800 = PRODUCT_DEFINITION_SHAPE ( 'NONE', 'NONE',  #14154 ) ;
#27801 = LINE ( 'NONE', #45109, #65962 ) ;
#27802 = CARTESIAN_POINT ( 'NONE',  ( -7.499999999999968914, 79.99999999999998579, -189.9999999999999147 ) ) ;
#27803 = DIRECTION ( 'NONE',  ( -0.000000000000000000, -0.000000000000000000, -1.000000000000000000 ) ) ;
#27804 = FACE_OUTER_BOUND ( 'NONE', #19035, .T. ) ;
#27805 = CIRCLE ( 'NONE', #67409, 77.49900000000000944 ) ;
#27806 = CARTESIAN_POINT ( 'NONE',  ( 97.30629616937498838, -209.9999999999999716, 86.30906250086715659 ) ) ;
#27807 = AXIS2_PLACEMENT_3D ( 'NONE', #4970, #10209, #32394 ) ;
#27808 = VERTEX_POINT ( 'NONE', #67631 ) ;
#27809 = ORIENTED_EDGE ( 'NONE', *, *, #59722, .F. ) ;
#27810 = VECTOR ( 'NONE', #66426, 1000.000000000000000 ) ;
#27811 = FACE_OUTER_BOUND ( 'NONE', #57958, .T. ) ;
#27812 = ORIENTED_EDGE ( 'NONE', *, *, #53374, .T. ) ;
#27813 = CYLINDRICAL_SURFACE ( 'NONE', #20953, 15.50000000000000000 ) ;
#27814 = CARTESIAN_POINT ( 'NONE',  ( 92.69370383062501162, -208.6684592857803295, 77.52489583420046415 ) ) ;
#27815 = ORIENTED_EDGE ( 'NONE', *, *, #38044, .F. ) ;
#27816 = CARTESIAN_POINT ( 'NONE',  ( 96.15314808468748708, -208.0026889286704943, 81.33489583420049485 ) ) ;
#27817 = VERTEX_POINT ( 'NONE', #37218 ) ;
#27818 = DIRECTION ( 'NONE',  ( -1.000000000000000000, -0.000000000000000000, -0.000000000000000000 ) ) ;
#27819 = ORIENTED_EDGE ( 'NONE', *, *, #73461, .T. ) ;
#27820 = VECTOR ( 'NONE', #49669, 1000.000000000000000 ) ;
#27821 = DIRECTION ( 'NONE',  ( 0.000000000000000000, 0.7431448254773954654, 0.6691306063588569053 ) ) ;
#27822 = AXIS2_PLACEMENT_3D ( 'NONE', #9631, #66417, #32549 ) ;
#27823 = EDGE_CURVE ( 'NONE', #17352, #19508, #34525, .T. ) ;
#27824 = FACE_OUTER_BOUND ( 'NONE', #67614, .T. ) ;
#27825 = VECTOR ( 'NONE', #58405, 1000.000000000000000 ) ;
#27826 = SHAPE_REPRESENTATION ( 'radial ball bearing_68_iso_ISO 15 RBB - 3025 - 14,SI,NC,14_68', ( #43395 ), #61521 ) ;
#27827 = ORIENTED_EDGE ( 'NONE', *, *, #39885, .F. ) ;
#27828 = FACE_OUTER_BOUND ( 'NONE', #63374, .T. ) ;
#27829 = DIRECTION ( 'NONE',  ( 1.000000000000000000, 0.000000000000000000, 0.000000000000000000 ) ) ;
#27830 = EDGE_CURVE ( 'NONE', #19590, #69518, #15371, .T. ) ;
#27831 = ORIENTED_EDGE ( 'NONE', *, *, #14190, .F. ) ;
#27832 = DIRECTION ( 'NONE',  ( 0.000000000000000000, 0.8526401643540897357, 0.5224985647159527957 ) ) ;
#27833 = VERTEX_POINT ( 'NONE', #28142 ) ;
#27834 = DIRECTION ( 'NONE',  ( 0.000000000000000000, 0.000000000000000000, 1.000000000000000000 ) ) ;
#27835 = EDGE_CURVE ( 'NONE', #49658, #5816, #28511, .T. ) ;
#27836 = ORIENTED_EDGE ( 'NONE', *, *, #63592, .F. ) ;
#27837 = ORIENTED_EDGE ( 'NONE', *, *, #59788, .F. ) ;
#27838 = ORIENTED_EDGE ( 'NONE', *, *, #33870, .F. ) ;
#27839 = CARTESIAN_POINT ( 'NONE',  ( 97.30629616937498838, -208.6684592857803011, 76.67822916753378593 ) ) ;
#27840 = CONTEXT_DEPENDENT_SHAPE_REPRESENTATION ( #7132, #12237 ) ;
#27841 = DIRECTION ( 'NONE',  ( -1.000000000000000000, 0.000000000000000000, 0.000000000000000000 ) ) ;
#27842 = ORIENTED_EDGE ( 'NONE', *, *, #23264, .F. ) ;
#27843 = ORIENTED_EDGE ( 'NONE', *, *, #44051, .F. ) ;
#27844 = VERTEX_POINT ( 'NONE', #40177 ) ;
#27845 = DIRECTION ( 'NONE',  ( 0.000000000000000000, 0.000000000000000000, -1.000000000000000000 ) ) ;
#27846 = EDGE_CURVE ( 'NONE', #40890, #33344, #28505, .T. ) ;
#27847 = CARTESIAN_POINT ( 'NONE',  ( -92.69370383062504004, 90.00000000000004263, 76.78406250086715090 ) ) ;
#27848 = EDGE_CURVE ( 'NONE', #41714, #35387, #50704, .T. ) ;
#27849 = EDGE_LOOP ( 'NONE', ( #15356, #1913, #40969, #51150 ) ) ;
#27850 = CARTESIAN_POINT ( 'NONE',  ( 92.69370383062498320, 88.66845928578037217, 75.72572916753381378 ) ) ;
#27851 = VERTEX_POINT ( 'NONE', #62002 ) ;
#27852 = CARTESIAN_POINT ( 'NONE',  ( 92.34999999999999432, 90.00000000000002842, 80.47499999999999432 ) ) ;
#27853 = CARTESIAN_POINT ( 'NONE',  ( -93.84685191531248449, -208.0026889286704943, 84.98614583420047097 ) ) ;
#27854 = EDGE_LOOP ( 'NONE', ( #33190, #53325, #66391, #1473 ) ) ;
#27855 = CARTESIAN_POINT ( 'NONE',  ( 96.90829729882862864, -211.8387227684681591, 74.99954709728268654 ) ) ;
#27856 = FACE_OUTER_BOUND ( 'NONE', #64997, .T. ) ;
#27857 = CARTESIAN_POINT ( 'NONE',  ( 96.32499999999998863, 87.70503267997126784, 81.32166666666667254 ) ) ;
#27858 = CARTESIAN_POINT ( 'NONE',  ( -96.15314808468747287, -208.0026889286704943, 78.10697916753380809 ) ) ;
#27859 = CIRCLE ( 'NONE', #7427, 3.299999999999983391 ) ;
#27860 = CARTESIAN_POINT ( 'NONE',  ( 15.00000000000000000, 9.615535125378766423, -24.73947219025917121 ) ) ;
#27861 = CARTESIAN_POINT ( 'NONE',  ( -3.000000000000000000, -14.54903810567645195, -22.19967320028775504 ) ) ;
#27862 = CARTESIAN_POINT ( 'NONE',  ( 5.999999999999999112, -60.67117009219175827, 55.16347631943019536 ) ) ;
#27863 = EDGE_CURVE ( 'NONE', #70343, #31915, #64131, .T. ) ;
#27864 = ADVANCED_FACE ( 'NONE', ( #12605 ), #70112, .T. ) ;
#27865 = CIRCLE ( 'NONE', #59109, 5.000000000000000888 ) ;
#27866 = VERTEX_POINT ( 'NONE', #17244 ) ;
#27867 = CARTESIAN_POINT ( 'NONE',  ( 10.00000000000000000, 0.000000000000000000, 0.000000000000000000 ) ) ;
#27868 = DIRECTION ( 'NONE',  ( 0.000000000000000000, -0.8090169943749433434, 0.5877852522924787992 ) ) ;
#27869 = CARTESIAN_POINT ( 'NONE',  ( 4.999999999999999112, -38.55633173627022359, 16.65560815589396526 ) ) ;
#27870 = AXIS2_PLACEMENT_3D ( 'NONE', #10481, #50705, #44716 ) ;
#27871 = CARTESIAN_POINT ( 'NONE',  ( -97.30629616937501680, 91.33154071421968467, 83.23989583420046756 ) ) ;
#27872 = DIRECTION ( 'NONE',  ( 0.000000000000000000, 0.000000000000000000, 1.000000000000000000 ) ) ;
#27873 = CARTESIAN_POINT ( 'NONE',  ( -22.67106064244953245, -113.6342314410295842, 5.500000000000000000 ) ) ;
#27874 = CIRCLE ( 'NONE', #3900, 16.00000000000000355 ) ;
#27875 = ORIENTED_EDGE ( 'NONE', *, *, #48656, .F. ) ;
#27876 = LINE ( 'NONE', #50800, #50958 ) ;
#27877 = CIRCLE ( 'NONE', #25471, 82.00000000000000000 ) ;
#27878 = LINE ( 'NONE', #67739, #32797 ) ;
#27879 = DIRECTION ( 'NONE',  ( 0.000000000000000000, 0.000000000000000000, 1.000000000000000000 ) ) ;
#27880 = TOROIDAL_SURFACE ( 'NONE', #19452, 22.90000000000000213, 0.5999999999999937605 ) ;
#27881 = DIRECTION ( 'NONE',  ( 1.000000000000000000, -0.000000000000000000, 0.000000000000000000 ) ) ;
#27882 = DIRECTION ( 'NONE',  ( -1.000000000000000000, -0.000000000000000000, 0.000000000000000000 ) ) ;
#27883 = DIRECTION ( 'NONE',  ( -1.000000000000000000, 0.000000000000000000, -0.000000000000000000 ) ) ;
#27884 = CARTESIAN_POINT ( 'NONE',  ( -96.15314808468745866, -211.9973110713294489, 79.74739583420048916 ) ) ;
#27885 = CARTESIAN_POINT ( 'NONE',  ( 6.000000000000000000, -39.47590169984795239, -71.87247863392455827 ) ) ;
#27886 = ORIENTED_EDGE ( 'NONE', *, *, #23505, .T. ) ;
#27887 = CARTESIAN_POINT ( 'NONE',  ( -20.63749999999999218, 1.052885139195391297E-13, 12.50000000000021139 ) ) ;
#27888 = DIRECTION ( 'NONE',  ( -1.000000000000000000, -0.000000000000000000, -0.000000000000000000 ) ) ;
#27889 = CARTESIAN_POINT ( 'NONE',  ( 0.000000000000000000, -14.66109333815513160, 73.73191006444567108 ) ) ;
#27890 = ORIENTED_EDGE ( 'NONE', *, *, #9668, .T. ) ;
#27891 = CARTESIAN_POINT ( 'NONE',  ( 96.32499999999997442, 92.29496732002878900, 77.16770833506762983 ) ) ;
#27892 = FACE_OUTER_BOUND ( 'NONE', #38690, .T. ) ;
#27893 = CARTESIAN_POINT ( 'NONE',  ( 10.00000000000000000, 21.40280677340372151, 36.13751322684426981 ) ) ;
#27894 = ORIENTED_EDGE ( 'NONE', *, *, #35801, .T. ) ;
#27895 = ADVANCED_FACE ( 'NONE', ( #68005, #10480, #6966, #7352, #47199, #33789, #22518 ), #56362, .T. ) ;
#27896 = LINE ( 'NONE', #72631, #13239 ) ;
#27897 = PLANE ( 'NONE',  #60747 ) ;
#27898 = ORIENTED_EDGE ( 'NONE', *, *, #27499, .F. ) ;
#27899 = EDGE_CURVE ( 'NONE', #60573, #18312, #24631, .T. ) ;
#27900 = CARTESIAN_POINT ( 'NONE',  ( 95.00000000000000000, -207.3369185715606307, 88.21406250086712930 ) ) ;
#27901 = CARTESIAN_POINT ( 'NONE',  ( 0.000000000000000000, 0.000000000000000000, 52.00000000000002132 ) ) ;
#27902 = ORIENTED_EDGE ( 'NONE', *, *, #38130, .F. ) ;
#27903 = EDGE_CURVE ( 'NONE', #69628, #39489, #40897, .T. ) ;
#27904 = PLANE ( 'NONE',  #48874 ) ;
#27905 = ORIENTED_EDGE ( 'NONE', *, *, #1560, .F. ) ;
#27906 = CARTESIAN_POINT ( 'NONE',  ( -93.67499999999998295, -207.7050326799711968, 84.78770833506763438 ) ) ;
#27907 = ORIENTED_EDGE ( 'NONE', *, *, #5887, .T. ) ;
#27908 = LINE ( 'NONE', #5743, #67259 ) ;
#27909 = VECTOR ( 'NONE', #48254, 1000.000000000000000 ) ;
#27910 = ORIENTED_EDGE ( 'NONE', *, *, #36804, .F. ) ;
#27911 = EDGE_CURVE ( 'NONE', #57906, #55377, #58470, .T. ) ;
#27912 = ORIENTED_EDGE ( 'NONE', *, *, #24602, .F. ) ;
#27913 = VERTEX_POINT ( 'NONE', #53206 ) ;
#27914 = DIRECTION ( 'NONE',  ( -1.000000000000000000, 0.000000000000000000, 0.000000000000000000 ) ) ;
#27915 = ADVANCED_FACE ( 'NONE', ( #62384 ), #68391, .T. ) ;
#27916 = CIRCLE ( 'NONE', #29096, 82.00000000000000000 ) ;
#27917 = ORIENTED_EDGE ( 'NONE', *, *, #28839, .T. ) ;
#27918 = ORIENTED_EDGE ( 'NONE', *, *, #9864, .F. ) ;
#27919 =( BOUNDED_CURVE ( )  B_SPLINE_CURVE ( 2, ( #63968, #74113, #69950, #24113, #16985, #12439, #57586 ),
 .UNSPECIFIED., .F., .F. ) 
 B_SPLINE_CURVE_WITH_KNOTS ( ( 3, 2, 2, 3 ),
 ( 0.1270039290051391268, 0.1340595452767650020, 0.1411153108176473325, 0.1481709449575320525 ),
 .UNSPECIFIED. ) 
 CURVE ( )  GEOMETRIC_REPRESENTATION_ITEM ( )  RATIONAL_B_SPLINE_CURVE ( ( 0.9999943314824810692, 0.8660282381031599863, 1.000000000000000000, 0.8660254037844387076, 1.000000000000000000, 0.8660278988213697682, 0.9999950100190690971 ) ) 
 REPRESENTATION_ITEM ( '' )  );
#27920 = CARTESIAN_POINT ( 'NONE',  ( 96.32499999999998863, 87.70503267997126784, 88.94166666666666288 ) ) ;
#27921 = DIRECTION ( 'NONE',  ( 0.000000000000000000, 0.000000000000000000, -1.000000000000000000 ) ) ;
#27922 = EDGE_CURVE ( 'NONE', #61856, #37995, #45460, .T. ) ;
#27923 = DIRECTION ( 'NONE',  ( -0.5000000000000006661, 0.8660254037844382635, 0.000000000000000000 ) ) ;
#27924 = ORIENTED_EDGE ( 'NONE', *, *, #41085, .F. ) ;
#27925 = VERTEX_POINT ( 'NONE', #39065 ) ;
#27926 = ORIENTED_EDGE ( 'NONE', *, *, #57625, .T. ) ;
#27927 = CARTESIAN_POINT ( 'NONE',  ( 97.30629616937498838, 88.66845928578037217, 88.63739583420047552 ) ) ;
#27928 = VECTOR ( 'NONE', #27960, 1000.000000000000000 ) ;
#27929 = ORIENTED_EDGE ( 'NONE', *, *, #58551, .T. ) ;
#27930 = CARTESIAN_POINT ( 'NONE',  ( 96.15314808468750130, -211.9973110713294489, 86.04447916753380809 ) ) ;
#27931 = CIRCLE ( 'NONE', #47156, 42.00000000000000000 ) ;
#27932 = CYLINDRICAL_SURFACE ( 'NONE', #43829, 4.750000000000000000 ) ;
#27933 = CYLINDRICAL_SURFACE ( 'NONE', #64238, 31.99999999999998579 ) ;
#27934 = CARTESIAN_POINT ( 'NONE',  ( 10.00000000000000000, 39.04073710021344112, 15.48615015657596317 ) ) ;
#27935 = DIRECTION ( 'NONE',  ( 0.000000000000000000, 0.000000000000000000, 1.000000000000000000 ) ) ;
#27936 = DIRECTION ( 'NONE',  ( -1.000000000000000000, 0.000000000000000000, 0.000000000000000000 ) ) ;
#27937 = CARTESIAN_POINT ( 'NONE',  ( -92.69370383062498320, -208.6684592857803011, 86.83822916753381094 ) ) ;
#27938 = EDGE_CURVE ( 'NONE', #10371, #68327, #40543, .T. ) ;
#27939 = CARTESIAN_POINT ( 'NONE',  ( -96.15314808468751551, 88.00268892867056536, 86.09739583420049769 ) ) ;
#27940 = EDGE_CURVE ( 'NONE', #38016, #49934, #26139, .T. ) ;
#27941 = VERTEX_POINT ( 'NONE', #62765 ) ;
#27943 = CARTESIAN_POINT ( 'NONE',  ( -95.00000000000002842, 87.33691857156074434, 85.99156250086714692 ) ) ;
#27942 = CARTESIAN_POINT ( 'NONE',  ( 93.84685191531248449, 91.99731107132950569, 86.36197916753381776 ) ) ;
#27944 = VERTEX_POINT ( 'NONE', #11227 ) ;
#27945 = FACE_OUTER_BOUND ( 'NONE', #17862, .T. ) ;
#27946 = DIRECTION ( 'NONE',  ( -1.000000000000000000, -0.000000000000000000, 0.000000000000000000 ) ) ;
#27947 = DIRECTION ( 'NONE',  ( 0.000000000000000000, -0.4539904997395540764, 0.8910065241883642351 ) ) ;
#27948 = DIRECTION ( 'NONE',  ( 0.000000000000000000, 0.000000000000000000, 1.000000000000000000 ) ) ;
#27949 = DIRECTION ( 'NONE',  ( -0.000000000000000000, -0.000000000000000000, -1.000000000000000000 ) ) ;
#27950 = CARTESIAN_POINT ( 'NONE',  ( 5.000000000000002665, -10.30890764327441822, 81.34940948281332851 ) ) ;
#27951 = CARTESIAN_POINT ( 'NONE',  ( 0.1915406271734537980, -118.5122795329289858, -2.500000000000000000 ) ) ;
#27952 = CARTESIAN_POINT ( 'NONE',  ( 10.00000000000000000, 35.53030884539084866, 12.26510123303271982 ) ) ;
#27953 = VERTEX_POINT ( 'NONE', #34160 ) ;
#27954 = EDGE_LOOP ( 'NONE', ( #71091, #72471, #23485, #12540 ) ) ;
#27955 = CARTESIAN_POINT ( 'NONE',  ( -92.35000000000003695, 90.00000000000004263, 81.42749999999999488 ) ) ;
#27956 = FACE_OUTER_BOUND ( 'NONE', #73245, .T. ) ;
#27957 = CARTESIAN_POINT ( 'NONE',  ( -97.65000000000001990, 90.00000000000004263, 78.57000000000000739 ) ) ;
#27958 = DIRECTION ( 'NONE',  ( -3.061616997868382648E-16, -1.000000000000000000, 0.000000000000000000 ) ) ;
#27959 = CARTESIAN_POINT ( 'NONE',  ( -96.32500000000001705, 92.29496732002878900, 79.81354166840095843 ) ) ;
#27960 = DIRECTION ( 'NONE',  ( -1.000000000000000000, 0.000000000000000000, 0.000000000000000000 ) ) ;
#27961 = CARTESIAN_POINT ( 'NONE',  ( -92.34999999999999432, -209.9999999999999716, 90.00000000000000000 ) ) ;
#27962 = CARTESIAN_POINT ( 'NONE',  ( -92.34999999999999432, -209.9999999999999716, 79.52249999999999375 ) ) ;
#27963 = ORIENTED_EDGE ( 'NONE', *, *, #53898, .T. ) ;
#27964 = CARTESIAN_POINT ( 'NONE',  ( -92.69370383062504004, 90.00000000000004263, 78.53031250086714010 ) ) ;
#27965 = DIRECTION ( 'NONE',  ( -0.000000000000000000, -0.000000000000000000, -1.000000000000000000 ) ) ;
#27966 = DIRECTION ( 'NONE',  ( 0.000000000000000000, 0.000000000000000000, 1.000000000000000000 ) ) ;
#27967 = AXIS2_PLACEMENT_3D ( 'NONE', #69880, #12007, #34943 ) ;
#27968 = CARTESIAN_POINT ( 'NONE',  ( -12.50000000000000000, -132.5000000000000000, 2.500000000000000000 ) ) ;
#27969 = CARTESIAN_POINT ( 'NONE',  ( -92.34999999999999432, -209.9999999999999716, 82.06250000000000000 ) ) ;
#27970 = DIRECTION ( 'NONE',  ( -1.000000000000000000, 0.000000000000000000, 0.000000000000000000 ) ) ;
#27971 = CARTESIAN_POINT ( 'NONE',  ( -92.69370383062498320, -211.3315407142195852, 89.43114583420049257 ) ) ;
#27972 = FILL_AREA_STYLE ('',( #44917 ) ) ;
#27973 = CIRCLE ( 'NONE', #38767, 16.00000000000000000 ) ;
#27974 = CARTESIAN_POINT ( 'NONE',  ( 92.69370383062498320, 88.66845928578035796, 80.96447916753382401 ) ) ;
#27975 = EDGE_CURVE ( 'NONE', #51621, #74311, #57105, .T. ) ;
#27976 = CARTESIAN_POINT ( 'NONE',  ( -94.99999999999997158, -207.3369185715606307, 81.38781250086715602 ) ) ;
#27977 = CARTESIAN_POINT ( 'NONE',  ( -2.500000000000011990, -62.44997998398397954, -275.0000000000000000 ) ) ;
#27978 = VERTEX_POINT ( 'NONE', #64866 ) ;
#27979 = CARTESIAN_POINT ( 'NONE',  ( -3.000000000000000000, -26.23277895567245821, -4.042438405570103477 ) ) ;
#27980 = DIRECTION ( 'NONE',  ( -1.000000000000000000, 0.000000000000000000, 0.000000000000000000 ) ) ;
#27981 = CARTESIAN_POINT ( 'NONE',  ( -20.63749999999998863, 1.408645127833826896E-13, 15.80000000000026539 ) ) ;
#27982 = AXIS2_PLACEMENT_3D ( 'NONE', #32293, #20280, #26661 ) ;
#27983 = VECTOR ( 'NONE', #10120, 1000.000000000000000 ) ;
#27984 = EDGE_CURVE ( 'NONE', #50169, #22009, #56717, .T. ) ;
#27985 = CARTESIAN_POINT ( 'NONE',  ( -97.30629616937501680, 88.66845928578038638, 79.69447916753381378 ) ) ;
#27986 = CARTESIAN_POINT ( 'NONE',  ( 97.30629616937498838, -211.3315407142195852, 79.11239583420046984 ) ) ;
#27987 = ORIENTED_EDGE ( 'NONE', *, *, #34196, .T. ) ;
#27988 = EDGE_CURVE ( 'NONE', #26527, #53791, #10527, .T. ) ;
#27989 = LINE ( 'NONE', #63710, #32280 ) ;
#27990 = VERTEX_POINT ( 'NONE', #25382 ) ;
#27991 = DIRECTION ( 'NONE',  ( 0.000000000000000000, 1.000000000000000000, 3.491481338843133750E-15 ) ) ;
#27992 = ORIENTED_EDGE ( 'NONE', *, *, #58392, .T. ) ;
#27993 = EDGE_CURVE ( 'NONE', #55165, #39002, #12937, .T. ) ;
#27994 = LINE ( 'NONE', #12918, #70587 ) ;
#27995 = ORIENTED_EDGE ( 'NONE', *, *, #62672, .T. ) ;
#27996 = ORIENTED_EDGE ( 'NONE', *, *, #15076, .T. ) ;
#27997 = ORIENTED_EDGE ( 'NONE', *, *, #67078, .F. ) ;
#27998 = CARTESIAN_POINT ( 'NONE',  ( -12.00000000000000000, 2.119128821244579932E-15, 17.30399999999999849 ) ) ;
#27999 = ORIENTED_EDGE ( 'NONE', *, *, #63190, .F. ) ;
#28000 = LINE ( 'NONE', #62618, #13584 ) ;
#28001 = CIRCLE ( 'NONE', #15984, 31.99999999999998579 ) ;
#28002 = CARTESIAN_POINT ( 'NONE',  ( 97.64999999999999147, -209.9999999999999716, 83.96750000000000114 ) ) ;
#28003 = CARTESIAN_POINT ( 'NONE',  ( 97.30629616937498838, 88.66845928578037217, 85.62114583420047609 ) ) ;
#28004 = EDGE_CURVE ( 'NONE', #33844, #19051, #3373, .T. ) ;
#28005 = DIRECTION ( 'NONE',  ( 0.000000000000000000, 0.000000000000000000, 1.000000000000000000 ) ) ;
#28006 = CARTESIAN_POINT ( 'NONE',  ( 95.00000000000000000, -213.0599564267049857, 78.09374999999998579 ) ) ;
#28007 = ORIENTED_EDGE ( 'NONE', *, *, #73152, .F. ) ;
#28008 = ORIENTED_EDGE ( 'NONE', *, *, #53907, .T. ) ;
#28009 = EDGE_LOOP ( 'NONE', ( #38082, #65924, #24168, #69625 ) ) ;
#28010 = ORIENTED_EDGE ( 'NONE', *, *, #27672, .F. ) ;
#28011 = LINE ( 'NONE', #69350, #16644 ) ;
#28012 = VECTOR ( 'NONE', #67010, 1000.000000000000000 ) ;
#28013 = CARTESIAN_POINT ( 'NONE',  ( 0.000000000000000000, -41.81611651403864727, 3.925862922256025289 ) ) ;
#28014 = CARTESIAN_POINT ( 'NONE',  ( -93.17363653571624127, 88.24022384386938711, 74.93163452119475210 ) ) ;
#28015 = FACE_OUTER_BOUND ( 'NONE', #44153, .T. ) ;
#28016 = DIRECTION ( 'NONE',  ( -1.000000000000000000, 1.776356839400250465E-15, 0.000000000000000000 ) ) ;
#28017 = DIRECTION ( 'NONE',  ( 0.000000000000000000, -1.000000000000000000, 1.181994176819165452E-15 ) ) ;
#28018 = VERTEX_POINT ( 'NONE', #36278 ) ;
#28019 = CARTESIAN_POINT ( 'NONE',  ( -96.32499999999996021, -207.7050326799711968, 81.08354166840096866 ) ) ;
#28021 = ORIENTED_EDGE ( 'NONE', *, *, #58726, .F. ) ;
#28020 = EDGE_CURVE ( 'NONE', #39761, #44032, #50127, .T. ) ;
#28022 = FACE_OUTER_BOUND ( 'NONE', #43213, .T. ) ;
#28023 = ADVANCED_FACE ( 'NONE', ( #70472 ), #37025, .F. ) ;
#28024 = ORIENTED_EDGE ( 'NONE', *, *, #42132, .F. ) ;
#28026 = CARTESIAN_POINT ( 'NONE',  ( -96.32500000000001705, 87.70503267997129626, 78.75520833506763552 ) ) ;
#28025 = CARTESIAN_POINT ( 'NONE',  ( 96.32499999999997442, 92.29496732002878900, 82.24770833506762813 ) ) ;
#28027 = AXIS2_PLACEMENT_3D ( 'NONE', #3255, #19765, #26522 ) ;
#28029 = ADVANCED_FACE ( 'NONE', ( #30627 ), #3576, .F. ) ;
#28028 = EDGE_LOOP ( 'NONE', ( #44104, #44319, #62126, #57078 ) ) ;
#28030 = CARTESIAN_POINT ( 'NONE',  ( 93.84685191531248449, 91.99731107132950569, 84.61572916753381435 ) ) ;
#28031 = CARTESIAN_POINT ( 'NONE',  ( -94.99999999999997158, -206.9400435732949575, 86.66624999999999091 ) ) ;
#28032 = DIRECTION ( 'NONE',  ( -1.000000000000000000, -0.000000000000000000, 0.000000000000000000 ) ) ;
#28033 = CARTESIAN_POINT ( 'NONE',  ( 11.99999999999999822, -59.03961581697432592, 46.53671651293927880 ) ) ;
#28034 = CARTESIAN_POINT ( 'NONE',  ( 0.000000000000000000, 0.000000000000000000, 0.000000000000000000 ) ) ;
#28035 = DIRECTION ( 'NONE',  ( 1.000000000000000000, 0.000000000000000000, -0.000000000000000000 ) ) ;
#28036 = EDGE_LOOP ( 'NONE', ( #7246, #31167, #10079, #71069 ) ) ;
#28037 = CARTESIAN_POINT ( 'NONE',  ( 0.000000000000000000, 0.000000000000000000, 0.000000000000000000 ) ) ;
#28039 = CARTESIAN_POINT ( 'NONE',  ( 10.00000000000000000, -33.79645857604501913, -16.45098606841161626 ) ) ;
#28038 = CIRCLE ( 'NONE', #4067, 31.99999999999998579 ) ;
#28040 = AXIS2_PLACEMENT_3D ( 'NONE', #32209, #20582, #48772 ) ;
#28041 = DIRECTION ( 'NONE',  ( 7.962523111839282146E-16, -1.065814103640130873E-14, -1.000000000000000000 ) ) ;
#28042 = ORIENTED_EDGE ( 'NONE', *, *, #60726, .F. ) ;
#28043 = ORIENTED_EDGE ( 'NONE', *, *, #65389, .T. ) ;
#28044 = CYLINDRICAL_SURFACE ( 'NONE', #19164, 2.649999999999985700 ) ;
#28045 = DIRECTION ( 'NONE',  ( -1.000000000000000000, 0.000000000000000000, -0.000000000000000000 ) ) ;
#28046 = DIRECTION ( 'NONE',  ( -1.000000000000000000, 0.000000000000000000, 0.000000000000000000 ) ) ;
#28047 = CARTESIAN_POINT ( 'NONE',  ( 26.09152095774781799, -124.8716048804687375, 5.500000000000000000 ) ) ;
#28048 = CARTESIAN_POINT ( 'NONE',  ( -93.84685191531247028, -211.9973110713294489, 82.39322916753381776 ) ) ;
#28049 = ORIENTED_EDGE ( 'NONE', *, *, #25779, .T. ) ;
#28050 = CARTESIAN_POINT ( 'NONE',  ( 10.00000000000000000, 62.20884554314020676, 46.21855187248652896 ) ) ;
#28051 = ORIENTED_EDGE ( 'NONE', *, *, #48119, .T. ) ;
#28052 = AXIS2_PLACEMENT_3D ( 'NONE', #47451, #71100, #70734 ) ;
#28053 = CARTESIAN_POINT ( 'NONE',  ( 10.00000000000000000, 0.000000000000000000, 0.000000000000000000 ) ) ;
#28054 = LINE ( 'NONE', #12612, #41478 ) ;
#28055 = LINE ( 'NONE', #283, #24919 ) ;
#28056 = CARTESIAN_POINT ( 'NONE',  ( 94.99999999999998579, 87.33691857156068750, 75.19656250086714522 ) ) ;
#28057 = DIRECTION ( 'NONE',  ( 0.000000000000000000, 0.000000000000000000, 1.000000000000000000 ) ) ;
#28058 = LINE ( 'NONE', #16797, #52879 ) ;
#28059 = DIRECTION ( 'NONE',  ( -1.000000000000000000, -0.000000000000000000, -0.000000000000000000 ) ) ;
#28060 = DIRECTION ( 'NONE',  ( -0.000000000000000000, -0.000000000000000000, -1.000000000000000000 ) ) ;
#28061 = CARTESIAN_POINT ( 'NONE',  ( 12.00000000000000000, -23.29833615347104470, 3.418703333116808629 ) ) ;
#28062 = LINE ( 'NONE', #39360, #1027 ) ;
#28063 = AXIS2_PLACEMENT_3D ( 'NONE', #7229, #8703, #31620 ) ;
#28064 = DIRECTION ( 'NONE',  ( -0.3853207896976523772, 0.9227826878668550226, 0.000000000000000000 ) ) ;
#28065 = CARTESIAN_POINT ( 'NONE',  ( 25.81725066941077884, -113.8380548628854854, 2.500000000000000000 ) ) ;
#28066 = CIRCLE ( 'NONE', #38865, 82.00000000000000000 ) ;
#28067 = CARTESIAN_POINT ( 'NONE',  ( -92.69370383062498320, -208.6684592857803295, 89.53697916753382913 ) ) ;
#28068 = CARTESIAN_POINT ( 'NONE',  ( 0.000000000000000000, 0.000000000000000000, 0.000000000000000000 ) ) ;
#28070 = ADVANCED_FACE ( 'NONE', ( #47932 ), #70854, .F. ) ;
#28069 = VERTEX_POINT ( 'NONE', #53572 ) ;
#28071 = DIRECTION ( 'NONE',  ( 0.000000000000000000, 0.000000000000000000, -1.000000000000000000 ) ) ;
#28072 = CARTESIAN_POINT ( 'NONE',  ( -97.30629616937501680, 88.66845928578038638, 79.53572916753380184 ) ) ;
#28073 = VECTOR ( 'NONE', #7397, 999.9999999999998863 ) ;
#28074 = EDGE_CURVE ( 'NONE', #32803, #70819, #26102, .T. ) ;
#28075 = DIRECTION ( 'NONE',  ( 0.000000000000000000, -0.8910065241883722287, 0.4539904997395382558 ) ) ;
#28076 = EDGE_CURVE ( 'NONE', #4971, #38198, #8461, .T. ) ;
#28077 = ORIENTED_EDGE ( 'NONE', *, *, #13811, .T. ) ;
#28078 = AXIS2_PLACEMENT_3D ( 'NONE', #28940, #11276, #12015 ) ;
#28079 = CARTESIAN_POINT ( 'NONE',  ( -20.63749999999997797, 1.882991779351789328E-13, 20.20000000000035101 ) ) ;
#28081 = DIRECTION ( 'NONE',  ( 0.000000000000000000, 0.000000000000000000, 1.000000000000000000 ) ) ;
#28080 = AXIS2_PLACEMENT_3D ( 'NONE', #11074, #22351, #15963 ) ;
#28082 = FACE_OUTER_BOUND ( 'NONE', #52021, .T. ) ;
#28083 = EDGE_CURVE ( 'NONE', #34215, #24836, #978, .T. ) ;
#28084 = AXIS2_PLACEMENT_3D ( 'NONE', #23819, #68590, #932 ) ;
#28085 = LINE ( 'NONE', #55920, #46752 ) ;
#28086 = VECTOR ( 'NONE', #20754, 1000.000000000000000 ) ;
#28087 = CARTESIAN_POINT ( 'NONE',  ( 95.00000000000000000, -212.6630814284392557, 75.35531250086715715 ) ) ;
#28088 = ORIENTED_EDGE ( 'NONE', *, *, #26603, .F. ) ;
#28089 = ORIENTED_EDGE ( 'NONE', *, *, #17427, .F. ) ;
#28090 = CARTESIAN_POINT ( 'NONE',  ( -92.35000000000547971, -210.0000054026037049, 81.50687481489497088 ) ) ;
#28091 = EDGE_CURVE ( 'NONE', #17154, #18663, #9351, .T. ) ;
#28092 = DIRECTION ( 'NONE',  ( 0.000000000000000000, 0.000000000000000000, 1.000000000000000000 ) ) ;
#28093 = CARTESIAN_POINT ( 'NONE',  ( -92.35000000000006537, -209.9999992849074317, 85.31687502647974952 ) ) ;
#28094 = DIRECTION ( 'NONE',  ( -0.000000000000000000, -0.000000000000000000, -1.000000000000000000 ) ) ;
#28095 = EDGE_CURVE ( 'NONE', #48030, #42459, #52601, .T. ) ;
#28096 = CARTESIAN_POINT ( 'NONE',  ( 92.35000000000000853, -209.9999872712505180, 81.82437456149078514 ) ) ;
#28097 = CARTESIAN_POINT ( 'NONE',  ( 96.32499999999998863, -207.7050326799711968, 87.24833333333333485 ) ) ;
#28098 = AXIS2_PLACEMENT_3D ( 'NONE', #26078, #20812, #49006 ) ;
#28099 = ORIENTED_EDGE ( 'NONE', *, *, #31894, .T. ) ;
#28100 = CARTESIAN_POINT ( 'NONE',  ( -92.35000000000005116, 88.47002178664754979, 81.45395833506763950 ) ) ;
#28101 = ORIENTED_EDGE ( 'NONE', *, *, #50674, .F. ) ;
#28102 = ORIENTED_EDGE ( 'NONE', *, *, #8936, .F. ) ;
#28103 = FACE_OUTER_BOUND ( 'NONE', #28798, .T. ) ;
#28104 = SURFACE_SIDE_STYLE ('',( #32994 ) ) ;
#28105 = FACE_OUTER_BOUND ( 'NONE', #33383, .T. ) ;
#28106 = VERTEX_POINT ( 'NONE', #59592 ) ;
#28107 = DIRECTION ( 'NONE',  ( 0.000000000000000000, 1.000000000000000000, 0.000000000000000000 ) ) ;
#28108 = CARTESIAN_POINT ( 'NONE',  ( 92.35000000000002274, -211.5299782133524502, 78.06729166840096923 ) ) ;
#28109 = CARTESIAN_POINT ( 'NONE',  ( 92.34999999999999432, 88.47002178664753558, 81.79791666666666572 ) ) ;
#28110 = ORIENTED_EDGE ( 'NONE', *, *, #53661, .T. ) ;
#28111 = CARTESIAN_POINT ( 'NONE',  ( 96.32499999999998863, -207.7050326799711968, 75.26270833506764291 ) ) ;
#28112 = EDGE_LOOP ( 'NONE', ( #8933, #66388, #40245, #2528 ) ) ;
#28113 = EDGE_CURVE ( 'NONE', #54110, #44982, #20477, .T. ) ;
#28114 = CARTESIAN_POINT ( 'NONE',  ( -92.34999999999999432, -209.9999999999999716, 82.77687500173431090 ) ) ;
#28115 = ADVANCED_FACE ( 'NONE', ( #66351 ), #20090, .T. ) ;
#28116 = AXIS2_PLACEMENT_3D ( 'NONE', #19440, #19070, #1830 ) ;
#28117 = ORIENTED_EDGE ( 'NONE', *, *, #29923, .F. ) ;
#28118 = CARTESIAN_POINT ( 'NONE',  ( -97.30629616937501680, 91.33154071421968467, 85.93864583420051417 ) ) ;
#28119 = CARTESIAN_POINT ( 'NONE',  ( 97.30629616937498838, 88.66845928578037217, 77.84239583420045960 ) ) ;
#28120 = ORIENTED_EDGE ( 'NONE', *, *, #59426, .F. ) ;
#28121 = CYLINDRICAL_SURFACE ( 'NONE', #69382, 77.49899999999999523 ) ;
#28122 = CARTESIAN_POINT ( 'NONE',  ( -3.000000000000000000, 23.50000000000000000, -1.500000000000001332 ) ) ;
#28123 = CARTESIAN_POINT ( 'NONE',  ( -26.50044424985128089, 0.001194404165032690894, -49.00000000000068923 ) ) ;
#28124 = DIRECTION ( 'NONE',  ( -1.000000000000000000, -0.000000000000000000, -0.000000000000000000 ) ) ;
#28125 = ORIENTED_EDGE ( 'NONE', *, *, #66151, .T. ) ;
#28126 = DIRECTION ( 'NONE',  ( 0.000000000000000000, -0.1045284632676578285, 0.9945218953682729568 ) ) ;
#28127 = CARTESIAN_POINT ( 'NONE',  ( -92.69370383062498320, -208.6684592857803011, 77.31322916753380525 ) ) ;
#28128 = AXIS2_PLACEMENT_3D ( 'NONE', #50754, #12381, #19136 ) ;
#28129 = ORIENTED_EDGE ( 'NONE', *, *, #33617, .T. ) ;
#28130 = ORIENTED_EDGE ( 'NONE', *, *, #5904, .T. ) ;
#28131 = CARTESIAN_POINT ( 'NONE',  ( 97.64999999999997726, 88.47002178664752137, 80.10458333333330927 ) ) ;
#28132 = ORIENTED_EDGE ( 'NONE', *, *, #58838, .F. ) ;
#28133 = CARTESIAN_POINT ( 'NONE',  ( 92.34999999999999432, 90.00000000000002842, 77.93499999999998806 ) ) ;
#28134 = AXIS2_PLACEMENT_3D ( 'NONE', #48444, #65743, #15722 ) ;
#28135 = CARTESIAN_POINT ( 'NONE',  ( -94.99999999999997158, -213.0599564267049857, 78.09374999999998579 ) ) ;
#28136 = ORIENTED_EDGE ( 'NONE', *, *, #46587, .F. ) ;
#28137 = CARTESIAN_POINT ( 'NONE',  ( -96.15314808468747287, -208.0026889286704943, 89.69572916753382685 ) ) ;
#28138 = EDGE_LOOP ( 'NONE', ( #28238, #71644, #13256, #11937 ) ) ;
#28139 = VECTOR ( 'NONE', #46669, 1000.000000000000000 ) ;
#28140 = CARTESIAN_POINT ( 'NONE',  ( -92.35000000000003695, 90.00000000000004263, 76.98250000000000171 ) ) ;
#28141 = DIRECTION ( 'NONE',  ( -1.000000000000000000, -0.000000000000000000, 0.000000000000000000 ) ) ;
#28142 = CARTESIAN_POINT ( 'NONE',  ( 23.41451323550360186, -132.5004227906269989, 5.500000000000000000 ) ) ;
#28143 = CARTESIAN_POINT ( 'NONE',  ( 10.00000000000000000, 0.000000000000000000, 0.000000000000000000 ) ) ;
#28144 = DIRECTION ( 'NONE',  ( -1.000000000000000000, -0.000000000000000000, -0.000000000000000000 ) ) ;
#28145 = AXIS2_PLACEMENT_3D ( 'NONE', #9853, #39546, #33513 ) ;
#28146 = VECTOR ( 'NONE', #12543, 1000.000000000000227 ) ;
#28147 = CARTESIAN_POINT ( 'NONE',  ( 5.000000000000000000, 31.52238457039599595, 27.75498641678753842 ) ) ;
#28148 = CARTESIAN_POINT ( 'NONE',  ( 96.15314808468748708, 88.00268892867053694, 86.04447916753380809 ) ) ;
#28149 = CARTESIAN_POINT ( 'NONE',  ( -93.07557990970624928, -211.8218417373838349, 75.00000000000000000 ) ) ;
#28150 = CARTESIAN_POINT ( 'NONE',  ( 0.000000000000000000, 0.000000000000000000, 0.000000000000000000 ) ) ;
#28151 = CIRCLE ( 'NONE', #30557, 15.99999999999999822 ) ;
#28152 = CARTESIAN_POINT ( 'NONE',  ( -95.00000000000002842, 90.00000000000004263, 90.00000000000000000 ) ) ;
#28153 = DIRECTION ( 'NONE',  ( 0.000000000000000000, 0.000000000000000000, -1.000000000000000000 ) ) ;
#28154 = DIRECTION ( 'NONE',  ( -1.000000000000000000, 0.000000000000000000, 0.000000000000000000 ) ) ;
#28155 = DIRECTION ( 'NONE',  ( -1.000000000000000000, -0.000000000000000000, 0.000000000000000000 ) ) ;
#28156 = CARTESIAN_POINT ( 'NONE',  ( 0.000000000000000000, -51.03279382321048985, -55.19960302592120627 ) ) ;
#28157 = AXIS2_PLACEMENT_3D ( 'NONE', #17280, #50742, #51119 ) ;
#28158 =( BOUNDED_CURVE ( )  B_SPLINE_CURVE ( 2, ( #71690, #20580, #61178, #43533, #38234, #26202, #66811 ),
 .UNSPECIFIED., .F., .F. ) 
 B_SPLINE_CURVE_WITH_KNOTS ( ( 3, 2, 2, 3 ),
 ( 0.1693384224419981210, 0.1763941385220586522, 0.1834499040629413158, 0.1905056698837213069 ),
 .UNSPECIFIED. ) 
 CURVE ( )  GEOMETRIC_REPRESENTATION_ITEM ( )  RATIONAL_B_SPLINE_CURVE ( ( 0.9999981216929102468, 0.8660263429445670402, 1.000000000000000000, 0.8660254037844387076, 1.000000000000000000, 0.8660254037844387076, 1.000000000000000000 ) ) 
 REPRESENTATION_ITEM ( '' )  );
#28159 = CARTESIAN_POINT ( 'NONE',  ( 0.000000000000000000, -75.11764819372145041, -2.946379043147127064 ) ) ;
#28160 = LINE ( 'NONE', #50345, #8834 ) ;
#28161 = CIRCLE ( 'NONE', #35366, 31.99999999999999289 ) ;
#28162 = EDGE_CURVE ( 'NONE', #38565, #13389, #25945, .T. ) ;
#28163 = CARTESIAN_POINT ( 'NONE',  ( -3.759344165985237129, 0.000000000000000000, 0.000000000000000000 ) ) ;
#28164 = CARTESIAN_POINT ( 'NONE',  ( -93.84685191531252713, 88.00268892867056536, 89.21947916753380525 ) ) ;
#28165 = DIRECTION ( 'NONE',  ( 0.000000000000000000, 0.000000000000000000, 1.000000000000000000 ) ) ;
#28166 = EDGE_CURVE ( 'NONE', #54291, #59733, #7731, .T. ) ;
#28167 = CARTESIAN_POINT ( 'NONE',  ( -96.32499999999996021, -212.2949673200287179, 83.75583333333332803 ) ) ;
#28168 = EDGE_CURVE ( 'NONE', #52333, #59827, #38506, .T. ) ;
#28169 = EDGE_CURVE ( 'NONE', #45064, #46185, #27378, .T. ) ;
#28170 = CARTESIAN_POINT ( 'NONE',  ( 92.34999999999999432, 90.00000000000002842, 85.55499999999999261 ) ) ;
#28171 = LINE ( 'NONE', #39468, #53903 ) ;
#28172 = DIRECTION ( 'NONE',  ( -1.000000000000000000, -0.000000000000000000, -0.000000000000000000 ) ) ;
#28173 = CARTESIAN_POINT ( 'NONE',  ( -96.32500000000001705, 87.70503267997129626, 77.48520833506763950 ) ) ;
#28174 = ADVANCED_FACE ( 'NONE', ( #33219 ), #5058, .F. ) ;
#28175 = VECTOR ( 'NONE', #71732, 1000.000000000000000 ) ;
#28176 = CARTESIAN_POINT ( 'NONE',  ( 95.00000000000000000, -212.6630814284392557, 85.51531250086713953 ) ) ;
#28177 = ORIENTED_EDGE ( 'NONE', *, *, #53240, .F. ) ;
#28178 = ORIENTED_EDGE ( 'NONE', *, *, #37797, .T. ) ;
#28179 = LINE ( 'NONE', #11619, #49984 ) ;
#28180 = ORIENTED_EDGE ( 'NONE', *, *, #3277, .F. ) ;
#28181 = EDGE_CURVE ( 'NONE', #25226, #20333, #63420, .T. ) ;
#28182 = DIRECTION ( 'NONE',  ( 0.000000000000000000, 0.000000000000000000, 1.000000000000000000 ) ) ;
#28183 = CARTESIAN_POINT ( 'NONE',  ( 96.15314808468748708, -208.0026889286704943, 78.63614583420047666 ) ) ;
#28184 = AXIS2_PLACEMENT_3D ( 'NONE', #51108, #22547, #68419 ) ;
#28186 = EDGE_LOOP ( 'NONE', ( #62486, #27831, #62917, #71149 ) ) ;
#28185 = EDGE_CURVE ( 'NONE', #60502, #58170, #57397, .T. ) ;
#28187 = VECTOR ( 'NONE', #24882, 1000.000000000000000 ) ;
#28188 = CARTESIAN_POINT ( 'NONE',  ( 93.84685191531249870, -208.0026889286704943, 82.71072916753381321 ) ) ;
#28189 = ORIENTED_EDGE ( 'NONE', *, *, #26838, .T. ) ;
#28190 = DIRECTION ( 'NONE',  ( -1.000000000000000000, 0.000000000000000000, 0.000000000000000000 ) ) ;
#28191 = ORIENTED_EDGE ( 'NONE', *, *, #66308, .T. ) ;
#28192 = EDGE_CURVE ( 'NONE', #1535, #47891, #23801, .T. ) ;
#28194 = ADVANCED_FACE ( 'NONE', ( #9926 ), #61818, .T. ) ;
#28193 = CIRCLE ( 'NONE', #3009, 16.00000000000000355 ) ;
#28195 = VERTEX_POINT ( 'NONE', #33974 ) ;
#28196 = LINE ( 'NONE', #67684, #22516 ) ;
#28197 = DIRECTION ( 'NONE',  ( -1.000000000000000000, 0.000000000000000000, 0.000000000000000000 ) ) ;
#28198 = ORIENTED_EDGE ( 'NONE', *, *, #67234, .F. ) ;
#28199 = CARTESIAN_POINT ( 'NONE',  ( 92.35000000000000853, -211.5299782133524218, 76.79729166840095900 ) ) ;
#28200 = CARTESIAN_POINT ( 'NONE',  ( 97.64999999999999147, -209.9999999999999716, 85.31687500173428873 ) ) ;
#28201 = ORIENTED_EDGE ( 'NONE', *, *, #38696, .T. ) ;
#28202 = CARTESIAN_POINT ( 'NONE',  ( -11.59999999999999787, 0.000000000000000000, 52.00000000000002132 ) ) ;
#28203 = EDGE_CURVE ( 'NONE', #37554, #973, #55426, .T. ) ;
#28204 = ORIENTED_EDGE ( 'NONE', *, *, #39675, .T. ) ;
#28205 = FACE_OUTER_BOUND ( 'NONE', #42785, .T. ) ;
#28206 = ORIENTED_EDGE ( 'NONE', *, *, #60393, .T. ) ;
#28207 = EDGE_CURVE ( 'NONE', #56010, #38741, #45446, .T. ) ;
#28208 = VERTEX_POINT ( 'NONE', #27199 ) ;
#28209 = ORIENTED_EDGE ( 'NONE', *, *, #53883, .F. ) ;
#28210 = CARTESIAN_POINT ( 'NONE',  ( 97.30629616937498838, -211.3315407142195852, 76.57239583420046358 ) ) ;
#28211 = DIRECTION ( 'NONE',  ( -1.000000000000000000, 0.000000000000000000, -0.000000000000000000 ) ) ;
#28212 = ORIENTED_EDGE ( 'NONE', *, *, #50607, .T. ) ;
#28213 = ORIENTED_EDGE ( 'NONE', *, *, #22776, .T. ) ;
#28214 = VECTOR ( 'NONE', #68585, 1000.000000000000000 ) ;
#28215 = EDGE_LOOP ( 'NONE', ( #16713, #24473, #61539, #69549 ) ) ;
#28216 = DIRECTION ( 'NONE',  ( 1.000000000000000000, 0.000000000000000000, 0.000000000000000000 ) ) ;
#28217 = CARTESIAN_POINT ( 'NONE',  ( -92.69370383062502583, 91.33154071421968467, 76.20197916753382117 ) ) ;
#28218 = ORIENTED_EDGE ( 'NONE', *, *, #12373, .T. ) ;
#28219 = CARTESIAN_POINT ( 'NONE',  ( 94.99999999999998579, 92.66308142843935514, 74.87906250086713555 ) ) ;
#28220 = EDGE_LOOP ( 'NONE', ( #15665, #49270, #56058, #51061 ) ) ;
#28221 = DIRECTION ( 'NONE',  ( 0.6575728627325955200, -0.7533909544171996098, 0.000000000000000000 ) ) ;
#28222 = CARTESIAN_POINT ( 'NONE',  ( -97.30629616937495996, -209.9999999999999716, 85.83281250086714920 ) ) ;
#28223 = VERTEX_POINT ( 'NONE', #56921 ) ;
#28224 = DIRECTION ( 'NONE',  ( 0.000000000000000000, 0.000000000000000000, 1.000000000000000000 ) ) ;
#28225 = PLANE ( 'NONE',  #50009 ) ;
#28226 = CARTESIAN_POINT ( 'NONE',  ( 95.00000000000000000, -206.9400435732949575, 87.93624999999998693 ) ) ;
#28227 = CARTESIAN_POINT ( 'NONE',  ( -92.69370383062498320, -208.6684592857803295, 77.31322916753380525 ) ) ;
#28228 = LINE ( 'NONE', #12054, #72252 ) ;
#28229 = CARTESIAN_POINT ( 'NONE',  ( 0.000000000000000000, -9.188173127307592836, 40.98264845739746676 ) ) ;
#28230 = VECTOR ( 'NONE', #39694, 1000.000000000000114 ) ;
#28231 = FACE_OUTER_BOUND ( 'NONE', #23327, .T. ) ;
#28232 = CARTESIAN_POINT ( 'NONE',  ( -97.65000000000007674, 91.52997821335250705, 76.61208333333333087 ) ) ;
#28233 = DIRECTION ( 'NONE',  ( 0.000000000000000000, -0.000000000000000000, -1.000000000000000000 ) ) ;
#28234 = CARTESIAN_POINT ( 'NONE',  ( -97.30629616937501680, 90.00000000000004263, 82.02281250086714692 ) ) ;
#28235 = DIRECTION ( 'NONE',  ( 0.000000000000000000, 0.000000000000000000, 1.000000000000000000 ) ) ;
#28236 = CARTESIAN_POINT ( 'NONE',  ( 0.000000000000000000, 38.55633173627010279, 16.65560815589424593 ) ) ;
#28237 = AXIS2_PLACEMENT_3D ( 'NONE', #9507, #67771, #59255 ) ;
#28238 = ORIENTED_EDGE ( 'NONE', *, *, #5612, .T. ) ;
#28239 = LINE ( 'NONE', #35006, #17204 ) ;
#28240 = EDGE_CURVE ( 'NONE', #40893, #56929, #67237, .T. ) ;
#28242 = CARTESIAN_POINT ( 'NONE',  ( 97.64999999999999147, -209.9999999999999716, 89.12687500173430521 ) ) ;
#28241 = AXIS2_PLACEMENT_3D ( 'NONE', #62703, #5918, #11168 ) ;
#28243 = CARTESIAN_POINT ( 'NONE',  ( 92.35000000000000853, -209.9999999999999716, 90.00000000000000000 ) ) ;
#28244 = EDGE_CURVE ( 'NONE', #232, #45393, #66987, .T. ) ;
#28245 = DIRECTION ( 'NONE',  ( 0.000000000000000000, 0.000000000000000000, -1.000000000000000000 ) ) ;
#28246 = CARTESIAN_POINT ( 'NONE',  ( -94.99999999999997158, -212.6630814284392557, 79.80031250086715033 ) ) ;
#28247 = VECTOR ( 'NONE', #58953, 1000.000000000000000 ) ;
#28248 = EDGE_CURVE ( 'NONE', #53818, #63724, #15938, .T. ) ;
#28249 = ADVANCED_FACE ( 'NONE', ( #58386 ), #29070, .F. ) ;
#28250 = CARTESIAN_POINT ( 'NONE',  ( 10.00000000000000000, 0.000000000000000000, 0.000000000000000000 ) ) ;
#28251 = ORIENTED_EDGE ( 'NONE', *, *, #70165, .F. ) ;
#28252 = DIRECTION ( 'NONE',  ( 0.000000000000000000, 0.5877852522924741363, -0.8090169943749465631 ) ) ;
#28253 = CIRCLE ( 'NONE', #4140, 16.00000000000000000 ) ;
#28254 = CARTESIAN_POINT ( 'NONE',  ( -97.65000000000001990, 90.00000000000004263, 80.55437500173430010 ) ) ;
#28255 = DIRECTION ( 'NONE',  ( 0.000000000000000000, 0.7071067811865489050, -0.7071067811865462405 ) ) ;
#28256 = CARTESIAN_POINT ( 'NONE',  ( -97.64999999980587120, -210.0000198427943587, 86.27002759516035724 ) ) ;
#28257 = DIRECTION ( 'NONE',  ( -1.000000000000000000, 0.000000000000000000, 0.000000000000000000 ) ) ;
#28258 = MECHANICAL_DESIGN_GEOMETRIC_PRESENTATION_REPRESENTATION (  '', ( #10299 ), #51128 ) ;
#28259 = EDGE_CURVE ( 'NONE', #12497, #27167, #64631, .T. ) ;
#28260 = CARTESIAN_POINT ( 'NONE',  ( 10.00000000000000000, 0.000000000000000000, 0.000000000000000000 ) ) ;
#28261 = ADVANCED_FACE ( 'NONE', ( #23807 ), #40358, .T. ) ;
#28262 = VERTEX_POINT ( 'NONE', #17064 ) ;
#28263 = LINE ( 'NONE', #46679, #72054 ) ;
#28264 = DIRECTION ( 'NONE',  ( -0.000000000000000000, -0.000000000000000000, 1.000000000000000000 ) ) ;
#28265 = ORIENTED_EDGE ( 'NONE', *, *, #16228, .T. ) ;
#28266 = CARTESIAN_POINT ( 'NONE',  ( 97.30629616937498838, -208.6684592857803295, 86.83822916753381094 ) ) ;
#28267 = LINE ( 'NONE', #69611, #41874 ) ;
#28268 = ORIENTED_EDGE ( 'NONE', *, *, #19489, .F. ) ;
#28269 = EDGE_LOOP ( 'NONE', ( #68893, #17297, #66643, #38658 ) ) ;
#28270 = CARTESIAN_POINT ( 'NONE',  ( 6.782329983125267248, 10.49999999999999645, -105.0000000000000000 ) ) ;
#28271 = ORIENTED_EDGE ( 'NONE', *, *, #34368, .F. ) ;
#28272 = EDGE_CURVE ( 'NONE', #49986, #67800, #47122, .T. ) ;
#28273 = EDGE_CURVE ( 'NONE', #68894, #32156, #70022, .T. ) ;
#28274 = CARTESIAN_POINT ( 'NONE',  ( 95.00000000000000000, -213.0599564267049857, 81.90375000000000227 ) ) ;
#28275 = ORIENTED_EDGE ( 'NONE', *, *, #6484, .T. ) ;
#28276 = CARTESIAN_POINT ( 'NONE',  ( -92.34999999999999432, -209.9999999999999716, 75.07749999999998636 ) ) ;
#28277 = ORIENTED_EDGE ( 'NONE', *, *, #36405, .F. ) ;
#28278 = VERTEX_POINT ( 'NONE', #64408 ) ;
#28279 = CARTESIAN_POINT ( 'NONE',  ( -3.000000000000000000, -3.948201729842348850, 23.21447184625293048 ) ) ;
#28280 = EDGE_LOOP ( 'NONE', ( #51411, #53950, #5424, #73049 ) ) ;
#28281 = EDGE_LOOP ( 'NONE', ( #30504, #40689, #60412, #18895 ) ) ;
#28282 = CARTESIAN_POINT ( 'NONE',  ( 94.99999999999998579, 86.94004357329500010, 89.52375000000000682 ) ) ;
#28283 = CYLINDRICAL_SURFACE ( 'NONE', #60004, 2.649999999999999467 ) ;
#28285 = CARTESIAN_POINT ( 'NONE',  ( 10.00000000000000000, 0.8261519478431083030, 77.49459641780886443 ) ) ;
#28284 = AXIS2_PLACEMENT_3D ( 'NONE', #27282, #16770, #11486 ) ;
#28286 = VERTEX_POINT ( 'NONE', #23081 ) ;
#28287 = ORIENTED_EDGE ( 'NONE', *, *, #72987, .F. ) ;
#28288 = ORIENTED_EDGE ( 'NONE', *, *, #869, .F. ) ;
#28289 = CARTESIAN_POINT ( 'NONE',  ( 93.84685191531248449, 91.99731107132950569, 83.82197916753381151 ) ) ;
#28290 = EDGE_LOOP ( 'NONE', ( #58699, #32897, #40210, #7405 ) ) ;
#28291 = AXIS2_PLACEMENT_3D ( 'NONE', #20061, #36251, #59192 ) ;
#28292 = CARTESIAN_POINT ( 'NONE',  ( 97.30629616937498838, -208.6684592857803011, 84.93322916753379559 ) ) ;
#28293 = CARTESIAN_POINT ( 'NONE',  ( 0.000000000000000000, -26.01480285779885904, 70.53064760720306481 ) ) ;
#28294 = CARTESIAN_POINT ( 'NONE',  ( 23.49916127795269105, -121.5130826919798039, -2.500000000000000000 ) ) ;
#28295 = CIRCLE ( 'NONE', #19920, 16.00000000000000000 ) ;
#28296 = CARTESIAN_POINT ( 'NONE',  ( 0.000000000000000000, -25.88420570971381807, -27.13269053701123212 ) ) ;
#28297 = CARTESIAN_POINT ( 'NONE',  ( -92.34999999999999432, -209.9999999999999716, 89.04749999999999943 ) ) ;
#28298 = AXIS2_PLACEMENT_3D ( 'NONE', #8918, #72063, #66441 ) ;
#28299 = LINE ( 'NONE', #58359, #68477 ) ;
#28300 = CARTESIAN_POINT ( 'NONE',  ( -10.00000000000000000, 0.000000000000000000, 0.000000000000000000 ) ) ;
#28301 = CARTESIAN_POINT ( 'NONE',  ( -96.15314808468747287, -208.0026889286704943, 86.99697916753380866 ) ) ;
#28302 = CARTESIAN_POINT ( 'NONE',  ( -92.69370383062504004, 90.00000000000004263, 85.67406250086715147 ) ) ;
#28303 = ORIENTED_EDGE ( 'NONE', *, *, #8676, .T. ) ;
#28304 = VECTOR ( 'NONE', #43791, 1000.000000000000000 ) ;
#28306 = CARTESIAN_POINT ( 'NONE',  ( -97.30629616937501680, 91.33154071421968467, 83.87489583420047268 ) ) ;
#28305 = CARTESIAN_POINT ( 'NONE',  ( 94.99999999999998579, 87.33691857156068750, 82.81656250086713555 ) ) ;
#28307 = CIRCLE ( 'NONE', #47527, 31.99999999999998224 ) ;
#28308 = ORIENTED_EDGE ( 'NONE', *, *, #63262, .T. ) ;
#28309 = DIRECTION ( 'NONE',  ( -1.000000000000000000, -0.000000000000000000, 0.000000000000000000 ) ) ;
#28310 = DIRECTION ( 'NONE',  ( 1.000000000000000000, 0.000000000000000000, 0.000000000000000000 ) ) ;
#28311 = CARTESIAN_POINT ( 'NONE',  ( -20.63750000000001350, -1.626958204894327051E-13, -12.50000000000024158 ) ) ;
#28312 = CARTESIAN_POINT ( 'NONE',  ( 97.64999999999999147, 90.00000000000002842, 87.14249999999999829 ) ) ;
#28313 = FACE_OUTER_BOUND ( 'NONE', #48008, .T. ) ;
#28314 = CARTESIAN_POINT ( 'NONE',  ( 0.000000000000000000, 59.46389618802034960, -49.70050353004825894 ) ) ;
#28315 = LINE ( 'NONE', #72331, #38568 ) ;
#28316 = CYLINDRICAL_SURFACE ( 'NONE', #34326, 42.00000000000000000 ) ;
#28317 = DIRECTION ( 'NONE',  ( -1.000000000000000000, 0.000000000000000000, 0.000000000000000000 ) ) ;
#28318 = VERTEX_POINT ( 'NONE', #1298 ) ;
#28319 = STYLED_ITEM ( 'NONE', ( #53891 ), #37419 ) ;
#28320 = EDGE_LOOP ( 'NONE', ( #44866, #48542, #45347, #19599 ) ) ;
#28321 = CARTESIAN_POINT ( 'NONE',  ( -96.32500000000001705, 87.70503267997129626, 78.04083333333333883 ) ) ;
#28322 = LINE ( 'NONE', #21951, #61973 ) ;
#28323 = DIRECTION ( 'NONE',  ( 0.000000000000000000, -0.5877852522924802425, 0.8090169943749422332 ) ) ;
#28324 = CARTESIAN_POINT ( 'NONE',  ( 1.952604744559289694E-12, 0.000000000000000000, -75.00000000000000000 ) ) ;
#28325 = CARTESIAN_POINT ( 'NONE',  ( -93.67499999999998295, -207.7050326799711968, 89.78833333333332689 ) ) ;
#28326 = DIRECTION ( 'NONE',  ( -1.000000000000000000, 0.000000000000000000, -0.000000000000000000 ) ) ;
#28327 = CYLINDRICAL_SURFACE ( 'NONE', #25238, 12.49999999999999645 ) ;
#28328 = ORIENTED_EDGE ( 'NONE', *, *, #19536, .F. ) ;
#28329 = CARTESIAN_POINT ( 'NONE',  ( -96.15314808468752972, 91.99731107132950569, 78.10697916753380809 ) ) ;
#28330 = EDGE_CURVE ( 'NONE', #18041, #15423, #74196, .T. ) ;
#28331 = DIRECTION ( 'NONE',  ( 0.000000000000000000, -1.000000000000000000, -2.312964634635746211E-15 ) ) ;
#28332 = ADVANCED_BREP_SHAPE_REPRESENTATION ( '', ( #37782, #43395 ), #7372 ) ;
#28333 = EDGE_CURVE ( 'NONE', #71434, #26872, #11409, .T. ) ;
#28334 = DIRECTION ( 'NONE',  ( -1.000000000000000000, 0.000000000000000000, 0.000000000000000000 ) ) ;
#28335 = DIRECTION ( 'NONE',  ( 0.000000000000000000, 0.9781476007338041345, 0.2079116908177664480 ) ) ;
#28336 = EDGE_CURVE ( 'NONE', #51303, #237, #4605, .T. ) ;
#28337 = CARTESIAN_POINT ( 'NONE',  ( 10.00000000000000000, 0.000000000000000000, 0.000000000000000000 ) ) ;
#28338 = CARTESIAN_POINT ( 'NONE',  ( -97.65000000000001990, 91.52997821335253548, 82.32708333333334849 ) ) ;
#28339 = CARTESIAN_POINT ( 'NONE',  ( -94.99999999999997158, -207.3369185715606307, 89.00781250086716057 ) ) ;
#28340 = SHAPE_REPRESENTATION_RELATIONSHIP ( 'NONE' , 'NONE' ,  #66992, #68699 ) ;
#28341 = EDGE_CURVE ( 'NONE', #58950, #21877, #71801, .T. ) ;
#28342 = EDGE_CURVE ( 'NONE', #62549, #37645, #41827, .T. ) ;
#28343 = CIRCLE ( 'NONE', #7949, 42.00000000000000000 ) ;
#28344 = CARTESIAN_POINT ( 'NONE',  ( 97.30629616937498838, 90.00000000000002842, 78.05406250086716113 ) ) ;
#28345 = CARTESIAN_POINT ( 'NONE',  ( -96.15314808468745866, -211.9973110713294489, 78.47739583420049314 ) ) ;
#28346 = LINE ( 'NONE', #27977, #43472 ) ;
#28347 = VERTEX_POINT ( 'NONE', #35454 ) ;
#28348 = CARTESIAN_POINT ( 'NONE',  ( -97.64999999996715019, 90.00000839192523472, 86.90410584365564262 ) ) ;
#28349 = FACE_OUTER_BOUND ( 'NONE', #3367, .T. ) ;
#28350 = CARTESIAN_POINT ( 'NONE',  ( 10.00000000000000000, -36.88895765772628010, -6.736453364083947015 ) ) ;
#28351 = AXIS2_PLACEMENT_3D ( 'NONE', #57503, #12724, #18367 ) ;
#28352 = CIRCLE ( 'NONE', #31946, 31.99999999999999645 ) ;
#28353 = CARTESIAN_POINT ( 'NONE',  ( -95.00000000000002842, 87.33691857156074434, 79.80031250086715033 ) ) ;
#28355 = ADVANCED_FACE ( 'NONE', ( #68573 ), #62952, .F. ) ;
#28354 = CARTESIAN_POINT ( 'NONE',  ( 96.15314808468750130, -211.9973110713294489, 80.32947916753380468 ) ) ;
#28356 = ORIENTED_EDGE ( 'NONE', *, *, #47229, .T. ) ;
#28357 = EDGE_CURVE ( 'NONE', #3072, #72829, #53784, .T. ) ;
#28358 = AXIS2_PLACEMENT_3D ( 'NONE', #2024, #54239, #24909 ) ;
#28359 = DIRECTION ( 'NONE',  ( -1.000000000000000000, 0.000000000000000000, 0.000000000000000000 ) ) ;
#28360 = ORIENTED_EDGE ( 'NONE', *, *, #12544, .F. ) ;
#28361 = VECTOR ( 'NONE', #71403, 1000.000000000000000 ) ;
#28362 =( BOUNDED_CURVE ( )  B_SPLINE_CURVE ( 2, ( #52198, #22531, #10878, #745, #28902, #23634, #45847, #56752, #5996 ),
 .UNSPECIFIED., .F., .F. ) 
 B_SPLINE_CURVE_WITH_KNOTS ( ( 3, 2, 2, 2, 3 ),
 ( 0.1058364832022827828, 0.1128922486541179687, 0.1199480141950002993, 0.1270037797358826437, 0.1270039290051390157 ),
 .UNSPECIFIED. ) 
 CURVE ( )  GEOMETRIC_REPRESENTATION_ITEM ( )  RATIONAL_B_SPLINE_CURVE ( ( 1.000000000000000000, 0.8660254037844387076, 1.000000000000000000, 0.8660254037844387076, 1.000000000000000000, 0.8660254037844387076, 1.000000000000000000, 0.9999971656812808307, 0.9999943314824852880 ) ) 
 REPRESENTATION_ITEM ( '' )  );
#28363 = CARTESIAN_POINT ( 'NONE',  ( 10.00000000000000000, 0.000000000000000000, 0.000000000000000000 ) ) ;
#28364 = ORIENTED_EDGE ( 'NONE', *, *, #19872, .F. ) ;
#28365 = CARTESIAN_POINT ( 'NONE',  ( -97.65000000000001990, 90.00000000000004263, 79.20499999999999829 ) ) ;
#28366 = EDGE_CURVE ( 'NONE', #55652, #9807, #2935, .T. ) ;
#28367 = EDGE_CURVE ( 'NONE', #6700, #10235, #5785, .T. ) ;
#28368 = VECTOR ( 'NONE', #14676, 1000.000000000000000 ) ;
#28369 = VERTEX_POINT ( 'NONE', #7264 ) ;
#28370 = EDGE_LOOP ( 'NONE', ( #23936, #69220, #50376, #29299 ) ) ;
#28371 = EDGE_LOOP ( 'NONE', ( #66116, #73531, #570 ) ) ;
#28372 = CARTESIAN_POINT ( 'NONE',  ( 93.84685191531251292, -211.9973110713294489, 75.30239583420048177 ) ) ;
#28373 = ORIENTED_EDGE ( 'NONE', *, *, #49829, .T. ) ;
#28374 = DIRECTION ( 'NONE',  ( 0.000000000000000000, 0.7071067811865436870, 0.7071067811865513475 ) ) ;
#28375 = CARTESIAN_POINT ( 'NONE',  ( -3.961125083139900749, -143.2122702051246677, 5.500000000000000000 ) ) ;
#28376 = CARTESIAN_POINT ( 'NONE',  ( 93.84685191531248449, 91.99731107132950569, 82.71072916753381321 ) ) ;
#28377 = CARTESIAN_POINT ( 'NONE',  ( 92.35000000000002274, -211.5299782133524502, 78.62291666666668277 ) ) ;
#28378 = EDGE_LOOP ( 'NONE', ( #57201, #69827, #37810, #66663 ) ) ;
#28379 = VERTEX_POINT ( 'NONE', #18890 ) ;
#28380 = ORIENTED_EDGE ( 'NONE', *, *, #18339, .F. ) ;
#28381 = ORIENTED_EDGE ( 'NONE', *, *, #36505, .T. ) ;
#28382 = DIRECTION ( 'NONE',  ( 0.6064928550163531940, 0.7950889364178782559, 0.000000000000000000 ) ) ;
#28383 = DIRECTION ( 'NONE',  ( 0.000000000000000000, 0.1564344650402313408, -0.9876883405951376593 ) ) ;
#28384 = DIRECTION ( 'NONE',  ( -0.000000000000000000, -0.000000000000000000, 1.000000000000000000 ) ) ;
#28385 = CARTESIAN_POINT ( 'NONE',  ( 26.47460221209471598, -121.8961639463267090, 5.500000000000000000 ) ) ;
#28386 = CARTESIAN_POINT ( 'NONE',  ( 6.000000000000000000, -71.87247863392384772, -39.47590169984923136 ) ) ;
#28387 = DIRECTION ( 'NONE',  ( 0.000000000000000000, -0.8910065241883626808, -0.4539904997395570740 ) ) ;
#28388 = ORIENTED_EDGE ( 'NONE', *, *, #38944, .T. ) ;
#28389 = CARTESIAN_POINT ( 'NONE',  ( -92.34999999999999432, -209.9999999999999716, 83.41187500173430180 ) ) ;
#28390 = ORIENTED_EDGE ( 'NONE', *, *, #5299, .F. ) ;
#28391 = DIRECTION ( 'NONE',  ( -1.000000000000000000, 0.000000000000000000, 0.000000000000000000 ) ) ;
#28392 = ORIENTED_EDGE ( 'NONE', *, *, #53043, .T. ) ;
#28394 = CARTESIAN_POINT ( 'NONE',  ( -96.32500000000001705, 92.29496732002878900, 80.44854166840097776 ) ) ;
#28393 = CARTESIAN_POINT ( 'NONE',  ( 93.67499999999998295, 92.29496732002878900, 79.17854166840096752 ) ) ;
#28395 = VERTEX_POINT ( 'NONE', #47482 ) ;
#28396 = CARTESIAN_POINT ( 'NONE',  ( 97.30629616937498838, 91.33154071421968467, 85.09197916753380753 ) ) ;
#28397 = CIRCLE ( 'NONE', #70398, 11.59999999999999787 ) ;
#28398 = DIRECTION ( 'NONE',  ( 1.000000000000000000, 0.000000000000000000, 0.000000000000000000 ) ) ;
#28400 = EDGE_CURVE ( 'NONE', #27944, #5496, #32203, .T. ) ;
#28399 = DIRECTION ( 'NONE',  ( -0.000000000000000000, -0.000000000000000000, 1.000000000000000000 ) ) ;
#28401 = FACE_OUTER_BOUND ( 'NONE', #17464, .T. ) ;
#28402 = CARTESIAN_POINT ( 'NONE',  ( 6.250000000000005329, 0.000000000000000000, 0.000000000000000000 ) ) ;
#28403 = CARTESIAN_POINT ( 'NONE',  ( 15.00000000000000000, -18.13022148937263012, -15.02647892043543898 ) ) ;
#28404 = ORIENTED_EDGE ( 'NONE', *, *, #5984, .F. ) ;
#28405 = DIRECTION ( 'NONE',  ( 0.000000000000000000, 0.000000000000000000, -1.000000000000000000 ) ) ;
#28406 = CARTESIAN_POINT ( 'NONE',  ( 97.64999999981932888, -210.0000309431867436, 78.33187387208516839 ) ) ;
#28407 = DIRECTION ( 'NONE',  ( 0.000000000000000000, -0.5877852522924801315, 0.8090169943749421222 ) ) ;
#28408 = VERTEX_POINT ( 'NONE', #13625 ) ;
#28409 = VECTOR ( 'NONE', #55830, 1000.000000000000000 ) ;
#28410 = ORIENTED_EDGE ( 'NONE', *, *, #1235, .F. ) ;
#28411 = EDGE_CURVE ( 'NONE', #61965, #32631, #16601, .T. ) ;
#28412 = VECTOR ( 'NONE', #32545, 1000.000000000000000 ) ;
#28413 = CARTESIAN_POINT ( 'NONE',  ( 11.99999999999999822, -50.23322058963300663, -64.81221759200398935 ) ) ;
#28414 = EDGE_CURVE ( 'NONE', #2800, #64355, #59883, .T. ) ;
#28415 = PRODUCT_DEFINITION_SHAPE ( 'NONE', 'NONE',  #74355 ) ;
#28416 = CARTESIAN_POINT ( 'NONE',  ( 0.000000000000000000, 64.81221759200417409, -50.23322058963276504 ) ) ;
#28417 = AXIS2_PLACEMENT_3D ( 'NONE', #66537, #50714, #32671 ) ;
#28418 = FACE_OUTER_BOUND ( 'NONE', #62049, .T. ) ;
#28419 = PLANE ( 'NONE',  #40148 ) ;
#28420 = CARTESIAN_POINT ( 'NONE',  ( -97.30629616937497417, -208.6684592857803011, 82.12864583420048348 ) ) ;
#28421 = ORIENTED_EDGE ( 'NONE', *, *, #7586, .T. ) ;
#28422 = VERTEX_POINT ( 'NONE', #13263 ) ;
#28423 = EDGE_CURVE ( 'NONE', #38008, #46993, #42224, .T. ) ;
#28424 = CARTESIAN_POINT ( 'NONE',  ( 11.99999999999999822, 0.000000000000000000, 0.000000000000000000 ) ) ;
#28425 = CARTESIAN_POINT ( 'NONE',  ( -94.95306897617061281, -212.6495843973424655, 75.00000002508416230 ) ) ;
#28426 = STYLED_ITEM ( 'NONE', ( #30391 ), #38137 ) ;
#28427 = DIRECTION ( 'NONE',  ( 0.000000000000000000, 0.4067366430757989870, 0.9135454576426015327 ) ) ;
#28428 = CARTESIAN_POINT ( 'NONE',  ( 94.99999999999998579, 92.66308142843932671, 75.51406250086714067 ) ) ;
#28429 = CARTESIAN_POINT ( 'NONE',  ( 0.000000000000000000, 0.000000000000000000, -184.9999999999999432 ) ) ;
#28430 = DIRECTION ( 'NONE',  ( -1.000000000000000000, -0.000000000000000000, -0.000000000000000000 ) ) ;
#28431 = CARTESIAN_POINT ( 'NONE',  ( -7.469491406282094736, 4.756046723998911929, 32.98187577049606745 ) ) ;
#28432 = CARTESIAN_POINT ( 'NONE',  ( -97.64999999960622290, -209.9999706925929672, 76.74344264316562203 ) ) ;
#28433 = CARTESIAN_POINT ( 'NONE',  ( -92.35000000000003695, 89.99999997442942856, 84.04687500080852658 ) ) ;
#28434 = AXIS2_PLACEMENT_3D ( 'NONE', #51947, #35035, #45960 ) ;
#28435 = CARTESIAN_POINT ( 'NONE',  ( 10.00000000000000000, 0.000000000000000000, 0.000000000000000000 ) ) ;
#28436 = EDGE_CURVE ( 'NONE', #41131, #54917, #53490, .T. ) ;
#28437 = CARTESIAN_POINT ( 'NONE',  ( 96.15314808468748708, 88.00268892867053694, 87.47322916753381605 ) ) ;
#28438 = CARTESIAN_POINT ( 'NONE',  ( -97.30629616937495996, -209.9999999999999716, 89.80156250086714920 ) ) ;
#28439 = CARTESIAN_POINT ( 'NONE',  ( 11.99999999999999822, 77.49459641780886443, -0.8261519478433960728 ) ) ;
#28440 = ORIENTED_EDGE ( 'NONE', *, *, #26389, .F. ) ;
#28441 = DIRECTION ( 'NONE',  ( -1.000000000000000000, 0.000000000000000000, 0.000000000000000000 ) ) ;
#28442 = CARTESIAN_POINT ( 'NONE',  ( -93.84685191531252713, 88.00268892867056536, 79.05947916753380866 ) ) ;
#28444 = EDGE_CURVE ( 'NONE', #44775, #4487, #59137, .T. ) ;
#28443 = LINE ( 'NONE', #67568, #60996 ) ;
#28445 = EDGE_CURVE ( 'NONE', #57981, #14321, #39426, .T. ) ;
#28446 = VERTEX_POINT ( 'NONE', #24544 ) ;
#28447 = CARTESIAN_POINT ( 'NONE',  ( 93.67500000000001137, -212.2949673200287179, 80.02520833506763154 ) ) ;
#28448 = ADVANCED_FACE ( 'NONE', ( #70767 ), #59506, .T. ) ;
#28449 = CARTESIAN_POINT ( 'NONE',  ( 97.64999999999999147, 90.00000000000002842, 83.33250000000001023 ) ) ;
#28450 = AXIS2_PLACEMENT_3D ( 'NONE', #5, #23999, #51443 ) ;
#28451 = CARTESIAN_POINT ( 'NONE',  ( 10.00000000000000000, 31.46837873494978055, 68.27212725128286763 ) ) ;
#28452 = AXIS2_PLACEMENT_3D ( 'NONE', #19588, #9055, #24868 ) ;
#28453 = CARTESIAN_POINT ( 'NONE',  ( 95.00000000000000000, -207.3369185715606307, 76.94281250086714863 ) ) ;
#28454 = VECTOR ( 'NONE', #20737, 1000.000000000000000 ) ;
#28455 = ORIENTED_EDGE ( 'NONE', *, *, #70849, .T. ) ;
#28456 = AXIS2_PLACEMENT_3D ( 'NONE', #35549, #58482, #64502 ) ;
#28457 = ORIENTED_EDGE ( 'NONE', *, *, #3403, .F. ) ;
#28458 = CARTESIAN_POINT ( 'NONE',  ( 92.69370383062501162, -208.6684592857803295, 85.93864583420051417 ) ) ;
#28459 = DIRECTION ( 'NONE',  ( 0.000000000000000000, 0.000000000000000000, 1.000000000000000000 ) ) ;
#28460 = CARTESIAN_POINT ( 'NONE',  ( 0.000000000000000000, 0.000000000000000000, -43.79999999999998295 ) ) ;
#28461 = DIRECTION ( 'NONE',  ( -1.000000000000000000, -0.000000000000000000, 0.000000000000000000 ) ) ;
#28462 = DIRECTION ( 'NONE',  ( 1.000000000000000000, 0.000000000000000000, 0.000000000000000000 ) ) ;
#28463 = CARTESIAN_POINT ( 'NONE',  ( 6.000000000000000000, 3.894527615417885169, 81.90746397400390322 ) ) ;
#28464 = CARTESIAN_POINT ( 'NONE',  ( 95.00000000000000000, -206.9400435732949575, 88.57124999999999204 ) ) ;
#28465 = ORIENTED_EDGE ( 'NONE', *, *, #16824, .T. ) ;
#28466 = VERTEX_POINT ( 'NONE', #30910 ) ;
#28467 = VERTEX_POINT ( 'NONE', #1661 ) ;
#28468 = ORIENTED_EDGE ( 'NONE', *, *, #18815, .F. ) ;
#28469 = CARTESIAN_POINT ( 'NONE',  ( 10.00000000000000000, -65.58780272294048075, -36.73666225445966660 ) ) ;
#28470 = CARTESIAN_POINT ( 'NONE',  ( 2.925285743277526329, 4.084588180558403891, -5.989444439476610427 ) ) ;
#28471 = DIRECTION ( 'NONE',  ( -1.000000000000000000, -0.000000000000000000, -0.000000000000000000 ) ) ;
#28472 = CARTESIAN_POINT ( 'NONE',  ( 95.00000000000000000, -213.0599564267049857, 78.17312500173430578 ) ) ;
#28473 = CARTESIAN_POINT ( 'NONE',  ( 92.34999999999999432, 90.00000000000002842, 83.01499999999998636 ) ) ;
#28474 = VECTOR ( 'NONE', #43940, 1000.000000000000000 ) ;
#28475 = VERTEX_POINT ( 'NONE', #2404 ) ;
#28476 = DIRECTION ( 'NONE',  ( 2.603472992746261562E-14, 2.546204323184492723E-14, -1.000000000000000000 ) ) ;
#28477 = EDGE_CURVE ( 'NONE', #45442, #13480, #40597, .T. ) ;
#28478 = ORIENTED_EDGE ( 'NONE', *, *, #69812, .F. ) ;
#28479 = DIRECTION ( 'NONE',  ( -0.000000000000000000, -0.000000000000000000, 1.000000000000000000 ) ) ;
#28480 = VERTEX_POINT ( 'NONE', #26017 ) ;
#28481 = PLANE ( 'NONE',  #6815 ) ;
#28482 = CARTESIAN_POINT ( 'NONE',  ( -97.30629616937501680, 88.66845928578038638, 80.32947916753381890 ) ) ;
#28483 = CARTESIAN_POINT ( 'NONE',  ( 97.30629616937498838, 90.00000000000002842, 77.89531250086714920 ) ) ;
#28484 = ORIENTED_EDGE ( 'NONE', *, *, #73943, .T. ) ;
#28485 = CARTESIAN_POINT ( 'NONE',  ( 11.99999999999999822, 0.000000000000000000, 0.000000000000000000 ) ) ;
#28486 = CARTESIAN_POINT ( 'NONE',  ( 10.00000000000000000, 0.000000000000000000, 0.000000000000000000 ) ) ;
#28487 = DIRECTION ( 'NONE',  ( -1.000000000000000000, 0.000000000000000000, 0.000000000000000000 ) ) ;
#28488 = DIRECTION ( 'NONE',  ( 0.000000000000000000, -0.8910065241883722287, 0.4539904997395383668 ) ) ;
#28489 = ORIENTED_EDGE ( 'NONE', *, *, #169, .T. ) ;
#28490 = DIRECTION ( 'NONE',  ( 0.000000000000000000, 0.5224985647159440250, 0.8526401643540951758 ) ) ;
#28491 = CARTESIAN_POINT ( 'NONE',  ( -97.30629616937497417, -208.6684592857803011, 78.15989583420048348 ) ) ;
#28492 = ORIENTED_EDGE ( 'NONE', *, *, #20258, .F. ) ;
#28493 = ORIENTED_EDGE ( 'NONE', *, *, #17389, .F. ) ;
#28494 = EDGE_CURVE ( 'NONE', #44032, #6380, #41835, .T. ) ;
#28495 = FACE_BOUND ( 'NONE', #6581, .T. ) ;
#28496 = EDGE_CURVE ( 'NONE', #38411, #12079, #64781, .T. ) ;
#28497 = ORIENTED_EDGE ( 'NONE', *, *, #33699, .T. ) ;
#28498 = DIRECTION ( 'NONE',  ( -1.000000000000000000, 0.000000000000000000, 0.000000000000000000 ) ) ;
#28499 = DIRECTION ( 'NONE',  ( 1.000000000000000000, 0.000000000000000000, 0.000000000000000000 ) ) ;
#28500 = EDGE_LOOP ( 'NONE', ( #15428, #33031, #20691, #8917 ) ) ;
#28501 = CARTESIAN_POINT ( 'NONE',  ( -94.99999999999997158, -207.3369185715606307, 76.14906250086716000 ) ) ;
#28502 = ORIENTED_EDGE ( 'NONE', *, *, #9367, .T. ) ;
#28503 = CARTESIAN_POINT ( 'NONE',  ( 0.000000000000000000, 0.000000000000000000, 0.000000000000000000 ) ) ;
#28504 = CARTESIAN_POINT ( 'NONE',  ( 11.99999999999999822, 22.90783923731740401, -78.73519480814930205 ) ) ;
#28505 = LINE ( 'NONE', #33398, #74189 ) ;
#28506 = CARTESIAN_POINT ( 'NONE',  ( 11.99999999999999822, 14.66109333815564852, -73.73191006444555740 ) ) ;
#28507 = AXIS2_PLACEMENT_3D ( 'NONE', #28570, #51516, #40240 ) ;
#28508 = EDGE_CURVE ( 'NONE', #57225, #32534, #9396, .T. ) ;
#28509 = EDGE_CURVE ( 'NONE', #30261, #1192, #19009, .T. ) ;
#28510 = PLANE ( 'NONE',  #61857 ) ;
#28511 = CIRCLE ( 'NONE', #70508, 1.000000000000000000 ) ;
#28512 = CARTESIAN_POINT ( 'NONE',  ( 12.00000000000000000, 18.84667830672579925, -18.68964196561269375 ) ) ;
#28513 = CARTESIAN_POINT ( 'NONE',  ( 94.99999999999998579, 92.66308142843932671, 84.40406250086714124 ) ) ;
#28514 = AXIS2_PLACEMENT_3D ( 'NONE', #11064, #22724, #4699 ) ;
#28515 = DIRECTION ( 'NONE',  ( 0.000000000000000000, 0.000000000000000000, 1.000000000000000000 ) ) ;
#28516 = DIRECTION ( 'NONE',  ( 1.000000000000000000, -3.061616997868382648E-16, -0.000000000000000000 ) ) ;
#28517 = CARTESIAN_POINT ( 'NONE',  ( 10.00000000000000000, -16.65560815589383381, -38.55633173627028754 ) ) ;
#28518 = DIRECTION ( 'NONE',  ( -0.000000000000000000, -0.000000000000000000, 1.000000000000000000 ) ) ;
#28519 = CARTESIAN_POINT ( 'NONE',  ( 0.000000000000000000, 2.946379043146343246, 75.11764819372150725 ) ) ;
#28520 = CARTESIAN_POINT ( 'NONE',  ( 0.7178748134486927501, 5.359037475107204962, -1.327869168827484403 ) ) ;
#28521 = CARTESIAN_POINT ( 'NONE',  ( -23.97194136764370498, -131.3950000906648938, -5.500000000000000000 ) ) ;
#28522 = CARTESIAN_POINT ( 'NONE',  ( 0.7800914985199594032, -118.7188063167744900, -2.500000000000000000 ) ) ;
#28523 = ADVANCED_FACE ( 'NONE', ( #67733 ), #4656, .T. ) ;
#28524 = DIRECTION ( 'NONE',  ( 1.000000000000000000, -0.000000000000000000, 0.000000000000000000 ) ) ;
#28525 = DIRECTION ( 'NONE',  ( -1.000000000000000000, 0.000000000000000000, 0.000000000000000000 ) ) ;
#28526 = DIRECTION ( 'NONE',  ( 1.000000000000000000, -0.000000000000000000, 0.000000000000000000 ) ) ;
#28527 = DIRECTION ( 'NONE',  ( -1.000000000000000000, 1.047380211910311281E-14, 2.618450529775778123E-14 ) ) ;
#28528 = STYLED_ITEM ( 'NONE', ( #65735 ), #39004 ) ;
#28529 = CARTESIAN_POINT ( 'NONE',  ( -92.34999999999999432, -211.5299782133524502, 80.73958333333332860 ) ) ;
#28530 = AXIS2_PLACEMENT_3D ( 'NONE', #13676, #32073, #59557 ) ;
#28532 = ADVANCED_FACE ( 'NONE', ( #32023 ), #73035, .T. ) ;
#28531 = CARTESIAN_POINT ( 'NONE',  ( 97.64999999999989200, 88.47002178664747873, 85.81958333333332689 ) ) ;
#28533 = EDGE_CURVE ( 'NONE', #48094, #37368, #2257, .T. ) ;
#28534 = EDGE_CURVE ( 'NONE', #60050, #50746, #20750, .T. ) ;
#28535 = EDGE_LOOP ( 'NONE', ( #26709, #23575, #33094, #44295 ) ) ;
#28536 = CARTESIAN_POINT ( 'NONE',  ( -93.67500000000003979, 92.29496732002878900, 77.08833333333332405 ) ) ;
#28537 = CARTESIAN_POINT ( 'NONE',  ( 94.99999999999998579, 90.00000000000002842, 90.00000000000000000 ) ) ;
#28538 = PLANE ( 'NONE',  #49040 ) ;
#28539 = CARTESIAN_POINT ( 'NONE',  ( -92.35000000000006537, 90.00000034979574082, 77.69687501385438111 ) ) ;
#28540 = CARTESIAN_POINT ( 'NONE',  ( 93.84685191531249870, -208.0026889286704943, 85.25072916753381946 ) ) ;
#28541 = ORIENTED_EDGE ( 'NONE', *, *, #44563, .T. ) ;
#28542 = ORIENTED_EDGE ( 'NONE', *, *, #32133, .T. ) ;
#28543 = DIRECTION ( 'NONE',  ( -0.000000000000000000, -0.000000000000000000, -1.000000000000000000 ) ) ;
#28544 = ORIENTED_EDGE ( 'NONE', *, *, #50214, .F. ) ;
#28545 = CARTESIAN_POINT ( 'NONE',  ( 0.000000000000000000, 0.000000000000000000, 0.000000000000000000 ) ) ;
#28546 = CARTESIAN_POINT ( 'NONE',  ( 95.00000000000000000, -212.6630814284392557, 78.37156250086714238 ) ) ;
#28547 = VECTOR ( 'NONE', #20977, 1000.000000000000000 ) ;
#28548 = EDGE_LOOP ( 'NONE', ( #51200, #8539 ) ) ;
#28549 = CARTESIAN_POINT ( 'NONE',  ( 92.69370383062501162, -208.6684592857803011, 81.49364583420047836 ) ) ;
#28550 = VECTOR ( 'NONE', #36665, 1000.000000000000000 ) ;
#28551 = ORIENTED_EDGE ( 'NONE', *, *, #43714, .F. ) ;
#28552 = CARTESIAN_POINT ( 'NONE',  ( 1.560000000000000053, -0.8660254037844384856, -1.500000000000000000 ) ) ;
#28553 = ORIENTED_EDGE ( 'NONE', *, *, #67561, .F. ) ;
#28554 = ORIENTED_EDGE ( 'NONE', *, *, #40467, .F. ) ;
#28555 = AXIS2_PLACEMENT_3D ( 'NONE', #26282, #72868, #43240 ) ;
#28556 = LINE ( 'NONE', #51499, #59265 ) ;
#28557 = EDGE_LOOP ( 'NONE', ( #13844, #5967, #73846, #33747 ) ) ;
#28558 = CARTESIAN_POINT ( 'NONE',  ( 92.35000000000000853, -209.9999678257246103, 76.74437388893714740 ) ) ;
#28559 = CARTESIAN_POINT ( 'NONE',  ( 92.35000000000002274, -211.5299782133524502, 85.68729166840097378 ) ) ;
#28560 = ORIENTED_EDGE ( 'NONE', *, *, #65558, .F. ) ;
#28561 = CYLINDRICAL_SURFACE ( 'NONE', #15487, 31.99999999999998579 ) ;
#28562 = EDGE_CURVE ( 'NONE', #29240, #47328, #43700, .T. ) ;
#28563 = VERTEX_POINT ( 'NONE', #10572 ) ;
#28564 =( BOUNDED_CURVE ( )  B_SPLINE_CURVE ( 2, ( #70272, #18778, #13142, #437, #45904, #35698, #36082 ),
 .UNSPECIFIED., .F., .F. ) 
 B_SPLINE_CURVE_WITH_KNOTS ( ( 3, 2, 2, 3 ),
 ( 0.5416666666666665186, 0.5486111111111110494, 0.5555555555555553582, 0.5624999999999997780 ),
 .UNSPECIFIED. ) 
 CURVE ( )  GEOMETRIC_REPRESENTATION_ITEM ( )  RATIONAL_B_SPLINE_CURVE ( ( 1.000000000000002220, 0.8660254037844365982, 1.000000000000000000, 0.8660254037844387076, 1.000000000000000000, 0.8660254037844430375, 0.9999999999999956701 ) ) 
 REPRESENTATION_ITEM ( '' )  );
#28565 = DIRECTION ( 'NONE',  ( -1.000000000000000000, 0.000000000000000000, 0.000000000000000000 ) ) ;
#28566 = VERTEX_POINT ( 'NONE', #61723 ) ;
#28567 = ADVANCED_FACE ( 'NONE', ( #9843 ), #16591, .T. ) ;
#28568 = VERTEX_POINT ( 'NONE', #45179 ) ;
#28569 = ORIENTED_EDGE ( 'NONE', *, *, #71042, .F. ) ;
#28570 = CARTESIAN_POINT ( 'NONE',  ( 10.00000000000000000, 6.555932627142418312, 37.01155633439060466 ) ) ;
#28571 = DIRECTION ( 'NONE',  ( 0.000000000000000000, -0.1564344650402381687, 0.9876883405951365491 ) ) ;
#28573 = EDGE_CURVE ( 'NONE', #62140, #52314, #19065, .T. ) ;
#28572 = ORIENTED_EDGE ( 'NONE', *, *, #74296, .F. ) ;
#28574 = AXIS2_PLACEMENT_3D ( 'NONE', #52140, #47611, #53619 ) ;
#28575 = ORIENTED_EDGE ( 'NONE', *, *, #41227, .T. ) ;
#28576 = CIRCLE ( 'NONE', #70586, 77.49899999999998101 ) ;
#28577 = EDGE_LOOP ( 'NONE', ( #44881, #27552, #60261, #62722 ) ) ;
#28578 = DIRECTION ( 'NONE',  ( -1.000000000000000000, 0.000000000000000000, -0.000000000000000000 ) ) ;
#28579 = ADVANCED_FACE ( 'NONE', ( #66622 ), #3483, .T. ) ;
#28580 = DIRECTION ( 'NONE',  ( -1.000000000000000000, 0.000000000000000000, 0.000000000000000000 ) ) ;
#28581 = VECTOR ( 'NONE', #68612, 1000.000000000000000 ) ;
#28582 = AXIS2_PLACEMENT_3D ( 'NONE', #1668, #65162, #35820 ) ;
#28583 = CARTESIAN_POINT ( 'NONE',  ( -93.67500000000003979, 87.70503267997129626, 87.67166666666666686 ) ) ;
#28584 = ORIENTED_EDGE ( 'NONE', *, *, #46017, .T. ) ;
#28585 = CARTESIAN_POINT ( 'NONE',  ( 92.69370383062498320, 88.66845928578037217, 75.09072916753382287 ) ) ;
#28586 = CIRCLE ( 'NONE', #64609, 77.49899999999999523 ) ;
#28587 = ORIENTED_EDGE ( 'NONE', *, *, #13512, .T. ) ;
#28588 =( BOUNDED_CURVE ( )  B_SPLINE_CURVE ( 2, ( #45808, #56714, #52159, #39786, #69816, #34132, #68732 ),
 .UNSPECIFIED., .F., .F. ) 
 B_SPLINE_CURVE_WITH_KNOTS ( ( 3, 2, 2, 3 ),
 ( 0.3175094496506953301, 0.3245652148805889814, 0.3316209804214713674, 0.3386766260338263668 ),
 .UNSPECIFIED. ) 
 CURVE ( )  GEOMETRIC_REPRESENTATION_ITEM ( )  RATIONAL_B_SPLINE_CURVE ( ( 1.000000000000000000, 0.8660254037844387076, 1.000000000000000000, 0.8660254037844387076, 1.000000000000000000, 0.8660276809825581124, 0.9999954456811732673 ) ) 
 REPRESENTATION_ITEM ( '' )  );
#28589 = DIRECTION ( 'NONE',  ( 1.000000000000000000, 0.000000000000000000, 0.000000000000000000 ) ) ;
#28590 = CARTESIAN_POINT ( 'NONE',  ( -97.30629616937495996, -209.9999999999999716, 84.56281250086713897 ) ) ;
#28591 = VERTEX_POINT ( 'NONE', #27115 ) ;
#28592 = DIRECTION ( 'NONE',  ( -1.000000000000000000, -0.000000000000000000, 0.000000000000000000 ) ) ;
#28593 = CARTESIAN_POINT ( 'NONE',  ( 15.00000000000000000, -10.45096189432314127, 21.10159698893440350 ) ) ;
#28594 = FACE_OUTER_BOUND ( 'NONE', #24089, .T. ) ;
#28595 = CARTESIAN_POINT ( 'NONE',  ( -93.84685191531247028, -211.9973110713294489, 76.51947916753380241 ) ) ;
#28596 = EDGE_CURVE ( 'NONE', #14685, #25432, #14222, .T. ) ;
#28597 = CARTESIAN_POINT ( 'NONE',  ( 11.99999999999999822, 31.47745569255237896, -68.26794271651228030 ) ) ;
#28598 = DIRECTION ( 'NONE',  ( 0.000000000000000000, 0.000000000000000000, 1.000000000000000000 ) ) ;
#28599 = PLANE ( 'NONE',  #6111 ) ;
#28600 = CARTESIAN_POINT ( 'NONE',  ( 2.500000000000000000, 16.00000000000000000, 0.000000000000000000 ) ) ;
#28601 = CARTESIAN_POINT ( 'NONE',  ( 0.000000000000000000, -6.736453364083290651, -36.88895765772640090 ) ) ;
#28602 = CARTESIAN_POINT ( 'NONE',  ( -96.15314808468752972, 91.99731107132950569, 78.10697916753380809 ) ) ;
#28603 = DIRECTION ( 'NONE',  ( 0.000000000000000000, 0.000000000000000000, 1.000000000000000000 ) ) ;
#28604 = CARTESIAN_POINT ( 'NONE',  ( 0.000000000000000000, 0.000000000000000000, -275.0000000000000000 ) ) ;
#28605 = EDGE_CURVE ( 'NONE', #33095, #15883, #46659, .T. ) ;
#28606 = STYLED_ITEM ( 'NONE', ( #33271 ), #62892 ) ;
#28607 = ORIENTED_EDGE ( 'NONE', *, *, #959, .T. ) ;
#28608 = EDGE_CURVE ( 'NONE', #52621, #29721, #9467, .T. ) ;
#28609 = DIRECTION ( 'NONE',  ( 0.000000000000000000, 0.000000000000000000, 1.000000000000000000 ) ) ;
#28610 = CIRCLE ( 'NONE', #8168, 37.49900000000000233 ) ;
#28611 = VECTOR ( 'NONE', #35012, 1000.000000000000000 ) ;
#28612 = EDGE_CURVE ( 'NONE', #27381, #18231, #71863, .T. ) ;
#28613 = CARTESIAN_POINT ( 'NONE',  ( 10.00000000000000000, 30.80686688397041451, -21.53537804866048688 ) ) ;
#28614 = CARTESIAN_POINT ( 'NONE',  ( 0.000000000000000000, 36.88895765772633695, 6.736453364083687667 ) ) ;
#28616 = AXIS2_PLACEMENT_3D ( 'NONE', #6168, #40735, #46010 ) ;
#28615 = DIRECTION ( 'NONE',  ( -1.000000000000000000, -0.000000000000000000, -0.000000000000000000 ) ) ;
#28617 = LINE ( 'NONE', #51559, #52559 ) ;
#28618 = CARTESIAN_POINT ( 'NONE',  ( 97.64999999999821512, 90.00000306648260562, 75.79187510780352000 ) ) ;
#28619 = CARTESIAN_POINT ( 'NONE',  ( -96.15314808468747287, -208.0026889286704943, 78.26572916753382003 ) ) ;
#28620 = AXIS2_PLACEMENT_3D ( 'NONE', #66641, #42976, #26766 ) ;
#28621 = DIRECTION ( 'NONE',  ( 1.000000000000000000, 0.000000000000000000, 0.000000000000000000 ) ) ;
#28622 = EDGE_CURVE ( 'NONE', #10925, #72940, #72973, .T. ) ;
#28623 = VERTEX_POINT ( 'NONE', #10208 ) ;
#28624 = DIRECTION ( 'NONE',  ( 1.000000000000000000, 0.000000000000000000, 0.000000000000000000 ) ) ;
#28625 = PLANE ( 'NONE',  #69409 ) ;
#28626 = DIRECTION ( 'NONE',  ( 0.000000000000000000, -0.5000000000000012212, -0.8660254037844380415 ) ) ;
#28627 = EDGE_CURVE ( 'NONE', #27456, #7986, #50797, .T. ) ;
#28628 = DIRECTION ( 'NONE',  ( 2.603472992746261562E-14, 2.546204323184492723E-14, -1.000000000000000000 ) ) ;
#28629 = VECTOR ( 'NONE', #48318, 1000.000000000000000 ) ;
#28630 = AXIS2_PLACEMENT_3D ( 'NONE', #14328, #6842, #1981 ) ;
#28631 = CARTESIAN_POINT ( 'NONE',  ( 12.50000000000000000, -107.5000000000000000, 2.500000000000000000 ) ) ;
#28632 = VERTEX_POINT ( 'NONE', #15858 ) ;
#28633 = AXIS2_PLACEMENT_3D ( 'NONE', #59056, #6802, #19189 ) ;
#28634 = DIRECTION ( 'NONE',  ( -1.000000000000000000, 0.000000000000000000, -0.000000000000000000 ) ) ;
#28635 = DIRECTION ( 'NONE',  ( -1.000000000000000000, 0.000000000000000000, -0.000000000000000000 ) ) ;
#28636 = ORIENTED_EDGE ( 'NONE', *, *, #69867, .F. ) ;
#28637 = CARTESIAN_POINT ( 'NONE',  ( -3.000000000000000000, -10.45096189432314837, -21.10159698893440350 ) ) ;
#28638 = CARTESIAN_POINT ( 'NONE',  ( -10.00000000000000000, 0.000000000000000000, 0.000000000000000000 ) ) ;
#28639 = VERTEX_POINT ( 'NONE', #33131 ) ;
#28640 = CARTESIAN_POINT ( 'NONE',  ( 0.000000000000000000, 0.000000000000000000, 0.000000000000000000 ) ) ;
#28641 = ORIENTED_EDGE ( 'NONE', *, *, #36001, .T. ) ;
#28642 = DIRECTION ( 'NONE',  ( 0.000000000000000000, 0.000000000000000000, 1.000000000000000000 ) ) ;
#28643 = ORIENTED_EDGE ( 'NONE', *, *, #26062, .F. ) ;
#28644 = CARTESIAN_POINT ( 'NONE',  ( -93.67499999999998295, -212.2949673200287179, 80.13104166840095388 ) ) ;
#28645 = ORIENTED_EDGE ( 'NONE', *, *, #4631, .T. ) ;
#28646 = DIRECTION ( 'NONE',  ( -1.000000000000000000, -0.000000000000000000, 0.000000000000000000 ) ) ;
#28647 = VERTEX_POINT ( 'NONE', #49678 ) ;
#28648 = ORIENTED_EDGE ( 'NONE', *, *, #41516, .F. ) ;
#28649 = CARTESIAN_POINT ( 'NONE',  ( 0.000000000000000000, -74.65374052328644439, -8.840884882375878107 ) ) ;
#28650 = CIRCLE ( 'NONE', #53888, 21.00000000000000000 ) ;
#28651 = ORIENTED_EDGE ( 'NONE', *, *, #44063, .T. ) ;
#28652 = ORIENTED_EDGE ( 'NONE', *, *, #23102, .F. ) ;
#28653 = CARTESIAN_POINT ( 'NONE',  ( 0.000000000000000000, 0.000000000000000000, 0.000000000000000000 ) ) ;
#28654 = AXIS2_PLACEMENT_3D ( 'NONE', #30235, #71561, #53176 ) ;
#28655 = DIRECTION ( 'NONE',  ( -1.000000000000000000, -0.000000000000000000, -0.000000000000000000 ) ) ;
#28656 = VECTOR ( 'NONE', #12159, 1000.000000000000114 ) ;
#28657 = EDGE_LOOP ( 'NONE', ( #15991, #71008, #63911, #35623 ) ) ;
#28658 = VECTOR ( 'NONE', #59421, 1000.000000000000114 ) ;
#28659 = EDGE_CURVE ( 'NONE', #57179, #24964, #22677, .T. ) ;
#28660 = ORIENTED_EDGE ( 'NONE', *, *, #45185, .F. ) ;
#28661 = CARTESIAN_POINT ( 'NONE',  ( 96.15314808468748708, 88.00268892867053694, 86.67947916753381321 ) ) ;
#28662 = ORIENTED_EDGE ( 'NONE', *, *, #28627, .T. ) ;
#28663 = CARTESIAN_POINT ( 'NONE',  ( 97.30629616937498838, -211.3315407142195852, 80.38239583420049428 ) ) ;
#28664 = PRODUCT_CONTEXT ( 'NONE', #60386, 'mechanical' ) ;
#28665 = DIRECTION ( 'NONE',  ( 0.000000000000000000, 0.000000000000000000, -1.000000000000000000 ) ) ;
#28666 = AXIS2_PLACEMENT_3D ( 'NONE', #4222, #38046, #68103 ) ;
#28667 = ADVANCED_FACE ( 'NONE', ( #21479 ), #44442, .F. ) ;
#28668 = CARTESIAN_POINT ( 'NONE',  ( -92.34999999999999432, -209.9999999999999716, 90.00000000000000000 ) ) ;
#28669 = CARTESIAN_POINT ( 'NONE',  ( 92.35000000000000853, -209.9999999999999716, 82.37999999999999545 ) ) ;
#28670 = CIRCLE ( 'NONE', #74300, 15.70000000000327312 ) ;
#28671 = DIRECTION ( 'NONE',  ( -1.000000000000000000, 0.000000000000000000, 0.000000000000000000 ) ) ;
#28672 = DIRECTION ( 'NONE',  ( 0.000000000000000000, 0.000000000000000000, 1.000000000000000000 ) ) ;
#28673 = ADVANCED_FACE ( 'NONE', ( #6795 ), #23357, .T. ) ;
#28674 = DIRECTION ( 'NONE',  ( -1.000000000000000000, 0.000000000000000000, 0.000000000000000000 ) ) ;
#28675 = CARTESIAN_POINT ( 'NONE',  ( -94.99999999999997158, -212.6630814284392557, 89.16656250086712987 ) ) ;
#28676 = CARTESIAN_POINT ( 'NONE',  ( -93.84685191531254134, 91.99731107132950569, 87.04989583420048405 ) ) ;
#28677 = ORIENTED_EDGE ( 'NONE', *, *, #22953, .F. ) ;
#28679 = CARTESIAN_POINT ( 'NONE',  ( -93.84685191531252713, 88.00268892867056536, 86.04447916753380809 ) ) ;
#28678 = CARTESIAN_POINT ( 'NONE',  ( 93.84685191531248449, 91.99731107132950569, 84.45697916753380241 ) ) ;
#28680 = VERTEX_POINT ( 'NONE', #68485 ) ;
#28681 = CARTESIAN_POINT ( 'NONE',  ( -93.67500000000003979, 87.70503267997129626, 78.86104166840097207 ) ) ;
#28682 = LINE ( 'NONE', #5777, #70986 ) ;
#28683 = LINE ( 'NONE', #63291, #66777 ) ;
#28684 = CYLINDRICAL_SURFACE ( 'NONE', #3268, 2.649999999999985700 ) ;
#28685 = VECTOR ( 'NONE', #1015, 1000.000000000000000 ) ;
#28686 = CARTESIAN_POINT ( 'NONE',  ( -92.69370383062498320, -208.6684592857803295, 86.83822916753381094 ) ) ;
#28687 = CARTESIAN_POINT ( 'NONE',  ( 30.50000000000000000, -120.0000000000000000, -5.500000000000000000 ) ) ;
#28688 = AXIS2_PLACEMENT_3D ( 'NONE', #43957, #43231, #3021 ) ;
#28689 = CARTESIAN_POINT ( 'NONE',  ( 92.35000000000000853, -209.9999999999999716, 90.00000000000000000 ) ) ;
#28690 = CARTESIAN_POINT ( 'NONE',  ( 10.00000000000000000, -68.27212725128298132, 31.46837873494953541 ) ) ;
#28691 = CARTESIAN_POINT ( 'NONE',  ( 5.000000000000000000, -31.52238457039579345, -27.75498641678775158 ) ) ;
#28692 = ORIENTED_EDGE ( 'NONE', *, *, #56112, .T. ) ;
#28693 = AXIS2_PLACEMENT_3D ( 'NONE', #71067, #30841, #42892 ) ;
#28694 = AXIS2_PLACEMENT_3D ( 'NONE', #64281, #13855, #2265 ) ;
#28695 = VERTEX_POINT ( 'NONE', #28982 ) ;
#28696 = CIRCLE ( 'NONE', #67115, 77.49899999999999523 ) ;
#28697 = EDGE_CURVE ( 'NONE', #11224, #55326, #21407, .T. ) ;
#28698 = CIRCLE ( 'NONE', #64712, 82.00000000000000000 ) ;
#28699 = CARTESIAN_POINT ( 'NONE',  ( -97.65000000000001990, 91.52997821335253548, 78.51708333333334622 ) ) ;
#28700 = DIRECTION ( 'NONE',  ( 0.000000000000000000, 0.000000000000000000, 1.000000000000000000 ) ) ;
#28701 = CARTESIAN_POINT ( 'NONE',  ( -93.59478774260932710, -208.1321859400969174, 74.80441578173234518 ) ) ;
#28702 = DIRECTION ( 'NONE',  ( 0.000000000000000000, 0.000000000000000000, 1.000000000000000000 ) ) ;
#28703 = DIRECTION ( 'NONE',  ( 0.000000000000000000, 0.000000000000000000, 1.000000000000000000 ) ) ;
#28704 = CARTESIAN_POINT ( 'NONE',  ( 11.99999999999999822, 11.30684508768450769, -76.66974797899825944 ) ) ;
#28705 = CARTESIAN_POINT ( 'NONE',  ( -97.64999999999996305, -209.9999999999999716, 78.57000000000000739 ) ) ;
#28706 = CIRCLE ( 'NONE', #7080, 3.250000000000001332 ) ;
#28707 = ORIENTED_EDGE ( 'NONE', *, *, #72184, .T. ) ;
#28708 = CARTESIAN_POINT ( 'NONE',  ( -93.84685191531252713, 88.00268892867056536, 77.78947916753381264 ) ) ;
#28709 = CARTESIAN_POINT ( 'NONE',  ( 10.00000000000000000, 37.48860685352291000, 0.8828120875901893649 ) ) ;
#28710 = ADVANCED_FACE ( 'NONE', ( #6440 ), #63218, .F. ) ;
#28711 = EDGE_CURVE ( 'NONE', #26180, #55579, #23847, .T. ) ;
#28712 = DIRECTION ( 'NONE',  ( 0.000000000000000000, 0.2334453638559060851, -0.9723699203976764460 ) ) ;
#28713 = CYLINDRICAL_SURFACE ( 'NONE', #34673, 31.99999999999998579 ) ;
#28714 = CARTESIAN_POINT ( 'NONE',  ( 0.000000000000000000, 0.000000000000000000, 0.000000000000000000 ) ) ;
#28715 = CARTESIAN_POINT ( 'NONE',  ( 10.00000000000000000, -70.52718814184240159, -26.02418014898383802 ) ) ;
#28716 = CARTESIAN_POINT ( 'NONE',  ( -92.69370383062498320, -208.6684592857803011, 88.90197916753382401 ) ) ;
#28717 =( BOUNDED_CURVE ( )  B_SPLINE_CURVE ( 2, ( #67371, #44825, #33520, #10979, #56482, #67750, #40289 ),
 .UNSPECIFIED., .F., .F. ) 
 B_SPLINE_CURVE_WITH_KNOTS ( ( 3, 2, 2, 3 ),
 ( 0.08333333333333288462, 0.09027777777777759582, 0.09722222222222230703, 0.1041666666666670182 ),
 .UNSPECIFIED. ) 
 CURVE ( )  GEOMETRIC_REPRESENTATION_ITEM ( )  RATIONAL_B_SPLINE_CURVE ( ( 1.000000000000008660, 0.8660254037844301589, 1.000000000000000000, 0.8660254037844387076, 1.000000000000000000, 0.8660254037844320463, 1.000000000000006661 ) ) 
 REPRESENTATION_ITEM ( '' )  );
#28718 = EDGE_CURVE ( 'NONE', #19228, #37462, #58680, .T. ) ;
#28719 = CARTESIAN_POINT ( 'NONE',  ( 92.69370383062498320, 91.33154071421968467, 75.77864583420048916 ) ) ;
#28720 = AXIS2_PLACEMENT_3D ( 'NONE', #36270, #53943, #71952 ) ;
#28721 = CARTESIAN_POINT ( 'NONE',  ( -92.69370383062498320, -211.3315407142195852, 79.27114583420048177 ) ) ;
#28722 = LINE ( 'NONE', #5077, #69849 ) ;
#28723 = ORIENTED_EDGE ( 'NONE', *, *, #18163, .T. ) ;
#28724 = LINE ( 'NONE', #47503, #64116 ) ;
#28725 = CARTESIAN_POINT ( 'NONE',  ( -96.32499999999996021, -212.2949673200287179, 75.50083333333331836 ) ) ;
#28726 = VECTOR ( 'NONE', #45063, 1000.000000000000000 ) ;
#28727 = LINE ( 'NONE', #212, #52129 ) ;
#28728 = AXIS2_PLACEMENT_3D ( 'NONE', #53312, #48406, #37142 ) ;
#28729 = AXIS2_PLACEMENT_3D ( 'NONE', #22545, #4906, #45488 ) ;
#28730 = CARTESIAN_POINT ( 'NONE',  ( -93.33920801875068207, 88.39975876321990711, 74.80065669543250806 ) ) ;
#28731 = CARTESIAN_POINT ( 'NONE',  ( 97.30629616937498838, -211.3315407142195852, 81.01739583420048518 ) ) ;
#28732 = VERTEX_POINT ( 'NONE', #16973 ) ;
#28733 = CARTESIAN_POINT ( 'NONE',  ( 10.00000000000000000, 33.71516098798738881, 74.74816331893441657 ) ) ;
#28734 = ORIENTED_EDGE ( 'NONE', *, *, #30825, .T. ) ;
#28735 = CARTESIAN_POINT ( 'NONE',  ( -52.50000000000002132, 0.000000000000000000, -175.0000000000000000 ) ) ;
#28736 = VERTEX_POINT ( 'NONE', #29708 ) ;
#28737 = AXIS2_PLACEMENT_3D ( 'NONE', #37940, #65772, #14631 ) ;
#28738 = CARTESIAN_POINT ( 'NONE',  ( 92.35000000000000853, -209.9999999999999716, 77.29999999999999716 ) ) ;
#28739 = AXIS2_PLACEMENT_3D ( 'NONE', #2825, #14434, #1719 ) ;
#28740 = AXIS2_PLACEMENT_3D ( 'NONE', #5953, #40145, #5580 ) ;
#28741 = VERTEX_POINT ( 'NONE', #40270 ) ;
#28742 = ORIENTED_EDGE ( 'NONE', *, *, #9402, .F. ) ;
#28743 = CIRCLE ( 'NONE', #45629, 31.99999999999998934 ) ;
#28744 = VERTEX_POINT ( 'NONE', #52286 ) ;
#28745 = VECTOR ( 'NONE', #64702, 1000.000000000000000 ) ;
#28746 = CARTESIAN_POINT ( 'NONE',  ( 95.00000000000000000, -206.9400435732949575, 79.76062500173429726 ) ) ;
#28747 = EDGE_LOOP ( 'NONE', ( #60513, #11720, #67904, #41601 ) ) ;
#28748 =( REPRESENTATION_RELATIONSHIP ('NONE','NONE', #31117, #27826 ) REPRESENTATION_RELATIONSHIP_WITH_TRANSFORMATION ( #32361 )SHAPE_REPRESENTATION_RELATIONSHIP( ) );
#28749 = ORIENTED_EDGE ( 'NONE', *, *, #2511, .F. ) ;
#28750 = CARTESIAN_POINT ( 'NONE',  ( 92.69370383062498320, 88.66845928578037217, 84.13947916753383538 ) ) ;
#28751 = CARTESIAN_POINT ( 'NONE',  ( 97.64999999999997726, -208.4700217866474645, 78.94041666666666401 ) ) ;
#28752 = ORIENTED_EDGE ( 'NONE', *, *, #3163, .F. ) ;
#28753 = VERTEX_POINT ( 'NONE', #57572 ) ;
#28754 = EDGE_CURVE ( 'NONE', #68962, #18236, #65885, .T. ) ;
#28755 = ORIENTED_EDGE ( 'NONE', *, *, #29030, .F. ) ;
#28756 = VERTEX_POINT ( 'NONE', #22992 ) ;
#28757 = CARTESIAN_POINT ( 'NONE',  ( -4.653126046682595884, -146.1313684676804314, 2.500000000000000000 ) ) ;
#28758 = DIRECTION ( 'NONE',  ( 0.000000000000000000, 0.000000000000000000, 1.000000000000000000 ) ) ;
#28759 = DIRECTION ( 'NONE',  ( -1.000000000000000000, 0.000000000000000000, 0.000000000000000000 ) ) ;
#28760 = ADVANCED_FACE ( 'NONE', ( #45927 ), #39913, .T. ) ;
#28761 = CARTESIAN_POINT ( 'NONE',  ( 11.99999999999999822, 41.76937507738788469, 62.50329211542452157 ) ) ;
#28762 = CARTESIAN_POINT ( 'NONE',  ( 0.000000000000000000, 37.58145647212453611, 0.6853352020791767529 ) ) ;
#28763 = CARTESIAN_POINT ( 'NONE',  ( 0.000000000000000000, -8.830959090342926032, 74.65491531819115778 ) ) ;
#28764 = DIRECTION ( 'NONE',  ( 1.000000000000000000, 0.000000000000000000, 0.000000000000000000 ) ) ;
#28765 = DIRECTION ( 'NONE',  ( 0.000000000000000000, 0.000000000000000000, 1.000000000000000000 ) ) ;
#28767 = ORIENTED_EDGE ( 'NONE', *, *, #48033, .F. ) ;
#28766 = ADVANCED_FACE ( 'NONE', ( #39535, #62862 ), #51170, .F. ) ;
#28768 = CARTESIAN_POINT ( 'NONE',  ( -93.67499999999998295, -212.2949673200287179, 82.67104166840096013 ) ) ;
#28769 = ORIENTED_EDGE ( 'NONE', *, *, #47709, .T. ) ;
#28770 = CARTESIAN_POINT ( 'NONE',  ( -2.977765906491215642, 0.000000000000000000, -15.39727592589476579 ) ) ;
#28771 = ORIENTED_EDGE ( 'NONE', *, *, #44211, .F. ) ;
#28773 = CARTESIAN_POINT ( 'NONE',  ( -92.35000000000003695, 90.00000000000004263, 80.23687500173429044 ) ) ;
#28772 = CARTESIAN_POINT ( 'NONE',  ( 92.34999999999999432, 91.52997821335252127, 77.96145833506763267 ) ) ;
#28774 = EDGE_CURVE ( 'NONE', #36870, #60602, #46649, .T. ) ;
#28775 = AXIS2_PLACEMENT_3D ( 'NONE', #53611, #19397, #2155 ) ;
#28776 = ORIENTED_EDGE ( 'NONE', *, *, #48064, .F. ) ;
#28777 = CARTESIAN_POINT ( 'NONE',  ( 93.84685191531248449, 88.00268892867053694, 79.74739583420048916 ) ) ;
#28778 = DIRECTION ( 'NONE',  ( -1.000000000000000000, 0.000000000000000000, 0.000000000000000000 ) ) ;
#28779 = CARTESIAN_POINT ( 'NONE',  ( 99.99999999999998579, 95.00000000000001421, -90.00000000000002842 ) ) ;
#28780 = CIRCLE ( 'NONE', #31187, 30.50000000000000000 ) ;
#28781 = CARTESIAN_POINT ( 'NONE',  ( -11.99999999999999645, 1.574895783703496238E-15, -12.85999999999999943 ) ) ;
#28782 = DIRECTION ( 'NONE',  ( 0.000000000000000000, 0.000000000000000000, 1.000000000000000000 ) ) ;
#28783 = CIRCLE ( 'NONE', #34745, 52.50000000000002132 ) ;
#28784 = ORIENTED_EDGE ( 'NONE', *, *, #29359, .F. ) ;
#28786 = EDGE_CURVE ( 'NONE', #27527, #47885, #45493, .T. ) ;
#28785 = LINE ( 'NONE', #10758, #18363 ) ;
#28787 = PLANE ( 'NONE',  #30124 ) ;
#28788 = CARTESIAN_POINT ( 'NONE',  ( 0.000000000000000000, 75.11764819372149304, 29.05362095685338986 ) ) ;
#28789 = VERTEX_POINT ( 'NONE', #62484 ) ;
#28790 = ORIENTED_EDGE ( 'NONE', *, *, #18182, .F. ) ;
#28791 = VECTOR ( 'NONE', #11170, 1000.000000000000000 ) ;
#28792 = ADVANCED_FACE ( 'NONE', ( #24102 ), #17338, .T. ) ;
#28793 = EDGE_CURVE ( 'NONE', #21165, #11119, #41877, .T. ) ;
#28794 = CARTESIAN_POINT ( 'NONE',  ( -6.719258119307965238, -15.35072898742050107, -1.199999999999999956 ) ) ;
#28795 = PLANE ( 'NONE',  #71423 ) ;
#28796 = CARTESIAN_POINT ( 'NONE',  ( 95.00000000000000000, -209.9999999999999716, 90.00000000000000000 ) ) ;
#28797 = CARTESIAN_POINT ( 'NONE',  ( -96.15314808468747287, -208.0026889286704943, 80.17072916753382117 ) ) ;
#28798 = EDGE_LOOP ( 'NONE', ( #23750, #32535, #1537, #36809 ) ) ;
#28799 = CONICAL_SURFACE ( 'NONE', #49176, 15.39727592589476579, 0.2094395102393128150 ) ;
#28800 = DIRECTION ( 'NONE',  ( 0.000000000000000000, 0.3090169943749410120, 0.9510565162951557516 ) ) ;
#28801 = AXIS2_PLACEMENT_3D ( 'NONE', #27703, #40753, #73930 ) ;
#28802 = EDGE_CURVE ( 'NONE', #38492, #3018, #9460, .T. ) ;
#28803 = EDGE_CURVE ( 'NONE', #66673, #38385, #74101, .T. ) ;
#28804 = AXIS2_PLACEMENT_3D ( 'NONE', #26839, #26472, #49406 ) ;
#28805 = CARTESIAN_POINT ( 'NONE',  ( -3.000000000000000000, -18.13022148937263012, 15.02647892043544608 ) ) ;
#28806 = FACE_OUTER_BOUND ( 'NONE', #56676, .T. ) ;
#28807 = CARTESIAN_POINT ( 'NONE',  ( 96.15314808468748708, 91.99731107132950569, 74.82614583420047438 ) ) ;
#28808 = DIRECTION ( 'NONE',  ( 0.000000000000000000, 0.000000000000000000, 1.000000000000000000 ) ) ;
#28809 = CARTESIAN_POINT ( 'NONE',  ( 0.000000000000000000, 0.000000000000000000, 0.000000000000000000 ) ) ;
#28810 = CARTESIAN_POINT ( 'NONE',  ( 10.00000000000000000, 35.91791733033570466, -68.67312586194960033 ) ) ;
#28811 = AXIS2_PLACEMENT_3D ( 'NONE', #73313, #26710, #5304 ) ;
#28812 = DIRECTION ( 'NONE',  ( -1.000000000000000000, 0.000000000000000000, -0.000000000000000000 ) ) ;
#28813 = CIRCLE ( 'NONE', #32389, 16.00000000000000355 ) ;
#28814 = DIRECTION ( 'NONE',  ( 0.000000000000000000, 0.000000000000000000, 1.000000000000000000 ) ) ;
#28815 = LINE ( 'NONE', #650, #5782 ) ;
#28816 =( BOUNDED_CURVE ( )  B_SPLINE_CURVE ( 2, ( #69247, #68520, #46319, #62899, #18475, #17736, #18117, #58335, #46690 ),
 .UNSPECIFIED., .F., .F. ) 
 B_SPLINE_CURVE_WITH_KNOTS ( ( 3, 2, 2, 2, 3 ),
 ( 0.2751748541904411316, 0.2822306216352944985, 0.2892863871761764960, 0.2963421527170585490, 0.2963422021981251264 ),
 .UNSPECIFIED. ) 
 CURVE ( )  GEOMETRIC_REPRESENTATION_ITEM ( )  RATIONAL_B_SPLINE_CURVE ( ( 1.000000000000000000, 0.8660254037844387076, 1.000000000000000000, 0.8660254037844387076, 1.000000000000000000, 0.8660254037844387076, 1.000000000000000000, 0.9999990604554704898, 0.9999981209241187718 ) ) 
 REPRESENTATION_ITEM ( '' )  );
#28817 = CARTESIAN_POINT ( 'NONE',  ( 93.84685191531248449, 88.00268892867053694, 88.63739583420048973 ) ) ;
#28818 = CARTESIAN_POINT ( 'NONE',  ( 11.99999999999999822, 27.74655509720779989, -77.16300072079630468 ) ) ;
#28819 = ORIENTED_EDGE ( 'NONE', *, *, #43480, .T. ) ;
#28820 = DIRECTION ( 'NONE',  ( 0.000000000000000000, 0.000000000000000000, 1.000000000000000000 ) ) ;
#28821 = CARTESIAN_POINT ( 'NONE',  ( -96.15314808468752972, 91.99731107132950569, 81.28197916753380525 ) ) ;
#28822 = LINE ( 'NONE', #50262, #67464 ) ;
#28823 = VERTEX_POINT ( 'NONE', #24825 ) ;
#28825 = CYLINDRICAL_SURFACE ( 'NONE', #15037, 21.00000000000000000 ) ;
#28824 = VECTOR ( 'NONE', #34290, 1000.000000000000227 ) ;
#28826 = CARTESIAN_POINT ( 'NONE',  ( 93.67499999999999716, 87.70503267997126784, 83.12083333333332291 ) ) ;
#28827 = CARTESIAN_POINT ( 'NONE',  ( 0.000000000000000000, -10.30890764327323872, -81.34940948281348483 ) ) ;
#28828 = CIRCLE ( 'NONE', #61260, 3.299999999999997158 ) ;
#28829 = CARTESIAN_POINT ( 'NONE',  ( 0.000000000000000000, 76.69515212746057387, -29.01471420065479379 ) ) ;
#28830 = CARTESIAN_POINT ( 'NONE',  ( 93.84685191531249870, -208.0026889286704943, 75.72572916753382799 ) ) ;
#28831 = DIRECTION ( 'NONE',  ( 0.000000000000000000, 0.9510565162951544194, -0.3090169943749447867 ) ) ;
#28832 = ORIENTED_EDGE ( 'NONE', *, *, #22167, .F. ) ;
#28833 = ADVANCED_FACE ( 'NONE', ( #2680 ), #14279, .T. ) ;
#28834 = ORIENTED_EDGE ( 'NONE', *, *, #7378, .F. ) ;
#28835 = ADVANCED_FACE ( 'NONE', ( #1938 ), #53400, .T. ) ;
#28836 = CARTESIAN_POINT ( 'NONE',  ( 95.00000000000000000, -212.6630814284392557, 85.51531250086715374 ) ) ;
#28837 = CARTESIAN_POINT ( 'NONE',  ( 0.000000000000000000, 0.000000000000000000, 0.000000000000000000 ) ) ;
#28838 = CARTESIAN_POINT ( 'NONE',  ( -21.67772167707813935, -110.8034581014852762, 2.500000000000000000 ) ) ;
#28839 = EDGE_CURVE ( 'NONE', #13145, #61765, #7173, .T. ) ;
#28840 = CARTESIAN_POINT ( 'NONE',  ( 5.000000000000000000, 1.352381405509861523, -0.8629530094790043293 ) ) ;
#28841 = DIRECTION ( 'NONE',  ( 0.000000000000000000, 0.000000000000000000, -1.000000000000000000 ) ) ;
#28842 = CARTESIAN_POINT ( 'NONE',  ( 95.00000000000000000, -213.0599564267049857, 81.98312500173430806 ) ) ;
#28843 = CARTESIAN_POINT ( 'NONE',  ( 95.00000000000000000, -206.9400435732949575, 87.30124999999999602 ) ) ;
#28844 = EDGE_CURVE ( 'NONE', #62061, #69818, #47884, .T. ) ;
#28845 = AXIS2_PLACEMENT_3D ( 'NONE', #6789, #63213, #56828 ) ;
#28846 = VERTEX_POINT ( 'NONE', #48498 ) ;
#28847 = ORIENTED_EDGE ( 'NONE', *, *, #382, .F. ) ;
#28848 = ORIENTED_EDGE ( 'NONE', *, *, #18001, .T. ) ;
#28849 = ORIENTED_EDGE ( 'NONE', *, *, #41492, .F. ) ;
#28850 = DIRECTION ( 'NONE',  ( 0.000000000000000000, -0.2334453638558922350, -0.9723699203976797767 ) ) ;
#28851 = CIRCLE ( 'NONE', #30081, 31.99999999999998579 ) ;
#28852 = PRESENTATION_STYLE_ASSIGNMENT (( #5943 ) ) ;
#28853 = CARTESIAN_POINT ( 'NONE',  ( -97.30629616937501680, 90.00000000000004263, 87.26156250086715715 ) ) ;
#28854 = EDGE_CURVE ( 'NONE', #17876, #2885, #25929, .T. ) ;
#28855 = CYLINDRICAL_SURFACE ( 'NONE', #35334, 31.99999999999998579 ) ;
#28856 = CIRCLE ( 'NONE', #15666, 16.00000000000000000 ) ;
#28857 = CARTESIAN_POINT ( 'NONE',  ( -97.64999999999993463, 88.47002178664750716, 83.70291666666668107 ) ) ;
#28858 = CARTESIAN_POINT ( 'NONE',  ( 97.64999999999997726, -208.4700217866474645, 75.84479166840098685 ) ) ;
#28859 = CARTESIAN_POINT ( 'NONE',  ( 94.99999999999998579, 86.94004357329500010, 78.09374999999998579 ) ) ;
#28860 = VERTEX_POINT ( 'NONE', #30820 ) ;
#28861 = CARTESIAN_POINT ( 'NONE',  ( -23.30023580412278505, -123.4057321492263384, 5.500000000000000000 ) ) ;
#28862 = ORIENTED_EDGE ( 'NONE', *, *, #61978, .T. ) ;
#28863 = CARTESIAN_POINT ( 'NONE',  ( -97.64999999999996305, -209.9999999999999716, 84.28499999999999659 ) ) ;
#28864 = ORIENTED_EDGE ( 'NONE', *, *, #61789, .T. ) ;
#28865 = CARTESIAN_POINT ( 'NONE',  ( -92.35000000000003695, 90.00000000000004263, 89.12687500173430521 ) ) ;
#28866 = CARTESIAN_POINT ( 'NONE',  ( -93.84685191531254134, 91.99731107132950569, 80.69989583420047552 ) ) ;
#28867 = ADVANCED_FACE ( 'NONE', ( #70296 ), #48857, .F. ) ;
#28868 = CARTESIAN_POINT ( 'NONE',  ( 92.69370383062498320, 90.00000000000002842, 89.80156250086714920 ) ) ;
#28869 = ORIENTED_EDGE ( 'NONE', *, *, #11520, .T. ) ;
#28870 = LINE ( 'NONE', #51421, #26160 ) ;
#28871 = DIRECTION ( 'NONE',  ( 0.000000000000000000, 0.000000000000000000, 1.000000000000000000 ) ) ;
#28872 = CARTESIAN_POINT ( 'NONE',  ( 92.35000000000000853, -209.9999999999999716, 85.55499999999999261 ) ) ;
#28873 = DIRECTION ( 'NONE',  ( 1.000000000000000000, 0.000000000000000000, 0.000000000000000000 ) ) ;
#28874 = VERTEX_POINT ( 'NONE', #36839 ) ;
#28875 = DIRECTION ( 'NONE',  ( 0.000000000000000000, -0.7431448254773878048, 0.6691306063588654540 ) ) ;
#28876 = VECTOR ( 'NONE', #42053, 1000.000000000000114 ) ;
#28877 = CARTESIAN_POINT ( 'NONE',  ( -93.84685191531248449, -208.0026889286704943, 78.00114583420048575 ) ) ;
#28878 = ORIENTED_EDGE ( 'NONE', *, *, #30469, .F. ) ;
#28879 = EDGE_LOOP ( 'NONE', ( #33830, #23488, #44793, #72179 ) ) ;
#28880 = DIRECTION ( 'NONE',  ( -1.000000000000000000, 0.000000000000000000, -0.000000000000000000 ) ) ;
#28881 = EDGE_CURVE ( 'NONE', #10255, #28789, #67040, .T. ) ;
#28882 = VERTEX_POINT ( 'NONE', #19909 ) ;
#28883 = EDGE_CURVE ( 'NONE', #1244, #13145, #65066, .T. ) ;
#28884 = DIRECTION ( 'NONE',  ( 0.000000000000000000, 0.000000000000000000, 1.000000000000000000 ) ) ;
#28885 = DIRECTION ( 'NONE',  ( 1.000000000000000000, 0.000000000000000000, 0.000000000000000000 ) ) ;
#28886 = ORIENTED_EDGE ( 'NONE', *, *, #20562, .F. ) ;
#28887 = CARTESIAN_POINT ( 'NONE',  ( -92.69370383062498320, -208.6684592857803011, 76.04322916753380923 ) ) ;
#28888 = ORIENTED_EDGE ( 'NONE', *, *, #17902, .T. ) ;
#28889 = CYLINDRICAL_SURFACE ( 'NONE', #68667, 31.99999999999999289 ) ;
#28890 = CYLINDRICAL_SURFACE ( 'NONE', #4491, 82.00000000000000000 ) ;
#28891 = DIRECTION ( 'NONE',  ( 1.000000000000000000, 0.000000000000000000, 0.000000000000000000 ) ) ;
#28892 = ORIENTED_EDGE ( 'NONE', *, *, #25693, .T. ) ;
#28893 = AXIS2_PLACEMENT_3D ( 'NONE', #39448, #16888, #62391 ) ;
#28894 = CYLINDRICAL_SURFACE ( 'NONE', #5470, 82.00000000000000000 ) ;
#28896 = CARTESIAN_POINT ( 'NONE',  ( 97.30629616937498838, 88.66845928578035796, 86.09739583420048348 ) ) ;
#28895 = AXIS2_PLACEMENT_3D ( 'NONE', #20167, #71293, #48014 ) ;
#28897 = CARTESIAN_POINT ( 'NONE',  ( -93.67499999999998295, -212.2949673200287179, 83.86166666666666458 ) ) ;
#28898 = CARTESIAN_POINT ( 'NONE',  ( -97.30629616937501680, 90.00000000000004263, 89.64281250086713726 ) ) ;
#28899 = DIRECTION ( 'NONE',  ( -1.000000000000000000, 0.000000000000000000, 0.000000000000000000 ) ) ;
#28900 = DIRECTION ( 'NONE',  ( -1.000000000000000000, 0.000000000000000000, 0.000000000000000000 ) ) ;
#28901 = DIRECTION ( 'NONE',  ( 1.000000000000000000, -0.000000000000000000, -0.000000000000000000 ) ) ;
#28902 = CARTESIAN_POINT ( 'NONE',  ( 93.67500000000001137, -212.2949673200287179, 87.64520833506762187 ) ) ;
#28903 = CARTESIAN_POINT ( 'NONE',  ( 12.49999999999999645, 0.000000000000000000, -175.0000000000000000 ) ) ;
#28904 = CARTESIAN_POINT ( 'NONE',  ( 5.000000000000002665, -80.55351364060599906, 15.33399622253456585 ) ) ;
#28905 = VECTOR ( 'NONE', #43969, 1000.000000000000000 ) ;
#28906 = DIRECTION ( 'NONE',  ( -1.000000000000000000, -0.000000000000000000, -0.000000000000000000 ) ) ;
#28907 = LINE ( 'NONE', #45480, #1784 ) ;
#28908 = VECTOR ( 'NONE', #22796, 1000.000000000000000 ) ;
#28909 = CARTESIAN_POINT ( 'NONE',  ( 0.000000000000000000, -64.81221759200306565, -50.23322058963418613 ) ) ;
#28910 = VECTOR ( 'NONE', #4114, 1000.000000000000000 ) ;
#28911 = CIRCLE ( 'NONE', #38525, 31.99999999999998934 ) ;
#28912 = EDGE_CURVE ( 'NONE', #25862, #34228, #68347, .T. ) ;
#28913 = DIRECTION ( 'NONE',  ( 0.000000000000000000, 0.000000000000000000, -1.000000000000000000 ) ) ;
#28914 = CARTESIAN_POINT ( 'NONE',  ( -92.35000000000003695, 90.00000000000004263, 76.98250000000000171 ) ) ;
#28915 = CARTESIAN_POINT ( 'NONE',  ( 7.999999999999991118, -2.038709499516292069E-13, -20.20000000000036167 ) ) ;
#28916 = DIRECTION ( 'NONE',  ( 1.000000000000000000, 0.000000000000000000, 0.000000000000000000 ) ) ;
#28917 = PLANE ( 'NONE',  #31773 ) ;
#28918 = CARTESIAN_POINT ( 'NONE',  ( 0.000000000000000000, -68.55367621811174672, 44.99326035066030727 ) ) ;
#28919 = CARTESIAN_POINT ( 'NONE',  ( 93.84685191531249870, -208.0026889286704943, 86.52072916753382970 ) ) ;
#28920 = EDGE_LOOP ( 'NONE', ( #60015, #23618, #45403, #52808 ) ) ;
#28921 = ADVANCED_FACE ( 'NONE', ( #7540 ), #36467, .T. ) ;
#28922 = VERTEX_POINT ( 'NONE', #8651 ) ;
#28923 = EDGE_CURVE ( 'NONE', #18767, #19565, #7899, .T. ) ;
#28924 = LINE ( 'NONE', #17277, #63175 ) ;
#28925 = EDGE_LOOP ( 'NONE', ( #57232, #58744, #56972, #67341 ) ) ;
#28926 = PLANE ( 'NONE',  #49773 ) ;
#28927 = CARTESIAN_POINT ( 'NONE',  ( 10.00000000000000000, 21.32104025579158701, -30.84782396557194772 ) ) ;
#28928 = ORIENTED_EDGE ( 'NONE', *, *, #50465, .T. ) ;
#28929 = CARTESIAN_POINT ( 'NONE',  ( 92.69370383062501162, -211.3315407142195852, 82.23447916753383424 ) ) ;
#28930 = EDGE_CURVE ( 'NONE', #7986, #55747, #52719, .T. ) ;
#28931 = EDGE_CURVE ( 'NONE', #11579, #68891, #4716, .T. ) ;
#28932 = VECTOR ( 'NONE', #21681, 1000.000000000000000 ) ;
#28933 = AXIS2_PLACEMENT_3D ( 'NONE', #38861, #74178, #49756 ) ;
#28934 = VERTEX_POINT ( 'NONE', #48132 ) ;
#28935 = DIRECTION ( 'NONE',  ( -1.000000000000000000, -0.000000000000000000, -0.000000000000000000 ) ) ;
#28936 = ORIENTED_EDGE ( 'NONE', *, *, #68375, .F. ) ;
#28937 = CIRCLE ( 'NONE', #70947, 37.49900000000000233 ) ;
#28938 = ORIENTED_EDGE ( 'NONE', *, *, #22344, .F. ) ;
#28939 = DIRECTION ( 'NONE',  ( 0.000000000000000000, 0.000000000000000000, 1.000000000000000000 ) ) ;
#28940 = CARTESIAN_POINT ( 'NONE',  ( 0.000000000000000000, 0.000000000000000000, -6.000000000000000000 ) ) ;
#28941 = VERTEX_POINT ( 'NONE', #13171 ) ;
#28942 = CARTESIAN_POINT ( 'NONE',  ( 92.35000000039376289, -209.9999706925934504, 76.74344264317686282 ) ) ;
#28943 = CARTESIAN_POINT ( 'NONE',  ( 92.35000000000002274, -211.5299782133524502, 86.95729166840096980 ) ) ;
#28944 = ORIENTED_EDGE ( 'NONE', *, *, #883, .T. ) ;
#28945 = DIRECTION ( 'NONE',  ( -1.000000000000000000, 0.000000000000000000, -0.000000000000000000 ) ) ;
#28946 = ORIENTED_EDGE ( 'NONE', *, *, #67726, .T. ) ;
#28947 = CARTESIAN_POINT ( 'NONE',  ( 5.000000000000000888, -2.886751345948134873, -2.080000000000000071 ) ) ;
#28948 = ADVANCED_FACE ( 'NONE', ( #42495 ), #71044, .T. ) ;
#28949 = EDGE_LOOP ( 'NONE', ( #57525, #29495, #68705, #24419 ) ) ;
#28950 = AXIS2_PLACEMENT_3D ( 'NONE', #59689, #59315, #71312 ) ;
#28951 = VERTEX_POINT ( 'NONE', #59050 ) ;
#28952 = ORIENTED_EDGE ( 'NONE', *, *, #60687, .T. ) ;
#28953 = DIRECTION ( 'NONE',  ( 1.000000000000000000, 0.000000000000000000, 0.000000000000000000 ) ) ;
#28954 = AXIS2_PLACEMENT_3D ( 'NONE', #63669, #12138, #69660 ) ;
#28955 = DIRECTION ( 'NONE',  ( 0.000000000000000000, 0.000000000000000000, -1.000000000000000000 ) ) ;
#28956 = EDGE_LOOP ( 'NONE', ( #7402, #69561, #12091, #63629 ) ) ;
#28957 = ORIENTED_EDGE ( 'NONE', *, *, #4812, .F. ) ;
#28958 = ORIENTED_EDGE ( 'NONE', *, *, #23625, .T. ) ;
#28959 = CARTESIAN_POINT ( 'NONE',  ( -23.50044424985255276, 0.001194404164626844313, -64.00000000000000000 ) ) ;
#28960 = VECTOR ( 'NONE', #7822, 1000.000000000000000 ) ;
#28961 = DIRECTION ( 'NONE',  ( -1.000000000000000000, 0.000000000000000000, 0.000000000000000000 ) ) ;
#28962 = CARTESIAN_POINT ( 'NONE',  ( -97.65000000000001990, 90.00000000000004263, 88.73000000000000398 ) ) ;
#28963 = ADVANCED_FACE ( 'NONE', ( #59790 ), #31198, .F. ) ;
#28964 = ORIENTED_EDGE ( 'NONE', *, *, #39471, .F. ) ;
#28965 = DIRECTION ( 'NONE',  ( 2.603472992746261562E-14, 2.546204323184492723E-14, -1.000000000000000000 ) ) ;
#28966 = AXIS2_PLACEMENT_3D ( 'NONE', #54163, #25577, #43988 ) ;
#28967 = ORIENTED_EDGE ( 'NONE', *, *, #30646, .F. ) ;
#28968 = CARTESIAN_POINT ( 'NONE',  ( 0.000000000000000000, -41.91543099594819921, 2.663952781846001816 ) ) ;
#28969 = CARTESIAN_POINT ( 'NONE',  ( -92.69370383062498320, -209.9999999999999716, 85.51531250086713953 ) ) ;
#28970 = ORIENTED_EDGE ( 'NONE', *, *, #30068, .F. ) ;
#28971 = ADVANCED_FACE ( 'NONE', ( #38329 ), #49962, .T. ) ;
#28972 = DIRECTION ( 'NONE',  ( 0.000000000000000000, 0.000000000000000000, 1.000000000000000000 ) ) ;
#28973 = CARTESIAN_POINT ( 'NONE',  ( 92.55058773059857913, -210.6792855350292086, 74.93153462041254897 ) ) ;
#28974 = CARTESIAN_POINT ( 'NONE',  ( 11.99999999999999822, 68.67312586195046720, -35.91791733033404199 ) ) ;
#28975 = CARTESIAN_POINT ( 'NONE',  ( -97.30629616937497417, -211.3315407142195852, 76.99572916753380980 ) ) ;
#28976 = DIRECTION ( 'NONE',  ( 2.603472992746261562E-14, 2.546204323184492723E-14, -1.000000000000000000 ) ) ;
#28977 = CARTESIAN_POINT ( 'NONE',  ( 10.00000000000000000, 0.000000000000000000, 0.000000000000000000 ) ) ;
#28978 = DIRECTION ( 'NONE',  ( 1.000000000000000000, 0.000000000000000000, -0.000000000000000000 ) ) ;
#28979 = LINE ( 'NONE', #51911, #42334 ) ;
#28980 = DIRECTION ( 'NONE',  ( 0.000000000000000000, 0.5877852522924685852, 0.8090169943749507819 ) ) ;
#28981 = CARTESIAN_POINT ( 'NONE',  ( -93.84685191531252713, 88.00268892867056536, 77.15447916753380753 ) ) ;
#28982 = CARTESIAN_POINT ( 'NONE',  ( 11.99999999999999822, 3.894527615419054456, -81.90746397400384637 ) ) ;
#28983 = CARTESIAN_POINT ( 'NONE',  ( 1.560000000000000053, 0.000000000000000000, 2.999999999999998668 ) ) ;
#28984 = ORIENTED_EDGE ( 'NONE', *, *, #31632, .F. ) ;
#28985 = CARTESIAN_POINT ( 'NONE',  ( 92.35000000007821086, 90.00001303125209517, 79.28395951162845279 ) ) ;
#28986 = VECTOR ( 'NONE', #46729, 1000.000000000000114 ) ;
#28987 = VECTOR ( 'NONE', #73634, 1000.000000000000000 ) ;
#28988 = DIRECTION ( 'NONE',  ( 0.000000000000000000, -0.1564344650402381687, 0.9876883405951365491 ) ) ;
#28989 = DIRECTION ( 'NONE',  ( 0.000000000000000000, 0.000000000000000000, 1.000000000000000000 ) ) ;
#28990 = CARTESIAN_POINT ( 'NONE',  ( 10.00000000000000000, 35.91791733033570466, -68.67312586194960033 ) ) ;
#28991 = CARTESIAN_POINT ( 'NONE',  ( -22.67106064244953245, -113.6342314410295842, -5.500000000000000000 ) ) ;
#28992 = CARTESIAN_POINT ( 'NONE',  ( -93.67500000000003979, 92.29496732002878900, 85.42270833506762528 ) ) ;
#28993 = CARTESIAN_POINT ( 'NONE',  ( -97.64999999999994884, -208.4700217866474645, 89.94708333333333883 ) ) ;
#28994 = AXIS2_PLACEMENT_3D ( 'NONE', #49849, #50974, #73522 ) ;
#28995 = DIRECTION ( 'NONE',  ( -1.000000000000000000, -0.000000000000000000, 0.000000000000000000 ) ) ;
#28996 = ORIENTED_EDGE ( 'NONE', *, *, #388, .T. ) ;
#28997 = PLANE ( 'NONE',  #65909 ) ;
#28998 = DIRECTION ( 'NONE',  ( 0.000000000000000000, -0.8910065241883626808, -0.4539904997395570740 ) ) ;
#28999 = SURFACE_SIDE_STYLE ('',( #52675 ) ) ;
#29000 = CARTESIAN_POINT ( 'NONE',  ( 16.84844760790522855, -103.5491698323862124, 2.500000000000000000 ) ) ;
#29001 = EDGE_CURVE ( 'NONE', #16368, #8743, #55134, .T. ) ;
#29002 = AXIS2_PLACEMENT_3D ( 'NONE', #49404, #41921, #7704 ) ;
#29003 = CIRCLE ( 'NONE', #69845, 16.00000000000000000 ) ;
#29004 = VECTOR ( 'NONE', #64893, 1000.000000000000000 ) ;
#29005 = EDGE_CURVE ( 'NONE', #3846, #28823, #16140, .T. ) ;
#29006 = DIRECTION ( 'NONE',  ( 0.000000000000000000, 0.000000000000000000, 1.000000000000000000 ) ) ;
#29007 = VERTEX_POINT ( 'NONE', #43616 ) ;
#29009 = EDGE_CURVE ( 'NONE', #64475, #56506, #8281, .T. ) ;
#29008 = LINE ( 'NONE', #62509, #39658 ) ;
#29010 = CARTESIAN_POINT ( 'NONE',  ( 10.00000000000000000, 0.000000000000000000, 0.000000000000000000 ) ) ;
#29011 = ORIENTED_EDGE ( 'NONE', *, *, #19674, .F. ) ;
#29012 =( BOUNDED_CURVE ( )  B_SPLINE_CURVE ( 2, ( #51206, #39942, #10614, #45214, #17734, #11354, #496 ),
 .UNSPECIFIED., .F., .F. ) 
 B_SPLINE_CURVE_WITH_KNOTS ( ( 3, 2, 2, 3 ),
 ( 0.02083333333333322115, 0.02777777777777762705, 0.03472222222222204335, 0.04166666666666644231 ),
 .UNSPECIFIED. ) 
 CURVE ( )  GEOMETRIC_REPRESENTATION_ITEM ( )  RATIONAL_B_SPLINE_CURVE ( ( 1.000000000000002220, 0.8660254037844365982, 1.000000000000000000, 0.8660254037844387076, 1.000000000000000000, 0.8660254037844430375, 0.9999999999999956701 ) ) 
 REPRESENTATION_ITEM ( '' )  );
#29013 = CARTESIAN_POINT ( 'NONE',  ( 97.30629616937498838, -211.3315407142195852, 88.00239583420047040 ) ) ;
#29014 = ORIENTED_EDGE ( 'NONE', *, *, #34709, .T. ) ;
#29015 = ADVANCED_FACE ( 'NONE', ( #20665 ), #39078, .F. ) ;
#29016 = ORIENTED_EDGE ( 'NONE', *, *, #51088, .F. ) ;
#29017 = CARTESIAN_POINT ( 'NONE',  ( -7.400000000000003908, -1.056673655988042765E-14, -5.892267102755452808E-15 ) ) ;
#29018 = ORIENTED_EDGE ( 'NONE', *, *, #48396, .F. ) ;
#29019 = DIRECTION ( 'NONE',  ( -1.000000000000000000, -0.000000000000000000, 0.000000000000000000 ) ) ;
#29020 = ORIENTED_EDGE ( 'NONE', *, *, #59741, .F. ) ;
#29021 = LINE ( 'NONE', #21237, #10500 ) ;
#29022 = VERTEX_POINT ( 'NONE', #15387 ) ;
#29023 = VERTEX_POINT ( 'NONE', #60894 ) ;
#29024 = CARTESIAN_POINT ( 'NONE',  ( 10.00000000000000000, -41.19522573413687638, -65.64334221924953283 ) ) ;
#29025 = ORIENTED_EDGE ( 'NONE', *, *, #46371, .T. ) ;
#29026 = ADVANCED_FACE ( 'NONE', ( #66538 ), #37959, .T. ) ;
#29027 = ORIENTED_EDGE ( 'NONE', *, *, #66046, .F. ) ;
#29028 =( BOUNDED_CURVE ( )  B_SPLINE_CURVE ( 2, ( #50971, #5130, #62266, #33674, #38585, #10750, #17132 ),
 .UNSPECIFIED., .F., .F. ) 
 B_SPLINE_CURVE_WITH_KNOTS ( ( 3, 2, 2, 3 ),
 ( 0.4166666666666662966, 0.4236111111111106609, 0.4305555555555550806, 0.4374999999999994449 ),
 .UNSPECIFIED. ) 
 CURVE ( )  GEOMETRIC_REPRESENTATION_ITEM ( )  RATIONAL_B_SPLINE_CURVE ( ( 1.000000000000007550, 0.8660254037844311581, 1.000000000000000000, 0.8660254037844387076, 1.000000000000000000, 0.8660254037844493658, 0.9999999999999893419 ) ) 
 REPRESENTATION_ITEM ( '' )  );
#29029 = CARTESIAN_POINT ( 'NONE',  ( 92.98340954502093325, 88.39448418669219620, 74.95309847082319266 ) ) ;
#29030 = EDGE_CURVE ( 'NONE', #28223, #20209, #71912, .T. ) ;
#29031 = ADVANCED_FACE ( 'NONE', ( #62013 ), #4508, .T. ) ;
#29032 = EDGE_LOOP ( 'NONE', ( #50297, #39873, #13935, #26069 ) ) ;
#29033 = VECTOR ( 'NONE', #13884, 1000.000000000000000 ) ;
#29034 = VERTEX_POINT ( 'NONE', #10492 ) ;
#29035 = CARTESIAN_POINT ( 'NONE',  ( 93.84685191531248449, 88.00268892867053694, 85.30364583420046642 ) ) ;
#29037 = ORIENTED_EDGE ( 'NONE', *, *, #27903, .T. ) ;
#29036 = ADVANCED_FACE ( 'NONE', ( #49229 ), #71780, .T. ) ;
#29038 = CARTESIAN_POINT ( 'NONE',  ( 92.69370383062501162, -211.3315407142195852, 81.44072916753381719 ) ) ;
#29039 = APPLICATION_PROTOCOL_DEFINITION ( 'draft international standard', 'automotive_design', 1998, #64237 ) ;
#29040 = CARTESIAN_POINT ( 'NONE',  ( -10.00000000000000000, 0.000000000000000000, 0.000000000000000000 ) ) ;
#29042 = CARTESIAN_POINT ( 'NONE',  ( -94.60587738269659042, -212.6434372237803530, 75.00000000000001421 ) ) ;
#29041 = AXIS2_PLACEMENT_3D ( 'NONE', #27498, #22239, #10960 ) ;
#29043 = CARTESIAN_POINT ( 'NONE',  ( 11.99999999999999822, -73.72996012237449293, 14.67089635893687571 ) ) ;
#29044 = CARTESIAN_POINT ( 'NONE',  ( 0.000000000000000000, -60.67117009219096957, -55.16347631943106933 ) ) ;
#29045 = DIRECTION ( 'NONE',  ( 0.000000000000000000, 0.7604059656000276002, 0.6494480483301875440 ) ) ;
#29046 = DIRECTION ( 'NONE',  ( 0.000000000000000000, 0.000000000000000000, 1.000000000000000000 ) ) ;
#29047 = CARTESIAN_POINT ( 'NONE',  ( -92.69370383062498320, -209.9999999999999716, 85.51531250086713953 ) ) ;
#29048 = CARTESIAN_POINT ( 'NONE',  ( -96.15314808468751551, 88.00268892867056536, 82.92239583420048632 ) ) ;
#29049 = VECTOR ( 'NONE', #1928, 1000.000000000000000 ) ;
#29050 = EDGE_CURVE ( 'NONE', #33020, #66879, #56321, .T. ) ;
#29051 = ORIENTED_EDGE ( 'NONE', *, *, #22094, .F. ) ;
#29053 = CARTESIAN_POINT ( 'NONE',  ( -97.30629616937501680, 88.66845928578038638, 85.25072916753379104 ) ) ;
#29052 = CARTESIAN_POINT ( 'NONE',  ( 97.30629616937498838, 91.33154071421968467, 84.93322916753379559 ) ) ;
#29054 = VECTOR ( 'NONE', #33661, 1000.000000000000000 ) ;
#29055 = EDGE_LOOP ( 'NONE', ( #44842, #71627 ) ) ;
#29056 = CARTESIAN_POINT ( 'NONE',  ( -93.67500000000003979, 92.29496732002878900, 87.88333333333332575 ) ) ;
#29057 = CARTESIAN_POINT ( 'NONE',  ( 10.00000000000000000, -36.13751322684434797, 21.40280677340358295 ) ) ;
#29058 = PLANE ( 'NONE',  #23529 ) ;
#29059 = CARTESIAN_POINT ( 'NONE',  ( 0.000000000000000000, 15.48615015657581750, 39.04073710021349797 ) ) ;
#29060 = CARTESIAN_POINT ( 'NONE',  ( -94.99999999999997158, -212.6630814284392557, 87.89656250086713385 ) ) ;
#29061 = DIRECTION ( 'NONE',  ( -1.000000000000000000, -0.000000000000000000, 0.000000000000000000 ) ) ;
#29062 = CARTESIAN_POINT ( 'NONE',  ( 10.00000000000000000, 37.16516213103277977, 4.992566952385115719 ) ) ;
#29063 = DIRECTION ( 'NONE',  ( -0.000000000000000000, -0.000000000000000000, 1.000000000000000000 ) ) ;
#29064 = CIRCLE ( 'NONE', #12202, 77.49899999999999523 ) ;
#29065 = CARTESIAN_POINT ( 'NONE',  ( 10.00000000000000000, -35.38097989696520074, 12.42422080174625520 ) ) ;
#29066 = VERTEX_POINT ( 'NONE', #72522 ) ;
#29067 = ORIENTED_EDGE ( 'NONE', *, *, #65667, .F. ) ;
#29068 = CARTESIAN_POINT ( 'NONE',  ( -95.00000000000002842, 86.94004357329504273, 76.82374999999998977 ) ) ;
#29069 = CARTESIAN_POINT ( 'NONE',  ( 92.35000000000012221, -211.5299782133525071, 88.78291666666667936 ) ) ;
#29070 = CYLINDRICAL_SURFACE ( 'NONE', #1034, 2.649999999999985700 ) ;
#29071 = CARTESIAN_POINT ( 'NONE',  ( 11.99999999999999822, -51.03279382321125723, 55.19960302592048862 ) ) ;
#29072 = LINE ( 'NONE', #52000, #57827 ) ;
#29073 = LINE ( 'NONE', #70389, #10804 ) ;
#29074 = ORIENTED_EDGE ( 'NONE', *, *, #26287, .F. ) ;
#29075 = CARTESIAN_POINT ( 'NONE',  ( -97.30629616937501680, 90.00000000000004263, 78.84781250086714977 ) ) ;
#29076 = DIRECTION ( 'NONE',  ( 0.000000000000000000, -0.07845909572783056618, -0.9969173337331290741 ) ) ;
#29077 = DIRECTION ( 'NONE',  ( -1.000000000000000000, 0.000000000000000000, 0.000000000000000000 ) ) ;
#29078 = DIRECTION ( 'NONE',  ( -1.000000000000000000, -0.000000000000000000, -0.000000000000000000 ) ) ;
#29079 = DIRECTION ( 'NONE',  ( 0.000000000000000000, -0.9135454576426010886, 0.4067366430757998752 ) ) ;
#29080 = CARTESIAN_POINT ( 'NONE',  ( -97.30629616937497417, -208.6684592857803011, 85.93864583420048575 ) ) ;
#29081 = CARTESIAN_POINT ( 'NONE',  ( 93.84685191531248449, 88.00268892867053694, 75.93739583420048689 ) ) ;
#29082 = EDGE_CURVE ( 'NONE', #8991, #66021, #55986, .T. ) ;
#29083 = CARTESIAN_POINT ( 'NONE',  ( -96.15314808468747287, -208.0026889286704943, 81.44072916753381719 ) ) ;
#29084 = CARTESIAN_POINT ( 'NONE',  ( -96.32500000000001705, 92.29496732002878900, 84.89354166840095672 ) ) ;
#29085 = ORIENTED_EDGE ( 'NONE', *, *, #45583, .T. ) ;
#29086 = CARTESIAN_POINT ( 'NONE',  ( 15.00000000000000000, 9.615535125378766423, -24.73947219025917121 ) ) ;
#29087 = CARTESIAN_POINT ( 'NONE',  ( -94.46769236096045574, -213.2667778271279246, 74.92222617501695936 ) ) ;
#29088 = CARTESIAN_POINT ( 'NONE',  ( 93.67500000000001137, -212.2949673200287179, 78.75520833506763552 ) ) ;
#29089 = EDGE_CURVE ( 'NONE', #961, #16368, #21025, .T. ) ;
#29090 = CIRCLE ( 'NONE', #48314, 16.00000000000000000 ) ;
#29091 = EDGE_CURVE ( 'NONE', #66590, #23737, #11868, .T. ) ;
#29092 = EDGE_CURVE ( 'NONE', #37544, #71894, #15521, .T. ) ;
#29093 = DIRECTION ( 'NONE',  ( 1.000000000000000000, 0.000000000000000000, 0.000000000000000000 ) ) ;
#29094 = CARTESIAN_POINT ( 'NONE',  ( 97.30629616937498838, -208.6684592857803011, 77.31322916753380525 ) ) ;
#29095 = ORIENTED_EDGE ( 'NONE', *, *, #6372, .F. ) ;
#29096 = AXIS2_PLACEMENT_3D ( 'NONE', #28143, #10862, #57106 ) ;
#29097 = DIRECTION ( 'NONE',  ( 0.000000000000000000, 0.000000000000000000, 1.000000000000000000 ) ) ;
#29098 = VERTEX_POINT ( 'NONE', #37596 ) ;
#29099 = VECTOR ( 'NONE', #17593, 1000.000000000000114 ) ;
#29100 = EDGE_CURVE ( 'NONE', #31915, #64655, #31935, .T. ) ;
#29101 = CARTESIAN_POINT ( 'NONE',  ( 2.949999999999999734, 0.000000000000000000, 0.000000000000000000 ) ) ;
#29102 = ORIENTED_EDGE ( 'NONE', *, *, #7744, .T. ) ;
#29103 = ADVANCED_FACE ( 'NONE', ( #23273 ), #33803, .T. ) ;
#29104 = AXIS2_PLACEMENT_3D ( 'NONE', #1056, #5564, #58154 ) ;
#29105 = DIRECTION ( 'NONE',  ( 0.000000000000000000, 1.000000000000000000, 1.301042606982602757E-15 ) ) ;
#29106 = VECTOR ( 'NONE', #19178, 1000.000000000000000 ) ;
#29107 = VERTEX_POINT ( 'NONE', #46566 ) ;
#29108 = ORIENTED_EDGE ( 'NONE', *, *, #19501, .T. ) ;
#29109 = ORIENTED_EDGE ( 'NONE', *, *, #56901, .F. ) ;
#29110 = DIRECTION ( 'NONE',  ( 0.000000000000000000, 0.000000000000000000, 1.000000000000000000 ) ) ;
#29111 = ORIENTED_EDGE ( 'NONE', *, *, #37171, .F. ) ;
#29112 = ORIENTED_EDGE ( 'NONE', *, *, #32603, .T. ) ;
#29113 = CARTESIAN_POINT ( 'NONE',  ( 94.99999999999998579, 87.33691857156068750, 84.24531250086715772 ) ) ;
#29114 = EDGE_CURVE ( 'NONE', #26992, #46185, #62777, .T. ) ;
#29115 = DIRECTION ( 'NONE',  ( -1.000000000000000000, -0.000000000000000000, 0.000000000000000000 ) ) ;
#29116 = EDGE_LOOP ( 'NONE', ( #9296, #11635, #56965, #21436, #24967, #74072 ) ) ;
#29117 = ORIENTED_EDGE ( 'NONE', *, *, #13728, .F. ) ;
#29118 = ORIENTED_EDGE ( 'NONE', *, *, #38810, .F. ) ;
#29119 = EDGE_LOOP ( 'NONE', ( #49093, #20085, #46831, #15841 ) ) ;
#29120 = CARTESIAN_POINT ( 'NONE',  ( 11.99999999999999822, 11.30684508768450769, -76.66974797899825944 ) ) ;
#29121 = EDGE_CURVE ( 'NONE', #18110, #69032, #11975, .T. ) ;
#29122 = ADVANCED_FACE ( 'NONE', ( #46205 ), #16509, .T. ) ;
#29123 = DIRECTION ( 'NONE',  ( 1.000000000000000000, 0.000000000000000000, 0.000000000000000000 ) ) ;
#29124 = CARTESIAN_POINT ( 'NONE',  ( -92.35000000000003695, 90.00000000000004263, 87.77749999999998920 ) ) ;
#29125 = FACE_OUTER_BOUND ( 'NONE', #35866, .T. ) ;
#29126 = CARTESIAN_POINT ( 'NONE',  ( 10.00000000000000000, 30.84782396557218931, 21.32104025579126017 ) ) ;
#29127 = CARTESIAN_POINT ( 'NONE',  ( 93.67500000000001137, -212.2949673200287179, 82.56520833506762358 ) ) ;
#29128 = DIRECTION ( 'NONE',  ( -0.000000000000000000, -0.9945218953682741780, 0.1045284632676447834 ) ) ;
#29129 = CARTESIAN_POINT ( 'NONE',  ( 94.99999999999998579, 90.00000000000002842, 90.00000000000000000 ) ) ;
#29130 = ORIENTED_EDGE ( 'NONE', *, *, #43843, .T. ) ;
#29131 = CARTESIAN_POINT ( 'NONE',  ( -92.34999999999999432, -208.4700217866474645, 79.65479166840096070 ) ) ;
#29132 = ORIENTED_EDGE ( 'NONE', *, *, #47109, .F. ) ;
#29133 = DIRECTION ( 'NONE',  ( -1.000000000000000000, 0.000000000000000000, -0.000000000000000000 ) ) ;
#29134 = EDGE_CURVE ( 'NONE', #3531, #12759, #34536, .T. ) ;
#29135 = VERTEX_POINT ( 'NONE', #29256 ) ;
#29137 = CARTESIAN_POINT ( 'NONE',  ( -96.32500000000001705, 87.70503267997129626, 79.39020833506762642 ) ) ;
#29136 = CARTESIAN_POINT ( 'NONE',  ( 97.64999999999997726, 91.52997821335252127, 79.65479166840096070 ) ) ;
#29138 = EDGE_LOOP ( 'NONE', ( #8765, #9355, #33214, #58187, #38276, #84, #5003, #35253, #13459, #59932, #72320, #24877, #65358, #15539, #8200, #50857, #24795, #52047, #44864, #57439, #13119, #65479, #32801, #66373, #1294, #29520, #53723, #14378, #41306, #61332, #5938, #38202, #3740, #7669, #34773, #48083, #73315, #58786, #49364, #38384, #56080, #38748, #28271, #67889, #69971, #69101, #15202, #38378, #1048, #46816, #55702, #70906, #20803, #62529, #55376, #57537, #32550, #18480, #30497, #28888, #11287, #72426, #37561, #42638, #60991, #10677, #70149, #64225, #14506, #1902, #21672, #54191, #40308, #59656, #8030, #60007, #42201, #9499, #32069, #41990, #53243, #38, #21984, #36036, #15069, #20921, #34407, #3358, #62148, #44313, #59844, #41330, #28360, #262, #41970, #37447, #71210, #26614, #56412, #58259, #46725, #40164, #3106, #68438, #803, #36446, #52839, #73616, #26367, #69195, #12182, #5036, #45818, #9990, #20963, #22852, #4421, #35005, #32693, #56149, #35196, #25363, #39575, #53991, #15343, #6747, #34893, #32366, #13128, #35884, #1907, #10331, #19676, #22487, #20615, #18641, #50468, #45586, #66518, #1063, #10663, #38963, #6589, #3236, #21458, #35663, #7513, #68976, #24047, #599, #3656, #71541, #50572, #57611, #48272, #67368, #62243, #25832, #52974, #17566, #9605, #21991, #47418, #64556, #35991, #11651, #10730, #50082, #9124, #70380, #64623, #5368, #68751, #69468, #45128, #10853, #69020, #72384, #58467, #52881, #60560, #30118, #20892, #49731, #41, #2165, #73346, #51962, #39859, #48482, #61529, #17974, #50779, #18107, #37738, #48830, #60931, #14295, #23622, #5279, #7866, #34127, #56039, #29663, #28749, #54107, #51373, #54799, #65037, #1971, #65331, #45598, #65475, #44782, #57775, #43499, #21074, #49890, #73674, #13430, #6486, #57083, #35044, #33980, #68717, #70096, #15902, #52179, #5111, #48722, #9513, #49013, #71875, #65392, #39581, #49501, #37929, #3089, #64096, #30408, #21815, #4091, #59155, #34106, #46525, #20353, #67350, #64744, #4934, #30596, #46952, #9527, #64413, #60204, #55499, #12304, #21905, #57092, #65936, #72078, #52335, #39704, #71827, #12432, #52034, #30750, #17404, #51586, #48750, #43131, #65039, #68704, #49661, #5090, #25231, #41343, #11837, #1700, #28102, #3095, #40134, #32876, #2984, #42998, #64194, #51297, #49441, #12215, #8886, #62029, #67601, #31634, #57451, #29653, #49027, #34234, #2797, #19756, #972, #30401, #4833, #5510, #24581, #38368, #22597, #1822, #24670, #44468, #12271, #19408, #56400, #9880, #4311, #74175, #10472, #41138, #56113, #4865, #60028, #9549, #73319, #16565, #1189, #53005, #68079 ) ) ;
#29139 = CARTESIAN_POINT ( 'NONE',  ( 92.69370383062498320, 91.33154071421968467, 80.85864583420048746 ) ) ;
#29140 = FACE_OUTER_BOUND ( 'NONE', #44290, .T. ) ;
#29141 = CARTESIAN_POINT ( 'NONE',  ( -92.35000000000005116, 91.52997821335253548, 86.63979166840096013 ) ) ;
#29142 = CARTESIAN_POINT ( 'NONE',  ( 11.99999999999999822, -46.53671651293907274, -59.03961581697448935 ) ) ;
#29143 = PRESENTATION_LAYER_ASSIGNMENT (  '', '', ( #23159 ) ) ;
#29144 = ORIENTED_EDGE ( 'NONE', *, *, #10580, .T. ) ;
#29145 = CARTESIAN_POINT ( 'NONE',  ( 0.000000000000000000, 0.000000000000000000, 0.000000000000000000 ) ) ;
#29146 = CARTESIAN_POINT ( 'NONE',  ( 0.000000000000000000, -22.48208911017474065, -35.47612816024548721 ) ) ;
#29147 = CARTESIAN_POINT ( 'NONE',  ( 5.204170427930421283E-15, 0.000000000000000000, -12.79999999999999893 ) ) ;
#29148 = ORIENTED_EDGE ( 'NONE', *, *, #21301, .F. ) ;
#29149 = VECTOR ( 'NONE', #52035, 1000.000000000000000 ) ;
#29150 = EDGE_LOOP ( 'NONE', ( #1247, #25969, #15062, #49311 ) ) ;
#29151 =( BOUNDED_CURVE ( )  B_SPLINE_CURVE ( 2, ( #4978, #45938, #10218, #15488, #32767, #67742, #55715 ),
 .UNSPECIFIED., .F., .F. ) 
 B_SPLINE_CURVE_WITH_KNOTS ( ( 3, 2, 2, 3 ),
 ( 0.000000000000000000, 0.006944444444444406762, 0.01388888888888881352, 0.02083333333333322115 ),
 .UNSPECIFIED. ) 
 CURVE ( )  GEOMETRIC_REPRESENTATION_ITEM ( )  RATIONAL_B_SPLINE_CURVE ( ( 1.000000000000000000, 0.8660254037844387076, 1.000000000000000000, 0.8660254037844387076, 1.000000000000000000, 0.8660254037844408170, 0.9999999999999978906 ) ) 
 REPRESENTATION_ITEM ( '' )  );
#29152 = CARTESIAN_POINT ( 'NONE',  ( -0.8815729230226008184, -93.47222532549339746, 5.500000000000000000 ) ) ;
#29153 = CARTESIAN_POINT ( 'NONE',  ( 94.99999999999998579, 90.00000000000002842, 90.00000000000000000 ) ) ;
#29154 = LINE ( 'NONE', #1384, #579 ) ;
#29155 = AXIS2_PLACEMENT_3D ( 'NONE', #69377, #56637, #63030 ) ;
#29156 = CARTESIAN_POINT ( 'NONE',  ( -93.84685191531248449, -208.0026889286704943, 76.25489583420049655 ) ) ;
#29157 = ORIENTED_EDGE ( 'NONE', *, *, #48863, .T. ) ;
#29158 = CARTESIAN_POINT ( 'NONE',  ( 0.000000000000000000, 27.74655509720669500, 77.16300072079670258 ) ) ;
#29159 = AXIS2_PLACEMENT_3D ( 'NONE', #20840, #43795, #26848 ) ;
#29160 = CYLINDRICAL_SURFACE ( 'NONE', #33504, 30.50000000000000000 ) ;
#29161 = DIRECTION ( 'NONE',  ( 0.000000000000000000, 0.000000000000000000, 1.000000000000000000 ) ) ;
#29162 = CARTESIAN_POINT ( 'NONE',  ( 97.30629616937498838, 88.66845928578035796, 75.30239583420048177 ) ) ;
#29163 = CARTESIAN_POINT ( 'NONE',  ( 11.99999999999999822, -55.20638768913797634, 51.02545421589302777 ) ) ;
#29164 = CARTESIAN_POINT ( 'NONE',  ( 26.09152095774781444, -124.8716048804687375, 2.500000000000000000 ) ) ;
#29165 = DIRECTION ( 'NONE',  ( 0.000000000000000000, 0.000000000000000000, 1.000000000000000000 ) ) ;
#29166 = FACE_OUTER_BOUND ( 'NONE', #29744, .T. ) ;
#29167 = CARTESIAN_POINT ( 'NONE',  ( 12.83284365640956182, 1.571570090778038719E-15, 0.000000000000000000 ) ) ;
#29168 = DIRECTION ( 'NONE',  ( 0.000000000000000000, -0.1564344650402170744, -0.9876883405951398798 ) ) ;
#29169 = CARTESIAN_POINT ( 'NONE',  ( 97.30629616937498838, 90.00000000000002842, 85.67406250086715147 ) ) ;
#29170 = CARTESIAN_POINT ( 'NONE',  ( -22.67106064244953245, -113.6342314410295842, 5.500000000000000000 ) ) ;
#29171 = CARTESIAN_POINT ( 'NONE',  ( -97.65000000000001990, 90.00000000000004263, 90.00000000000000000 ) ) ;
#29172 = ORIENTED_EDGE ( 'NONE', *, *, #26044, .F. ) ;
#29173 = CARTESIAN_POINT ( 'NONE',  ( 11.99999999999999822, 0.000000000000000000, 0.000000000000000000 ) ) ;
#29174 = CARTESIAN_POINT ( 'NONE',  ( -97.30629616937501680, 90.00000000000004263, 80.11781250086713158 ) ) ;
#29175 = EDGE_CURVE ( 'NONE', #2120, #1262, #28362, .T. ) ;
#29176 = EDGE_CURVE ( 'NONE', #53734, #2347, #5622, .T. ) ;
#29177 = EDGE_CURVE ( 'NONE', #64823, #72774, #73638, .T. ) ;
#29178 = CARTESIAN_POINT ( 'NONE',  ( 93.84685191531249870, -208.0026889286704943, 86.36197916753381776 ) ) ;
#29179 = APPLICATION_CONTEXT ( 'automotive_design' ) ;
#29180 = ORIENTED_EDGE ( 'NONE', *, *, #43119, .F. ) ;
#29181 = CARTESIAN_POINT ( 'NONE',  ( 10.00000000000000000, 17.80606268964585226, -33.00180498840028775 ) ) ;
#29182 = CARTESIAN_POINT ( 'NONE',  ( 97.64999999999997726, -208.4700217866474929, 87.19541666666667368 ) ) ;
#29183 = AXIS2_PLACEMENT_3D ( 'NONE', #43402, #25711, #14797 ) ;
#29184 = CARTESIAN_POINT ( 'NONE',  ( 10.00000000000000000, 0.8261519478431083030, 77.49459641780886443 ) ) ;
#29185 = DIRECTION ( 'NONE',  ( -0.000000000000000000, -0.000000000000000000, 1.000000000000000000 ) ) ;
#29186 = VECTOR ( 'NONE', #38074, 1000.000000000000000 ) ;
#29187 = EDGE_LOOP ( 'NONE', ( #12512, #22934 ) ) ;
#29188 = ORIENTED_EDGE ( 'NONE', *, *, #73427, .F. ) ;
#29189 = EDGE_CURVE ( 'NONE', #53667, #6723, #64391, .T. ) ;
#29190 = CARTESIAN_POINT ( 'NONE',  ( 97.30629616937498838, -209.9999999999999716, 83.13406250086715943 ) ) ;
#29191 = DIRECTION ( 'NONE',  ( -1.000000000000000000, -0.000000000000000000, 0.000000000000000000 ) ) ;
#29192 = DIRECTION ( 'NONE',  ( -0.000000000000000000, -0.000000000000000000, 1.000000000000000000 ) ) ;
#29193 = CIRCLE ( 'NONE', #61638, 31.99999999999998579 ) ;
#29194 = DIRECTION ( 'NONE',  ( 0.9827303690289282967, 0.1850432970638667407, -0.000000000000000000 ) ) ;
#29195 = CARTESIAN_POINT ( 'NONE',  ( 96.32499999999997442, 92.29496732002878900, 83.51770833506763836 ) ) ;
#29196 = CIRCLE ( 'NONE', #73641, 12.75000000000265565 ) ;
#29197 = FACE_OUTER_BOUND ( 'NONE', #21439, .T. ) ;
#29198 = CARTESIAN_POINT ( 'NONE',  ( 97.64999999999997726, -208.4700217866474645, 84.65541666666666742 ) ) ;
#29199 = ORIENTED_EDGE ( 'NONE', *, *, #10421, .T. ) ;
#29200 = ORIENTED_EDGE ( 'NONE', *, *, #27639, .F. ) ;
#29201 = VERTEX_POINT ( 'NONE', #17622 ) ;
#29202 = AXIS2_PLACEMENT_3D ( 'NONE', #44339, #4885, #5249 ) ;
#29203 = ORIENTED_EDGE ( 'NONE', *, *, #34272, .T. ) ;
#29205 = CIRCLE ( 'NONE', #42424, 12.49999999999999645 ) ;
#29204 = PLANE ( 'NONE',  #2247 ) ;
#29206 = EDGE_CURVE ( 'NONE', #2617, #40220, #71120, .T. ) ;
#29208 = EDGE_CURVE ( 'NONE', #45217, #48031, #59923, .T. ) ;
#29207 = CIRCLE ( 'NONE', #72457, 31.99999999999998934 ) ;
#29209 =( LENGTH_UNIT ( ) NAMED_UNIT ( * ) SI_UNIT ( .MILLI., .METRE. ) );
#29210 = CARTESIAN_POINT ( 'NONE',  ( -92.69370383062502583, 88.66845928578038638, 88.16114583420048234 ) ) ;
#29211 = DIRECTION ( 'NONE',  ( -1.000000000000000000, 0.000000000000000000, 0.000000000000000000 ) ) ;
#29212 = CARTESIAN_POINT ( 'NONE',  ( 10.00000000000000000, -59.03342792756297541, 46.54456581323783126 ) ) ;
#29213 = CARTESIAN_POINT ( 'NONE',  ( 92.35000000000002274, -211.5299782133524502, 76.16229166840095388 ) ) ;
#29214 = CARTESIAN_POINT ( 'NONE',  ( 92.34999999999999432, 90.00000000000002842, 79.20499999999999829 ) ) ;
#29215 = EDGE_LOOP ( 'NONE', ( #42575, #45771 ) ) ;
#29216 = DIRECTION ( 'NONE',  ( 0.000000000000000000, 0.000000000000000000, 1.000000000000000000 ) ) ;
#29217 = ORIENTED_EDGE ( 'NONE', *, *, #33699, .F. ) ;
#29218 = CYLINDRICAL_SURFACE ( 'NONE', #5702, 31.99999999999999289 ) ;
#29219 = VERTEX_POINT ( 'NONE', #18718 ) ;
#29220 = CARTESIAN_POINT ( 'NONE',  ( -100.0000000000000142, 85.00000000000002842, 90.00000000000000000 ) ) ;
#29221 = CARTESIAN_POINT ( 'NONE',  ( -92.69370383062504004, 90.00000000000004263, 81.22906250086715829 ) ) ;
#29222 = CARTESIAN_POINT ( 'NONE',  ( 93.84685191531248449, 91.99731107132950569, 89.06072916753382174 ) ) ;
#29223 = ORIENTED_EDGE ( 'NONE', *, *, #16716, .T. ) ;
#29224 = CARTESIAN_POINT ( 'NONE',  ( -11.59999999999999787, 0.000000000000000000, 53.20000000000001705 ) ) ;
#29225 = CYLINDRICAL_SURFACE ( 'NONE', #60479, 77.49899999999999523 ) ;
#29226 = DIRECTION ( 'NONE',  ( 0.000000000000000000, 0.000000000000000000, 1.000000000000000000 ) ) ;
#29227 = PLANE ( 'NONE',  #3525 ) ;
#29228 = ORIENTED_EDGE ( 'NONE', *, *, #8987, .F. ) ;
#29229 = CARTESIAN_POINT ( 'NONE',  ( 0.000000000000000000, 0.000000000000000000, 0.000000000000000000 ) ) ;
#29230 = CARTESIAN_POINT ( 'NONE',  ( -94.99999999999997158, -212.6630814284392557, 77.10156250086711793 ) ) ;
#29231 = ORIENTED_EDGE ( 'NONE', *, *, #5810, .F. ) ;
#29232 = ORIENTED_EDGE ( 'NONE', *, *, #48525, .T. ) ;
#29233 = ORIENTED_EDGE ( 'NONE', *, *, #46857, .F. ) ;
#29234 = CARTESIAN_POINT ( 'NONE',  ( 10.00000000000000000, -37.22597642581161637, 5.202137450156258502 ) ) ;
#29235 = AXIS2_PLACEMENT_3D ( 'NONE', #50152, #26499, #32866 ) ;
#29236 = DIRECTION ( 'NONE',  ( 0.000000000000000000, 0.000000000000000000, 1.000000000000000000 ) ) ;
#29237 = EDGE_LOOP ( 'NONE', ( #15850, #73294, #51671, #64294 ) ) ;
#29238 =( BOUNDED_CURVE ( )  B_SPLINE_CURVE ( 2, ( #23214, #34853, #12649, #63810, #45788, #11909, #34475, #17928, #41233 ),
 .UNSPECIFIED., .F., .F. ) 
 B_SPLINE_CURVE_WITH_KNOTS ( ( 3, 2, 2, 2, 3 ),
 ( 0.8043570860693807223, 0.8043572716645402965, 0.8114130372054574325, 0.8184688027463743465, 0.8255245790604923695 ),
 .UNSPECIFIED. ) 
 CURVE ( )  GEOMETRIC_REPRESENTATION_ITEM ( )  RATIONAL_B_SPLINE_CURVE ( ( 0.9999929520383388226, 0.9999964759264720060, 1.000000000000000000, 0.8660254037844387076, 1.000000000000000000, 0.8660254037844387076, 1.000000000000000000, 0.8660254037844387076, 1.000000000000000000 ) ) 
 REPRESENTATION_ITEM ( '' )  );
#29239 = CARTESIAN_POINT ( 'NONE',  ( -92.69370383062498320, -211.3315407142195852, 88.16114583420048234 ) ) ;
#29240 = VERTEX_POINT ( 'NONE', #36754 ) ;
#29241 = FACE_OUTER_BOUND ( 'NONE', #45657, .T. ) ;
#29242 = CARTESIAN_POINT ( 'NONE',  ( -43.60332556124591719, -107.0000000000000000, 102.9091629284897493 ) ) ;
#29243 = ORIENTED_EDGE ( 'NONE', *, *, #6046, .T. ) ;
#29244 = CIRCLE ( 'NONE', #50880, 3.299999999999983391 ) ;
#29245 = DIRECTION ( 'NONE',  ( 0.000000000000000000, 0.000000000000000000, -1.000000000000000000 ) ) ;
#29246 = ORIENTED_EDGE ( 'NONE', *, *, #24751, .F. ) ;
#29247 = DIRECTION ( 'NONE',  ( -1.000000000000000000, -0.000000000000000000, 0.000000000000000000 ) ) ;
#29248 = AXIS2_PLACEMENT_3D ( 'NONE', #21327, #38265, #10433 ) ;
#29249 = CARTESIAN_POINT ( 'NONE',  ( 15.00000000000000000, 24.81905959214275370, 9.408202855044498492 ) ) ;
#29250 = CARTESIAN_POINT ( 'NONE',  ( 96.15314808468748708, 91.99731107132950569, 84.35114583420048007 ) ) ;
#29251 = CARTESIAN_POINT ( 'NONE',  ( 0.000000000000000000, 0.000000000000000000, 0.000000000000000000 ) ) ;
#29252 = DIRECTION ( 'NONE',  ( -0.000000000000000000, -0.000000000000000000, 1.000000000000000000 ) ) ;
#29253 = DIRECTION ( 'NONE',  ( 0.000000000000000000, 0.4999999999999938938, -0.8660254037844421493 ) ) ;
#29254 = CARTESIAN_POINT ( 'NONE',  ( 0.000000000000000000, -120.0000000000000000, -5.500000000000000000 ) ) ;
#29255 = DIRECTION ( 'NONE',  ( 0.000000000000000000, 0.8910065241883688980, -0.4539904997395446951 ) ) ;
#29256 = CARTESIAN_POINT ( 'NONE',  ( -97.64999999953586496, -210.0000309672219601, 77.38038495123339544 ) ) ;
#29257 = DIRECTION ( 'NONE',  ( 0.000000000000000000, 0.9238795325112851842, 0.3826834323650938341 ) ) ;
#29258 = CIRCLE ( 'NONE', #490, 77.49900000000000944 ) ;
#29259 = VECTOR ( 'NONE', #41133, 1000.000000000000000 ) ;
#29260 = DIRECTION ( 'NONE',  ( -1.000000000000000000, 0.000000000000000000, 0.000000000000000000 ) ) ;
#29261 = PRODUCT_DEFINITION ( 'UNKNOWN', '', #31660, #14564 ) ;
#29262 = EDGE_CURVE ( 'NONE', #23771, #16386, #57567, .T. ) ;
#29263 = LINE ( 'NONE', #34540, #7351 ) ;
#29264 = VECTOR ( 'NONE', #42399, 1000.000000000000114 ) ;
#29265 = LINE ( 'NONE', #56758, #68993 ) ;
#29266 = AXIS2_PLACEMENT_3D ( 'NONE', #36848, #48503, #48139 ) ;
#29267 = CARTESIAN_POINT ( 'NONE',  ( 11.99999999999999822, 0.000000000000000000, 0.000000000000000000 ) ) ;
#29268 = EDGE_CURVE ( 'NONE', #6402, #47366, #31109, .T. ) ;
#29269 = EDGE_CURVE ( 'NONE', #4105, #29346, #54058, .T. ) ;
#29270 = CARTESIAN_POINT ( 'NONE',  ( 16.30584220631899228, -140.9432449716519784, 5.500000000000000000 ) ) ;
#29271 = ORIENTED_EDGE ( 'NONE', *, *, #65995, .F. ) ;
#29272 = ADVANCED_FACE ( 'NONE', ( #46940 ), #29998, .T. ) ;
#29273 = DIRECTION ( 'NONE',  ( 0.000000000000000000, 0.000000000000000000, 1.000000000000000000 ) ) ;
#29274 = LINE ( 'NONE', #35654, #4717 ) ;
#29275 = CARTESIAN_POINT ( 'NONE',  ( 10.00000000000000000, 0.000000000000000000, 0.000000000000000000 ) ) ;
#29276 = AXIS2_PLACEMENT_3D ( 'NONE', #39791, #33765, #45060 ) ;
#29277 = CARTESIAN_POINT ( 'NONE',  ( -92.35000000000005116, 88.47002178664754979, 77.64395833506762301 ) ) ;
#29278 = CYLINDRICAL_SURFACE ( 'NONE', #73963, 15.80000000000028315 ) ;
#29279 = CARTESIAN_POINT ( 'NONE',  ( 92.69370383062501162, -211.3315407142195852, 84.13947916753383538 ) ) ;
#29280 = ORIENTED_EDGE ( 'NONE', *, *, #27157, .F. ) ;
#29281 = ORIENTED_EDGE ( 'NONE', *, *, #33201, .T. ) ;
#29282 = EDGE_CURVE ( 'NONE', #40323, #38913, #1487, .T. ) ;
#29283 = EDGE_CURVE ( 'NONE', #3543, #69389, #69854, .T. ) ;
#29284 = VERTEX_POINT ( 'NONE', #64235 ) ;
#29285 = AXIS2_PLACEMENT_3D ( 'NONE', #67167, #31826, #54776 ) ;
#29286 = FACE_OUTER_BOUND ( 'NONE', #65487, .T. ) ;
#29287 = CARTESIAN_POINT ( 'NONE',  ( -97.64999999999996305, -209.9999999999999716, 90.00000000000000000 ) ) ;
#29288 = ORIENTED_EDGE ( 'NONE', *, *, #69046, .T. ) ;
#29289 = CARTESIAN_POINT ( 'NONE',  ( 96.15314808468748708, -208.0026889286704943, 78.79489583420048859 ) ) ;
#29290 = ORIENTED_EDGE ( 'NONE', *, *, #4280, .T. ) ;
#29291 = CARTESIAN_POINT ( 'NONE',  ( 23.11608002360578240, -124.4885236261218182, 5.500000000000000000 ) ) ;
#29292 = ORIENTED_EDGE ( 'NONE', *, *, #4784, .T. ) ;
#29293 = VERTEX_POINT ( 'NONE', #2597 ) ;
#29294 = CARTESIAN_POINT ( 'NONE',  ( 97.64999999999999147, -210.0000001051138270, 86.58687499784845443 ) ) ;
#29295 = LINE ( 'NONE', #56414, #24436 ) ;
#29296 = ORIENTED_EDGE ( 'NONE', *, *, #62755, .F. ) ;
#29297 = CARTESIAN_POINT ( 'NONE',  ( 0.000000000000000000, 0.000000000000000000, 0.000000000000000000 ) ) ;
#29298 = CARTESIAN_POINT ( 'NONE',  ( 92.35000000000002274, -208.4700217866474645, 85.58145833506763722 ) ) ;
#29299 = ORIENTED_EDGE ( 'NONE', *, *, #64767, .F. ) ;
#29300 = CYLINDRICAL_SURFACE ( 'NONE', #17795, 77.49899999999999523 ) ;
#29301 = AXIS2_PLACEMENT_3D ( 'NONE', #69084, #10828, #17570 ) ;
#29302 = ORIENTED_EDGE ( 'NONE', *, *, #6945, .F. ) ;
#29303 = CARTESIAN_POINT ( 'NONE',  ( 10.00000000000000000, 21.60688246758585862, 79.10210256391376049 ) ) ;
#29304 = CIRCLE ( 'NONE', #42583, 15.99999999999999822 ) ;
#29305 = ORIENTED_EDGE ( 'NONE', *, *, #16290, .T. ) ;
#29306 = CARTESIAN_POINT ( 'NONE',  ( 92.34999999999999432, 90.00000000000002842, 84.99937500173429328 ) ) ;
#29307 = ORIENTED_EDGE ( 'NONE', *, *, #36414, .F. ) ;
#29309 = AXIS2_PLACEMENT_3D ( 'NONE', #51274, #16703, #16329 ) ;
#29308 = SURFACE_SIDE_STYLE ('',( #6408 ) ) ;
#29310 = ORIENTED_EDGE ( 'NONE', *, *, #3733, .T. ) ;
#29311 = DIRECTION ( 'NONE',  ( 0.000000000000000000, 0.000000000000000000, 1.000000000000000000 ) ) ;
#29312 = AXIS2_PLACEMENT_3D ( 'NONE', #23106, #40021, #34366 ) ;
#29313 = CONTEXT_DEPENDENT_SHAPE_REPRESENTATION ( #68622, #51219 ) ;
#29314 = CARTESIAN_POINT ( 'NONE',  ( 0.000000000000000000, -23.16143007188376757, -73.95703589263997912 ) ) ;
#29315 = ORIENTED_EDGE ( 'NONE', *, *, #13212, .F. ) ;
#29316 = VERTEX_POINT ( 'NONE', #71319 ) ;
#29317 = ORIENTED_EDGE ( 'NONE', *, *, #11640, .F. ) ;
#29318 = CARTESIAN_POINT ( 'NONE',  ( 0.000000000000000000, 22.07842321921481243, 8.187992925817422218 ) ) ;
#29319 = LINE ( 'NONE', #47370, #1380 ) ;
#29320 = CARTESIAN_POINT ( 'NONE',  ( -93.67500000000003979, 92.29496732002878900, 87.24833333333333485 ) ) ;
#29321 = ORIENTED_EDGE ( 'NONE', *, *, #32420, .T. ) ;
#29322 = CARTESIAN_POINT ( 'NONE',  ( 95.00000000000000000, -206.9400435732949575, 89.84125000000000227 ) ) ;
#29323 = AXIS2_PLACEMENT_3D ( 'NONE', #11622, #51860, #56406 ) ;
#29324 = ORIENTED_EDGE ( 'NONE', *, *, #66737, .T. ) ;
#29325 = CARTESIAN_POINT ( 'NONE',  ( 26.49955575014872622, 0.001194404164634644498, -48.99999999999931788 ) ) ;
#29326 = CARTESIAN_POINT ( 'NONE',  ( -97.30629616937497417, -208.6684592857803011, 87.04989583420048405 ) ) ;
#29327 = ORIENTED_EDGE ( 'NONE', *, *, #35996, .F. ) ;
#29328 = CARTESIAN_POINT ( 'NONE',  ( -97.64999999999996305, -209.9999999999999716, 79.28437500173430408 ) ) ;
#29329 = CARTESIAN_POINT ( 'NONE',  ( 93.46017751755566394, -212.0954260604421222, 74.96680960279266515 ) ) ;
#29330 = CARTESIAN_POINT ( 'NONE',  ( 94.99999999999998579, 86.94004357329502852, 81.26874999999999716 ) ) ;
#29331 = CARTESIAN_POINT ( 'NONE',  ( -97.30629616937495996, -209.9999999999999716, 75.67281250086713840 ) ) ;
#29332 = EDGE_CURVE ( 'NONE', #64355, #64095, #19824, .T. ) ;
#29333 = CIRCLE ( 'NONE', #14905, 77.49899999999998101 ) ;
#29334 = CARTESIAN_POINT ( 'NONE',  ( -0.0004442498508594591917, 0.001194404164628348752, -65.00000000000000000 ) ) ;
#29335 = DIRECTION ( 'NONE',  ( 0.000000000000000000, 0.000000000000000000, 1.000000000000000000 ) ) ;
#29336 = CARTESIAN_POINT ( 'NONE',  ( 0.000000000000000000, 0.000000000000000000, 0.000000000000000000 ) ) ;
#29337 = CYLINDRICAL_SURFACE ( 'NONE', #52781, 16.00000000000000000 ) ;
#29338 = EDGE_CURVE ( 'NONE', #63936, #10604, #25083, .T. ) ;
#29339 = DIRECTION ( 'NONE',  ( 0.000000000000000000, 0.000000000000000000, 1.000000000000000000 ) ) ;
#29340 = ADVANCED_FACE ( 'NONE', ( #58963 ), #60085, .T. ) ;
#29341 = DIRECTION ( 'NONE',  ( 0.000000000000000000, 0.000000000000000000, 1.000000000000000000 ) ) ;
#29342 = CARTESIAN_POINT ( 'NONE',  ( -95.00000000000002842, 92.66308142843932671, 78.68906250086713783 ) ) ;
#29343 = DIRECTION ( 'NONE',  ( -1.000000000000000000, 3.061616997868382648E-16, 0.000000000000000000 ) ) ;
#29344 = DIRECTION ( 'NONE',  ( 0.000000000000000000, -1.000000000000000000, 1.625241993126352200E-15 ) ) ;
#29345 = VECTOR ( 'NONE', #52093, 1000.000000000000000 ) ;
#29346 = VERTEX_POINT ( 'NONE', #30368 ) ;
#29347 = DIRECTION ( 'NONE',  ( 0.000000000000000000, 0.000000000000000000, 1.000000000000000000 ) ) ;
#29348 = EDGE_CURVE ( 'NONE', #10428, #42999, #52565, .T. ) ;
#29349 = DIRECTION ( 'NONE',  ( -1.000000000000000000, -0.000000000000000000, 0.000000000000000000 ) ) ;
#29350 = CARTESIAN_POINT ( 'NONE',  ( 0.000000000000000000, 0.000000000000000000, 12.50000000000000000 ) ) ;
#29351 = VECTOR ( 'NONE', #43935, 1000.000000000000000 ) ;
#29352 = CARTESIAN_POINT ( 'NONE',  ( -10.43921258969510824, -98.89258801967538659, 2.500000000000000000 ) ) ;
#29353 = CARTESIAN_POINT ( 'NONE',  ( -0.0004442498508594591917, 0.001194404164628348752, -65.00000000000000000 ) ) ;
#29354 = DIRECTION ( 'NONE',  ( 0.000000000000000000, 0.000000000000000000, -1.000000000000000000 ) ) ;
#29355 = CARTESIAN_POINT ( 'NONE',  ( -93.84685191531247028, -211.9973110713294489, 76.04322916753382344 ) ) ;
#29356 = DIRECTION ( 'NONE',  ( 0.000000000000000000, 0.9723699203976773342, -0.2334453638559024491 ) ) ;
#29357 = ORIENTED_EDGE ( 'NONE', *, *, #9776, .F. ) ;
#29358 = AXIS2_PLACEMENT_3D ( 'NONE', #9652, #39345, #73164 ) ;
#29359 = EDGE_CURVE ( 'NONE', #72240, #54635, #7098, .T. ) ;
#29360 = DIRECTION ( 'NONE',  ( -1.000000000000000000, 0.000000000000000000, 0.000000000000000000 ) ) ;
#29361 = CIRCLE ( 'NONE', #68985, 37.49900000000001654 ) ;
#29362 = DIRECTION ( 'NONE',  ( -1.000000000000000000, -0.000000000000000000, -0.000000000000000000 ) ) ;
#29363 = DIRECTION ( 'NONE',  ( -1.000000000000000000, -0.000000000000000000, 0.000000000000000000 ) ) ;
#29364 = CARTESIAN_POINT ( 'NONE',  ( 0.000000000000000000, -68.26794271651239399, -31.47745569255214093 ) ) ;
#29365 = CIRCLE ( 'NONE', #66630, 31.99999999999999645 ) ;
#29366 = VECTOR ( 'NONE', #44065, 1000.000000000000000 ) ;
#29367 = CARTESIAN_POINT ( 'NONE',  ( -997.5739745962155212, 0.000000000000000000, 0.000000000000000000 ) ) ;
#29368 = ORIENTED_EDGE ( 'NONE', *, *, #71981, .F. ) ;
#29369 = EDGE_CURVE ( 'NONE', #71558, #1809, #30964, .T. ) ;
#29370 = CARTESIAN_POINT ( 'NONE',  ( 5.000000000000000000, 39.04073710021366139, -15.48615015657542138 ) ) ;
#29371 = EDGE_CURVE ( 'NONE', #4351, #26140, #64580, .T. ) ;
#29372 = ORIENTED_EDGE ( 'NONE', *, *, #44740, .F. ) ;
#29373 = CARTESIAN_POINT ( 'NONE',  ( 97.30629616937498838, -211.3315407142195852, 84.19239583420048234 ) ) ;
#29374 = CARTESIAN_POINT ( 'NONE',  ( 0.000000000000000000, -51.02545421589285723, -55.20638768913812555 ) ) ;
#29375 = EDGE_CURVE ( 'NONE', #38563, #8717, #36377, .T. ) ;
#29376 = EDGE_LOOP ( 'NONE', ( #5120, #49942, #57890, #9138 ) ) ;
#29377 = CIRCLE ( 'NONE', #30563, 77.49899999999999523 ) ;
#29378 = DIRECTION ( 'NONE',  ( 0.000000000000000000, 0.000000000000000000, 1.000000000000000000 ) ) ;
#29379 = ORIENTED_EDGE ( 'NONE', *, *, #45932, .T. ) ;
#29380 = DIRECTION ( 'NONE',  ( 0.000000000000000000, 0.000000000000000000, 1.000000000000000000 ) ) ;
#29381 = VERTEX_POINT ( 'NONE', #30733 ) ;
#29382 = CARTESIAN_POINT ( 'NONE',  ( -92.69370383062504004, 90.00000000000004263, 79.32406250086715715 ) ) ;
#29383 = ORIENTED_EDGE ( 'NONE', *, *, #13878, .T. ) ;
#29384 = EDGE_LOOP ( 'NONE', ( #16358, #38125, #31142, #6491 ) ) ;
#29385 = VERTEX_POINT ( 'NONE', #53678 ) ;
#29386 = DIRECTION ( 'NONE',  ( -1.000000000000000000, 0.000000000000000000, 0.000000000000000000 ) ) ;
#29387 = ORIENTED_EDGE ( 'NONE', *, *, #73652, .F. ) ;
#29388 = DIRECTION ( 'NONE',  ( 1.000000000000000000, 0.000000000000000000, 0.000000000000000000 ) ) ;
#29389 = EDGE_LOOP ( 'NONE', ( #53344, #50012, #29654, #51942 ) ) ;
#29390 = CARTESIAN_POINT ( 'NONE',  ( 95.04693102382854875, 87.35041560265749183, 75.00000002508419072 ) ) ;
#29391 = ORIENTED_EDGE ( 'NONE', *, *, #25330, .T. ) ;
#29392 = ORIENTED_EDGE ( 'NONE', *, *, #35043, .F. ) ;
#29393 = EDGE_LOOP ( 'NONE', ( #48176, #71817, #21610, #25773 ) ) ;
#29394 = CARTESIAN_POINT ( 'NONE',  ( 97.30629616937498838, -209.9999999999999716, 81.70531250086713726 ) ) ;
#29395 = ITEM_DEFINED_TRANSFORMATION ( 'NONE', 'NONE', #26769,  #43395 ) ;
#29396 = DIRECTION ( 'NONE',  ( -1.000000000000000000, 0.000000000000000000, -0.000000000000000000 ) ) ;
#29397 = LINE ( 'NONE', #68908, #58115 ) ;
#29398 = DIRECTION ( 'NONE',  ( -1.000000000000000000, 0.000000000000000000, -0.000000000000000000 ) ) ;
#29399 = CARTESIAN_POINT ( 'NONE',  ( 10.00000000000000000, 46.54456581323888997, -59.03342792756214408 ) ) ;
#29400 = CARTESIAN_POINT ( 'NONE',  ( 0.4966694826857007139, -118.5846133302278247, 2.500000000000000000 ) ) ;
#29401 = FACE_OUTER_BOUND ( 'NONE', #26189, .T. ) ;
#29402 = CARTESIAN_POINT ( 'NONE',  ( -93.84685191531247028, -211.9973110713294489, 86.04447916753380809 ) ) ;
#29403 = CARTESIAN_POINT ( 'NONE',  ( -97.30629616937501680, 91.33154071421968467, 83.39864583420050792 ) ) ;
#29404 = VERTEX_POINT ( 'NONE', #2219 ) ;
#29405 = CARTESIAN_POINT ( 'NONE',  ( 92.69370383062498320, 91.33154071421968467, 85.77989583420048803 ) ) ;
#29406 = ORIENTED_EDGE ( 'NONE', *, *, #1854, .T. ) ;
#29407 = CARTESIAN_POINT ( 'NONE',  ( -92.35000000000003695, 90.00002660292287260, 78.96687592183759818 ) ) ;
#29408 = CIRCLE ( 'NONE', #73799, 42.00000000000000000 ) ;
#29409 = CARTESIAN_POINT ( 'NONE',  ( -97.30629616937501680, 90.00000000000004263, 89.64281250086713726 ) ) ;
#29410 = DIRECTION ( 'NONE',  ( -0.9227826878668540234, -0.3853207896976546531, 0.000000000000000000 ) ) ;
#29411 = CARTESIAN_POINT ( 'NONE',  ( 92.35000000000000853, -209.9999999999999716, 85.55499999999999261 ) ) ;
#29412 = CARTESIAN_POINT ( 'NONE',  ( -92.69370383062498320, -209.9999999999999716, 86.15031250086714465 ) ) ;
#29413 = DIRECTION ( 'NONE',  ( 1.000000000000000000, 0.000000000000000000, -0.000000000000000000 ) ) ;
#29414 = ADVANCED_FACE ( 'NONE', ( #48043 ), #70956, .T. ) ;
#29415 = DIRECTION ( 'NONE',  ( -1.000000000000000000, -0.000000000000000000, 0.000000000000000000 ) ) ;
#29416 = CARTESIAN_POINT ( 'NONE',  ( 0.000000000000000000, 37.48860685352291000, -0.8828120875901940279 ) ) ;
#29417 = CIRCLE ( 'NONE', #71430, 16.00000000000000000 ) ;
#29418 = CARTESIAN_POINT ( 'NONE',  ( -97.65000000000001990, 90.00000000000004263, 77.29999999999999716 ) ) ;
#29419 = ORIENTED_EDGE ( 'NONE', *, *, #74167, .F. ) ;
#29420 = ORIENTED_EDGE ( 'NONE', *, *, #2815, .T. ) ;
#29421 = ADVANCED_FACE ( 'NONE', ( #20584 ), #16047, .F. ) ;
#29422 = CIRCLE ( 'NONE', #48652, 30.50000000000000000 ) ;
#29423 = CARTESIAN_POINT ( 'NONE',  ( -95.00000000000002842, 86.94004357329504273, 78.09374999999998579 ) ) ;
#29424 = EDGE_CURVE ( 'NONE', #21420, #54327, #63412, .T. ) ;
#29425 = CARTESIAN_POINT ( 'NONE',  ( -10.00000000000000000, 0.000000000000000000, 0.000000000000000000 ) ) ;
#29426 = CARTESIAN_POINT ( 'NONE',  ( -97.30629616937501680, 88.66845928578038638, 87.15572916753380639 ) ) ;
#29427 = DIRECTION ( 'NONE',  ( 1.000000000000000000, 0.000000000000000000, 0.000000000000000000 ) ) ;
#29428 = CYLINDRICAL_SURFACE ( 'NONE', #61419, 16.00000000000000355 ) ;
#29429 = CARTESIAN_POINT ( 'NONE',  ( 95.00000000000000000, -206.9400435732949575, 77.85562500173431033 ) ) ;
#29430 = DIRECTION ( 'NONE',  ( -0.000000000000000000, -0.000000000000000000, -1.000000000000000000 ) ) ;
#29431 = VERTEX_POINT ( 'NONE', #55160 ) ;
#29432 = CARTESIAN_POINT ( 'NONE',  ( -96.15314808468752972, 91.99731107132950569, 79.37697916753380412 ) ) ;
#29433 = VECTOR ( 'NONE', #72042, 1000.000000000000000 ) ;
#29434 = ADVANCED_FACE ( 'NONE', ( #66092 ), #14562, .T. ) ;
#29435 = FACE_OUTER_BOUND ( 'NONE', #14416, .T. ) ;
#29436 = LINE ( 'NONE', #46756, #2177 ) ;
#29437 = DIRECTION ( 'NONE',  ( -0.000000000000000000, -0.000000000000000000, -1.000000000000000000 ) ) ;
#29438 = DIRECTION ( 'NONE',  ( 1.000000000000000000, 0.000000000000000000, 0.000000000000000000 ) ) ;
#29439 = VECTOR ( 'NONE', #41940, 1000.000000000000114 ) ;
#29440 = LINE ( 'NONE', #52382, #40015 ) ;
#29441 = CARTESIAN_POINT ( 'NONE',  ( -93.84685191531247028, -211.9973110713294489, 84.93322916753382401 ) ) ;
#29442 = CARTESIAN_POINT ( 'NONE',  ( 93.67500000000001137, -207.7050326799711968, 79.17854166840096752 ) ) ;
#29443 =( BOUNDED_CURVE ( )  B_SPLINE_CURVE ( 2, ( #49592, #25926, #3766, #72881, #61266, #55244, #21383 ),
 .UNSPECIFIED., .F., .F. ) 
 B_SPLINE_CURVE_WITH_KNOTS ( ( 3, 2, 2, 3 ),
 ( 0.1874999999999999167, 0.1944444444444443365, 0.2013888888888887285, 0.2083333333333331483 ),
 .UNSPECIFIED. ) 
 CURVE ( )  GEOMETRIC_REPRESENTATION_ITEM ( )  RATIONAL_B_SPLINE_CURVE ( ( 1.000000000000001554, 0.8660254037844371533, 1.000000000000000000, 0.8660254037844387076, 1.000000000000000000, 0.8660254037844424824, 0.9999999999999962252 ) ) 
 REPRESENTATION_ITEM ( '' )  );
#29444 = EDGE_CURVE ( 'NONE', #41704, #18817, #46164, .T. ) ;
#29445 = CARTESIAN_POINT ( 'NONE',  ( 97.30629616937498838, 91.33154071421968467, 77.47197916753381719 ) ) ;
#29446 = CARTESIAN_POINT ( 'NONE',  ( -96.15314808468745866, -211.9973110713294489, 75.93739583420048689 ) ) ;
#29447 = DIRECTION ( 'NONE',  ( 0.000000000000000000, 0.000000000000000000, 1.000000000000000000 ) ) ;
#29448 = VERTEX_POINT ( 'NONE', #66815 ) ;
#29449 = DIRECTION ( 'NONE',  ( -1.000000000000000000, -0.000000000000000000, -0.000000000000000000 ) ) ;
#29450 = DIRECTION ( 'NONE',  ( 0.000000000000000000, 0.000000000000000000, 1.000000000000000000 ) ) ;
#29451 = DIRECTION ( 'NONE',  ( -0.000000000000000000, -0.000000000000000000, 1.000000000000000000 ) ) ;
#29452 = AXIS2_PLACEMENT_3D ( 'NONE', #45778, #34465, #50269 ) ;
#29453 = DIRECTION ( 'NONE',  ( 1.000000000000000000, 0.000000000000000000, 0.000000000000000000 ) ) ;
#29454 = CARTESIAN_POINT ( 'NONE',  ( 92.69370383062501162, -211.3315407142195852, 75.72572916753381378 ) ) ;
#29455 = ORIENTED_EDGE ( 'NONE', *, *, #34272, .F. ) ;
#29456 = ADVANCED_FACE ( 'NONE', ( #32589 ), #55537, .T. ) ;
#29457 = EDGE_CURVE ( 'NONE', #66558, #40071, #53781, .T. ) ;
#29458 = CARTESIAN_POINT ( 'NONE',  ( 10.00000000000000000, 0.000000000000000000, 0.000000000000000000 ) ) ;
#29459 = ORIENTED_EDGE ( 'NONE', *, *, #34623, .F. ) ;
#29460 = CIRCLE ( 'NONE', #23473, 1.500000000000000000 ) ;
#29461 = DIRECTION ( 'NONE',  ( -1.000000000000000000, 0.000000000000000000, 0.000000000000000000 ) ) ;
#29462 = CIRCLE ( 'NONE', #23475, 31.99999999999999289 ) ;
#29463 = VERTEX_POINT ( 'NONE', #26947 ) ;
#29464 = CARTESIAN_POINT ( 'NONE',  ( 0.000000000000000000, 33.80338159004283938, 16.23288003029508886 ) ) ;
#29465 = AXIS2_PLACEMENT_3D ( 'NONE', #37382, #20448, #31346 ) ;
#29466 = EDGE_LOOP ( 'NONE', ( #60592, #13620 ) ) ;
#29467 = ORIENTED_EDGE ( 'NONE', *, *, #28366, .F. ) ;
#29468 = VECTOR ( 'NONE', #49045, 1000.000000000000000 ) ;
#29469 = ORIENTED_EDGE ( 'NONE', *, *, #3733, .F. ) ;
#29470 = CARTESIAN_POINT ( 'NONE',  ( 10.00000000000000000, 37.22597642581150268, 5.202137450157037435 ) ) ;
#29471 = ORIENTED_EDGE ( 'NONE', *, *, #4703, .F. ) ;
#29472 = AXIS2_PLACEMENT_3D ( 'NONE', #56164, #39254, #15571 ) ;
#29473 = AXIS2_PLACEMENT_3D ( 'NONE', #67347, #15848, #39905 ) ;
#29474 = VERTEX_POINT ( 'NONE', #27314 ) ;
#29475 = CARTESIAN_POINT ( 'NONE',  ( 97.30629616937498838, 91.33154071421968467, 83.18697916753382060 ) ) ;
#29476 = CARTESIAN_POINT ( 'NONE',  ( 15.00000000000000000, -3.948201729842032215, 23.21447184625297666 ) ) ;
#29477 = CARTESIAN_POINT ( 'NONE',  ( 97.64999999999999147, -209.9999999999999716, 75.07749999999998636 ) ) ;
#29478 = AXIS2_PLACEMENT_3D ( 'NONE', #65228, #36637, #69742 ) ;
#29479 = EDGE_LOOP ( 'NONE', ( #11342, #61871, #41604, #13064 ) ) ;
#29480 = VERTEX_POINT ( 'NONE', #8563 ) ;
#29481 = B_SPLINE_CURVE_WITH_KNOTS ( 'NONE', 3,
 ( #9984, #28014, #63010, #61878 ),
 .UNSPECIFIED., .F., .F.,
 ( 4, 4 ),
 ( 2.446487931514586224E-06, 1.000000000000000000 ),
 .UNSPECIFIED. ) ;
#29482 = ORIENTED_EDGE ( 'NONE', *, *, #653, .T. ) ;
#29483 = ORIENTED_EDGE ( 'NONE', *, *, #62697, .T. ) ;
#29484 = DIRECTION ( 'NONE',  ( -1.000000000000000000, 0.000000000000000000, 0.000000000000000000 ) ) ;
#29485 = ORIENTED_EDGE ( 'NONE', *, *, #72893, .F. ) ;
#29486 = CARTESIAN_POINT ( 'NONE',  ( 0.000000000000000000, 0.000000000000000000, 0.000000000000000000 ) ) ;
#29487 = CARTESIAN_POINT ( 'NONE',  ( 94.99999999999998579, 93.05995642670504253, 84.12624999999999886 ) ) ;
#29488 = CARTESIAN_POINT ( 'NONE',  ( -10.00000000000000000, 0.000000000000000000, 0.000000000000000000 ) ) ;
#29489 = DIRECTION ( 'NONE',  ( -1.000000000000000000, 0.000000000000000000, 0.000000000000000000 ) ) ;
#29490 = CARTESIAN_POINT ( 'NONE',  ( 0.000000000000000000, 0.000000000000000000, 0.000000000000000000 ) ) ;
#29491 = CARTESIAN_POINT ( 'NONE',  ( 0.000000000000000000, 33.79645857604513992, -16.45098606841138178 ) ) ;
#29492 = LINE ( 'NONE', #35151, #69255 ) ;
#29493 = EDGE_LOOP ( 'NONE', ( #240, #70336, #60624, #20179 ) ) ;
#29494 = CARTESIAN_POINT ( 'NONE',  ( -94.99999999999997158, -213.0599564267049857, 78.17312500173430578 ) ) ;
#29495 = ORIENTED_EDGE ( 'NONE', *, *, #41669, .T. ) ;
#29496 = DIRECTION ( 'NONE',  ( -1.000000000000000000, 0.000000000000000000, 0.000000000000000000 ) ) ;
#29497 = EDGE_LOOP ( 'NONE', ( #71383, #73871, #38978, #11462 ) ) ;
#29498 = EDGE_CURVE ( 'NONE', #2397, #70414, #26193, .T. ) ;
#29500 = CARTESIAN_POINT ( 'NONE',  ( -93.67500000000003979, 87.70503267997129626, 78.86104166840097207 ) ) ;
#29499 = CARTESIAN_POINT ( 'NONE',  ( 92.34999999999999432, 88.47002178664753558, 78.06729166840096923 ) ) ;
#29501 = VERTEX_POINT ( 'NONE', #73185 ) ;
#29502 = CARTESIAN_POINT ( 'NONE',  ( 93.84685191531248449, 88.00268892867053694, 78.47739583420049314 ) ) ;
#29503 = DIRECTION ( 'NONE',  ( 0.000000000000000000, -0.000000000000000000, -1.000000000000000000 ) ) ;
#29504 = CARTESIAN_POINT ( 'NONE',  ( 11.99999999999999822, -59.03961581697367933, -46.53671651294010303 ) ) ;
#29505 = EDGE_CURVE ( 'NONE', #37728, #49062, #72074, .T. ) ;
#29506 = CARTESIAN_POINT ( 'NONE',  ( 11.99999999999999822, 54.21277698773675979, 55.38113227695801299 ) ) ;
#29507 = FACE_OUTER_BOUND ( 'NONE', #71169, .T. ) ;
#29508 = EDGE_LOOP ( 'NONE', ( #41075, #12473, #12684, #47888 ) ) ;
#29509 = DIRECTION ( 'NONE',  ( -0.1276937514489705217, -0.9918136447140101231, 0.000000000000000000 ) ) ;
#29510 = CARTESIAN_POINT ( 'NONE',  ( -94.99999999999997158, -209.9999999999999716, 90.00000000000000000 ) ) ;
#29511 = ORIENTED_EDGE ( 'NONE', *, *, #68281, .T. ) ;
#29512 = ADVANCED_FACE ( 'NONE', ( #31847 ), #20196, .T. ) ;
#29513 = ORIENTED_EDGE ( 'NONE', *, *, #53161, .T. ) ;
#29514 = EDGE_CURVE ( 'NONE', #24241, #23404, #40589, .T. ) ;
#29515 = FACE_OUTER_BOUND ( 'NONE', #15812, .T. ) ;
#29516 = LINE ( 'NONE', #58855, #15031 ) ;
#29517 = CARTESIAN_POINT ( 'NONE',  ( 10.00000000000000000, 35.38097989696528600, -12.42422080174602605 ) ) ;
#29518 = CARTESIAN_POINT ( 'NONE',  ( -97.30629616937497417, -211.3315407142195852, 77.78947916753381264 ) ) ;
#29519 = CIRCLE ( 'NONE', #35540, 31.99999999999999289 ) ;
#29520 = ORIENTED_EDGE ( 'NONE', *, *, #26303, .T. ) ;
#29521 = EDGE_CURVE ( 'NONE', #32536, #71453, #16597, .T. ) ;
#29522 = DIRECTION ( 'NONE',  ( 1.000000000000000000, -0.000000000000000000, -0.000000000000000000 ) ) ;
#29523 = CIRCLE ( 'NONE', #42585, 82.00000000000000000 ) ;
#29524 = DIRECTION ( 'NONE',  ( -0.000000000000000000, -0.000000000000000000, 1.000000000000000000 ) ) ;
#29525 = CIRCLE ( 'NONE', #53527, 31.99999999999998934 ) ;
#29526 = CARTESIAN_POINT ( 'NONE',  ( 25.81725066941077529, -113.8380548628854854, -5.500000000000000000 ) ) ;
#29527 = DIRECTION ( 'NONE',  ( 0.000000000000000000, 0.5877852522924741363, -0.8090169943749465631 ) ) ;
#29528 = LINE ( 'NONE', #1393, #57671 ) ;
#29529 = VECTOR ( 'NONE', #9382, 999.9999999999998863 ) ;
#29530 = DIRECTION ( 'NONE',  ( 1.000000000000000000, 0.000000000000000000, 0.000000000000000000 ) ) ;
#29531 = DIRECTION ( 'NONE',  ( -0.000000000000000000, -0.000000000000000000, -1.000000000000000000 ) ) ;
#29532 = LINE ( 'NONE', #34444, #422 ) ;
#29533 = CARTESIAN_POINT ( 'NONE',  ( 1.560000000000000053, 0.8660254037844389297, 1.500000000000000000 ) ) ;
#29534 = AXIS2_PLACEMENT_3D ( 'NONE', #38877, #57281, #67819 ) ;
#29535 = EDGE_CURVE ( 'NONE', #25802, #31031, #36043, .T. ) ;
#29536 = CIRCLE ( 'NONE', #63221, 17.50000000000000355 ) ;
#29537 = EDGE_CURVE ( 'NONE', #7680, #31960, #49876, .T. ) ;
#29538 = CARTESIAN_POINT ( 'NONE',  ( 94.99999999999998579, 92.66308142843932671, 87.73781250086715033 ) ) ;
#29539 = CARTESIAN_POINT ( 'NONE',  ( -97.30629616937497417, -208.6684592857803295, 87.84364583420048689 ) ) ;
#29540 = LINE ( 'NONE', #65261, #250 ) ;
#29541 = VERTEX_POINT ( 'NONE', #11158 ) ;
#29542 = LINE ( 'NONE', #53234, #10000 ) ;
#29543 = CARTESIAN_POINT ( 'NONE',  ( -92.69370383062504004, 90.00000000000004263, 76.62531250086713897 ) ) ;
#29544 = ADVANCED_FACE ( 'NONE', ( #50625 ), #34079, .T. ) ;
#29545 = CIRCLE ( 'NONE', #45192, 11.59999999999999787 ) ;
#29546 = CARTESIAN_POINT ( 'NONE',  ( 95.00000000000000000, -207.3369185715606307, 87.57906250086713840 ) ) ;
#29547 = EDGE_CURVE ( 'NONE', #22970, #72913, #66984, .T. ) ;
#29548 = ORIENTED_EDGE ( 'NONE', *, *, #3103, .F. ) ;
#29549 = LINE ( 'NONE', #59537, #42067 ) ;
#29550 = VERTEX_POINT ( 'NONE', #11878 ) ;
#29551 = EDGE_CURVE ( 'NONE', #73160, #1543, #28062, .T. ) ;
#29552 = CARTESIAN_POINT ( 'NONE',  ( 92.35000000000000853, -209.9999999999999716, 75.39499999999999602 ) ) ;
#29553 = DIRECTION ( 'NONE',  ( 1.000000000000000000, -3.061616997868382648E-16, -0.000000000000000000 ) ) ;
#29554 = ORIENTED_EDGE ( 'NONE', *, *, #57485, .F. ) ;
#29555 = EDGE_LOOP ( 'NONE', ( #259, #18015, #56120, #1506 ) ) ;
#29556 = CARTESIAN_POINT ( 'NONE',  ( 93.84685191531249870, -208.0026889286704943, 81.44072916753381719 ) ) ;
#29557 = DIRECTION ( 'NONE',  ( -0.000000000000000000, -0.000000000000000000, 1.000000000000000000 ) ) ;
#29558 = DIRECTION ( 'NONE',  ( 0.000000000000000000, 0.000000000000000000, -1.000000000000000000 ) ) ;
#29559 = CARTESIAN_POINT ( 'NONE',  ( 5.000000000000000000, 2.886751345948134428, -2.080000000000000071 ) ) ;
#29560 = CARTESIAN_POINT ( 'NONE',  ( 0.000000000000000000, -63.18004540533059554, 44.88180994100355292 ) ) ;
#29561 = CARTESIAN_POINT ( 'NONE',  ( 6.000000000000000000, 74.18225833017888249, 34.94270380257665209 ) ) ;
#29562 = CARTESIAN_POINT ( 'NONE',  ( 93.67500000000001137, -207.7050326799711968, 83.54416666666666913 ) ) ;
#29563 = ORIENTED_EDGE ( 'NONE', *, *, #24363, .T. ) ;
#29564 = ORIENTED_EDGE ( 'NONE', *, *, #18354, .F. ) ;
#29565 = EDGE_LOOP ( 'NONE', ( #58349, #49545, #22940, #66069 ) ) ;
#29566 = EDGE_LOOP ( 'NONE', ( #58266, #70599, #73491, #44112, #24876, #39220 ) ) ;
#29567 = DIRECTION ( 'NONE',  ( -1.000000000000000000, 0.000000000000000000, 0.000000000000000000 ) ) ;
#29568 = CARTESIAN_POINT ( 'NONE',  ( -95.00000000000002842, 87.33691857156074434, 87.42031250086715488 ) ) ;
#29569 = DIRECTION ( 'NONE',  ( 0.000000000000000000, 0.000000000000000000, 1.000000000000000000 ) ) ;
#29570 = AXIS2_PLACEMENT_3D ( 'NONE', #10362, #11472, #33281 ) ;
#29571 = CARTESIAN_POINT ( 'NONE',  ( 92.35000000000000853, -209.9999999999999716, 90.00000000000000000 ) ) ;
#29572 = CARTESIAN_POINT ( 'NONE',  ( 92.35000000000002274, -211.5299782133524502, 76.79729166840095900 ) ) ;
#29573 = CARTESIAN_POINT ( 'NONE',  ( 94.99999999999998579, 86.94004357329500010, 76.82374999999998977 ) ) ;
#29574 = ORIENTED_EDGE ( 'NONE', *, *, #21395, .T. ) ;
#29575 = CARTESIAN_POINT ( 'NONE',  ( -97.64999999999994884, -211.5299782133524502, 88.86229166840097093 ) ) ;
#29576 = ORIENTED_EDGE ( 'NONE', *, *, #5800, .F. ) ;
#29577 = CIRCLE ( 'NONE', #41569, 42.00000000000000000 ) ;
#29578 = ORIENTED_EDGE ( 'NONE', *, *, #70833, .F. ) ;
#29579 = CARTESIAN_POINT ( 'NONE',  ( -92.35000000000005116, 91.52997821335253548, 89.17979166840096639 ) ) ;
#29580 = CARTESIAN_POINT ( 'NONE',  ( -95.00000000000002842, 92.66308142843932671, 80.75281250086716511 ) ) ;
#29581 = CARTESIAN_POINT ( 'NONE',  ( 94.99999999999998579, 92.66308142843935514, 74.87906250086713555 ) ) ;
#29582 = ORIENTED_EDGE ( 'NONE', *, *, #2147, .T. ) ;
#29583 = DIRECTION ( 'NONE',  ( -1.000000000000000000, -0.000000000000000000, -0.000000000000000000 ) ) ;
#29584 = DIRECTION ( 'NONE',  ( 0.000000000000000000, 0.000000000000000000, 1.000000000000000000 ) ) ;
#29585 = CARTESIAN_POINT ( 'NONE',  ( 0.000000000000000000, 16.23288003029497162, 33.80338159004289622 ) ) ;
#29586 = EDGE_CURVE ( 'NONE', #16540, #25590, #11921, .T. ) ;
#29587 = CARTESIAN_POINT ( 'NONE',  ( -96.32499999999996021, -207.7050326799711968, 86.16354166840096696 ) ) ;
#29588 = ORIENTED_EDGE ( 'NONE', *, *, #56654, .F. ) ;
#29589 = CARTESIAN_POINT ( 'NONE',  ( 5.000000000000002665, -71.87247863392386193, -39.47590169984923136 ) ) ;
#29590 = CARTESIAN_POINT ( 'NONE',  ( 0.000000000000000000, -18.89407956138310496, 75.16055320797023853 ) ) ;
#29591 = ORIENTED_EDGE ( 'NONE', *, *, #6397, .F. ) ;
#29592 = ADVANCED_FACE ( 'NONE', ( #61926 ), #45758, .T. ) ;
#29593 = AXIS2_PLACEMENT_3D ( 'NONE', #40211, #44750, #63162 ) ;
#29594 = ORIENTED_EDGE ( 'NONE', *, *, #22355, .F. ) ;
#29595 = FACE_BOUND ( 'NONE', #51355, .T. ) ;
#29596 = EDGE_CURVE ( 'NONE', #49911, #16321, #34568, .T. ) ;
#29597 = ADVANCED_FACE ( 'NONE', ( #17899 ), #22062, .T. ) ;
#29598 = VERTEX_POINT ( 'NONE', #11513 ) ;
#29599 = DIRECTION ( 'NONE',  ( -1.000000000000000000, 0.000000000000000000, -0.000000000000000000 ) ) ;
#29600 = FACE_OUTER_BOUND ( 'NONE', #53704, .T. ) ;
#29601 = VERTEX_POINT ( 'NONE', #74305 ) ;
#29602 = CARTESIAN_POINT ( 'NONE',  ( -97.30629616937497417, -208.6684592857803011, 89.11364583420049712 ) ) ;
#29603 = ORIENTED_EDGE ( 'NONE', *, *, #58666, .F. ) ;
#29604 = CARTESIAN_POINT ( 'NONE',  ( 10.00000000000000000, 39.47590169984943742, -71.87247863392373404 ) ) ;
#29605 = CARTESIAN_POINT ( 'NONE',  ( 0.000000000000000000, -44.88180994100419952, 63.18004540533013369 ) ) ;
#29606 = ORIENTED_EDGE ( 'NONE', *, *, #993, .F. ) ;
#29607 = ORIENTED_EDGE ( 'NONE', *, *, #56543, .F. ) ;
#29608 = LINE ( 'NONE', #46194, #10391 ) ;
#29609 = AXIS2_PLACEMENT_3D ( 'NONE', #44305, #22114, #66501 ) ;
#29611 = EDGE_CURVE ( 'NONE', #47064, #42482, #69045, .T. ) ;
#29610 = DIRECTION ( 'NONE',  ( 0.000000000000000000, 0.000000000000000000, 1.000000000000000000 ) ) ;
#29612 = CARTESIAN_POINT ( 'NONE',  ( 92.69370383062498320, 91.33154071421968467, 80.69989583420046131 ) ) ;
#29613 = LINE ( 'NONE', #739, #38826 ) ;
#29614 = CARTESIAN_POINT ( 'NONE',  ( 0.000000000000000000, 37.16516213103285082, -4.992566952384588141 ) ) ;
#29615 = LINE ( 'NONE', #48038, #10863 ) ;
#29616 = CARTESIAN_POINT ( 'NONE',  ( 0.000000000000000000, -0.6853352020793173072, 37.58145647212453611 ) ) ;
#29617 = EDGE_CURVE ( 'NONE', #39587, #10916, #9343, .T. ) ;
#29618 = DIRECTION ( 'NONE',  ( 3.035766082959412415E-16, 1.000000000000000000, 0.000000000000000000 ) ) ;
#29619 = DIRECTION ( 'NONE',  ( 0.000000000000000000, 0.000000000000000000, 1.000000000000000000 ) ) ;
#29620 = DIRECTION ( 'NONE',  ( 0.000000000000000000, 0.000000000000000000, -1.000000000000000000 ) ) ;
#29621 = APPLICATION_CONTEXT ( 'automotive_design' ) ;
#29622 = AXIS2_PLACEMENT_3D ( 'NONE', #23257, #11961, #69478 ) ;
#29623 = DIRECTION ( 'NONE',  ( -8.119982227976398872E-16, -1.065814103640131188E-14, -1.000000000000000000 ) ) ;
#29624 = VECTOR ( 'NONE', #15430, 1000.000000000000000 ) ;
#29625 = CARTESIAN_POINT ( 'NONE',  ( 15.00000000000000000, -25.60904388321916159, 6.976881207771517879 ) ) ;
#29626 = CARTESIAN_POINT ( 'NONE',  ( -95.00000000000002842, 92.66308142843932671, 85.67406250086715147 ) ) ;
#29627 = EDGE_CURVE ( 'NONE', #10925, #70197, #28815, .T. ) ;
#29628 = EDGE_CURVE ( 'NONE', #31772, #26087, #17777, .T. ) ;
#29629 = LINE ( 'NONE', #6361, #22668 ) ;
#29630 = VECTOR ( 'NONE', #24532, 1000.000000000000000 ) ;
#29631 = FACE_OUTER_BOUND ( 'NONE', #27849, .T. ) ;
#29632 = AXIS2_PLACEMENT_3D ( 'NONE', #56372, #28154, #5253 ) ;
#29633 = ORIENTED_EDGE ( 'NONE', *, *, #73220, .T. ) ;
#29634 = DIRECTION ( 'NONE',  ( -1.000000000000000000, 0.000000000000000000, 0.000000000000000000 ) ) ;
#29635 = CARTESIAN_POINT ( 'NONE',  ( 92.35001469846380928, -208.4700133004854194, 76.05645774805350356 ) ) ;
#29636 = AXIS2_PLACEMENT_3D ( 'NONE', #16520, #28913, #34930 ) ;
#29637 = CARTESIAN_POINT ( 'NONE',  ( 0.000000000000000000, -10.96151621346461447, -35.95386929396268272 ) ) ;
#29638 = CARTESIAN_POINT ( 'NONE',  ( 10.00000000000000000, 78.73519480814985627, -22.90783923731548910 ) ) ;
#29639 = CARTESIAN_POINT ( 'NONE',  ( 0.000000000000000000, -71.87247863392443037, 39.47590169984818687 ) ) ;
#29640 = CARTESIAN_POINT ( 'NONE',  ( 97.30629616937498838, -208.6684592857803011, 80.64697916753382856 ) ) ;
#29641 = CIRCLE ( 'NONE', #3295, 82.00000000000000000 ) ;
#29642 = VERTEX_POINT ( 'NONE', #23543 ) ;
#29643 = ORIENTED_EDGE ( 'NONE', *, *, #58465, .T. ) ;
#29644 = CIRCLE ( 'NONE', #5649, 31.99999999999999289 ) ;
#29645 = CARTESIAN_POINT ( 'NONE',  ( 11.99999999999999822, 0.000000000000000000, 0.000000000000000000 ) ) ;
#29646 = VERTEX_POINT ( 'NONE', #290 ) ;
#29647 = DIRECTION ( 'NONE',  ( 0.000000000000000000, 0.8090169943749486725, -0.5877852522924713607 ) ) ;
#29648 = CARTESIAN_POINT ( 'NONE',  ( 96.15314808468750130, -211.9973110713294489, 75.24947916753380639 ) ) ;
#29649 = ORIENTED_EDGE ( 'NONE', *, *, #7016, .F. ) ;
#29650 = CARTESIAN_POINT ( 'NONE',  ( 92.69370383062501162, -208.6684592857803011, 78.31864583420050963 ) ) ;
#29651 = ORIENTED_EDGE ( 'NONE', *, *, #7982, .F. ) ;
#29652 = CARTESIAN_POINT ( 'NONE',  ( -92.34999999999999432, -209.9999999999999716, 88.41249999999999432 ) ) ;
#29653 = ORIENTED_EDGE ( 'NONE', *, *, #58131, .T. ) ;
#29654 = ORIENTED_EDGE ( 'NONE', *, *, #31815, .T. ) ;
#29655 = DIRECTION ( 'NONE',  ( -1.000000000000000000, -0.000000000000000000, -0.000000000000000000 ) ) ;
#29656 = CARTESIAN_POINT ( 'NONE',  ( 5.999999999999998224, 0.000000000000000000, 5.000000000000000000 ) ) ;
#29657 = ORIENTED_EDGE ( 'NONE', *, *, #44908, .T. ) ;
#29658 = B_SPLINE_CURVE_WITH_KNOTS ( 'NONE', 3,
 ( #73, #34590, #29676, #52623, #16561, #57172, #22966, #68821, #12031, #17308, #23326, #40241, #57540, #51891 ),
 .UNSPECIFIED., .F., .F.,
 ( 4, 2, 2, 2, 2, 2, 4 ),
 ( 0.01481111731982464805, 0.01564725794959783214, 0.01648339857937101624, 0.01690146889425760829, 0.01731953920914420034, 0.01773760952403079239, 0.01815567983891738443 ),
 .UNSPECIFIED. ) ;
#29659 = CARTESIAN_POINT ( 'NONE',  ( 97.64999999999999147, -209.9999999999999716, 87.22187500173430408 ) ) ;
#29660 = CARTESIAN_POINT ( 'NONE',  ( 94.99999999999998579, 93.05995642670504253, 88.57124999999999204 ) ) ;
#29661 = ORIENTED_EDGE ( 'NONE', *, *, #3493, .T. ) ;
#29662 = FACE_OUTER_BOUND ( 'NONE', #15900, .T. ) ;
#29663 = ORIENTED_EDGE ( 'NONE', *, *, #48701, .T. ) ;
#29664 = ORIENTED_EDGE ( 'NONE', *, *, #42022, .T. ) ;
#29665 =( BOUNDED_CURVE ( )  B_SPLINE_CURVE ( 2, ( #28002, #44576, #73493, #20883, #16741, #61862, #10347 ),
 .UNSPECIFIED., .F., .F. ) 
 B_SPLINE_CURVE_WITH_KNOTS ( ( 3, 2, 2, 3 ),
 ( 0.3958333333333330373, 0.4027777777777774570, 0.4097222222222218768, 0.4166666666666662966 ),
 .UNSPECIFIED. ) 
 CURVE ( )  GEOMETRIC_REPRESENTATION_ITEM ( )  RATIONAL_B_SPLINE_CURVE ( ( 1.000000000000005329, 0.8660254037844333785, 1.000000000000000000, 0.8660254037844387076, 1.000000000000000000, 0.8660254037844462571, 0.9999999999999924505 ) ) 
 REPRESENTATION_ITEM ( '' )  );
#29666 = DIRECTION ( 'NONE',  ( 0.000000000000000000, 0.000000000000000000, 1.000000000000000000 ) ) ;
#29667 = PRESENTATION_LAYER_ASSIGNMENT (  '', '', ( #62110 ) ) ;
#29668 = VERTEX_POINT ( 'NONE', #62684 ) ;
#29670 = CARTESIAN_POINT ( 'NONE',  ( 94.99999999999998579, 86.94004357329500010, 87.06312500173430635 ) ) ;
#29669 = AXIS2_PLACEMENT_3D ( 'NONE', #30421, #24423, #54119 ) ;
#29671 = EDGE_CURVE ( 'NONE', #16822, #63002, #58608, .T. ) ;
#29672 = VERTEX_POINT ( 'NONE', #45383 ) ;
#29673 = ORIENTED_EDGE ( 'NONE', *, *, #40151, .T. ) ;
#29674 = CARTESIAN_POINT ( 'NONE',  ( 0.000000000000000000, -22.74946021919110706, -29.81001611431033282 ) ) ;
#29675 = ITEM_DEFINED_TRANSFORMATION ( 'NONE', 'NONE', #65229,  #43395 ) ;
#29676 = CARTESIAN_POINT ( 'NONE',  ( -5.000000000000000888, -2.488288133785819589, -1.689848211693934621 ) ) ;
#29677 = VERTEX_POINT ( 'NONE', #4801 ) ;
#29678 = VERTEX_POINT ( 'NONE', #22820 ) ;
#29679 = ADVANCED_FACE ( 'NONE', ( #17166 ), #16424, .T. ) ;
#29680 = ORIENTED_EDGE ( 'NONE', *, *, #64868, .F. ) ;
#29681 = AXIS2_PLACEMENT_3D ( 'NONE', #8838, #31753, #26857 ) ;
#29682 = DIRECTION ( 'NONE',  ( 0.000000000000000000, 0.000000000000000000, 1.000000000000000000 ) ) ;
#29683 = CARTESIAN_POINT ( 'NONE',  ( 12.49999999999999645, 0.000000000000000000, -125.0000000000000000 ) ) ;
#29684 = EDGE_CURVE ( 'NONE', #68371, #36612, #10788, .T. ) ;
#29685 = CARTESIAN_POINT ( 'NONE',  ( -97.65000000000001990, 91.52997821335253548, 87.40708333333333258 ) ) ;
#29686 = ORIENTED_EDGE ( 'NONE', *, *, #35471, .F. ) ;
#29687 = CARTESIAN_POINT ( 'NONE',  ( 97.65000000000000568, 88.47002178664753558, 82.00958333333333883 ) ) ;
#29688 = CARTESIAN_POINT ( 'NONE',  ( 10.00000000000000000, 36.72794159290241822, 65.59268652807223532 ) ) ;
#29689 = ORIENTED_EDGE ( 'NONE', *, *, #26802, .F. ) ;
#29690 = CARTESIAN_POINT ( 'NONE',  ( 92.34999999999999432, 90.00000000000002842, 75.39499999999999602 ) ) ;
#29691 = CARTESIAN_POINT ( 'NONE',  ( -96.15314808468745866, -211.9973110713294489, 81.49364583420047836 ) ) ;
#29693 = ORIENTED_EDGE ( 'NONE', *, *, #15029, .F. ) ;
#29692 = EDGE_CURVE ( 'NONE', #40404, #64515, #17530, .T. ) ;
#29694 = PLANE ( 'NONE',  #11012 ) ;
#29695 = CARTESIAN_POINT ( 'NONE',  ( 95.04693102382874770, -212.6495843973424940, 75.00000002508419072 ) ) ;
#29696 = CARTESIAN_POINT ( 'NONE',  ( 0.000000000000000000, 0.000000000000000000, -44.99999999999998579 ) ) ;
#29697 = CARTESIAN_POINT ( 'NONE',  ( -93.84685191531248449, -208.0026889286704943, 77.36614583420046642 ) ) ;
#29698 = CARTESIAN_POINT ( 'NONE',  ( -12.50000000000000000, -107.5000000000000000, 2.500000000000000000 ) ) ;
#29699 = AXIS2_PLACEMENT_3D ( 'NONE', #2539, #25045, #70898 ) ;
#29700 = DIRECTION ( 'NONE',  ( 0.000000000000000000, 0.2079116908177543743, 0.9781476007338066880 ) ) ;
#29701 = DIRECTION ( 'NONE',  ( 0.000000000000000000, 0.000000000000000000, 1.000000000000000000 ) ) ;
#29702 = DIRECTION ( 'NONE',  ( 0.000000000000000000, 0.000000000000000000, -1.000000000000000000 ) ) ;
#29703 = ADVANCED_FACE ( 'NONE', ( #29908 ), #48322, .T. ) ;
#29704 = CIRCLE ( 'NONE', #36909, 37.49900000000000944 ) ;
#29705 = CARTESIAN_POINT ( 'NONE',  ( 10.00000000000000000, 55.19960302592141232, -51.03279382321027668 ) ) ;
#29706 = EDGE_CURVE ( 'NONE', #59857, #4546, #36986, .T. ) ;
#29707 = CARTESIAN_POINT ( 'NONE',  ( -92.69370383062502583, 88.66845928578038638, 77.20739583420046870 ) ) ;
#29708 = CARTESIAN_POINT ( 'NONE',  ( 11.99999999999999822, -76.69515212745996280, -29.01471420065643869 ) ) ;
#29709 = DIRECTION ( 'NONE',  ( -1.000000000000000000, 0.000000000000000000, 0.000000000000000000 ) ) ;
#29710 = ORIENTED_EDGE ( 'NONE', *, *, #23177, .T. ) ;
#29711 = LINE ( 'NONE', #7543, #48426 ) ;
#29712 = CARTESIAN_POINT ( 'NONE',  ( -3.351853367131006234, 3.838309248099018411, -6.000000000000003553 ) ) ;
#29713 = DIRECTION ( 'NONE',  ( 0.9435911131814402886, -0.3311129884571281101, 0.000000000000000000 ) ) ;
#29714 = EDGE_CURVE ( 'NONE', #11167, #2055, #23794, .T. ) ;
#29715 = EDGE_CURVE ( 'NONE', #66290, #27169, #70129, .T. ) ;
#29716 = CYLINDRICAL_SURFACE ( 'NONE', #1131, 2.649999999999985700 ) ;
#29717 = FACE_OUTER_BOUND ( 'NONE', #19305, .T. ) ;
#29718 = CYLINDRICAL_SURFACE ( 'NONE', #41349, 23.50000000000041922 ) ;
#29719 = CARTESIAN_POINT ( 'NONE',  ( -93.84685191531248449, -208.0026889286704943, 75.61989583420049144 ) ) ;
#29720 = CARTESIAN_POINT ( 'NONE',  ( 0.000000000000000000, -120.0000000000000000, 40.00000000000000711 ) ) ;
#29721 = VERTEX_POINT ( 'NONE', #36294 ) ;
#29722 = CIRCLE ( 'NONE', #47766, 31.99999999999998579 ) ;
#29723 = DIRECTION ( 'NONE',  ( -1.000000000000000000, -0.000000000000000000, -0.000000000000000000 ) ) ;
#29724 = CARTESIAN_POINT ( 'NONE',  ( 92.35000000000000853, -209.9999999999999716, 88.09499999999999886 ) ) ;
#29725 = DIRECTION ( 'NONE',  ( 0.000000000000000000, 0.000000000000000000, 1.000000000000000000 ) ) ;
#29726 = CIRCLE ( 'NONE', #27317, 16.00000000000000000 ) ;
#29727 = CARTESIAN_POINT ( 'NONE',  ( 92.34999999999999432, 90.00000000000002842, 79.20499999999999829 ) ) ;
#29728 = AXIS2_PLACEMENT_3D ( 'NONE', #49583, #3754, #44332 ) ;
#29729 = DIRECTION ( 'NONE',  ( 0.000000000000000000, 0.4999999999999995004, -0.8660254037844389297 ) ) ;
#29730 = ORIENTED_EDGE ( 'NONE', *, *, #60700, .T. ) ;
#29731 = DIRECTION ( 'NONE',  ( 0.000000000000000000, 0.000000000000000000, 1.000000000000000000 ) ) ;
#29732 = DIRECTION ( 'NONE',  ( 0.3090169943749573878, -0.9510565162951503115, 0.000000000000000000 ) ) ;
#29733 = ORIENTED_EDGE ( 'NONE', *, *, #634, .F. ) ;
#29734 = CARTESIAN_POINT ( 'NONE',  ( 92.69370383062501162, -209.9999999999999716, 86.46781250086714010 ) ) ;
#29735 = CARTESIAN_POINT ( 'NONE',  ( -97.64999999999994884, -210.0000359395364171, 83.72937624475883922 ) ) ;
#29736 = ORIENTED_EDGE ( 'NONE', *, *, #28414, .F. ) ;
#29737 = CARTESIAN_POINT ( 'NONE',  ( 97.30629616937498838, -209.9999999999999716, 89.48406250086715374 ) ) ;
#29738 = ORIENTED_EDGE ( 'NONE', *, *, #5274, .F. ) ;
#29739 = CARTESIAN_POINT ( 'NONE',  ( 0.000000000000000000, 14.60985201121729737, -18.46759930825687945 ) ) ;
#29740 = ORIENTED_EDGE ( 'NONE', *, *, #30529, .F. ) ;
#29741 = CARTESIAN_POINT ( 'NONE',  ( -97.30629616937501680, 90.00000000000004263, 79.64156250086715261 ) ) ;
#29742 = AXIS2_PLACEMENT_3D ( 'NONE', #24318, #47249, #70156 ) ;
#29743 = ORIENTED_EDGE ( 'NONE', *, *, #59865, .T. ) ;
#29744 = EDGE_LOOP ( 'NONE', ( #19862, #27628, #23119, #5878 ) ) ;
#29745 = CIRCLE ( 'NONE', #71773, 82.00000000000000000 ) ;
#29746 = CARTESIAN_POINT ( 'NONE',  ( -2.499999999999969802, 76.29999999999999716, -255.0000000000000000 ) ) ;
#29747 = ADVANCED_FACE ( 'NONE', ( #18268 ), #64510, .T. ) ;
#29748 = AXIS2_PLACEMENT_3D ( 'NONE', #11531, #16819, #57407 ) ;
#29749 = EDGE_LOOP ( 'NONE', ( #2019, #32231, #17190, #12203 ) ) ;
#29750 = CARTESIAN_POINT ( 'NONE',  ( -10.90093335751250692, 0.000000000000000000, -13.71399988598171049 ) ) ;
#29751 = CARTESIAN_POINT ( 'NONE',  ( 97.65000000000000568, -211.5299782133524218, 79.46958333333331836 ) ) ;
#29753 = ADVANCED_FACE ( 'NONE', ( #23916 ), #2514, .F. ) ;
#29752 = VECTOR ( 'NONE', #57205, 1000.000000000000000 ) ;
#29754 = ORIENTED_EDGE ( 'NONE', *, *, #51760, .T. ) ;
#29755 = DIRECTION ( 'NONE',  ( 0.000000000000000000, -0.5877852522924624790, -0.8090169943749551118 ) ) ;
#29756 = EDGE_CURVE ( 'NONE', #17478, #16649, #18944, .T. ) ;
#29757 = ORIENTED_EDGE ( 'NONE', *, *, #40380, .T. ) ;
#29758 = VECTOR ( 'NONE', #40290, 1000.000000000000000 ) ;
#29759 = CARTESIAN_POINT ( 'NONE',  ( 93.32700159667687956, 88.01659165168841525, 74.96344747200082281 ) ) ;
#29760 = ORIENTED_EDGE ( 'NONE', *, *, #68828, .T. ) ;
#29761 = EDGE_CURVE ( 'NONE', #42455, #34388, #12257, .T. ) ;
#29762 = EDGE_LOOP ( 'NONE', ( #52820, #28277, #17961, #10990 ) ) ;
#29763 = ORIENTED_EDGE ( 'NONE', *, *, #22956, .T. ) ;
#29764 = CARTESIAN_POINT ( 'NONE',  ( 96.15314808468748708, -208.0026889286704943, 82.44614583420046472 ) ) ;
#29765 = SHAPE_DEFINITION_REPRESENTATION ( #21786, #72820 ) ;
#29766 = DIRECTION ( 'NONE',  ( -1.000000000000000000, -0.000000000000000000, -0.000000000000000000 ) ) ;
#29767 = DIRECTION ( 'NONE',  ( 0.000000000000000000, -0.3826834323650970537, 0.9238795325112838519 ) ) ;
#29768 = LINE ( 'NONE', #69274, #25750 ) ;
#29769 = EDGE_CURVE ( 'NONE', #20594, #54282, #6982, .T. ) ;
#29770 = DIRECTION ( 'NONE',  ( 1.000000000000000000, 0.000000000000000000, -0.000000000000000000 ) ) ;
#29771 = DIRECTION ( 'NONE',  ( -1.000000000000000000, 0.000000000000000000, 0.000000000000000000 ) ) ;
#29772 = DIRECTION ( 'NONE',  ( -1.000000000000000000, -0.000000000000000000, 0.000000000000000000 ) ) ;
#29773 = CARTESIAN_POINT ( 'NONE',  ( -96.15314808468747287, -208.0026889286704943, 85.72697916753379843 ) ) ;
#29774 = CARTESIAN_POINT ( 'NONE',  ( -92.69370383062502583, 91.33154071421968467, 81.28197916753381946 ) ) ;
#29775 = ORIENTED_EDGE ( 'NONE', *, *, #33809, .F. ) ;
#29776 = CARTESIAN_POINT ( 'NONE',  ( 97.30629616937498838, 90.00000000000002842, 81.07031250086714635 ) ) ;
#29777 = ORIENTED_EDGE ( 'NONE', *, *, #44165, .T. ) ;
#29778 = CARTESIAN_POINT ( 'NONE',  ( 0.000000000000000000, 0.000000000000000000, 0.000000000000000000 ) ) ;
#29779 = DIRECTION ( 'NONE',  ( 0.000000000000000000, 0.000000000000000000, 1.000000000000000000 ) ) ;
#29780 = EDGE_CURVE ( 'NONE', #56518, #15417, #15403, .T. ) ;
#29781 = VECTOR ( 'NONE', #60034, 1000.000000000000000 ) ;
#29782 = CARTESIAN_POINT ( 'NONE',  ( 11.99999999999999822, 0.000000000000000000, 0.000000000000000000 ) ) ;
#29783 = DIRECTION ( 'NONE',  ( 0.9730327541852497042, -0.2306669878475622604, 0.000000000000000000 ) ) ;
#29784 = CARTESIAN_POINT ( 'NONE',  ( -92.34999999999999432, -209.9999999999999716, 90.00000000000000000 ) ) ;
#29785 = CARTESIAN_POINT ( 'NONE',  ( -93.84685191531248449, -208.0026889286704943, 86.25614583420048120 ) ) ;
#29786 = AXIS2_PLACEMENT_3D ( 'NONE', #33986, #50146, #39266 ) ;
#29787 = AXIS2_PLACEMENT_3D ( 'NONE', #44638, #67558, #54790 ) ;
#29788 = CARTESIAN_POINT ( 'NONE',  ( 10.00000000000000000, -37.48860685352291711, 0.8828120875899322373 ) ) ;
#29789 = DIRECTION ( 'NONE',  ( -1.000000000000000000, 0.000000000000000000, 0.000000000000000000 ) ) ;
#29790 = CARTESIAN_POINT ( 'NONE',  ( 11.99999999999999822, 22.90783923731629201, 78.73519480814962890 ) ) ;
#29791 = CARTESIAN_POINT ( 'NONE',  ( 97.65000000000000568, 91.52997821335250705, 80.21041666666666003 ) ) ;
#29792 = ORIENTED_EDGE ( 'NONE', *, *, #9944, .T. ) ;
#29793 = AXIS2_PLACEMENT_3D ( 'NONE', #22712, #18527, #28323 ) ;
#29794 = ORIENTED_EDGE ( 'NONE', *, *, #51158, .T. ) ;
#29795 = AXIS2_PLACEMENT_3D ( 'NONE', #61930, #36851, #8282 ) ;
#29796 = CARTESIAN_POINT ( 'NONE',  ( -97.65000000000001990, 91.52997821335253548, 77.88208333333332689 ) ) ;
#29797 = EDGE_CURVE ( 'NONE', #4344, #11208, #69769, .T. ) ;
#29798 = CARTESIAN_POINT ( 'NONE',  ( -92.34999999999999432, -209.9999999999999716, 78.88750000000000284 ) ) ;
#29799 = EDGE_CURVE ( 'NONE', #51292, #72197, #49059, .T. ) ;
#29800 = CARTESIAN_POINT ( 'NONE',  ( -92.69370383062504004, 90.00000000000004263, 89.32531250086714181 ) ) ;
#29801 = DIRECTION ( 'NONE',  ( -1.000000000000000000, -0.000000000000000000, -0.000000000000000000 ) ) ;
#29802 = LINE ( 'NONE', #5796, #25408 ) ;
#29803 = CYLINDRICAL_SURFACE ( 'NONE', #73301, 42.00000000000000000 ) ;
#29804 = CARTESIAN_POINT ( 'NONE',  ( -96.32499999999996021, -207.7050326799711968, 78.46416666666667084 ) ) ;
#29805 = ORIENTED_EDGE ( 'NONE', *, *, #718, .F. ) ;
#29806 = CARTESIAN_POINT ( 'NONE',  ( -92.69370383062502583, 91.33154071421968467, 76.04322916753380923 ) ) ;
#29807 = CIRCLE ( 'NONE', #46670, 16.00000000000000000 ) ;
#29808 = CARTESIAN_POINT ( 'NONE',  ( 12.69589495141918611, -96.69089767102708777, 2.500000000000000000 ) ) ;
#29809 = CARTESIAN_POINT ( 'NONE',  ( 10.00000000000000000, -2.663952781846440576, 41.91543099594817789 ) ) ;
#29810 = VECTOR ( 'NONE', #72928, 1000.000000000000000 ) ;
#29811 = CARTESIAN_POINT ( 'NONE',  ( 11.99999999999999822, -50.95692526931287603, -58.39081064771804819 ) ) ;
#29812 = DIRECTION ( 'NONE',  ( 0.000000000000000000, -0.4067366430757899942, 0.9135454576426055295 ) ) ;
#29813 = CIRCLE ( 'NONE', #23818, 31.99999999999999289 ) ;
#29814 = DIRECTION ( 'NONE',  ( 0.000000000000000000, 0.9510565162951521989, 0.3090169943749517256 ) ) ;
#29815 = CARTESIAN_POINT ( 'NONE',  ( -96.15314808468747287, -208.0026889286704943, 84.61572916753381435 ) ) ;
#29816 = AXIS2_PLACEMENT_3D ( 'NONE', #2445, #2064, #54997 ) ;
#29817 = DIRECTION ( 'NONE',  ( -0.000000000000000000, -1.000000000000000000, -0.000000000000000000 ) ) ;
#29818 = DIRECTION ( 'NONE',  ( -1.000000000000000000, -0.000000000000000000, -0.000000000000000000 ) ) ;
#29819 = CARTESIAN_POINT ( 'NONE',  ( -92.69370383062498320, -208.6684592857803295, 77.47197916753381719 ) ) ;
#29820 = DIRECTION ( 'NONE',  ( -0.000000000000000000, -0.000000000000000000, 1.000000000000000000 ) ) ;
#29821 = ORIENTED_EDGE ( 'NONE', *, *, #61190, .T. ) ;
#29822 = DIRECTION ( 'NONE',  ( 0.000000000000000000, 0.2334453638558991462, 0.9723699203976781114 ) ) ;
#29823 = CARTESIAN_POINT ( 'NONE',  ( 10.00000000000000000, 26.01480285779837232, 70.53064760720326376 ) ) ;
#29824 = DIRECTION ( 'NONE',  ( 1.000000000000000000, 0.000000000000000000, 0.000000000000000000 ) ) ;
#29825 = CARTESIAN_POINT ( 'NONE',  ( -95.00000000000002842, 92.66308142843932671, 76.30781250086715772 ) ) ;
#29826 = CARTESIAN_POINT ( 'NONE',  ( 92.69370383062501162, -211.3315407142195852, 76.99572916753380980 ) ) ;
#29827 = ORIENTED_EDGE ( 'NONE', *, *, #11370, .F. ) ;
#29828 = ADVANCED_FACE ( 'NONE', ( #31017 ), #58875, .F. ) ;
#29829 = CARTESIAN_POINT ( 'NONE',  ( -0.9515373497862389396, -96.47140937769621871, 5.500000000000000000 ) ) ;
#29830 = ORIENTED_EDGE ( 'NONE', *, *, #62402, .F. ) ;
#29831 = VECTOR ( 'NONE', #21939, 1000.000000000000000 ) ;
#29832 = CARTESIAN_POINT ( 'NONE',  ( 0.000000000000000000, 0.000000000000000000, 0.000000000000000000 ) ) ;
#29833 = ORIENTED_EDGE ( 'NONE', *, *, #15027, .F. ) ;
#29834 = CIRCLE ( 'NONE', #17826, 31.99999999999999289 ) ;
#29835 = CIRCLE ( 'NONE', #63466, 31.99999999999999645 ) ;
#29836 = DIRECTION ( 'NONE',  ( 0.000000000000000000, -1.301042606982602560E-15, 1.000000000000000000 ) ) ;
#29837 = AXIS2_PLACEMENT_3D ( 'NONE', #62097, #72247, #16220 ) ;
#29838 = ORIENTED_EDGE ( 'NONE', *, *, #28411, .T. ) ;
#29839 = ORIENTED_EDGE ( 'NONE', *, *, #32048, .T. ) ;
#29840 = EDGE_CURVE ( 'NONE', #20056, #44202, #12620, .T. ) ;
#29841 = ORIENTED_EDGE ( 'NONE', *, *, #16710, .F. ) ;
#29842 = CARTESIAN_POINT ( 'NONE',  ( 10.00000000000000000, 56.15606465355042332, -59.75363087400016582 ) ) ;
#29843 = EDGE_CURVE ( 'NONE', #41355, #12604, #19001, .T. ) ;
#29844 = ORIENTED_EDGE ( 'NONE', *, *, #62423, .T. ) ;
#29845 = ORIENTED_EDGE ( 'NONE', *, *, #18353, .T. ) ;
#29846 = CARTESIAN_POINT ( 'NONE',  ( 97.30629616937498838, 90.00000000000002842, 81.86406250086714920 ) ) ;
#29847 = LINE ( 'NONE', #52803, #53985 ) ;
#29848 = FACE_OUTER_BOUND ( 'NONE', #15906, .T. ) ;
#29849 = AXIS2_PLACEMENT_3D ( 'NONE', #39619, #62178, #45264 ) ;
#29850 = ORIENTED_EDGE ( 'NONE', *, *, #52112, .T. ) ;
#29851 = ADVANCED_FACE ( 'NONE', ( #41568 ), #30283, .T. ) ;
#29853 = ORIENTED_EDGE ( 'NONE', *, *, #53238, .F. ) ;
#29852 = VECTOR ( 'NONE', #4120, 1000.000000000000000 ) ;
#29854 = EDGE_CURVE ( 'NONE', #70242, #63158, #47582, .T. ) ;
#29855 = ORIENTED_EDGE ( 'NONE', *, *, #63613, .T. ) ;
#29856 = CARTESIAN_POINT ( 'NONE',  ( 10.00000000000000000, 6.555932627142418312, 37.01155633439060466 ) ) ;
#29857 = ORIENTED_EDGE ( 'NONE', *, *, #32125, .T. ) ;
#29858 = VECTOR ( 'NONE', #72843, 1000.000000000000000 ) ;
#29859 = DIRECTION ( 'NONE',  ( 1.000000000000000000, 0.000000000000000000, 0.000000000000000000 ) ) ;
#29860 = CARTESIAN_POINT ( 'NONE',  ( 0.000000000000000000, 0.000000000000000000, 0.000000000000000000 ) ) ;
#29861 = CYLINDRICAL_SURFACE ( 'NONE', #61528, 31.99999999999999289 ) ;
#29862 = LINE ( 'NONE', #18225, #9845 ) ;
#29863 = CARTESIAN_POINT ( 'NONE',  ( 95.00000000000000000, -213.0599564267049857, 87.06312500173429214 ) ) ;
#29864 = CARTESIAN_POINT ( 'NONE',  ( -3.000000000000000000, -4.261787119644969479, -26.19803753235780519 ) ) ;
#29865 = CIRCLE ( 'NONE', #45513, 37.49900000000000944 ) ;
#29866 = CARTESIAN_POINT ( 'NONE',  ( 0.000000000000000000, 41.91543099594818500, 2.663952781846294915 ) ) ;
#29867 = CIRCLE ( 'NONE', #58696, 1.500000000000000000 ) ;
#29868 = CARTESIAN_POINT ( 'NONE',  ( -92.34999999999999432, -209.9999999999999716, 80.87187500173430976 ) ) ;
#29869 = ORIENTED_EDGE ( 'NONE', *, *, #61211, .T. ) ;
#29870 = CARTESIAN_POINT ( 'NONE',  ( 10.00000000000000000, -68.67312586195023982, 35.91791733033450384 ) ) ;
#29871 = ORIENTED_EDGE ( 'NONE', *, *, #44492, .F. ) ;
#29873 = CARTESIAN_POINT ( 'NONE',  ( -92.35000000000005116, 91.52997821335253548, 76.47979166840096354 ) ) ;
#29872 = CARTESIAN_POINT ( 'NONE',  ( 94.99999999999998579, 93.05995642670504253, 79.12562500173429214 ) ) ;
#29874 = AXIS2_PLACEMENT_3D ( 'NONE', #69151, #7745, #760 ) ;
#29875 = ORIENTED_EDGE ( 'NONE', *, *, #19668, .F. ) ;
#29876 = CARTESIAN_POINT ( 'NONE',  ( 92.69370383062498320, 90.00000000000002842, 79.64156250086715261 ) ) ;
#29877 = EDGE_CURVE ( 'NONE', #37739, #7050, #64888, .T. ) ;
#29878 = DIRECTION ( 'NONE',  ( -0.000000000000000000, -0.000000000000000000, -1.000000000000000000 ) ) ;
#29879 = FACE_OUTER_BOUND ( 'NONE', #29376, .T. ) ;
#29880 = FACE_OUTER_BOUND ( 'NONE', #16959, .T. ) ;
#29881 = CARTESIAN_POINT ( 'NONE',  ( 10.00000000000000000, -35.53030884539094103, 12.26510123303246935 ) ) ;
#29882 = ORIENTED_EDGE ( 'NONE', *, *, #17232, .T. ) ;
#29883 = DIRECTION ( 'NONE',  ( 1.000000000000000000, 1.427937372958405461E-15, 7.962523111839130290E-16 ) ) ;
#29884 = CARTESIAN_POINT ( 'NONE',  ( 2.500000000000005773, 4.330127018922191873, -6.000000000000000000 ) ) ;
#29885 = ORIENTED_EDGE ( 'NONE', *, *, #6956, .T. ) ;
#29886 = VERTEX_POINT ( 'NONE', #73363 ) ;
#29887 = EDGE_CURVE ( 'NONE', #57102, #37315, #1085, .T. ) ;
#29888 = DIRECTION ( 'NONE',  ( 0.000000000000000000, 0.000000000000000000, 1.000000000000000000 ) ) ;
#29889 = CARTESIAN_POINT ( 'NONE',  ( -2.255011273957059359, -4.471571325851515510, -0.5083873451168858804 ) ) ;
#29890 = LINE ( 'NONE', #17882, #13317 ) ;
#29891 =( BOUNDED_CURVE ( )  B_SPLINE_CURVE ( 2, ( #1824, #64211, #70186, #58185, #19063, #42016, #64950 ),
 .UNSPECIFIED., .F., .F. ) 
 B_SPLINE_CURVE_WITH_KNOTS ( ( 3, 2, 2, 3 ),
 ( 0.5080151867253830389, 0.5150708844844118506, 0.5221266500252946807, 0.5291824299508929297 ),
 .UNSPECIFIED. ) 
 CURVE ( )  GEOMETRIC_REPRESENTATION_ITEM ( )  RATIONAL_B_SPLINE_CURVE ( ( 0.9999974259464162740, 0.8660266908235946248, 1.000000000000000000, 0.8660254037844387076, 1.000000000000000000, 0.8660254037844387076, 1.000000000000000000 ) ) 
 REPRESENTATION_ITEM ( '' )  );
#29892 = CARTESIAN_POINT ( 'NONE',  ( -93.84685191531247028, -211.9973110713294489, 78.58322916753382970 ) ) ;
#29893 = ADVANCED_FACE ( 'NONE', ( #54702 ), #56838, .T. ) ;
#29894 = EDGE_LOOP ( 'NONE', ( #18380, #40086, #50935, #42260 ) ) ;
#29895 = CIRCLE ( 'NONE', #3522, 23.50000000000041922 ) ;
#29896 = VECTOR ( 'NONE', #35729, 1000.000000000000000 ) ;
#29897 = DIRECTION ( 'NONE',  ( 0.000000000000000000, -0.6494480483301741103, -0.7604059656000390355 ) ) ;
#29898 = FACE_OUTER_BOUND ( 'NONE', #8817, .T. ) ;
#29899 = VECTOR ( 'NONE', #12707, 1000.000000000000227 ) ;
#29900 = LINE ( 'NONE', #47946, #43007 ) ;
#29901 = CARTESIAN_POINT ( 'NONE',  ( 11.99999999999999822, 0.000000000000000000, 0.000000000000000000 ) ) ;
#29902 = AXIS2_PLACEMENT_3D ( 'NONE', #30384, #30010, #52962 ) ;
#29903 = DIRECTION ( 'NONE',  ( 0.000000000000000000, 0.000000000000000000, 1.000000000000000000 ) ) ;
#29904 = DIRECTION ( 'NONE',  ( 0.000000000000000000, 0.000000000000000000, -1.000000000000000000 ) ) ;
#29905 = CARTESIAN_POINT ( 'NONE',  ( 10.00000000000000000, 62.50329211542435104, 41.76937507738811917 ) ) ;
#29906 = DIRECTION ( 'NONE',  ( 0.000000000000000000, 0.000000000000000000, 1.000000000000000000 ) ) ;
#29907 = CARTESIAN_POINT ( 'NONE',  ( 10.00000000000000000, 0.000000000000000000, 0.000000000000000000 ) ) ;
#29908 = FACE_OUTER_BOUND ( 'NONE', #35122, .T. ) ;
#29909 = CARTESIAN_POINT ( 'NONE',  ( 97.30629616937498838, 91.33154071421968467, 87.63197916753381378 ) ) ;
#29910 = AXIS2_PLACEMENT_3D ( 'NONE', #32202, #16415, #49139 ) ;
#29911 = CARTESIAN_POINT ( 'NONE',  ( -93.84685191531247028, -211.9973110713294489, 87.47322916753381605 ) ) ;
#29912 = PLANE ( 'NONE',  #71020 ) ;
#29913 = AXIS2_PLACEMENT_3D ( 'NONE', #17318, #40252, #63200 ) ;
#29914 = ORIENTED_EDGE ( 'NONE', *, *, #67206, .T. ) ;
#29915 = CARTESIAN_POINT ( 'NONE',  ( 97.64999999999999147, -209.9999999999999716, 79.52249999999999375 ) ) ;
#29916 = CARTESIAN_POINT ( 'NONE',  ( -97.64999999999994884, -208.4700217866474645, 81.05708333333333826 ) ) ;
#29917 = CARTESIAN_POINT ( 'NONE',  ( -96.15314808468752972, 91.99731107132950569, 76.83697916753381207 ) ) ;
#29918 = AXIS2_PLACEMENT_3D ( 'NONE', #26688, #49613, #66914 ) ;
#29919 = AXIS2_PLACEMENT_3D ( 'NONE', #12741, #58247, #46973 ) ;
#29920 = AXIS2_PLACEMENT_3D ( 'NONE', #33056, #9390, #66187 ) ;
#29921 = CARTESIAN_POINT ( 'NONE',  ( 93.84685191531251292, -211.9973110713294489, 87.20864583420046756 ) ) ;
#29922 = ORIENTED_EDGE ( 'NONE', *, *, #59180, .F. ) ;
#29923 = EDGE_CURVE ( 'NONE', #27079, #49481, #20109, .T. ) ;
#29924 = ORIENTED_EDGE ( 'NONE', *, *, #27975, .T. ) ;
#29925 = ORIENTED_EDGE ( 'NONE', *, *, #12954, .T. ) ;
#29926 = CARTESIAN_POINT ( 'NONE',  ( 26.47460221209471598, -121.8961639463267090, 2.500000000000000000 ) ) ;
#29927 = EDGE_CURVE ( 'NONE', #27546, #64186, #50441, .T. ) ;
#29928 = LINE ( 'NONE', #1421, #31829 ) ;
#29929 = ORIENTED_EDGE ( 'NONE', *, *, #9534, .T. ) ;
#29930 = EDGE_CURVE ( 'NONE', #23323, #74042, #55012, .T. ) ;
#29931 = ORIENTED_EDGE ( 'NONE', *, *, #62833, .F. ) ;
#29932 = CARTESIAN_POINT ( 'NONE',  ( 92.69370383062501162, -208.6684592857803295, 80.22364583420048234 ) ) ;
#29933 = CARTESIAN_POINT ( 'NONE',  ( 11.99999999999999822, 0.000000000000000000, 0.000000000000000000 ) ) ;
#29934 = FACE_OUTER_BOUND ( 'NONE', #55300, .T. ) ;
#29935 = CARTESIAN_POINT ( 'NONE',  ( 0.000000000000000000, -10.45096189432344147, 21.10159698893426494 ) ) ;
#29936 = CARTESIAN_POINT ( 'NONE',  ( 11.99999999999999822, 73.95703589263975175, 23.16143007188452785 ) ) ;
#29937 = AXIS2_PLACEMENT_3D ( 'NONE', #20269, #43233, #14634 ) ;
#29938 = ADVANCED_FACE ( 'NONE', ( #73731 ), #16600, .F. ) ;
#29939 = DIRECTION ( 'NONE',  ( 0.000000000000000000, -0.4539904997395350916, -0.8910065241883738940 ) ) ;
#29940 = CARTESIAN_POINT ( 'NONE',  ( 97.64999999999999147, -209.9999999999999716, 85.87249999999998806 ) ) ;
#29941 = CIRCLE ( 'NONE', #16771, 23.50000000000041922 ) ;
#29942 = ORIENTED_EDGE ( 'NONE', *, *, #44164, .T. ) ;
#29943 = EDGE_CURVE ( 'NONE', #23233, #55121, #64625, .T. ) ;
#29944 = ORIENTED_EDGE ( 'NONE', *, *, #67200, .F. ) ;
#29945 = CIRCLE ( 'NONE', #61198, 82.00000000000000000 ) ;
#29946 = ORIENTED_EDGE ( 'NONE', *, *, #7060, .T. ) ;
#29947 = ORIENTED_EDGE ( 'NONE', *, *, #14926, .T. ) ;
#29948 = CARTESIAN_POINT ( 'NONE',  ( 11.99999999999999822, 0.000000000000000000, 0.000000000000000000 ) ) ;
#29949 = CARTESIAN_POINT ( 'NONE',  ( -95.00000000000002842, 92.66308142843932671, 88.37281250086715545 ) ) ;
#29950 = CARTESIAN_POINT ( 'NONE',  ( 10.00000000000000000, -12.42422080174663712, 35.38097989696507994 ) ) ;
#29951 = CIRCLE ( 'NONE', #21587, 77.49899999999999523 ) ;
#29952 = DIRECTION ( 'NONE',  ( 0.000000000000000000, 0.8910065241883657894, 0.4539904997395510788 ) ) ;
#29953 = CARTESIAN_POINT ( 'NONE',  ( 97.64999999999997726, -208.4700217866474645, 74.57479166840096241 ) ) ;
#29954 = CARTESIAN_POINT ( 'NONE',  ( 94.99999999999998579, 93.05995642670504253, 77.77624999999999034 ) ) ;
#29955 = VERTEX_POINT ( 'NONE', #45190 ) ;
#29956 = CYLINDRICAL_SURFACE ( 'NONE', #11946, 82.00000000000000000 ) ;
#29957 = ORIENTED_EDGE ( 'NONE', *, *, #5196, .F. ) ;
#29958 = CARTESIAN_POINT ( 'NONE',  ( 97.64999999999997726, -211.5299782133524218, 80.10458333333330927 ) ) ;
#29959 = EDGE_CURVE ( 'NONE', #73572, #32622, #61029, .T. ) ;
#29960 = ORIENTED_EDGE ( 'NONE', *, *, #12405, .F. ) ;
#29961 = CARTESIAN_POINT ( 'NONE',  ( -96.32500000000001705, 92.29496732002878900, 87.43354166840096298 ) ) ;
#29962 = CARTESIAN_POINT ( 'NONE',  ( 96.15314808468748708, 91.99731107132950569, 74.82614583420047438 ) ) ;
#29963 = EDGE_CURVE ( 'NONE', #17478, #57845, #52661, .T. ) ;
#29964 = ORIENTED_EDGE ( 'NONE', *, *, #53571, .F. ) ;
#29965 = EDGE_CURVE ( 'NONE', #32553, #2885, #35799, .T. ) ;
#29966 = CARTESIAN_POINT ( 'NONE',  ( 10.00000000000000000, 36.88895765772642932, -6.736453364083163642 ) ) ;
#29967 = CARTESIAN_POINT ( 'NONE',  ( 0.000000000000000000, 0.000000000000000000, 0.000000000000000000 ) ) ;
#29968 = CIRCLE ( 'NONE', #17958, 31.99999999999999289 ) ;
#29969 = DIRECTION ( 'NONE',  ( -1.000000000000000000, 0.000000000000000000, 0.000000000000000000 ) ) ;
#29970 = DIRECTION ( 'NONE',  ( -1.000000000000000000, -0.000000000000000000, 0.000000000000000000 ) ) ;
#29971 = VERTEX_POINT ( 'NONE', #59993 ) ;
#29972 = DIRECTION ( 'NONE',  ( 0.000000000000000000, 0.000000000000000000, 1.000000000000000000 ) ) ;
#29973 = EDGE_CURVE ( 'NONE', #36744, #71285, #11803, .T. ) ;
#29974 = CIRCLE ( 'NONE', #66011, 16.00000000000000000 ) ;
#29976 = CARTESIAN_POINT ( 'NONE',  ( -92.69370383062498320, -211.3315407142195852, 75.30239583420048177 ) ) ;
#29975 = AXIS2_PLACEMENT_3D ( 'NONE', #11492, #62657, #67531 ) ;
#29977 = ORIENTED_EDGE ( 'NONE', *, *, #26784, .F. ) ;
#29978 = ORIENTED_EDGE ( 'NONE', *, *, #64365, .T. ) ;
#29979 = DIRECTION ( 'NONE',  ( 0.000000000000000000, 0.000000000000000000, 1.000000000000000000 ) ) ;
#29980 = VECTOR ( 'NONE', #71922, 1000.000000000000000 ) ;
#29981 = VECTOR ( 'NONE', #50267, 1000.000000000000114 ) ;
#29982 = EDGE_CURVE ( 'NONE', #17939, #20251, #70610, .T. ) ;
#29983 = FACE_OUTER_BOUND ( 'NONE', #73898, .T. ) ;
#29984 = CARTESIAN_POINT ( 'NONE',  ( 0.000000000000000000, 50.23322058963442061, -64.81221759200289512 ) ) ;
#29985 = ORIENTED_EDGE ( 'NONE', *, *, #67817, .T. ) ;
#29986 = CARTESIAN_POINT ( 'NONE',  ( -94.99999999999997158, -212.6630814284392557, 87.42031250086715488 ) ) ;
#29987 = ORIENTED_EDGE ( 'NONE', *, *, #17176, .T. ) ;
#29988 = VERTEX_POINT ( 'NONE', #33139 ) ;
#29989 = VERTEX_POINT ( 'NONE', #8843 ) ;
#29990 = CARTESIAN_POINT ( 'NONE',  ( -97.64999999950686060, 89.99996796133669363, 83.73041644179562581 ) ) ;
#29991 = FACE_OUTER_BOUND ( 'NONE', #71901, .T. ) ;
#29992 = CARTESIAN_POINT ( 'NONE',  ( 94.99999999999998579, 92.66308142843932671, 82.49906250086715431 ) ) ;
#29993 = FACE_OUTER_BOUND ( 'NONE', #33856, .T. ) ;
#29994 = DIRECTION ( 'NONE',  ( 7.705842312279274921E-15, -1.000000000000000000, 2.546204323184492723E-14 ) ) ;
#29995 = DIRECTION ( 'NONE',  ( -1.000000000000000000, 0.000000000000000000, 0.000000000000000000 ) ) ;
#29996 = CARTESIAN_POINT ( 'NONE',  ( 0.000000000000000000, -1.278221433540502217, 26.51162292216071847 ) ) ;
#29997 = DIRECTION ( 'NONE',  ( 0.000000000000000000, 0.000000000000000000, 1.000000000000000000 ) ) ;
#29998 = CYLINDRICAL_SURFACE ( 'NONE', #16719, 42.00000000000000000 ) ;
#29999 = CARTESIAN_POINT ( 'NONE',  ( -35.37301231164799731, -117.0000000000000000, -2.500000000000000000 ) ) ;
#30000 = VECTOR ( 'NONE', #66022, 1000.000000000000000 ) ;
#30001 = CARTESIAN_POINT ( 'NONE',  ( 11.99999999999999822, -59.46389618801929089, -49.70050353004953081 ) ) ;
#30002 = DIRECTION ( 'NONE',  ( 1.000000000000000000, -0.000000000000000000, -0.000000000000000000 ) ) ;
#30003 = CARTESIAN_POINT ( 'NONE',  ( -97.30629616937501680, 90.00000000000004263, 87.10281250086714522 ) ) ;
#30004 = CARTESIAN_POINT ( 'NONE',  ( 10.00000000000000000, 77.19088730480534366, -6.903761155836915187 ) ) ;
#30005 = AXIS2_PLACEMENT_3D ( 'NONE', #57450, #55960, #68370 ) ;
#30006 = CYLINDRICAL_SURFACE ( 'NONE', #55268, 12.75000000000265565 ) ;
#30007 = ORIENTED_EDGE ( 'NONE', *, *, #10807, .T. ) ;
#30008 = FACE_OUTER_BOUND ( 'NONE', #40924, .T. ) ;
#30009 = CARTESIAN_POINT ( 'NONE',  ( 12.50000000000000000, -132.5000000000000000, -2.500000000000000000 ) ) ;
#30010 = DIRECTION ( 'NONE',  ( -1.000000000000000000, 0.000000000000000000, -0.000000000000000000 ) ) ;
#30011 = EDGE_CURVE ( 'NONE', #70, #30710, #29835, .T. ) ;
#30012 = VECTOR ( 'NONE', #29599, 1000.000000000000000 ) ;
#30013 = EDGE_CURVE ( 'NONE', #30109, #40304, #48688, .T. ) ;
#30014 = LINE ( 'NONE', #63153, #16440 ) ;
#30015 = VECTOR ( 'NONE', #25112, 1000.000000000000000 ) ;
#30016 = AXIS2_PLACEMENT_3D ( 'NONE', #55399, #73041, #6859 ) ;
#30017 = CIRCLE ( 'NONE', #72047, 2.650000000000540812 ) ;
#30018 = CARTESIAN_POINT ( 'NONE',  ( 96.15314808468750130, -211.9973110713294489, 83.66322916753382799 ) ) ;
#30019 = ADVANCED_FACE ( 'NONE', ( #71610 ), #56085, .T. ) ;
#30020 = ORIENTED_EDGE ( 'NONE', *, *, #49494, .T. ) ;
#30021 = VECTOR ( 'NONE', #56421, 1000.000000000000000 ) ;
#30022 = EDGE_CURVE ( 'NONE', #14616, #11957, #14217, .T. ) ;
#30023 = EDGE_LOOP ( 'NONE', ( #7005, #7064, #19323, #8338 ) ) ;
#30024 = AXIS2_PLACEMENT_3D ( 'NONE', #51197, #40673, #486 ) ;
#30025 = CARTESIAN_POINT ( 'NONE',  ( 0.000000000000000000, 49.70050353004977239, -59.46389618801908483 ) ) ;
#30026 = ORIENTED_EDGE ( 'NONE', *, *, #13888, .F. ) ;
#30027 = DIRECTION ( 'NONE',  ( -1.000000000000000000, 0.000000000000000000, -0.000000000000000000 ) ) ;
#30028 = ADVANCED_FACE ( 'NONE', ( #16232 ), #39171, .T. ) ;
#30029 = CARTESIAN_POINT ( 'NONE',  ( 97.30629616937498838, -209.9999999999999716, 75.35531250086714294 ) ) ;
#30030 = EDGE_LOOP ( 'NONE', ( #2814, #28287, #60956, #34005 ) ) ;
#30031 = CARTESIAN_POINT ( 'NONE',  ( 93.84685191531249870, -208.0026889286704943, 78.90072916753382515 ) ) ;
#30032 = ORIENTED_EDGE ( 'NONE', *, *, #33286, .F. ) ;
#30033 = DIRECTION ( 'NONE',  ( 0.000000000000000000, 1.000000000000000000, 0.000000000000000000 ) ) ;
#30034 = VERTEX_POINT ( 'NONE', #29352 ) ;
#30035 = AXIS2_PLACEMENT_3D ( 'NONE', #1125, #18000, #64606 ) ;
#30036 = VERTEX_POINT ( 'NONE', #51924 ) ;
#30037 = DIRECTION ( 'NONE',  ( 0.000000000000000000, 0.000000000000000000, 1.000000000000000000 ) ) ;
#30038 = DIRECTION ( 'NONE',  ( 0.000000000000000000, -0.7071067811865389130, -0.7071067811865562325 ) ) ;
#30039 = ORIENTED_EDGE ( 'NONE', *, *, #40263, .T. ) ;
#30040 = CARTESIAN_POINT ( 'NONE',  ( -92.35000000000003695, 90.00000000000004263, 83.96750000000000114 ) ) ;
#30041 = CARTESIAN_POINT ( 'NONE',  ( 92.35000000000002274, -208.4700217866474645, 83.67645833506762187 ) ) ;
#30042 = CARTESIAN_POINT ( 'NONE',  ( 97.64999999999997726, 91.52997821335252127, 88.46541666666665549 ) ) ;
#30043 = VERTEX_POINT ( 'NONE', #47037 ) ;
#30044 = CARTESIAN_POINT ( 'NONE',  ( 10.00000000000000000, -36.73666225445845157, -65.58780272294114866 ) ) ;
#30045 = DIRECTION ( 'NONE',  ( 1.000000000000000000, 0.000000000000000000, 0.000000000000000000 ) ) ;
#30046 = ORIENTED_EDGE ( 'NONE', *, *, #21888, .F. ) ;
#30047 = EDGE_LOOP ( 'NONE', ( #56241, #23409, #60307, #19105 ) ) ;
#30048 = CARTESIAN_POINT ( 'NONE',  ( 5.000000000000000000, -0.9645339558193165574, -0.6919071587033235327 ) ) ;
#30049 = ORIENTED_EDGE ( 'NONE', *, *, #40670, .F. ) ;
#30050 = CARTESIAN_POINT ( 'NONE',  ( 92.34999999999999432, 91.52997821335252127, 85.58145833506763722 ) ) ;
#30051 = VECTOR ( 'NONE', #7627, 1000.000000000000000 ) ;
#30052 = ORIENTED_EDGE ( 'NONE', *, *, #68989, .F. ) ;
#30053 =( NAMED_UNIT ( * ) PLANE_ANGLE_UNIT ( ) SI_UNIT ( $, .RADIAN. ) );
#30054 = EDGE_LOOP ( 'NONE', ( #38743, #53540, #48985, #6677 ) ) ;
#30055 = CYLINDRICAL_SURFACE ( 'NONE', #52488, 16.00000000000000000 ) ;
#30056 = VECTOR ( 'NONE', #33705, 1000.000000000000000 ) ;
#30057 = ADVANCED_FACE ( 'NONE', ( #69224 ), #57945, .T. ) ;
#30058 = ADVANCED_FACE ( 'NONE', ( #58309 ), #109, .F. ) ;
#30059 = CARTESIAN_POINT ( 'NONE',  ( -97.64999999999986358, -208.4700217866474361, 75.34208333333333485 ) ) ;
#30060 = ORIENTED_EDGE ( 'NONE', *, *, #4341, .F. ) ;
#30061 = ORIENTED_EDGE ( 'NONE', *, *, #13977, .F. ) ;
#30062 = AXIS2_PLACEMENT_3D ( 'NONE', #36722, #26179, #9641 ) ;
#30063 = EDGE_LOOP ( 'NONE', ( #13948, #23171, #31603, #8549 ) ) ;
#30064 = PLANE ( 'NONE',  #72149 ) ;
#30065 = DIRECTION ( 'NONE',  ( 0.000000000000000000, 0.000000000000000000, 1.000000000000000000 ) ) ;
#30066 = CARTESIAN_POINT ( 'NONE',  ( -95.00000000000002842, 86.94004357329504273, 88.88875000000000171 ) ) ;
#30067 = VERTEX_POINT ( 'NONE', #68491 ) ;
#30068 = EDGE_CURVE ( 'NONE', #11705, #67975, #12990, .T. ) ;
#30069 = FACE_OUTER_BOUND ( 'NONE', #57444, .T. ) ;
#30070 = CARTESIAN_POINT ( 'NONE',  ( 0.000000000000000000, 20.85821328998756385, -10.92862929874494959 ) ) ;
#30071 = ORIENTED_EDGE ( 'NONE', *, *, #31292, .T. ) ;
#30072 = LINE ( 'NONE', #71028, #44396 ) ;
#30073 = CARTESIAN_POINT ( 'NONE',  ( -94.99999999999997158, -207.3369185715606307, 82.49906250086714010 ) ) ;
#30074 = ORIENTED_EDGE ( 'NONE', *, *, #10015, .T. ) ;
#30075 = DIRECTION ( 'NONE',  ( -0.000000000000000000, -0.000000000000000000, 1.000000000000000000 ) ) ;
#30076 = DIRECTION ( 'NONE',  ( 0.000000000000000000, 0.000000000000000000, 1.000000000000000000 ) ) ;
#30077 = CARTESIAN_POINT ( 'NONE',  ( 94.99999999999998579, 93.05995642670504253, 89.28562500173430294 ) ) ;
#30078 = CARTESIAN_POINT ( 'NONE',  ( 11.99999999999999822, 65.58780272294129077, -36.73666225445822420 ) ) ;
#30079 = CIRCLE ( 'NONE', #22851, 16.00000000000000000 ) ;
#30080 = LINE ( 'NONE', #30442, #65568 ) ;
#30081 = AXIS2_PLACEMENT_3D ( 'NONE', #35784, #30152, #65496 ) ;
#30082 = AXIS2_PLACEMENT_3D ( 'NONE', #65768, #72135, #60508 ) ;
#30083 = DIRECTION ( 'NONE',  ( -1.000000000000000000, 0.000000000000000000, 0.000000000000000000 ) ) ;
#30084 = DIRECTION ( 'NONE',  ( -0.000000000000000000, -0.5000000000000003331, -0.8660254037844384856 ) ) ;
#30085 = DIRECTION ( 'NONE',  ( -7.632783294297813165E-16, -1.065814103640131188E-14, -1.000000000000000000 ) ) ;
#30086 = CIRCLE ( 'NONE', #64931, 37.49900000000000944 ) ;
#30087 = DIRECTION ( 'NONE',  ( -1.000000000000000000, 0.000000000000000000, 0.000000000000000000 ) ) ;
#30088 = CARTESIAN_POINT ( 'NONE',  ( 0.000000000000000000, -76.66974797899828786, -11.30684508768421992 ) ) ;
#30089 = CARTESIAN_POINT ( 'NONE',  ( -97.30629616937501680, 90.00000000000004263, 79.48281250086714067 ) ) ;
#30090 = DIRECTION ( 'NONE',  ( -0.000000000000000000, -0.000000000000000000, 1.000000000000000000 ) ) ;
#30091 = CARTESIAN_POINT ( 'NONE',  ( 97.65000000000004832, 88.47002178664756400, 76.29458333333333542 ) ) ;
#30092 = DIRECTION ( 'NONE',  ( 0.000000000000000000, 0.000000000000000000, -1.000000000000000000 ) ) ;
#30093 = CARTESIAN_POINT ( 'NONE',  ( 0.000000000000000000, 0.000000000000000000, 0.000000000000000000 ) ) ;
#30094 = CARTESIAN_POINT ( 'NONE',  ( -10.00000000000000000, 0.000000000000000000, 0.000000000000000000 ) ) ;
#30095 = CARTESIAN_POINT ( 'NONE',  ( 0.000000000000000000, -35.95386929396264009, 10.96151621346475658 ) ) ;
#30096 = DIRECTION ( 'NONE',  ( -1.000000000000000000, -0.000000000000000000, -0.000000000000000000 ) ) ;
#30097 = FACE_OUTER_BOUND ( 'NONE', #22767, .T. ) ;
#30098 = CARTESIAN_POINT ( 'NONE',  ( -97.30629616937497417, -208.6684592857803011, 76.41364583420049428 ) ) ;
#30099 = DIRECTION ( 'NONE',  ( -0.000000000000000000, -0.000000000000000000, -1.000000000000000000 ) ) ;
#30100 = VERTEX_POINT ( 'NONE', #57206 ) ;
#30101 = DIRECTION ( 'NONE',  ( 0.000000000000000000, 0.000000000000000000, -1.000000000000000000 ) ) ;
#30102 = DIRECTION ( 'NONE',  ( -7.685483754327489091E-16, -1.065814103640131188E-14, -1.000000000000000000 ) ) ;
#30103 = DIRECTION ( 'NONE',  ( -1.000000000000000000, 0.000000000000000000, 0.000000000000000000 ) ) ;
#30104 = CYLINDRICAL_SURFACE ( 'NONE', #35338, 26.50000000000552092 ) ;
#30105 = AXIS2_PLACEMENT_3D ( 'NONE', #58121, #7364, #18626 ) ;
#30106 = AXIS2_PLACEMENT_3D ( 'NONE', #16694, #5062, #68198 ) ;
#30107 = EDGE_CURVE ( 'NONE', #59010, #70889, #74229, .T. ) ;
#30108 = PLANE ( 'NONE',  #40329 ) ;
#30109 = VERTEX_POINT ( 'NONE', #63600 ) ;
#30110 = EDGE_CURVE ( 'NONE', #53386, #8327, #51423, .T. ) ;
#30111 = LINE ( 'NONE', #53062, #53922 ) ;
#30112 = CYLINDRICAL_SURFACE ( 'NONE', #39173, 31.99999999999998579 ) ;
#30113 = VERTEX_POINT ( 'NONE', #5713 ) ;
#30114 =( BOUNDED_CURVE ( )  B_SPLINE_CURVE ( 2, ( #74134, #29735, #62891, #11349, #492, #34284, #23024, #17732, #1238 ),
 .UNSPECIFIED., .F., .F. ) 
 B_SPLINE_CURVE_WITH_KNOTS ( ( 3, 2, 2, 2, 3 ),
 ( 0.3810111478283708664, 0.3810113392095190732, 0.3880671047504364868, 0.3951228702913539559, 0.4021785743347534581 ),
 .UNSPECIFIED. ) 
 CURVE ( )  GEOMETRIC_REPRESENTATION_ITEM ( )  RATIONAL_B_SPLINE_CURVE ( ( 0.9999927323218336106, 0.9999963660623495398, 1.000000000000000000, 0.8660254037844387076, 1.000000000000000000, 0.8660254037844387076, 1.000000000000000000, 0.8660265714968692352, 0.9999976645954944399 ) ) 
 REPRESENTATION_ITEM ( '' )  );
#30115 = EDGE_CURVE ( 'NONE', #67482, #1736, #469, .T. ) ;
#30116 = CARTESIAN_POINT ( 'NONE',  ( 96.15314808468748708, -208.0026889286704943, 84.98614583420047097 ) ) ;
#30117 = CARTESIAN_POINT ( 'NONE',  ( 95.00000000000000000, -207.3369185715606307, 87.10281250086715943 ) ) ;
#30118 = ORIENTED_EDGE ( 'NONE', *, *, #6534, .T. ) ;
#30119 = DIRECTION ( 'NONE',  ( -1.000000000000000000, 0.000000000000000000, -0.000000000000000000 ) ) ;
#30120 = CIRCLE ( 'NONE', #50530, 16.00000000000000000 ) ;
#30121 = EDGE_LOOP ( 'NONE', ( #63827, #65854, #40532, #61137, #55371, #50030, #66847, #34007, #38159, #16953, #11820, #22360, #30318, #37575, #6055, #22840, #16562, #47614, #24345, #73061, #69295, #69612, #74129, #13432, #62897, #1, #9483, #62988, #13863, #8330, #64958, #11145, #18377, #4639, #8167, #7588, #44680, #47587, #10340, #18396, #57985, #7526, #44584, #10477, #33448, #37680, #62443, #62577, #16834, #48006, #38924, #7718 ) ) ;
#30122 = DIRECTION ( 'NONE',  ( 1.000000000000000000, -0.000000000000000000, 0.000000000000000000 ) ) ;
#30123 = VERTEX_POINT ( 'NONE', #41388 ) ;
#30124 = AXIS2_PLACEMENT_3D ( 'NONE', #51722, #270, #23162 ) ;
#30125 = CARTESIAN_POINT ( 'NONE',  ( -92.69370383062502583, 91.33154071421968467, 81.28197916753381946 ) ) ;
#30126 = AXIS2_PLACEMENT_3D ( 'NONE', #5231, #3743, #26645 ) ;
#30127 = ORIENTED_EDGE ( 'NONE', *, *, #62895, .F. ) ;
#30128 = ORIENTED_EDGE ( 'NONE', *, *, #11109, .F. ) ;
#30129 = DIRECTION ( 'NONE',  ( 0.000000000000000000, 0.9723699203976773342, -0.2334453638559024213 ) ) ;
#30130 = VECTOR ( 'NONE', #71141, 1000.000000000000000 ) ;
#30131 = EDGE_LOOP ( 'NONE', ( #37659, #64076, #40384, #44234 ) ) ;
#30132 = DIRECTION ( 'NONE',  ( 0.000000000000000000, -0.9510565162951500895, -0.3090169943749583870 ) ) ;
#30133 = FACE_OUTER_BOUND ( 'NONE', #6848, .T. ) ;
#30134 = EDGE_CURVE ( 'NONE', #34985, #46802, #40647, .T. ) ;
#30135 = EDGE_CURVE ( 'NONE', #73972, #11744, #63226, .T. ) ;
#30136 = ORIENTED_EDGE ( 'NONE', *, *, #43894, .T. ) ;
#30137 = DIRECTION ( 'NONE',  ( -1.000000000000000000, -0.000000000000000000, 0.000000000000000000 ) ) ;
#30138 = ORIENTED_EDGE ( 'NONE', *, *, #42295, .T. ) ;
#30139 = LINE ( 'NONE', #69984, #70810 ) ;
#30140 = ORIENTED_EDGE ( 'NONE', *, *, #70041, .T. ) ;
#30141 = ORIENTED_EDGE ( 'NONE', *, *, #40392, .T. ) ;
#30142 = EDGE_LOOP ( 'NONE', ( #46892, #22744, #41143, #23665 ) ) ;
#30143 = CARTESIAN_POINT ( 'NONE',  ( 97.30629616937498838, -211.3315407142195852, 81.65239583420049030 ) ) ;
#30145 = EDGE_CURVE ( 'NONE', #35960, #10633, #5831, .T. ) ;
#30144 = DIRECTION ( 'NONE',  ( -1.000000000000000000, 0.000000000000000000, 0.000000000000000000 ) ) ;
#30146 = EDGE_CURVE ( 'NONE', #23492, #32553, #39922, .T. ) ;
#30147 = SHAPE_DEFINITION_REPRESENTATION ( #9143, #67135 ) ;
#30148 = CARTESIAN_POINT ( 'NONE',  ( -93.67499999999998295, -212.2949673200287179, 85.84604166840097150 ) ) ;
#30149 = CARTESIAN_POINT ( 'NONE',  ( 10.00000000000000000, -0.6853352020793173072, 37.58145647212453611 ) ) ;
#30150 = DIRECTION ( 'NONE',  ( -1.000000000000000000, 0.000000000000000000, 0.000000000000000000 ) ) ;
#30151 = DIRECTION ( 'NONE',  ( 0.000000000000000000, -0.9876883405951393247, 0.1564344650402204329 ) ) ;
#30152 = DIRECTION ( 'NONE',  ( -1.000000000000000000, 0.000000000000000000, 0.000000000000000000 ) ) ;
#30153 = CARTESIAN_POINT ( 'NONE',  ( 0.000000000000000000, 0.000000000000000000, -125.0000000000000000 ) ) ;
#30154 = CARTESIAN_POINT ( 'NONE',  ( -94.99999999999997158, -207.3369185715606307, 83.76906250086713612 ) ) ;
#30155 = CARTESIAN_POINT ( 'NONE',  ( -96.15314808468752972, 91.99731107132950569, 83.98072916753382344 ) ) ;
#30156 = ORIENTED_EDGE ( 'NONE', *, *, #8737, .T. ) ;
#30157 = CARTESIAN_POINT ( 'NONE',  ( 93.84685191531248449, 88.00268892867053694, 82.12864583420046927 ) ) ;
#30158 = ORIENTED_EDGE ( 'NONE', *, *, #48396, .T. ) ;
#30159 = CARTESIAN_POINT ( 'NONE',  ( 0.000000000000000000, -38.55633173626998911, -16.65560815589452304 ) ) ;
#30160 = LINE ( 'NONE', #18509, #44352 ) ;
#30161 = DIRECTION ( 'NONE',  ( 0.000000000000000000, 0.000000000000000000, 1.000000000000000000 ) ) ;
#30162 = LINE ( 'NONE', #34330, #58348 ) ;
#30163 = CARTESIAN_POINT ( 'NONE',  ( 15.00000000000000000, 8.688484142254226938, 21.88630264137359305 ) ) ;
#30164 = CARTESIAN_POINT ( 'NONE',  ( -93.84685191531247028, -211.9973110713294489, 86.67947916753381321 ) ) ;
#30165 = DIRECTION ( 'NONE',  ( -1.000000000000000000, -0.000000000000000000, 0.000000000000000000 ) ) ;
#30166 = PRESENTATION_LAYER_ASSIGNMENT (  '', '', ( #37375 ) ) ;
#30167 = AXIS2_PLACEMENT_3D ( 'NONE', #59864, #18877, #70372 ) ;
#30168 = CARTESIAN_POINT ( 'NONE',  ( 12.00000000000000000, -22.67460108101782978, -6.353146135317906840 ) ) ;
#30169 = CARTESIAN_POINT ( 'NONE',  ( -12.50000000000000000, -132.5000000000000000, 40.00000000000000000 ) ) ;
#30170 = VECTOR ( 'NONE', #62009, 1000.000000000000000 ) ;
#30171 = LINE ( 'NONE', #69663, #3660 ) ;
#30172 = ORIENTED_EDGE ( 'NONE', *, *, #50706, .T. ) ;
#30173 = VERTEX_POINT ( 'NONE', #18091 ) ;
#30174 = CARTESIAN_POINT ( 'NONE',  ( -93.67500000000003979, 92.29496732002878900, 75.18333333333332291 ) ) ;
#30175 = DIRECTION ( 'NONE',  ( -0.000000000000000000, 0.1045284632676570929, -0.9945218953682730678 ) ) ;
#30176 = VECTOR ( 'NONE', #53649, 1000.000000000000114 ) ;
#30177 = CARTESIAN_POINT ( 'NONE',  ( -95.00000000000002842, 87.33691857156074434, 89.16656250086712987 ) ) ;
#30178 = CARTESIAN_POINT ( 'NONE',  ( 3.429551818649054340, -146.3199197248623875, 5.500000000000000000 ) ) ;
#30179 = DIRECTION ( 'NONE',  ( 0.000000000000000000, 0.000000000000000000, 1.000000000000000000 ) ) ;
#30180 =( REPRESENTATION_RELATIONSHIP ('NONE','NONE', #31117, #51769 ) REPRESENTATION_RELATIONSHIP_WITH_TRANSFORMATION ( #19968 )SHAPE_REPRESENTATION_RELATIONSHIP( ) );
#30181 = CARTESIAN_POINT ( 'NONE',  ( 2.184357737007946383E-12, -120.0000000000000000, -48.99999999999997158 ) ) ;
#30182 = DIRECTION ( 'NONE',  ( -1.000000000000000000, 0.000000000000000000, -0.000000000000000000 ) ) ;
#30183 = EDGE_LOOP ( 'NONE', ( #47327, #24428, #25344, #40688 ) ) ;
#30184 = CYLINDRICAL_SURFACE ( 'NONE', #64462, 32.00000000000000000 ) ;
#30185 = AXIS2_PLACEMENT_3D ( 'NONE', #53566, #70846, #65231 ) ;
#30186 = CARTESIAN_POINT ( 'NONE',  ( -17.50000000000000355, 0.000000000000000000, 20.00000000000000000 ) ) ;
#30187 = VECTOR ( 'NONE', #23592, 999.9999999999998863 ) ;
#30188 = LINE ( 'NONE', #19278, #28656 ) ;
#30189 = LINE ( 'NONE', #1307, #26100 ) ;
#30190 = CARTESIAN_POINT ( 'NONE',  ( -92.35000000002592913, -210.0000117261698165, 82.77687459617060028 ) ) ;
#30191 = CARTESIAN_POINT ( 'NONE',  ( -96.15314808468745866, -211.9973110713294489, 86.09739583420049769 ) ) ;
#30192 = CIRCLE ( 'NONE', #49409, 77.49899999999999523 ) ;
#30193 = CARTESIAN_POINT ( 'NONE',  ( 0.000000000000000000, -79.10210256391383155, 21.60688246758558506 ) ) ;
#30194 = EDGE_CURVE ( 'NONE', #40539, #40791, #17827, .T. ) ;
#30195 = CIRCLE ( 'NONE', #32552, 77.49899999999999523 ) ;
#30196 = CYLINDRICAL_SURFACE ( 'NONE', #15385, 77.49899999999999523 ) ;
#30197 = PRODUCT_DEFINITION ( 'UNKNOWN', '', #18402, #31014 ) ;
#30198 = EDGE_CURVE ( 'NONE', #49339, #57981, #12437, .T. ) ;
#30199 = CARTESIAN_POINT ( 'NONE',  ( -92.69370383062498320, -211.3315407142195852, 75.46114583420049371 ) ) ;
#30200 = CARTESIAN_POINT ( 'NONE',  ( 92.35000000000000853, -209.9999999999999716, 90.00000000000000000 ) ) ;
#30201 = ORIENTED_EDGE ( 'NONE', *, *, #39848, .F. ) ;
#30202 = CARTESIAN_POINT ( 'NONE',  ( 11.99999999999999822, -46.54456581323762521, -59.03342792756313884 ) ) ;
#30203 = CARTESIAN_POINT ( 'NONE',  ( 5.000000000000002665, -2.543863470247813119, -81.96053171279905314 ) ) ;
#30204 = CARTESIAN_POINT ( 'NONE',  ( 97.65000000000000568, 91.52997821335252127, 85.36979166840096411 ) ) ;
#30205 = EDGE_CURVE ( 'NONE', #18161, #63726, #33433, .T. ) ;
#30206 = DIRECTION ( 'NONE',  ( 0.000000000000000000, 0.000000000000000000, -1.000000000000000000 ) ) ;
#30207 = CARTESIAN_POINT ( 'NONE',  ( 96.15314808468750130, -211.9973110713294489, 77.78947916753381264 ) ) ;
#30208 = VERTEX_POINT ( 'NONE', #46658 ) ;
#30209 = ADVANCED_FACE ( 'NONE', ( #41032 ), #29716, .F. ) ;
#30210 = CYLINDRICAL_SURFACE ( 'NONE', #41995, 2.649999999999985700 ) ;
#30211 = DIRECTION ( 'NONE',  ( 0.000000000000000000, 0.000000000000000000, 1.000000000000000000 ) ) ;
#30212 = ORIENTED_EDGE ( 'NONE', *, *, #48864, .T. ) ;
#30213 = EDGE_CURVE ( 'NONE', #27925, #16429, #18447, .T. ) ;
#30214 = DIRECTION ( 'NONE',  ( -1.000000000000000000, -0.000000000000000000, -0.000000000000000000 ) ) ;
#30215 = ORIENTED_EDGE ( 'NONE', *, *, #69316, .F. ) ;
#30216 = CIRCLE ( 'NONE', #30271, 4.700000000000000178 ) ;
#30217 = DIRECTION ( 'NONE',  ( -1.000000000000000000, 0.000000000000000000, 0.000000000000000000 ) ) ;
#30218 = AXIS2_PLACEMENT_3D ( 'NONE', #46650, #35724, #18084 ) ;
#30219 = VERTEX_POINT ( 'NONE', #58679 ) ;
#30220 = VERTEX_POINT ( 'NONE', #71788 ) ;
#30221 = ORIENTED_EDGE ( 'NONE', *, *, #50475, .T. ) ;
#30222 = CARTESIAN_POINT ( 'NONE',  ( -97.64999999999997726, -211.5299782133524502, 77.35291666666665833 ) ) ;
#30223 = EDGE_CURVE ( 'NONE', #26184, #35072, #13547, .T. ) ;
#30224 = AXIS2_PLACEMENT_3D ( 'NONE', #70101, #57359, #52833 ) ;
#30225 = EDGE_CURVE ( 'NONE', #28278, #59392, #32478, .T. ) ;
#30226 = VERTEX_POINT ( 'NONE', #54520 ) ;
#30227 = AXIS2_PLACEMENT_3D ( 'NONE', #58441, #30241, #12582 ) ;
#30228 = ORIENTED_EDGE ( 'NONE', *, *, #57746, .F. ) ;
#30229 = CARTESIAN_POINT ( 'NONE',  ( 97.30629616937498838, 90.00000000000002842, 78.68906250086715204 ) ) ;
#30230 = DIRECTION ( 'NONE',  ( 0.000000000000000000, -0.8660254037844432595, -0.4999999999999919509 ) ) ;
#30231 = CARTESIAN_POINT ( 'NONE',  ( 92.35000000000002274, -211.5299782133524502, 76.08291666666666231 ) ) ;
#30232 = VERTEX_POINT ( 'NONE', #64692 ) ;
#30233 = ORIENTED_EDGE ( 'NONE', *, *, #33338, .F. ) ;
#30234 = ORIENTED_EDGE ( 'NONE', *, *, #49729, .T. ) ;
#30235 = CARTESIAN_POINT ( 'NONE',  ( 0.000000000000000000, 0.000000000000000000, 0.000000000000000000 ) ) ;
#30236 = VERTEX_POINT ( 'NONE', #60541 ) ;
#30237 = VECTOR ( 'NONE', #8530, 1000.000000000000000 ) ;
#30238 = DIRECTION ( 'NONE',  ( 0.000000000000000000, 0.000000000000000000, -1.000000000000000000 ) ) ;
#30239 = DIRECTION ( 'NONE',  ( 0.000000000000000000, -0.4539904997395350361, -0.8910065241883738940 ) ) ;
#30240 = CARTESIAN_POINT ( 'NONE',  ( -94.94576887096278028, 92.38875495131968307, 74.83591575723764322 ) ) ;
#30241 = DIRECTION ( 'NONE',  ( -1.000000000000000000, 0.000000000000000000, -0.000000000000000000 ) ) ;
#30242 = CIRCLE ( 'NONE', #60272, 42.00000000000000000 ) ;
#30243 = CARTESIAN_POINT ( 'NONE',  ( -12.83284365640956182, 0.000000000000000000, 0.000000000000000000 ) ) ;
#30244 = DIRECTION ( 'NONE',  ( -1.000000000000000000, 0.000000000000000000, 0.000000000000000000 ) ) ;
#30245 = DIRECTION ( 'NONE',  ( -1.000000000000000000, 0.000000000000000000, -0.000000000000000000 ) ) ;
#30246 = CARTESIAN_POINT ( 'NONE',  ( -94.99999999999997158, -213.0599564267049857, 79.44312500173428759 ) ) ;
#30247 = DIRECTION ( 'NONE',  ( 0.000000000000000000, 0.000000000000000000, 1.000000000000000000 ) ) ;
#30248 = ORIENTED_EDGE ( 'NONE', *, *, #14004, .F. ) ;
#30250 = CARTESIAN_POINT ( 'NONE',  ( -92.35000000000005116, 88.47002178664754979, 77.00895833506763211 ) ) ;
#30249 = CARTESIAN_POINT ( 'NONE',  ( 97.64999999999997726, 88.47002178664753558, 75.73895833506765030 ) ) ;
#30251 = EDGE_LOOP ( 'NONE', ( #39034, #63181, #55492, #8971 ) ) ;
#30252 = CARTESIAN_POINT ( 'NONE',  ( 93.84685191531248449, 91.99731107132950569, 80.80572916753382628 ) ) ;
#30253 = DIRECTION ( 'NONE',  ( -1.000000000000000000, 0.000000000000000000, -0.000000000000000000 ) ) ;
#30254 = CARTESIAN_POINT ( 'NONE',  ( 10.00000000000000000, -26.08949754953005495, -27.05870788708258701 ) ) ;
#30255 = CARTESIAN_POINT ( 'NONE',  ( -7.500000000000016875, -80.00000000000001421, -269.9999999999999432 ) ) ;
#30256 = DIRECTION ( 'NONE',  ( 0.000000000000000000, 0.000000000000000000, -1.000000000000000000 ) ) ;
#30257 = CARTESIAN_POINT ( 'NONE',  ( 11.99999999999999822, 0.000000000000000000, 0.000000000000000000 ) ) ;
#30258 = ORIENTED_EDGE ( 'NONE', *, *, #18482, .T. ) ;
#30259 = CARTESIAN_POINT ( 'NONE',  ( 0.000000000000000000, 68.67312586194995561, 35.91791733033500122 ) ) ;
#30260 = LINE ( 'NONE', #36275, #64819 ) ;
#30261 = VERTEX_POINT ( 'NONE', #42876 ) ;
#30262 = ORIENTED_EDGE ( 'NONE', *, *, #66489, .F. ) ;
#30263 = PRODUCT_DEFINITION_SHAPE ( 'NONE', 'NONE',  #74365 ) ;
#30264 = DIRECTION ( 'NONE',  ( 0.000000000000000000, 0.000000000000000000, 1.000000000000000000 ) ) ;
#30265 = FACE_OUTER_BOUND ( 'NONE', #18216, .T. ) ;
#30266 = DIRECTION ( 'NONE',  ( -1.000000000000000000, -0.000000000000000000, -0.000000000000000000 ) ) ;
#30267 = DIRECTION ( 'NONE',  ( -1.000000000000000000, 0.000000000000000000, 0.000000000000000000 ) ) ;
#30268 = CARTESIAN_POINT ( 'NONE',  ( -96.15314808468745866, -211.9973110713294489, 77.20739583420048291 ) ) ;
#30269 = ORIENTED_EDGE ( 'NONE', *, *, #60375, .T. ) ;
#30270 = EDGE_CURVE ( 'NONE', #8861, #58897, #7095, .T. ) ;
#30271 = AXIS2_PLACEMENT_3D ( 'NONE', #57185, #17325, #63205 ) ;
#30272 = CARTESIAN_POINT ( 'NONE',  ( 0.000000000000000000, 0.000000000000000000, 40.80000000000001847 ) ) ;
#30273 = CARTESIAN_POINT ( 'NONE',  ( -11.70000000000000107, 0.000000000000000000, 0.000000000000000000 ) ) ;
#30274 = CIRCLE ( 'NONE', #20672, 42.00000000000000000 ) ;
#30275 = DIRECTION ( 'NONE',  ( -0.000000000000000000, -0.6691306063588569053, -0.7431448254773954654 ) ) ;
#30276 = CYLINDRICAL_SURFACE ( 'NONE', #72819, 77.49899999999999523 ) ;
#30277 = CARTESIAN_POINT ( 'NONE',  ( 12.49999999999999645, 1.530808498934191127E-15, 40.80000000000001847 ) ) ;
#30278 = CARTESIAN_POINT ( 'NONE',  ( 10.00000000000000000, -37.22597642581153821, -5.202137450156795850 ) ) ;
#30279 = EDGE_CURVE ( 'NONE', #32156, #16833, #14289, .T. ) ;
#30280 = DIRECTION ( 'NONE',  ( 1.000000000000000000, -0.000000000000000000, -0.000000000000000000 ) ) ;
#30281 = DIRECTION ( 'NONE',  ( -0.9730327541852491491, 0.2306669878475648139, 0.000000000000000000 ) ) ;
#30282 = EDGE_CURVE ( 'NONE', #16487, #24954, #58725, .T. ) ;
#30283 = CYLINDRICAL_SURFACE ( 'NONE', #35850, 16.00000000000000000 ) ;
#30284 = CIRCLE ( 'NONE', #7475, 31.99999999999998579 ) ;
#30285 = CARTESIAN_POINT ( 'NONE',  ( 92.69370383062498320, 88.66845928578035796, 83.50447916753383026 ) ) ;
#30286 = EDGE_CURVE ( 'NONE', #17504, #56961, #30460, .T. ) ;
#30287 = CARTESIAN_POINT ( 'NONE',  ( -93.84685191531248449, -208.0026889286704943, 85.77989583420048803 ) ) ;
#30288 = DIRECTION ( 'NONE',  ( 0.000000000000000000, 0.3090169943749482839, -0.9510565162951533091 ) ) ;
#30289 = ORIENTED_EDGE ( 'NONE', *, *, #67484, .T. ) ;
#30290 = CARTESIAN_POINT ( 'NONE',  ( 11.99999999999999822, 0.000000000000000000, 0.000000000000000000 ) ) ;
#30291 = CARTESIAN_POINT ( 'NONE',  ( -93.67499999999998295, -207.7050326799711968, 80.89833333333332632 ) ) ;
#30292 = CARTESIAN_POINT ( 'NONE',  ( -92.69370383062504004, 90.00000000000004263, 77.26031250086714408 ) ) ;
#30293 = CIRCLE ( 'NONE', #47112, 82.00000000000000000 ) ;
#30294 = AXIS2_PLACEMENT_3D ( 'NONE', #37004, #8441, #54664 ) ;
#30295 = CARTESIAN_POINT ( 'NONE',  ( 95.00000000000000000, -212.6630814284392557, 87.26156250086714294 ) ) ;
#30296 = ORIENTED_EDGE ( 'NONE', *, *, #70697, .T. ) ;
#30297 = ORIENTED_EDGE ( 'NONE', *, *, #19247, .T. ) ;
#30298 = EDGE_CURVE ( 'NONE', #65590, #18520, #53042, .T. ) ;
#30299 = ORIENTED_EDGE ( 'NONE', *, *, #17433, .T. ) ;
#30300 = CARTESIAN_POINT ( 'NONE',  ( 97.65000000000009095, -211.5299782133523649, 75.65958333333333030 ) ) ;
#30301 = DIRECTION ( 'NONE',  ( -1.000000000000000000, 0.000000000000000000, 0.000000000000000000 ) ) ;
#30302 = EDGE_LOOP ( 'NONE', ( #42029, #5097, #1448, #54199 ) ) ;
#30303 = ORIENTED_EDGE ( 'NONE', *, *, #2942, .F. ) ;
#30304 = CARTESIAN_POINT ( 'NONE',  ( 1.560000000000000053, 0.8660254037844389297, -1.500000000000000000 ) ) ;
#30305 = CARTESIAN_POINT ( 'NONE',  ( 93.84685191531249870, -208.0026889286704943, 80.80572916753382628 ) ) ;
#30306 = ADVANCED_FACE ( 'NONE', ( #53771 ), #24467, .T. ) ;
#30307 = CARTESIAN_POINT ( 'NONE',  ( 92.35000000000000853, -209.9999999999999716, 76.03000000000000114 ) ) ;
#30308 = EDGE_CURVE ( 'NONE', #36890, #32411, #51417, .T. ) ;
#30309 = CARTESIAN_POINT ( 'NONE',  ( 90.00000000000000000, 85.00000000000002842, -80.00000000000000000 ) ) ;
#30310 = CARTESIAN_POINT ( 'NONE',  ( 0.000000000000000000, 0.000000000000000000, 0.000000000000000000 ) ) ;
#30311 = CARTESIAN_POINT ( 'NONE',  ( 10.00000000000000000, -18.89407956138203204, -75.16055320797050854 ) ) ;
#30312 = EDGE_CURVE ( 'NONE', #59025, #73511, #48141, .T. ) ;
#30313 = LINE ( 'NONE', #684, #50145 ) ;
#30314 = CARTESIAN_POINT ( 'NONE',  ( 92.35000000000000853, -209.9999999999999716, 86.18999999999999773 ) ) ;
#30315 = VERTEX_POINT ( 'NONE', #66181 ) ;
#30316 = MECHANICAL_DESIGN_GEOMETRIC_PRESENTATION_REPRESENTATION (  '', ( #57968 ), #42355 ) ;
#30317 = ORIENTED_EDGE ( 'NONE', *, *, #53831, .F. ) ;
#30318 = ORIENTED_EDGE ( 'NONE', *, *, #24969, .F. ) ;
#30319 = ORIENTED_EDGE ( 'NONE', *, *, #4589, .T. ) ;
#30320 =( LENGTH_UNIT ( ) NAMED_UNIT ( * ) SI_UNIT ( .MILLI., .METRE. ) );
#30321 = SURFACE_STYLE_FILL_AREA ( #52147 ) ;
#30322 = CARTESIAN_POINT ( 'NONE',  ( -93.84685191531254134, 91.99731107132950569, 87.04989583420048405 ) ) ;
#30323 = DIRECTION ( 'NONE',  ( 0.000000000000000000, 0.000000000000000000, 1.000000000000000000 ) ) ;
#30324 = CARTESIAN_POINT ( 'NONE',  ( 10.00000000000000000, 65.58780272294129077, -36.73666225445822420 ) ) ;
#30325 = CARTESIAN_POINT ( 'NONE',  ( 96.15314808468750130, -211.9973110713294489, 87.31447916753380412 ) ) ;
#30326 = CARTESIAN_POINT ( 'NONE',  ( 97.64999999999997726, 91.52997821335252127, 77.03541666666666288 ) ) ;
#30327 = ORIENTED_EDGE ( 'NONE', *, *, #73518, .T. ) ;
#30328 = CARTESIAN_POINT ( 'NONE',  ( -2.499999999999970690, 73.00000000000001421, -208.2999999999999261 ) ) ;
#30329 = AXIS2_PLACEMENT_3D ( 'NONE', #19636, #59507, #47843 ) ;
#30330 = ORIENTED_EDGE ( 'NONE', *, *, #58886, .T. ) ;
#30331 = CARTESIAN_POINT ( 'NONE',  ( 97.64999999999999147, -209.9999999999999716, 80.15749999999999886 ) ) ;
#30332 = ORIENTED_EDGE ( 'NONE', *, *, #53392, .F. ) ;
#30333 = CARTESIAN_POINT ( 'NONE',  ( -95.00000000000002842, 86.94004357329504273, 87.06312500173430635 ) ) ;
#30334 = CIRCLE ( 'NONE', #49539, 31.99999999999999289 ) ;
#30335 =( BOUNDED_CURVE ( )  B_SPLINE_CURVE ( 2, ( #31318, #20033, #34842, #69783, #35202, #29182, #71532 ),
 .UNSPECIFIED., .F., .F. ) 
 B_SPLINE_CURVE_WITH_KNOTS ( ( 3, 2, 2, 3 ),
 ( 0.1666666666666666852, 0.1736111111111111049, 0.1805555555555554970, 0.1874999999999999167 ),
 .UNSPECIFIED. ) 
 CURVE ( )  GEOMETRIC_REPRESENTATION_ITEM ( )  RATIONAL_B_SPLINE_CURVE ( ( 0.9999999999999994449, 0.8660254037844392627, 1.000000000000000000, 0.8660254037844387076, 1.000000000000000000, 0.8660254037844402619, 0.9999999999999984457 ) ) 
 REPRESENTATION_ITEM ( '' )  );
#30336 = CARTESIAN_POINT ( 'NONE',  ( 92.69370383062498320, 88.66845928578037217, 75.72572916753381378 ) ) ;
#30337 = ORIENTED_EDGE ( 'NONE', *, *, #50859, .F. ) ;
#30338 = DIRECTION ( 'NONE',  ( 0.000000000000000000, 0.000000000000000000, -1.000000000000000000 ) ) ;
#30339 = DIRECTION ( 'NONE',  ( -1.000000000000000000, 0.000000000000000000, 0.000000000000000000 ) ) ;
#30340 = CARTESIAN_POINT ( 'NONE',  ( 0.000000000000000000, -13.04903810567675038, 19.60159698893425428 ) ) ;
#30341 = ORIENTED_EDGE ( 'NONE', *, *, #1137, .T. ) ;
#30342 = DIRECTION ( 'NONE',  ( 0.000000000000000000, -0.2079116908177664758, -0.9781476007338042455 ) ) ;
#30343 = CIRCLE ( 'NONE', #26742, 31.99999999999999289 ) ;
#30344 = CIRCLE ( 'NONE', #72367, 32.00000000000000000 ) ;
#30345 = DIRECTION ( 'NONE',  ( -1.000000000000000000, -0.000000000000000000, -0.000000000000000000 ) ) ;
#30346 = ORIENTED_EDGE ( 'NONE', *, *, #3147, .F. ) ;
#30347 = EDGE_LOOP ( 'NONE', ( #62717, #8106, #33179, #58640 ) ) ;
#30348 = CARTESIAN_POINT ( 'NONE',  ( 97.64999999999999147, -209.9999999999999716, 87.14249999999999829 ) ) ;
#30349 = CARTESIAN_POINT ( 'NONE',  ( 11.99999999999999822, 26.01480285779933510, -70.53064760720289428 ) ) ;
#30350 = DIRECTION ( 'NONE',  ( -1.000000000000000000, 0.000000000000000000, 0.000000000000000000 ) ) ;
#30351 = CARTESIAN_POINT ( 'NONE',  ( -96.15314808468747287, -208.0026889286704943, 88.42572916753381662 ) ) ;
#30352 = ORIENTED_EDGE ( 'NONE', *, *, #65289, .T. ) ;
#30353 = FACE_OUTER_BOUND ( 'NONE', #58114, .T. ) ;
#30354 = ORIENTED_EDGE ( 'NONE', *, *, #66190, .F. ) ;
#30355 = ADVANCED_FACE ( 'NONE', ( #42501 ), #25573, .T. ) ;
#30356 = ORIENTED_EDGE ( 'NONE', *, *, #33801, .T. ) ;
#30357 = CARTESIAN_POINT ( 'NONE',  ( -0.0004442498507136653329, 0.001194404164628348752, -70.59999999999999432 ) ) ;
#30358 = CARTESIAN_POINT ( 'NONE',  ( 0.000000000000000000, 0.000000000000000000, 0.000000000000000000 ) ) ;
#30359 = CARTESIAN_POINT ( 'NONE',  ( -10.00000000000000000, 0.000000000000000000, 0.000000000000000000 ) ) ;
#30360 = CARTESIAN_POINT ( 'NONE',  ( 97.30629616937498838, 91.33154071421968467, 80.48822916753380241 ) ) ;
#30361 = CARTESIAN_POINT ( 'NONE',  ( 11.99999999999999822, 0.000000000000000000, 0.000000000000000000 ) ) ;
#30362 = DIRECTION ( 'NONE',  ( 0.000000000000000000, 0.000000000000000000, -1.000000000000000000 ) ) ;
#30363 = EDGE_CURVE ( 'NONE', #52399, #71078, #47758, .T. ) ;
#30364 = DIRECTION ( 'NONE',  ( -1.000000000000000000, 0.000000000000000000, -0.000000000000000000 ) ) ;
#30365 = CARTESIAN_POINT ( 'NONE',  ( 0.000000000000000000, -23.29833615347104825, -3.418703333116803744 ) ) ;
#30366 = DIRECTION ( 'NONE',  ( 1.000000000000000000, -1.047380211910311281E-14, -2.618450529775778123E-14 ) ) ;
#30367 = ADVANCED_FACE ( 'NONE', ( #36850 ), #31574, .T. ) ;
#30368 = CARTESIAN_POINT ( 'NONE',  ( 0.000000000000000000, -66.50666863322028632, 39.78640506895582973 ) ) ;
#30369 = LINE ( 'NONE', #1851, #31498 ) ;
#30370 = CARTESIAN_POINT ( 'NONE',  ( 12.00000000000000000, -14.54903810567644484, 22.19967320028775504 ) ) ;
#30371 = EDGE_CURVE ( 'NONE', #56493, #60043, #33488, .T. ) ;
#30372 = DIRECTION ( 'NONE',  ( -1.000000000000000000, -0.000000000000000000, -0.000000000000000000 ) ) ;
#30373 = CARTESIAN_POINT ( 'NONE',  ( -97.30629616937501680, 88.66845928578038638, 85.88572916753381037 ) ) ;
#30374 = DIRECTION ( 'NONE',  ( -1.000000000000000000, 0.000000000000000000, -0.000000000000000000 ) ) ;
#30375 = AXIS2_PLACEMENT_3D ( 'NONE', #29832, #59170, #52789 ) ;
#30376 = CARTESIAN_POINT ( 'NONE',  ( -3.000000000000000000, 26.50000000000000355, 1.500000000000000000 ) ) ;
#30377 = EDGE_CURVE ( 'NONE', #55006, #23530, #54158, .T. ) ;
#30378 = EDGE_LOOP ( 'NONE', ( #13244, #14520, #45635, #59823 ) ) ;
#30379 = AXIS2_PLACEMENT_3D ( 'NONE', #74238, #50940, #50565 ) ;
#30380 = DIRECTION ( 'NONE',  ( -0.000000000000000000, 0.9135454576426060846, 0.4067366430757888285 ) ) ;
#30382 = CARTESIAN_POINT ( 'NONE',  ( 0.000000000000000000, 0.000000000000000000, 0.000000000000000000 ) ) ;
#30381 = VECTOR ( 'NONE', #6537, 1000.000000000000000 ) ;
#30383 = EDGE_CURVE ( 'NONE', #63593, #5952, #55994, .T. ) ;
#30384 = CARTESIAN_POINT ( 'NONE',  ( 10.00000000000000000, 27.05870788708267582, -26.08949754952995903 ) ) ;
#30385 = LINE ( 'NONE', #51853, #5574 ) ;
#30386 = VECTOR ( 'NONE', #19089, 1000.000000000000000 ) ;
#30387 = CARTESIAN_POINT ( 'NONE',  ( 95.00000000000000000, -212.6630814284392557, 83.61031250086716682 ) ) ;
#30388 = ORIENTED_EDGE ( 'NONE', *, *, #11475, .F. ) ;
#30389 = EDGE_LOOP ( 'NONE', ( #48366, #50126, #5135, #45358 ) ) ;
#30390 = EDGE_CURVE ( 'NONE', #63033, #7419, #71909, .T. ) ;
#30391 = PRESENTATION_STYLE_ASSIGNMENT (( #24039 ) ) ;
#30392 = VERTEX_POINT ( 'NONE', #15394 ) ;
#30393 = EDGE_CURVE ( 'NONE', #47808, #24268, #49114, .T. ) ;
#30394 = CARTESIAN_POINT ( 'NONE',  ( 97.64999999999999147, -209.9999999999999716, 88.41249999999999432 ) ) ;
#30395 = LINE ( 'NONE', #64262, #37588 ) ;
#30396 = ORIENTED_EDGE ( 'NONE', *, *, #67291, .F. ) ;
#30397 = CARTESIAN_POINT ( 'NONE',  ( 97.30629616937498838, -208.6684592857803011, 81.28197916753381946 ) ) ;
#30398 = ORIENTED_EDGE ( 'NONE', *, *, #13388, .T. ) ;
#30399 = DIRECTION ( 'NONE',  ( 0.6862798483830533369, 0.7273375899149812085, -0.000000000000000000 ) ) ;
#30400 = ORIENTED_EDGE ( 'NONE', *, *, #31884, .F. ) ;
#30401 = ORIENTED_EDGE ( 'NONE', *, *, #56433, .T. ) ;
#30402 = DIRECTION ( 'NONE',  ( -2.603472992745699578E-14, 2.546204323184531851E-14, -1.000000000000000000 ) ) ;
#30403 = DIRECTION ( 'NONE',  ( -1.000000000000000000, 0.000000000000000000, 0.000000000000000000 ) ) ;
#30404 = ORIENTED_EDGE ( 'NONE', *, *, #66780, .F. ) ;
#30405 = FACE_OUTER_BOUND ( 'NONE', #63386, .T. ) ;
#30406 = CARTESIAN_POINT ( 'NONE',  ( 92.35000000000002274, -211.5299782133524502, 81.87729166840097150 ) ) ;
#30407 = CARTESIAN_POINT ( 'NONE',  ( 93.67499999999998295, 92.29496732002878900, 87.98916666666666231 ) ) ;
#30408 = ORIENTED_EDGE ( 'NONE', *, *, #70232, .T. ) ;
#30409 = CYLINDRICAL_SURFACE ( 'NONE', #52678, 32.00000000000000000 ) ;
#30410 = CARTESIAN_POINT ( 'NONE',  ( 6.000000000000001776, 5.000000000000000000, 0.000000000000000000 ) ) ;
#30411 = AXIS2_PLACEMENT_3D ( 'NONE', #54057, #58962, #20195 ) ;
#30412 = ORIENTED_EDGE ( 'NONE', *, *, #24841, .T. ) ;
#30413 = VERTEX_POINT ( 'NONE', #54882 ) ;
#30414 = CARTESIAN_POINT ( 'NONE',  ( -96.15314808468752972, 91.99731107132950569, 86.52072916753382970 ) ) ;
#30415 = CARTESIAN_POINT ( 'NONE',  ( 93.84685191531248449, 88.00268892867053694, 86.57364583420047666 ) ) ;
#30416 = VERTEX_POINT ( 'NONE', #39461 ) ;
#30417 = CARTESIAN_POINT ( 'NONE',  ( 97.64999999999997726, 91.52997821335252127, 86.63979166840097434 ) ) ;
#30418 = DIRECTION ( 'NONE',  ( 0.000000000000000000, -0.8090169943749403458, -0.5877852522924830181 ) ) ;
#30419 = SHAPE_REPRESENTATION_RELATIONSHIP ( 'NONE' , 'NONE' ,  #30982, #65097 ) ;
#30420 = VERTEX_POINT ( 'NONE', #27797 ) ;
#30421 = CARTESIAN_POINT ( 'NONE',  ( 0.000000000000000000, -120.0000000000000000, -2.500000000000000000 ) ) ;
#30422 = ORIENTED_EDGE ( 'NONE', *, *, #21445, .F. ) ;
#30423 = AXIS2_PLACEMENT_3D ( 'NONE', #36323, #49086, #7762 ) ;
#30424 = ORIENTED_EDGE ( 'NONE', *, *, #4365, .F. ) ;
#30425 = VERTEX_POINT ( 'NONE', #33423 ) ;
#30426 = DIRECTION ( 'NONE',  ( 0.000000000000000000, 1.445602896647339410E-16, -1.000000000000000000 ) ) ;
#30427 = LINE ( 'NONE', #17684, #27722 ) ;
#30428 = CARTESIAN_POINT ( 'NONE',  ( -92.35000000000003695, 90.00000000000004263, 85.23749999999999716 ) ) ;
#30429 = ORIENTED_EDGE ( 'NONE', *, *, #45595, .F. ) ;
#30430 = CARTESIAN_POINT ( 'NONE',  ( 96.32499999999998863, 87.70503267997126784, 81.95666666666666345 ) ) ;
#30431 = VECTOR ( 'NONE', #17290, 999.9999999999998863 ) ;
#30432 = CARTESIAN_POINT ( 'NONE',  ( 0.000000000000000000, 68.26794271651307611, -31.47745569255064169 ) ) ;
#30433 = EDGE_LOOP ( 'NONE', ( #33081, #8626, #70710, #53712 ) ) ;
#30434 = FACE_OUTER_BOUND ( 'NONE', #14441, .T. ) ;
#30435 = CARTESIAN_POINT ( 'NONE',  ( -92.69370383062498320, -211.3315407142195852, 84.19239583420046813 ) ) ;
#30436 = ORIENTED_EDGE ( 'NONE', *, *, #25029, .T. ) ;
#30437 = DIRECTION ( 'NONE',  ( -1.000000000000000000, 3.061616997868382648E-16, 0.000000000000000000 ) ) ;
#30438 = DIRECTION ( 'NONE',  ( -0.000000000000000000, -0.000000000000000000, 1.000000000000000000 ) ) ;
#30439 = DIRECTION ( 'NONE',  ( 1.000000000000000000, 0.000000000000000000, 0.000000000000000000 ) ) ;
#30440 = LINE ( 'NONE', #8642, #15856 ) ;
#30441 = ADVANCED_FACE ( 'NONE', ( #38337 ), #21783, .T. ) ;
#30442 = CARTESIAN_POINT ( 'NONE',  ( -3.000000000000000000, 5.835314593368772229, -22.81335362449846826 ) ) ;
#30443 = AXIS2_PLACEMENT_3D ( 'NONE', #21293, #4796, #28057 ) ;
#30444 = AXIS2_PLACEMENT_3D ( 'NONE', #18993, #35554, #29906 ) ;
#30445 = ADVANCED_FACE ( 'NONE', ( #49240 ), #72890, .F. ) ;
#30446 = FACE_OUTER_BOUND ( 'NONE', #60048, .T. ) ;
#30447 = LINE ( 'NONE', #14271, #8459 ) ;
#30448 = DIRECTION ( 'NONE',  ( -2.603472992746261562E-14, -2.546204323184492723E-14, 1.000000000000000000 ) ) ;
#30449 = EDGE_CURVE ( 'NONE', #1351, #41590, #16709, .T. ) ;
#30450 = LINE ( 'NONE', #2676, #13494 ) ;
#30451 = CARTESIAN_POINT ( 'NONE',  ( 10.00000000000000000, 0.000000000000000000, 0.000000000000000000 ) ) ;
#30452 = CARTESIAN_POINT ( 'NONE',  ( -95.00000000000002842, 87.33691857156074434, 76.46656250086712703 ) ) ;
#30453 = CARTESIAN_POINT ( 'NONE',  ( 94.99999999999998579, 90.00000000000002842, 90.00000000000000000 ) ) ;
#30454 = PLANE ( 'NONE',  #23052 ) ;
#30455 = CARTESIAN_POINT ( 'NONE',  ( 0.000000000000000000, 35.95386929396241271, 10.96151621346552751 ) ) ;
#30456 = CIRCLE ( 'NONE', #49668, 13.90444123027096879 ) ;
#30457 = EDGE_CURVE ( 'NONE', #14882, #53902, #43126, .T. ) ;
#30458 = LINE ( 'NONE', #8659, #58106 ) ;
#30459 = DIRECTION ( 'NONE',  ( -1.000000000000000000, -0.000000000000000000, -0.000000000000000000 ) ) ;
#30460 = LINE ( 'NONE', #25937, #28658 ) ;
#30461 = DIRECTION ( 'NONE',  ( 0.000000000000000000, 0.4067366430757888285, 0.9135454576426060846 ) ) ;
#30462 = DIRECTION ( 'NONE',  ( 0.000000000000000000, 1.000000000000000000, 3.469446951953616555E-15 ) ) ;
#30463 = CARTESIAN_POINT ( 'NONE',  ( -94.99999999999997158, -207.3369185715606307, 77.57781250086715374 ) ) ;
#30464 = FACE_OUTER_BOUND ( 'NONE', #32517, .T. ) ;
#30465 = CIRCLE ( 'NONE', #72487, 16.00000000000000000 ) ;
#30466 = EDGE_CURVE ( 'NONE', #47594, #54289, #8277, .T. ) ;
#30467 = ORIENTED_EDGE ( 'NONE', *, *, #40948, .F. ) ;
#30468 = DIRECTION ( 'NONE',  ( -1.000000000000000000, -0.000000000000000000, -0.000000000000000000 ) ) ;
#30469 = EDGE_CURVE ( 'NONE', #67440, #64530, #21396, .T. ) ;
#30470 = CARTESIAN_POINT ( 'NONE',  ( 96.32499999999998863, -212.2949673200287179, 88.30666666666665776 ) ) ;
#30471 =( NAMED_UNIT ( * ) PLANE_ANGLE_UNIT ( ) SI_UNIT ( $, .RADIAN. ) );
#30472 = DIRECTION ( 'NONE',  ( -0.6575728627325957421, 0.7533909544171994987, 0.000000000000000000 ) ) ;
#30473 = EDGE_CURVE ( 'NONE', #27844, #30208, #26302, .T. ) ;
#30474 = EDGE_CURVE ( 'NONE', #31369, #19022, #73280, .T. ) ;
#30475 = AXIS2_PLACEMENT_3D ( 'NONE', #62439, #27447, #57160 ) ;
#30476 = CYLINDRICAL_SURFACE ( 'NONE', #1948, 82.00000000000000000 ) ;
#30477 = ORIENTED_EDGE ( 'NONE', *, *, #58305, .F. ) ;
#30478 = LINE ( 'NONE', #18827, #39541 ) ;
#30479 = ADVANCED_FACE ( 'NONE', ( #73649 ), #44354, .T. ) ;
#30480 = PLANE ( 'NONE',  #19935 ) ;
#30481 = ORIENTED_EDGE ( 'NONE', *, *, #28627, .F. ) ;
#30482 = AXIS2_PLACEMENT_3D ( 'NONE', #68348, #16089, #62726 ) ;
#30483 = CARTESIAN_POINT ( 'NONE',  ( 97.30629616937498838, -208.6684592857803295, 84.93322916753379559 ) ) ;
#30484 = CARTESIAN_POINT ( 'NONE',  ( 92.69370383062501162, -211.3315407142195852, 87.94947916753382344 ) ) ;
#30485 = AXIS2_PLACEMENT_3D ( 'NONE', #12541, #29449, #46772 ) ;
#30486 = ORIENTED_EDGE ( 'NONE', *, *, #33606, .F. ) ;
#30487 = CARTESIAN_POINT ( 'NONE',  ( -96.32500000000001705, 92.29496732002878900, 79.73416666666666686 ) ) ;
#30488 = ADVANCED_FACE ( 'NONE', ( #66546 ), #62021, .T. ) ;
#30489 = VERTEX_POINT ( 'NONE', #43983 ) ;
#30490 = VECTOR ( 'NONE', #41479, 1000.000000000000000 ) ;
#30491 = PLANE ( 'NONE',  #38246 ) ;
#30492 = ORIENTED_EDGE ( 'NONE', *, *, #40779, .F. ) ;
#30493 = CARTESIAN_POINT ( 'NONE',  ( -92.69370383062502583, 88.66845928578038638, 79.27114583420048177 ) ) ;
#30494 = ORIENTED_EDGE ( 'NONE', *, *, #23694, .F. ) ;
#30495 = EDGE_LOOP ( 'NONE', ( #22561, #33556 ) ) ;
#30496 = DIRECTION ( 'NONE',  ( -0.000000000000000000, -0.000000000000000000, -1.000000000000000000 ) ) ;
#30497 = ORIENTED_EDGE ( 'NONE', *, *, #35735, .F. ) ;
#30498 = LINE ( 'NONE', #24148, #22126 ) ;
#30499 = DIRECTION ( 'NONE',  ( -1.000000000000000000, -0.000000000000000000, -0.000000000000000000 ) ) ;
#30500 = ORIENTED_EDGE ( 'NONE', *, *, #38217, .T. ) ;
#30501 = CARTESIAN_POINT ( 'NONE',  ( 10.00000000000000000, -6.736453364083292428, -36.88895765772640800 ) ) ;
#30502 = EDGE_LOOP ( 'NONE', ( #45891, #26697, #62164, #2995 ) ) ;
#30503 = CARTESIAN_POINT ( 'NONE',  ( 0.000000000000000000, -51.03279382321048985, -55.19960302592120627 ) ) ;
#30504 = ORIENTED_EDGE ( 'NONE', *, *, #64446, .T. ) ;
#30505 = CIRCLE ( 'NONE', #24567, 31.99999999999999289 ) ;
#30506 = ORIENTED_EDGE ( 'NONE', *, *, #48959, .T. ) ;
#30507 = ORIENTED_EDGE ( 'NONE', *, *, #65022, .T. ) ;
#30508 = CARTESIAN_POINT ( 'NONE',  ( 97.30629616937498838, -211.3315407142195852, 79.11239583420046984 ) ) ;
#30509 = FACE_OUTER_BOUND ( 'NONE', #65600, .T. ) ;
#30510 = ITEM_DEFINED_TRANSFORMATION ( 'NONE', 'NONE', #13568,  #43395 ) ;
#30511 = CARTESIAN_POINT ( 'NONE',  ( -92.34999999999999432, -211.5299782133524218, 85.89895833506763267 ) ) ;
#30512 = DIRECTION ( 'NONE',  ( -0.8774505977381978905, -0.4796670183876304283, 0.000000000000000000 ) ) ;
#30513 = CYLINDRICAL_SURFACE ( 'NONE', #14955, 31.99999999999998579 ) ;
#30514 = DIRECTION ( 'NONE',  ( 1.000000000000000000, 0.000000000000000000, 0.000000000000000000 ) ) ;
#30515 = DIRECTION ( 'NONE',  ( 0.000000000000000000, 0.000000000000000000, -1.000000000000000000 ) ) ;
#30516 = DIRECTION ( 'NONE',  ( 0.000000000000000000, 0.000000000000000000, 1.000000000000000000 ) ) ;
#30517 = CARTESIAN_POINT ( 'NONE',  ( -96.15314808468745866, -211.9973110713294489, 80.85864583420047325 ) ) ;
#30518 = CARTESIAN_POINT ( 'NONE',  ( -93.84685191531254134, 91.99731107132950569, 82.60489583420049087 ) ) ;
#30519 = ORIENTED_EDGE ( 'NONE', *, *, #53815, .F. ) ;
#30520 = VECTOR ( 'NONE', #59680, 1000.000000000000000 ) ;
#30521 = CARTESIAN_POINT ( 'NONE',  ( 93.84685191531248449, 91.99731107132950569, 79.37697916753380412 ) ) ;
#30522 = ORIENTED_EDGE ( 'NONE', *, *, #63115, .F. ) ;
#30523 = CARTESIAN_POINT ( 'NONE',  ( 12.50000000000000000, -132.5000000000000000, 40.00000000000000000 ) ) ;
#30524 = LINE ( 'NONE', #53472, #11917 ) ;
#30525 = CARTESIAN_POINT ( 'NONE',  ( -92.34999999999999432, -211.5299782133524218, 76.92958333333332632 ) ) ;
#30526 = CYLINDRICAL_SURFACE ( 'NONE', #46333, 31.99999999999999289 ) ;
#30527 = DIRECTION ( 'NONE',  ( 0.000000000000000000, -0.3090169943749560555, -0.9510565162951506446 ) ) ;
#30528 = CARTESIAN_POINT ( 'NONE',  ( -92.69370383062498320, -211.3315407142195852, 82.92239583420045790 ) ) ;
#30529 = EDGE_CURVE ( 'NONE', #31227, #30208, #15024, .T. ) ;
#30530 = LINE ( 'NONE', #66251, #50575 ) ;
#30531 = CARTESIAN_POINT ( 'NONE',  ( 0.7195005275814480017, -121.3161758966073052, 2.500000000000000000 ) ) ;
#30532 = CARTESIAN_POINT ( 'NONE',  ( 92.34999999999999432, 90.00000000000002842, 80.47499999999999432 ) ) ;
#30533 = VERTEX_POINT ( 'NONE', #16516 ) ;
#30534 = CIRCLE ( 'NONE', #11327, 31.99999999999998934 ) ;
#30535 = ADVANCED_FACE ( 'NONE', ( #9385 ), #55256, .T. ) ;
#30536 = ORIENTED_EDGE ( 'NONE', *, *, #10078, .T. ) ;
#30537 = EDGE_CURVE ( 'NONE', #48253, #44200, #55630, .T. ) ;
#30538 = EDGE_CURVE ( 'NONE', #7056, #46924, #57489, .T. ) ;
#30539 = DIRECTION ( 'NONE',  ( 0.000000000000000000, 0.000000000000000000, 1.000000000000000000 ) ) ;
#30540 = CARTESIAN_POINT ( 'NONE',  ( 92.35000000001612364, -210.0000060634596082, 88.17456390440206349 ) ) ;
#30541 = CARTESIAN_POINT ( 'NONE',  ( -96.15314808468752972, 91.99731107132950569, 84.45697916753380241 ) ) ;
#30542 = DIRECTION ( 'NONE',  ( -1.000000000000000000, -0.000000000000000000, -0.000000000000000000 ) ) ;
#30543 = DIRECTION ( 'NONE',  ( 1.000000000000000000, 1.427937372958405461E-15, 7.962523111839130290E-16 ) ) ;
#30544 = CARTESIAN_POINT ( 'NONE',  ( 10.00000000000000000, -5.202137450156655518, 37.22597642581156663 ) ) ;
#30545 = VECTOR ( 'NONE', #52900, 1000.000000000000000 ) ;
#30546 = CARTESIAN_POINT ( 'NONE',  ( 0.000000000000000000, 50.95692526931414790, -58.39081064771693974 ) ) ;
#30547 = AXIS2_PLACEMENT_3D ( 'NONE', #39933, #34271, #23733 ) ;
#30548 = VERTEX_POINT ( 'NONE', #28909 ) ;
#30549 = DIRECTION ( 'NONE',  ( -1.000000000000000000, 0.000000000000000000, 0.000000000000000000 ) ) ;
#30550 = CIRCLE ( 'NONE', #26953, 32.00000000000000000 ) ;
#30551 = AXIS2_PLACEMENT_3D ( 'NONE', #2874, #9952, #50163 ) ;
#30552 = LINE ( 'NONE', #13633, #50153 ) ;
#30553 = LINE ( 'NONE', #6893, #55069 ) ;
#30554 = CARTESIAN_POINT ( 'NONE',  ( 0.000000000000000000, -0.6853352020793173072, 37.58145647212453611 ) ) ;
#30555 = DIRECTION ( 'NONE',  ( -1.000000000000000000, -0.000000000000000000, -0.000000000000000000 ) ) ;
#30556 = CARTESIAN_POINT ( 'NONE',  ( -94.99999999999997158, -212.6630814284392557, 86.15031250086714465 ) ) ;
#30557 = AXIS2_PLACEMENT_3D ( 'NONE', #58672, #53768, #24105 ) ;
#30558 = EDGE_CURVE ( 'NONE', #27167, #27292, #37105, .T. ) ;
#30559 = DIRECTION ( 'NONE',  ( 0.000000000000000000, -0.7431448254773862505, 0.6691306063588672304 ) ) ;
#30560 = CIRCLE ( 'NONE', #69007, 3.300000000000000711 ) ;
#30561 =( BOUNDED_CURVE ( )  B_SPLINE_CURVE ( 2, ( #34767, #64088, #589 ),
 .UNSPECIFIED., .F., .F. ) 
 B_SPLINE_CURVE_WITH_KNOTS ( ( 3, 3 ),
 ( 0.9791666666666669627, 0.9841647806526062636 ),
 .UNSPECIFIED. ) 
 CURVE ( )  GEOMETRIC_REPRESENTATION_ITEM ( )  RATIONAL_B_SPLINE_CURVE ( ( 0.9999999999999935607, 0.9035746763527958691, 0.9459494432169044398 ) ) 
 REPRESENTATION_ITEM ( '' )  );
#30562 = CARTESIAN_POINT ( 'NONE',  ( 92.69370383062498320, 91.33154071421968467, 75.14364583420049826 ) ) ;
#30563 = AXIS2_PLACEMENT_3D ( 'NONE', #71473, #65125, #60231 ) ;
#30564 = CARTESIAN_POINT ( 'NONE',  ( -93.84685191531247028, -211.9973110713294489, 77.94822916753382458 ) ) ;
#30565 = DIRECTION ( 'NONE',  ( 0.9781476007338070211, 2.546183866652750331E-17, 0.2079116908177527367 ) ) ;
#30566 = ORIENTED_EDGE ( 'NONE', *, *, #17647, .T. ) ;
#30567 = CARTESIAN_POINT ( 'NONE',  ( -92.35000000000674447, -209.9999940177768565, 82.14187520865739600 ) ) ;
#30568 = CYLINDRICAL_SURFACE ( 'NONE', #19016, 16.00000000000000000 ) ;
#30569 = CARTESIAN_POINT ( 'NONE',  ( -92.35000000005469190, 89.99998298270445218, 88.49187441316097136 ) ) ;
#30570 = EDGE_CURVE ( 'NONE', #68033, #22414, #40200, .T. ) ;
#30571 = ADVANCED_FACE ( 'NONE', ( #16900 ), #69500, .T. ) ;
#30572 = DIRECTION ( 'NONE',  ( 0.000000000000000000, 0.000000000000000000, 1.000000000000000000 ) ) ;
#30573 = CARTESIAN_POINT ( 'NONE',  ( 96.15314808468750130, -211.9973110713294489, 78.42447916753381776 ) ) ;
#30574 = ORIENTED_EDGE ( 'NONE', *, *, #63190, .T. ) ;
#30575 = DIRECTION ( 'NONE',  ( 1.000000000000000000, 0.000000000000000000, -0.000000000000000000 ) ) ;
#30576 = DIRECTION ( 'NONE',  ( -1.000000000000000000, -0.000000000000000000, 0.000000000000000000 ) ) ;
#30577 = ORIENTED_EDGE ( 'NONE', *, *, #44605, .T. ) ;
#30578 = CYLINDRICAL_SURFACE ( 'NONE', #69973, 82.00000000000000000 ) ;
#30579 = VERTEX_POINT ( 'NONE', #51841 ) ;
#30580 = PLANE ( 'NONE',  #43045 ) ;
#30581 = AXIS2_PLACEMENT_3D ( 'NONE', #49098, #54744, #70915 ) ;
#30582 = ORIENTED_EDGE ( 'NONE', *, *, #27544, .T. ) ;
#30583 = ORIENTED_EDGE ( 'NONE', *, *, #68774, .F. ) ;
#30584 = VERTEX_POINT ( 'NONE', #34543 ) ;
#30585 = LINE ( 'NONE', #26059, #50281 ) ;
#30586 = EDGE_LOOP ( 'NONE', ( #12219, #5229, #29511, #26440 ) ) ;
#30587 = ORIENTED_EDGE ( 'NONE', *, *, #72526, .F. ) ;
#30588 = CARTESIAN_POINT ( 'NONE',  ( 93.84685191531248449, 91.99731107132950569, 80.80572916753382628 ) ) ;
#30589 = CIRCLE ( 'NONE', #66624, 12.50000000000000000 ) ;
#30591 = DIRECTION ( 'NONE',  ( 0.6575728627325956310, -0.7533909544171997208, -1.230411769795008071E-16 ) ) ;
#30590 = AXIS2_PLACEMENT_3D ( 'NONE', #45148, #38390, #4561 ) ;
#30592 = ORIENTED_EDGE ( 'NONE', *, *, #15592, .T. ) ;
#30593 = ORIENTED_EDGE ( 'NONE', *, *, #41731, .T. ) ;
#30594 = EDGE_LOOP ( 'NONE', ( #56641, #36129, #1471, #26055 ) ) ;
#30595 = FACE_OUTER_BOUND ( 'NONE', #56795, .T. ) ;
#30596 = ORIENTED_EDGE ( 'NONE', *, *, #14495, .T. ) ;
#30597 = VECTOR ( 'NONE', #942, 1000.000000000000000 ) ;
#30598 = DIRECTION ( 'NONE',  ( 1.000000000000000000, 0.000000000000000000, 0.000000000000000000 ) ) ;
#30599 = CARTESIAN_POINT ( 'NONE',  ( 10.00000000000000000, 21.60688246758695641, -79.10210256391344785 ) ) ;
#30600 = DIRECTION ( 'NONE',  ( 0.000000000000000000, 0.000000000000000000, 1.000000000000000000 ) ) ;
#30601 = DIRECTION ( 'NONE',  ( -0.000000000000000000, -0.000000000000000000, -1.000000000000000000 ) ) ;
#30602 = CARTESIAN_POINT ( 'NONE',  ( -97.64999999999996305, -209.9999999999999716, 84.36437500173430237 ) ) ;
#30603 = CIRCLE ( 'NONE', #23441, 16.00000000000000355 ) ;
#30604 = DIRECTION ( 'NONE',  ( 0.000000000000000000, -0.9510565162951500895, -0.3090169943749583870 ) ) ;
#30605 = DIRECTION ( 'NONE',  ( -1.000000000000000000, 0.000000000000000000, 0.000000000000000000 ) ) ;
#30606 = CARTESIAN_POINT ( 'NONE',  ( -97.64999999999994884, -208.4700217866474645, 80.50145833506765314 ) ) ;
#30607 = CARTESIAN_POINT ( 'NONE',  ( 97.64999999999999147, -209.9999999999999716, 90.00000000000000000 ) ) ;
#30609 = CARTESIAN_POINT ( 'NONE',  ( -92.35000000000003695, 90.00000000000004263, 74.52187500173430124 ) ) ;
#30608 = CARTESIAN_POINT ( 'NONE',  ( 97.64999999999997726, 88.47002178664753558, 77.00895833506763211 ) ) ;
#30610 = ORIENTED_EDGE ( 'NONE', *, *, #33971, .F. ) ;
#30611 = CARTESIAN_POINT ( 'NONE',  ( 97.30629616937498838, 90.00000000000002842, 78.05406250086716113 ) ) ;
#30612 = DIRECTION ( 'NONE',  ( 0.000000000000000000, -0.9876883405951361050, -0.1564344650402419989 ) ) ;
#30613 = CARTESIAN_POINT ( 'NONE',  ( 15.00000000000000000, -22.67460108101774452, 6.353146135318220367 ) ) ;
#30614 = FACE_OUTER_BOUND ( 'NONE', #31721, .T. ) ;
#30615 = EDGE_CURVE ( 'NONE', #11307, #59498, #386, .T. ) ;
#30616 = FACE_OUTER_BOUND ( 'NONE', #58073, .T. ) ;
#30617 = CYLINDRICAL_SURFACE ( 'NONE', #5435, 16.00000000000000000 ) ;
#30618 = ORIENTED_EDGE ( 'NONE', *, *, #50479, .T. ) ;
#30619 = EDGE_CURVE ( 'NONE', #43631, #38411, #23282, .T. ) ;
#30620 = FACE_OUTER_BOUND ( 'NONE', #34306, .T. ) ;
#30621 = DIRECTION ( 'NONE',  ( -0.000000000000000000, -0.000000000000000000, 1.000000000000000000 ) ) ;
#30622 = ORIENTED_EDGE ( 'NONE', *, *, #51935, .F. ) ;
#30623 = EDGE_CURVE ( 'NONE', #59348, #35612, #29629, .T. ) ;
#30624 = CIRCLE ( 'NONE', #46258, 16.00000000000000355 ) ;
#30625 = ORIENTED_EDGE ( 'NONE', *, *, #24608, .T. ) ;
#30626 = EDGE_CURVE ( 'NONE', #38932, #14488, #64689, .T. ) ;
#30627 = FACE_OUTER_BOUND ( 'NONE', #54530, .T. ) ;
#30628 = CARTESIAN_POINT ( 'NONE',  ( 10.00000000000000000, 0.000000000000000000, 0.000000000000000000 ) ) ;
#30629 = DIRECTION ( 'NONE',  ( -1.000000000000000000, 0.000000000000000000, 0.000000000000000000 ) ) ;
#30630 = CARTESIAN_POINT ( 'NONE',  ( 0.000000000000000000, -21.53537804866103045, 30.80686688397002371 ) ) ;
#30631 = CARTESIAN_POINT ( 'NONE',  ( -93.84685191531247028, -211.9973110713294489, 77.31322916753381946 ) ) ;
#30632 = EDGE_CURVE ( 'NONE', #17145, #63489, #41875, .T. ) ;
#30633 = EDGE_LOOP ( 'NONE', ( #20766, #68736, #65722, #22113 ) ) ;
#30634 = CARTESIAN_POINT ( 'NONE',  ( 10.00000000000000000, -33.17418723428319538, 17.67226234102814431 ) ) ;
#30635 = VECTOR ( 'NONE', #60321, 1000.000000000000000 ) ;
#30636 = DIRECTION ( 'NONE',  ( -1.000000000000000000, 0.000000000000000000, -0.000000000000000000 ) ) ;
#30637 =( NAMED_UNIT ( * ) PLANE_ANGLE_UNIT ( ) SI_UNIT ( $, .RADIAN. ) );
#30638 = FACE_OUTER_BOUND ( 'NONE', #50050, .T. ) ;
#30639 = DIRECTION ( 'NONE',  ( 2.603472992746261562E-14, 2.546204323184492723E-14, -1.000000000000000000 ) ) ;
#30640 = CYLINDRICAL_SURFACE ( 'NONE', #63688, 31.99999999999999289 ) ;
#30641 = CARTESIAN_POINT ( 'NONE',  ( 97.64999999999999147, 90.00000000000002842, 89.68250000000000455 ) ) ;
#30642 = CARTESIAN_POINT ( 'NONE',  ( 10.00000000000000000, -17.67226234102801286, -33.17418723428327354 ) ) ;
#30643 = DIRECTION ( 'NONE',  ( 1.000000000000000000, 0.000000000000000000, 0.000000000000000000 ) ) ;
#30644 = EDGE_CURVE ( 'NONE', #41411, #2356, #11984, .T. ) ;
#30645 = DIRECTION ( 'NONE',  ( -1.000000000000000000, 0.000000000000000000, -0.000000000000000000 ) ) ;
#30646 = EDGE_CURVE ( 'NONE', #36423, #44854, #1123, .T. ) ;
#30647 = VECTOR ( 'NONE', #26176, 1000.000000000000114 ) ;
#30648 = CARTESIAN_POINT ( 'NONE',  ( 97.30629616937498838, 90.00000000000002842, 83.76906250086716454 ) ) ;
#30649 = CARTESIAN_POINT ( 'NONE',  ( -93.84685191531247028, -211.9973110713294489, 84.93322916753382401 ) ) ;
#30650 = FACE_OUTER_BOUND ( 'NONE', #29150, .T. ) ;
#30651 = EDGE_LOOP ( 'NONE', ( #72133, #52729, #2074, #25124 ) ) ;
#30652 = CARTESIAN_POINT ( 'NONE',  ( -12.50000000000000000, -107.5000000000000000, -40.00000000000000000 ) ) ;
#30653 = CARTESIAN_POINT ( 'NONE',  ( -97.64999999999996305, -209.9999999999999716, 80.47499999999999432 ) ) ;
#30654 = CARTESIAN_POINT ( 'NONE',  ( -97.30629616937501680, 91.33154071421968467, 76.25489583420049655 ) ) ;
#30655 = VECTOR ( 'NONE', #49892, 1000.000000000000000 ) ;
#30656 = ADVANCED_FACE ( 'NONE', ( #62786 ), #35292, .T. ) ;
#30657 = ADVANCED_FACE ( 'NONE', ( #46948 ), #52207, .T. ) ;
#30658 = CIRCLE ( 'NONE', #70309, 11.59999999999999787 ) ;
#30659 = CARTESIAN_POINT ( 'NONE',  ( 92.69370383062501162, -209.9999999999999716, 85.83281250086714920 ) ) ;
#30660 = ORIENTED_EDGE ( 'NONE', *, *, #382, .T. ) ;
#30661 = CARTESIAN_POINT ( 'NONE',  ( 11.99999999999999822, -8.966570791701281351, 81.50828551894223040 ) ) ;
#30662 = ORIENTED_EDGE ( 'NONE', *, *, #7641, .F. ) ;
#30663 = AXIS2_PLACEMENT_3D ( 'NONE', #47470, #24534, #40723 ) ;
#30664 = VERTEX_POINT ( 'NONE', #41304 ) ;
#30665 = CARTESIAN_POINT ( 'NONE',  ( 95.00000000000000000, -213.0599564267049857, 75.55375000000000796 ) ) ;
#30666 = DIRECTION ( 'NONE',  ( -1.000000000000000000, -0.000000000000000000, -0.000000000000000000 ) ) ;
#30667 = AXIS2_PLACEMENT_3D ( 'NONE', #19302, #52787, #53519 ) ;
#30668 = ORIENTED_EDGE ( 'NONE', *, *, #45182, .T. ) ;
#30669 = ORIENTED_EDGE ( 'NONE', *, *, #21306, .F. ) ;
#30670 = DIRECTION ( 'NONE',  ( 0.000000000000000000, -0.3090169943749549453, 0.9510565162951511997 ) ) ;
#30671 = CARTESIAN_POINT ( 'NONE',  ( 95.00000000000000000, -207.3369185715606307, 79.48281250086715488 ) ) ;
#30672 = DIRECTION ( 'NONE',  ( 0.000000000000000000, -0.3090169943749349057, -0.9510565162951577500 ) ) ;
#30673 = LINE ( 'NONE', #64537, #44789 ) ;
#30674 = FACE_OUTER_BOUND ( 'NONE', #24394, .T. ) ;
#30675 = CARTESIAN_POINT ( 'NONE',  ( -9.937067298023317008, 7.583184918921301865, -54.99999999999999289 ) ) ;
#30676 = CARTESIAN_POINT ( 'NONE',  ( 10.00000000000000000, 0.000000000000000000, 0.000000000000000000 ) ) ;
#30677 = CARTESIAN_POINT ( 'NONE',  ( 92.35000000000002274, -211.5299782133524502, 85.60791666666665378 ) ) ;
#30678 = EDGE_CURVE ( 'NONE', #55143, #31960, #34182, .T. ) ;
#30679 = ORIENTED_EDGE ( 'NONE', *, *, #42840, .T. ) ;
#30680 = VERTEX_POINT ( 'NONE', #57123 ) ;
#30681 = ORIENTED_EDGE ( 'NONE', *, *, #56282, .T. ) ;
#30682 = VERTEX_POINT ( 'NONE', #10887 ) ;
#30683 = CARTESIAN_POINT ( 'NONE',  ( 25.81725066941077529, -113.8380548628854854, 5.500000000000000000 ) ) ;
#30684 =( NAMED_UNIT ( * ) PLANE_ANGLE_UNIT ( ) SI_UNIT ( $, .RADIAN. ) );
#30685 = CARTESIAN_POINT ( 'NONE',  ( -97.30629616937501680, 91.33154071421968467, 84.66864583420047552 ) ) ;
#30686 = CARTESIAN_POINT ( 'NONE',  ( 0.000000000000000000, 67.80270845531887858, 46.11716303203210998 ) ) ;
#30687 = EDGE_CURVE ( 'NONE', #23480, #40077, #27532, .T. ) ;
#30688 = CARTESIAN_POINT ( 'NONE',  ( 10.00000000000000000, -33.00180498840035170, -17.80606268964575278 ) ) ;
#30689 = CARTESIAN_POINT ( 'NONE',  ( 93.67500000000001137, -212.2949673200287179, 74.94520833506761903 ) ) ;
#30690 = CARTESIAN_POINT ( 'NONE',  ( 94.99999999999998579, 93.05995642670504253, 75.87125000000000341 ) ) ;
#30691 = EDGE_CURVE ( 'NONE', #68921, #54538, #29941, .T. ) ;
#30692 = ORIENTED_EDGE ( 'NONE', *, *, #31414, .F. ) ;
#30693 = CARTESIAN_POINT ( 'NONE',  ( 5.000000000000000000, 3.925862922256160736, 41.81611651403863306 ) ) ;
#30694 = VERTEX_POINT ( 'NONE', #24 ) ;
#30695 = CARTESIAN_POINT ( 'NONE',  ( -92.34999999999999432, -209.9999999999999716, 85.23749999999999716 ) ) ;
#30697 = ORIENTED_EDGE ( 'NONE', *, *, #3257, .F. ) ;
#30696 = EDGE_CURVE ( 'NONE', #49620, #26331, #13158, .T. ) ;
#30698 = CARTESIAN_POINT ( 'NONE',  ( -93.67500000000003979, 92.29496732002878900, 84.78770833506763438 ) ) ;
#30699 = CARTESIAN_POINT ( 'NONE',  ( 93.84685191531248449, 91.99731107132950569, 85.88572916753381037 ) ) ;
#30700 = CIRCLE ( 'NONE', #18681, 77.49899999999999523 ) ;
#30701 = DIRECTION ( 'NONE',  ( 0.000000000000000000, 0.000000000000000000, 1.000000000000000000 ) ) ;
#30702 = EDGE_CURVE ( 'NONE', #67105, #15341, #7825, .T. ) ;
#30703 = FACE_OUTER_BOUND ( 'NONE', #30023, .T. ) ;
#30704 = CARTESIAN_POINT ( 'NONE',  ( -96.32499999999996021, -207.7050326799711968, 78.54354166840096241 ) ) ;
#30705 = DIRECTION ( 'NONE',  ( 0.000000000000000000, 0.000000000000000000, -1.000000000000000000 ) ) ;
#30706 = ORIENTED_EDGE ( 'NONE', *, *, #32725, .T. ) ;
#30707 = CYLINDRICAL_SURFACE ( 'NONE', #49499, 32.00000000000000000 ) ;
#30708 = CIRCLE ( 'NONE', #19861, 31.99999999999999645 ) ;
#30709 = CARTESIAN_POINT ( 'NONE',  ( -93.84685191531248449, -208.0026889286704943, 75.46114583420047950 ) ) ;
#30710 = VERTEX_POINT ( 'NONE', #47319 ) ;
#30711 = VERTEX_POINT ( 'NONE', #19101 ) ;
#30713 = CARTESIAN_POINT ( 'NONE',  ( 0.000000000000000000, 20.85821328998741109, 10.92862929874522315 ) ) ;
#30712 = AXIS2_PLACEMENT_3D ( 'NONE', #7721, #53579, #25005 ) ;
#30714 = DIRECTION ( 'NONE',  ( 0.000000000000000000, 0.000000000000000000, -1.000000000000000000 ) ) ;
#30715 = AXIS2_PLACEMENT_3D ( 'NONE', #59975, #13709, #36646 ) ;
#30716 = CIRCLE ( 'NONE', #25892, 16.00000000000000000 ) ;
#30717 = CARTESIAN_POINT ( 'NONE',  ( -94.99999999999997158, -212.6630814284392557, 89.32531250086715602 ) ) ;
#30718 = EDGE_LOOP ( 'NONE', ( #56441, #55182, #57050, #60279 ) ) ;
#30719 = EDGE_CURVE ( 'NONE', #24727, #55701, #64601, .T. ) ;
#30720 = DIRECTION ( 'NONE',  ( 1.000000000000000000, 0.000000000000000000, 0.000000000000000000 ) ) ;
#30721 = ORIENTED_EDGE ( 'NONE', *, *, #36150, .F. ) ;
#30722 = ORIENTED_EDGE ( 'NONE', *, *, #64614, .F. ) ;
#30723 = DIRECTION ( 'NONE',  ( 0.000000000000000000, -0.4539904997395351471, -0.8910065241883738940 ) ) ;
#30724 = CARTESIAN_POINT ( 'NONE',  ( 92.69370383062498320, 88.66845928578037217, 89.21947916753381946 ) ) ;
#30725 = AXIS2_PLACEMENT_3D ( 'NONE', #61660, #45875, #68041 ) ;
#30726 = CYLINDRICAL_SURFACE ( 'NONE', #19343, 82.00000000000000000 ) ;
#30727 = CARTESIAN_POINT ( 'NONE',  ( 96.15314808468748708, 91.99731107132950569, 81.17614583420048291 ) ) ;
#30728 = CARTESIAN_POINT ( 'NONE',  ( 11.99999999999999822, 20.41045688087824317, 72.35160999960824313 ) ) ;
#30729 = DIRECTION ( 'NONE',  ( 0.000000000000000000, 0.000000000000000000, 1.000000000000000000 ) ) ;
#30730 = CARTESIAN_POINT ( 'NONE',  ( 6.000000000000000000, 16.65972982744933972, 80.28980883073764119 ) ) ;
#30731 = DIRECTION ( 'NONE',  ( -0.000000000000000000, -0.000000000000000000, -1.000000000000000000 ) ) ;
#30732 = EDGE_CURVE ( 'NONE', #9512, #9077, #70218, .T. ) ;
#30733 = CARTESIAN_POINT ( 'NONE',  ( -92.35000000000003695, 90.00000000000004263, 87.77749999999998920 ) ) ;
#30734 = FACE_OUTER_BOUND ( 'NONE', #5053, .T. ) ;
#30735 = EDGE_CURVE ( 'NONE', #45993, #53141, #31125, .T. ) ;
#30736 = EDGE_CURVE ( 'NONE', #10762, #31821, #53322, .T. ) ;
#30737 = CYLINDRICAL_SURFACE ( 'NONE', #43258, 42.00000000000000000 ) ;
#30738 = CARTESIAN_POINT ( 'NONE',  ( 10.00000000000000000, 31.46837873494978055, 68.27212725128286763 ) ) ;
#30739 = ORIENTED_EDGE ( 'NONE', *, *, #70497, .T. ) ;
#30740 = CARTESIAN_POINT ( 'NONE',  ( -97.30629616937501680, 91.33154071421968467, 87.68489583420047495 ) ) ;
#30741 = CARTESIAN_POINT ( 'NONE',  ( 6.782329983125267248, 10.49999999999999645, -125.0000000000000000 ) ) ;
#30742 = DIRECTION ( 'NONE',  ( 1.000000000000000000, 0.000000000000000000, 0.000000000000000000 ) ) ;
#30743 = ORIENTED_EDGE ( 'NONE', *, *, #48123, .T. ) ;
#30744 = LINE ( 'NONE', #25490, #73855 ) ;
#30745 = DIRECTION ( 'NONE',  ( -1.000000000000000000, 0.000000000000000000, -0.000000000000000000 ) ) ;
#30746 = VECTOR ( 'NONE', #35442, 1000.000000000000000 ) ;
#30747 = DIRECTION ( 'NONE',  ( 0.000000000000000000, 0.000000000000000000, 1.000000000000000000 ) ) ;
#30748 = CARTESIAN_POINT ( 'NONE',  ( 93.84685191531249870, -208.0026889286704943, 81.44072916753381719 ) ) ;
#30749 = AXIS2_PLACEMENT_3D ( 'NONE', #12491, #18499, #29770 ) ;
#30750 = ORIENTED_EDGE ( 'NONE', *, *, #9099, .T. ) ;
#30751 = AXIS2_PLACEMENT_3D ( 'NONE', #8885, #38194, #37473 ) ;
#30752 = ORIENTED_EDGE ( 'NONE', *, *, #32822, .F. ) ;
#30753 = EDGE_CURVE ( 'NONE', #62900, #50450, #57562, .T. ) ;
#30754 = VERTEX_POINT ( 'NONE', #36024 ) ;
#30755 = CIRCLE ( 'NONE', #34373, 31.99999999999999289 ) ;
#30756 = DIRECTION ( 'NONE',  ( -1.000000000000000000, -0.000000000000000000, -0.000000000000000000 ) ) ;
#30757 = AXIS2_PLACEMENT_3D ( 'NONE', #10198, #33120, #57190 ) ;
#30758 =( BOUNDED_CURVE ( )  B_SPLINE_CURVE ( 2, ( #71701, #61931, #66454, #4420, #32212, #15306, #32595, #9673, #72077 ),
 .UNSPECIFIED., .F., .F. ) 
 B_SPLINE_CURVE_WITH_KNOTS ( ( 3, 2, 2, 2, 3 ),
 ( 0.8255245790564498254, 0.8325803338241195561, 0.8396360993650018312, 0.8466918649058843283, 0.8466920362367555963 ),
 .UNSPECIFIED. ) 
 CURVE ( )  GEOMETRIC_REPRESENTATION_ITEM ( )  RATIONAL_B_SPLINE_CURVE ( ( 1.000000000000000000, 0.8660254037844387076, 1.000000000000000000, 0.8660254037844387076, 1.000000000000000000, 0.8660254037844387076, 1.000000000000000000, 0.9999967467762123086, 0.9999934937104166810 ) ) 
 REPRESENTATION_ITEM ( '' )  );
#30759 = FACE_OUTER_BOUND ( 'NONE', #13001, .T. ) ;
#30760 = VERTEX_POINT ( 'NONE', #7459 ) ;
#30761 = CARTESIAN_POINT ( 'NONE',  ( 92.69370383062501162, -211.3315407142195852, 79.69447916753381378 ) ) ;
#30762 = ORIENTED_EDGE ( 'NONE', *, *, #31894, .F. ) ;
#30763 = DIRECTION ( 'NONE',  ( -0.000000000000000000, -0.000000000000000000, 1.000000000000000000 ) ) ;
#30764 = VERTEX_POINT ( 'NONE', #58585 ) ;
#30765 = ORIENTED_EDGE ( 'NONE', *, *, #51367, .T. ) ;
#30766 = CARTESIAN_POINT ( 'NONE',  ( 11.99999999999999822, 0.000000000000000000, 0.000000000000000000 ) ) ;
#30767 = AXIS2_PLACEMENT_3D ( 'NONE', #22551, #44372, #39854 ) ;
#30768 = CARTESIAN_POINT ( 'NONE',  ( 97.65000000000000568, -208.4700217866474645, 80.21041666666666003 ) ) ;
#30769 = EDGE_CURVE ( 'NONE', #70184, #50464, #74339, .T. ) ;
#30770 = VERTEX_POINT ( 'NONE', #12714 ) ;
#30771 = DIRECTION ( 'NONE',  ( 0.000000000000000000, -0.6494480483301903195, 0.7604059656000251577 ) ) ;
#30772 = CARTESIAN_POINT ( 'NONE',  ( 97.64999999999999147, -209.9999999999999716, 83.41187500173430180 ) ) ;
#30773 = CARTESIAN_POINT ( 'NONE',  ( 92.34999999999999432, 90.00000000000002842, 85.55499999999999261 ) ) ;
#30774 = ADVANCED_FACE ( 'NONE', ( #70583 ), #64243, .F. ) ;
#30775 = ORIENTED_EDGE ( 'NONE', *, *, #22226, .F. ) ;
#30776 = DIRECTION ( 'NONE',  ( 0.000000000000000000, 0.000000000000000000, 1.000000000000000000 ) ) ;
#30777 = CARTESIAN_POINT ( 'NONE',  ( 11.99999999999999822, 0.000000000000000000, 0.000000000000000000 ) ) ;
#30778 = ORIENTED_EDGE ( 'NONE', *, *, #65758, .F. ) ;
#30779 = ORIENTED_EDGE ( 'NONE', *, *, #3744, .T. ) ;
#30780 = CARTESIAN_POINT ( 'NONE',  ( -96.15314808468751551, 88.00268892867056536, 88.63739583420048973 ) ) ;
#30781 = CARTESIAN_POINT ( 'NONE',  ( 94.99999999999998579, 92.66308142843935514, 85.67406250086715147 ) ) ;
#30782 = ORIENTED_EDGE ( 'NONE', *, *, #23402, .T. ) ;
#30783 = CARTESIAN_POINT ( 'NONE',  ( 94.99999999999998579, 86.94004357329500010, 86.42812500173430124 ) ) ;
#30784 = EDGE_CURVE ( 'NONE', #30710, #66307, #35644, .T. ) ;
#30785 = ADVANCED_FACE ( 'NONE', ( #42051 ), #37148, .T. ) ;
#30786 =( LENGTH_UNIT ( ) NAMED_UNIT ( * ) SI_UNIT ( .MILLI., .METRE. ) );
#30787 = ORIENTED_EDGE ( 'NONE', *, *, #53153, .T. ) ;
#30788 = FACE_BOUND ( 'NONE', #34757, .T. ) ;
#30789 = ORIENTED_EDGE ( 'NONE', *, *, #2981, .F. ) ;
#30790 = VERTEX_POINT ( 'NONE', #8572 ) ;
#30791 = VERTEX_POINT ( 'NONE', #7086 ) ;
#30792 = CARTESIAN_POINT ( 'NONE',  ( -4.653126046682595884, -146.1313684676804314, 5.500000000000000000 ) ) ;
#30793 = PLANE ( 'NONE',  #16901 ) ;
#30794 = CARTESIAN_POINT ( 'NONE',  ( -92.35000000000003695, 90.00000000000004263, 85.87249999999998806 ) ) ;
#30795 = VERTEX_POINT ( 'NONE', #30004 ) ;
#30796 = DIRECTION ( 'NONE',  ( -1.000000000000000000, -0.000000000000000000, -0.000000000000000000 ) ) ;
#30797 = LINE ( 'NONE', #35703, #44311 ) ;
#30798 = EDGE_LOOP ( 'NONE', ( #10242, #47379, #74070, #30851 ) ) ;
#30799 = FACE_OUTER_BOUND ( 'NONE', #22292, .T. ) ;
#30800 = CARTESIAN_POINT ( 'NONE',  ( -92.69370383062498320, -209.9999999999999716, 82.34031250086714238 ) ) ;
#30801 = ORIENTED_EDGE ( 'NONE', *, *, #45498, .F. ) ;
#30803 = EDGE_CURVE ( 'NONE', #55469, #25695, #65717, .T. ) ;
#30802 = DIRECTION ( 'NONE',  ( 0.000000000000000000, -0.7071067811865389130, -0.7071067811865561215 ) ) ;
#30804 = CIRCLE ( 'NONE', #4383, 16.00000000000000000 ) ;
#30805 = CARTESIAN_POINT ( 'NONE',  ( 3.000000000000000000, 2.935248768560057897, -3.252606517456513302E-15 ) ) ;
#30806 = DIRECTION ( 'NONE',  ( -0.000000000000000000, -0.000000000000000000, 1.000000000000000000 ) ) ;
#30807 = LINE ( 'NONE', #24446, #29049 ) ;
#30808 = AXIS2_PLACEMENT_3D ( 'NONE', #63999, #46697, #58343 ) ;
#30809 = CYLINDRICAL_SURFACE ( 'NONE', #12633, 16.00000000000000000 ) ;
#30810 = AXIS2_PLACEMENT_3D ( 'NONE', #24900, #35797, #58752 ) ;
#30811 = DIRECTION ( 'NONE',  ( -1.000000000000000000, 0.000000000000000000, 0.000000000000000000 ) ) ;
#30812 = DIRECTION ( 'NONE',  ( -0.000000000000000000, -0.000000000000000000, -1.000000000000000000 ) ) ;
#30813 = VECTOR ( 'NONE', #53584, 1000.000000000000000 ) ;
#30814 = CARTESIAN_POINT ( 'NONE',  ( 97.24889018994936407, -210.5903413996855704, 74.79348190356850523 ) ) ;
#30815 = CARTESIAN_POINT ( 'NONE',  ( 11.99999999999999822, -36.72794159290288718, 65.59268652807197952 ) ) ;
#30816 = CARTESIAN_POINT ( 'NONE',  ( -92.35000000000003695, 89.99999999755290503, 75.15687493081163950 ) ) ;
#30817 = EDGE_CURVE ( 'NONE', #24340, #52404, #52773, .T. ) ;
#30818 = ADVANCED_FACE ( 'NONE', ( #2604 ), #54429, .F. ) ;
#30819 = CARTESIAN_POINT ( 'NONE',  ( -96.15314808468751551, 88.00268892867056536, 75.77864583420047495 ) ) ;
#30820 = CARTESIAN_POINT ( 'NONE',  ( 11.99999999999999822, -60.67117009219176538, 55.16347631943021668 ) ) ;
#30821 = LINE ( 'NONE', #54511, #50617 ) ;
#30822 = EDGE_CURVE ( 'NONE', #70837, #62740, #17935, .T. ) ;
#30823 = CIRCLE ( 'NONE', #878, 31.99999999999998579 ) ;
#30824 = UNCERTAINTY_MEASURE_WITH_UNIT (LENGTH_MEASURE( 1.000000000000000082E-05 ), #31507, 'distance_accuracy_value', 'NONE');
#30825 = EDGE_CURVE ( 'NONE', #12692, #30034, #18723, .T. ) ;
#30826 = DIRECTION ( 'NONE',  ( 1.000000000000000000, 0.000000000000000000, 0.000000000000000000 ) ) ;
#30827 = CARTESIAN_POINT ( 'NONE',  ( 0.000000000000000000, -6.736453364083817341, 36.88895765772630142 ) ) ;
#30828 = FACE_OUTER_BOUND ( 'NONE', #74225, .T. ) ;
#30829 = CARTESIAN_POINT ( 'NONE',  ( 92.34999999999999432, -211.5299782133524502, 77.35291666666665833 ) ) ;
#30830 = PLANE ( 'NONE',  #74234 ) ;
#30831 = LINE ( 'NONE', #2318, #65288 ) ;
#30832 = CARTESIAN_POINT ( 'NONE',  ( -93.67499999999998295, -212.2949673200287179, 88.30666666666665776 ) ) ;
#30833 = VECTOR ( 'NONE', #15156, 1000.000000000000000 ) ;
#30834 = LINE ( 'NONE', #18451, #18853 ) ;
#30835 = ORIENTED_EDGE ( 'NONE', *, *, #27048, .T. ) ;
#30836 = FACE_OUTER_BOUND ( 'NONE', #11915, .T. ) ;
#30837 = DIRECTION ( 'NONE',  ( 1.000000000000000000, 0.000000000000000000, 0.000000000000000000 ) ) ;
#30838 = CARTESIAN_POINT ( 'NONE',  ( 96.32499999999998863, -207.7050326799711968, 81.61270833506763722 ) ) ;
#30839 = CARTESIAN_POINT ( 'NONE',  ( 0.000000000000000000, 31.52238457039599595, 27.75498641678753842 ) ) ;
#30840 = VERTEX_POINT ( 'NONE', #42412 ) ;
#30841 = DIRECTION ( 'NONE',  ( -1.000000000000000000, 0.000000000000000000, 0.000000000000000000 ) ) ;
#30842 = VERTEX_POINT ( 'NONE', #13819 ) ;
#30843 = ADVANCED_FACE ( 'NONE', ( #67192 ), #9298, .F. ) ;
#30844 = CARTESIAN_POINT ( 'NONE',  ( 93.84685191531251292, -211.9973110713294489, 85.30364583420046642 ) ) ;
#30845 = CARTESIAN_POINT ( 'NONE',  ( 96.15314808468748708, -208.0026889286704943, 88.31989583420048007 ) ) ;
#30846 = AXIS2_PLACEMENT_3D ( 'NONE', #60157, #19166, #14638 ) ;
#30847 = ORIENTED_EDGE ( 'NONE', *, *, #27683, .T. ) ;
#30848 = EDGE_CURVE ( 'NONE', #36342, #54986, #22789, .T. ) ;
#30849 = CARTESIAN_POINT ( 'NONE',  ( 97.30629616937498838, -211.3315407142195852, 88.79614583420050167 ) ) ;
#30850 = VECTOR ( 'NONE', #48829, 1000.000000000000000 ) ;
#30851 = ORIENTED_EDGE ( 'NONE', *, *, #4780, .T. ) ;
#30852 = FACE_BOUND ( 'NONE', #38448, .T. ) ;
#30853 = ORIENTED_EDGE ( 'NONE', *, *, #39205, .F. ) ;
#30854 = CARTESIAN_POINT ( 'NONE',  ( -93.84685191531254134, 91.99731107132950569, 76.25489583420049655 ) ) ;
#30855 = EDGE_CURVE ( 'NONE', #26546, #24685, #34739, .T. ) ;
#30856 = ORIENTED_EDGE ( 'NONE', *, *, #44414, .F. ) ;
#30857 = AXIS2_PLACEMENT_3D ( 'NONE', #53389, #65780, #24445 ) ;
#30858 = VERTEX_POINT ( 'NONE', #60817 ) ;
#30859 = DIRECTION ( 'NONE',  ( 0.000000000000000000, 0.000000000000000000, 1.000000000000000000 ) ) ;
#30860 = AXIS2_PLACEMENT_3D ( 'NONE', #19731, #42678, #54333 ) ;
#30861 = ADVANCED_FACE ( 'NONE', ( #32215 ), #72804, .T. ) ;
#30862 = VERTEX_POINT ( 'NONE', #3692 ) ;
#30863 = LINE ( 'NONE', #35413, #32883 ) ;
#30864 = DIRECTION ( 'NONE',  ( -1.000000000000000000, 0.000000000000000000, -0.000000000000000000 ) ) ;
#30865 = ORIENTED_EDGE ( 'NONE', *, *, #57236, .F. ) ;
#30867 = CARTESIAN_POINT ( 'NONE',  ( 11.99999999999999822, 36.73666225445988687, -65.58780272294035285 ) ) ;
#30866 = PRODUCT_DEFINITION_SHAPE ( 'NONE', 'NONE',  #74367 ) ;
#30868 = AXIS2_PLACEMENT_3D ( 'NONE', #63970, #12077, #22627 ) ;
#30869 = ORIENTED_EDGE ( 'NONE', *, *, #14946, .T. ) ;
#30870 = CARTESIAN_POINT ( 'NONE',  ( -7.999999999999992895, -1.142349898368590025E-14, -6.370018489464426943E-15 ) ) ;
#30871 = ORIENTED_EDGE ( 'NONE', *, *, #71253, .F. ) ;
#30872 = ADVANCED_FACE ( 'NONE', ( #66457 ), #72446, .T. ) ;
#30873 = ORIENTED_EDGE ( 'NONE', *, *, #5612, .F. ) ;
#30874 = ORIENTED_EDGE ( 'NONE', *, *, #47603, .F. ) ;
#30875 = CARTESIAN_POINT ( 'NONE',  ( 97.30629616937498838, -208.6684592857803011, 77.94822916753381037 ) ) ;
#30876 = CARTESIAN_POINT ( 'NONE',  ( 10.00000000000000000, -81.96053171279899630, -2.543863470249235981 ) ) ;
#30877 = DIRECTION ( 'NONE',  ( 0.000000000000000000, 0.000000000000000000, -1.000000000000000000 ) ) ;
#30878 = VERTEX_POINT ( 'NONE', #26215 ) ;
#30879 = VECTOR ( 'NONE', #50279, 1000.000000000000000 ) ;
#30880 = CARTESIAN_POINT ( 'NONE',  ( -97.64999999999996305, -211.5299782133524218, 78.70229166840096013 ) ) ;
#30881 = PLANE ( 'NONE',  #49779 ) ;
#30882 = CARTESIAN_POINT ( 'NONE',  ( 94.99999999999998579, 90.00000000000002842, 90.00000000000000000 ) ) ;
#30883 = DIRECTION ( 'NONE',  ( 0.000000000000000000, 0.000000000000000000, 1.000000000000000000 ) ) ;
#30884 = DIRECTION ( 'NONE',  ( 1.000000000000000000, 0.000000000000000000, 0.000000000000000000 ) ) ;
#30885 = CARTESIAN_POINT ( 'NONE',  ( -96.15314808468747287, -208.0026889286704943, 80.01197916753380923 ) ) ;
#30886 = AXIS2_PLACEMENT_3D ( 'NONE', #342, #11559, #51050 ) ;
#30887 = CARTESIAN_POINT ( 'NONE',  ( -92.69370383062502583, 91.33154071421968467, 80.64697916753382856 ) ) ;
#30888 = ORIENTED_EDGE ( 'NONE', *, *, #67264, .T. ) ;
#30889 = ADVANCED_FACE ( 'NONE', ( #37518 ), #66098, .F. ) ;
#30890 = CARTESIAN_POINT ( 'NONE',  ( 93.84685191531248449, 88.00268892867053694, 81.49364583420047836 ) ) ;
#30891 = ORIENTED_EDGE ( 'NONE', *, *, #69519, .T. ) ;
#30892 = CARTESIAN_POINT ( 'NONE',  ( 92.35001943615621656, 91.52998943482253935, 78.59645755884380947 ) ) ;
#30893 = DIRECTION ( 'NONE',  ( -1.000000000000000000, 0.000000000000000000, -0.000000000000000000 ) ) ;
#30895 = ADVANCED_FACE ( 'NONE', ( #49885 ), #49521, .F. ) ;
#30894 = DIRECTION ( 'NONE',  ( -1.000000000000000000, -0.000000000000000000, -0.000000000000000000 ) ) ;
#30896 = CARTESIAN_POINT ( 'NONE',  ( -1.499592026101402853, -119.9650177866181764, -2.500000000000000000 ) ) ;
#30897 = DIRECTION ( 'NONE',  ( 0.000000000000000000, 0.000000000000000000, -1.000000000000000000 ) ) ;
#30898 = CARTESIAN_POINT ( 'NONE',  ( -94.99999999999997158, -212.6630814284392557, 84.08656250086714579 ) ) ;
#30899 = DIRECTION ( 'NONE',  ( -1.000000000000000000, -0.000000000000000000, 0.000000000000000000 ) ) ;
#30900 = LINE ( 'NONE', #53113, #60743 ) ;
#30901 = EDGE_CURVE ( 'NONE', #45600, #15888, #61187, .T. ) ;
#30902 = LINE ( 'NONE', #36546, #25093 ) ;
#30903 = ORIENTED_EDGE ( 'NONE', *, *, #36345, .T. ) ;
#30904 = ORIENTED_EDGE ( 'NONE', *, *, #50319, .F. ) ;
#30905 = DIRECTION ( 'NONE',  ( -0.2079116908177527367, 1.197885328332319922E-16, -0.9781476007338070211 ) ) ;
#30906 = CARTESIAN_POINT ( 'NONE',  ( -97.65000000000001990, 88.47002178664754979, 76.08291666666666231 ) ) ;
#30907 = CARTESIAN_POINT ( 'NONE',  ( -92.35000000000005116, 88.47002178664754979, 84.62895833506763665 ) ) ;
#30908 = ADVANCED_FACE ( 'NONE', ( #26591 ), #21307, .T. ) ;
#30909 = CARTESIAN_POINT ( 'NONE',  ( -93.84685191531252713, 88.00268892867056536, 86.67947916753381321 ) ) ;
#30910 = CARTESIAN_POINT ( 'NONE',  ( -3.000000000000000000, -26.23277895567245821, -4.042438405570103477 ) ) ;
#30911 = DIRECTION ( 'NONE',  ( -0.000000000000000000, -0.000000000000000000, -1.000000000000000000 ) ) ;
#30912 = CARTESIAN_POINT ( 'NONE',  ( 10.00000000000000000, 0.000000000000000000, 0.000000000000000000 ) ) ;
#30913 = CIRCLE ( 'NONE', #18894, 82.00000000000000000 ) ;
#30914 = ORIENTED_EDGE ( 'NONE', *, *, #1737, .T. ) ;
#30915 = EDGE_CURVE ( 'NONE', #67983, #47594, #9506, .T. ) ;
#30916 = CARTESIAN_POINT ( 'NONE',  ( -96.15314808468751551, 88.00268892867056536, 75.77864583420047495 ) ) ;
#30917 = VECTOR ( 'NONE', #56273, 1000.000000000000000 ) ;
#30918 = EDGE_CURVE ( 'NONE', #57888, #69736, #55544, .T. ) ;
#30919 = CARTESIAN_POINT ( 'NONE',  ( 3.000000000000000000, 0.000000000000000000, 0.000000000000000000 ) ) ;
#30920 = DIRECTION ( 'NONE',  ( -1.000000000000000000, 0.000000000000000000, 0.000000000000000000 ) ) ;
#30921 = VECTOR ( 'NONE', #3212, 1000.000000000000000 ) ;
#30922 = DIRECTION ( 'NONE',  ( 0.000000000000000000, 0.000000000000000000, -1.000000000000000000 ) ) ;
#30923 = DIRECTION ( 'NONE',  ( -1.000000000000000000, 0.000000000000000000, 0.000000000000000000 ) ) ;
#30924 = DIRECTION ( 'NONE',  ( 1.000000000000000000, 0.000000000000000000, 0.000000000000000000 ) ) ;
#30925 = CARTESIAN_POINT ( 'NONE',  ( -94.99999999999997158, -207.3369185715606307, 83.92781250086716227 ) ) ;
#30926 = AXIS2_PLACEMENT_3D ( 'NONE', #26759, #66988, #48599 ) ;
#30927 = DIRECTION ( 'NONE',  ( 0.000000000000000000, 0.000000000000000000, 1.000000000000000000 ) ) ;
#30928 = DIRECTION ( 'NONE',  ( -1.000000000000000000, -0.000000000000000000, -0.000000000000000000 ) ) ;
#30929 = CARTESIAN_POINT ( 'NONE',  ( -97.30629616937497417, -208.6684592857803295, 77.04864583420048518 ) ) ;
#30930 = CARTESIAN_POINT ( 'NONE',  ( 10.00000000000000000, 62.50329211542435104, 41.76937507738811917 ) ) ;
#30931 = ORIENTED_EDGE ( 'NONE', *, *, #43144, .T. ) ;
#30932 = DIRECTION ( 'NONE',  ( -1.000000000000000000, -0.000000000000000000, 0.000000000000000000 ) ) ;
#30933 = CARTESIAN_POINT ( 'NONE',  ( -3.000000000000000000, -20.55727247249748046, 16.78983467731285018 ) ) ;
#30934 = DIRECTION ( 'NONE',  ( -1.000000000000000000, -0.000000000000000000, -0.000000000000000000 ) ) ;
#30935 = AXIS2_PLACEMENT_3D ( 'NONE', #58345, #32894, #35047 ) ;
#30936 = VECTOR ( 'NONE', #30338, 1000.000000000000000 ) ;
#30938 = AXIS2_PLACEMENT_3D ( 'NONE', #674, #47236, #17920 ) ;
#30937 = CARTESIAN_POINT ( 'NONE',  ( -8.000000000000007105, -1.142349898368590025E-14, -6.370018489464426943E-15 ) ) ;
#30939 = CARTESIAN_POINT ( 'NONE',  ( 95.00000000000000000, -212.6630814284392557, 89.32531250086715602 ) ) ;
#30940 = EDGE_LOOP ( 'NONE', ( #8207, #33871, #39308, #8692 ) ) ;
#30941 = CARTESIAN_POINT ( 'NONE',  ( 97.64999999999999147, 90.00002467581458632, 87.22187585518555863 ) ) ;
#30942 = FACE_BOUND ( 'NONE', #50610, .T. ) ;
#30943 = DIRECTION ( 'NONE',  ( -1.000000000000000000, 0.000000000000000000, 0.000000000000000000 ) ) ;
#30944 = ORIENTED_EDGE ( 'NONE', *, *, #34064, .F. ) ;
#30945 = VECTOR ( 'NONE', #32037, 1000.000000000000000 ) ;
#30946 = CARTESIAN_POINT ( 'NONE',  ( 2.500000000000029754, 73.00000000000001421, -255.0000000000000000 ) ) ;
#30947 = ORIENTED_EDGE ( 'NONE', *, *, #26313, .T. ) ;
#30948 = ADVANCED_FACE ( 'NONE', ( #44265 ), #4424, .T. ) ;
#30949 = DIRECTION ( 'NONE',  ( 0.000000000000000000, 0.000000000000000000, 1.000000000000000000 ) ) ;
#30950 = EDGE_CURVE ( 'NONE', #47594, #9891, #67567, .T. ) ;
#30951 = ORIENTED_EDGE ( 'NONE', *, *, #60031, .F. ) ;
#30952 = EDGE_LOOP ( 'NONE', ( #40608, #22200, #64575, #8708 ) ) ;
#30954 = ORIENTED_EDGE ( 'NONE', *, *, #4249, .T. ) ;
#30953 = EDGE_CURVE ( 'NONE', #23374, #68543, #70841, .T. ) ;
#30955 = FACE_OUTER_BOUND ( 'NONE', #9488, .T. ) ;
#30956 = ORIENTED_EDGE ( 'NONE', *, *, #457, .F. ) ;
#30957 = ORIENTED_EDGE ( 'NONE', *, *, #64511, .F. ) ;
#30958 = CARTESIAN_POINT ( 'NONE',  ( 93.84685191531248449, 88.00268892867053694, 81.65239583420049030 ) ) ;
#30959 = CARTESIAN_POINT ( 'NONE',  ( 0.000000000000000000, 59.03342792756263435, 46.54456581323825048 ) ) ;
#30960 = AXIS2_PLACEMENT_3D ( 'NONE', #28469, #16839, #16460 ) ;
#30961 = CARTESIAN_POINT ( 'NONE',  ( -93.67500000000003979, 87.70503267997129626, 85.13166666666666060 ) ) ;
#30962 = CIRCLE ( 'NONE', #72979, 11.59999999999999787 ) ;
#30963 = ORIENTED_EDGE ( 'NONE', *, *, #36941, .F. ) ;
#30964 = CIRCLE ( 'NONE', #68231, 12.49999999999999645 ) ;
#30965 = ORIENTED_EDGE ( 'NONE', *, *, #68534, .T. ) ;
#30966 = ORIENTED_EDGE ( 'NONE', *, *, #58068, .F. ) ;
#30967 = LINE ( 'NONE', #59942, #32236 ) ;
#30968 = ORIENTED_EDGE ( 'NONE', *, *, #62213, .T. ) ;
#30969 = DIRECTION ( 'NONE',  ( -0.1736481776669304145, 0.9848077530122082424, 0.000000000000000000 ) ) ;
#30970 = DIRECTION ( 'NONE',  ( -1.000000000000000000, 0.000000000000000000, 0.000000000000000000 ) ) ;
#30971 = AXIS2_PLACEMENT_3D ( 'NONE', #35093, #58769, #51259 ) ;
#30972 = CARTESIAN_POINT ( 'NONE',  ( -97.50991008589734577, 90.12150787501450111, 74.91582548749275361 ) ) ;
#30973 = DIRECTION ( 'NONE',  ( -1.000000000000000000, 0.000000000000000000, -0.000000000000000000 ) ) ;
#30974 = CIRCLE ( 'NONE', #67043, 37.49900000000000944 ) ;
#30975 = DIRECTION ( 'NONE',  ( 0.000000000000000000, 1.000000000000000000, -1.224646799147353207E-16 ) ) ;
#30976 = LINE ( 'NONE', #48283, #2448 ) ;
#30977 = CARTESIAN_POINT ( 'NONE',  ( -10.00000000000000000, 0.000000000000000000, 0.000000000000000000 ) ) ;
#30978 = CARTESIAN_POINT ( 'NONE',  ( -94.99999999999997158, -206.9400435732949575, 74.68062500173429896 ) ) ;
#30979 = DIRECTION ( 'NONE',  ( 0.9827303690289279636, 0.1850432970638682395, -0.000000000000000000 ) ) ;
#30981 = CARTESIAN_POINT ( 'NONE',  ( -92.35000000000005116, 88.47002178664754979, 75.10395833506764518 ) ) ;
#30980 = CARTESIAN_POINT ( 'NONE',  ( 94.99999999999998579, 93.05995642670504253, 75.31562500173430408 ) ) ;
#30982 = SHAPE_REPRESENTATION ( 'fast gear_ISO - Spur gear 2M 40T 20PA 10FW ---S40A75H50L38.0N', ( #43395 ), #39845 ) ;
#30983 = VERTEX_POINT ( 'NONE', #20078 ) ;
#30984 = CARTESIAN_POINT ( 'NONE',  ( 97.30629616937498838, 90.00000000000002842, 77.41906250086715602 ) ) ;
#30985 = LINE ( 'NONE', #48663, #72127 ) ;
#30986 = LINE ( 'NONE', #19340, #57130 ) ;
#30987 = DIRECTION ( 'NONE',  ( -1.000000000000000000, 0.000000000000000000, 0.000000000000000000 ) ) ;
#30988 = CARTESIAN_POINT ( 'NONE',  ( -10.00000000000000000, 0.000000000000000000, 0.000000000000000000 ) ) ;
#30989 = DIRECTION ( 'NONE',  ( -1.000000000000000000, 0.000000000000000000, -0.000000000000000000 ) ) ;
#30990 = EDGE_LOOP ( 'NONE', ( #1138, #10415 ) ) ;
#30991 = CARTESIAN_POINT ( 'NONE',  ( -92.34999999999999432, -209.9999999999999716, 80.15749999999999886 ) ) ;
#30992 = EDGE_CURVE ( 'NONE', #42410, #17471, #41936, .T. ) ;
#30993 = ADVANCED_FACE ( 'NONE', ( #66342 ), #54312, .T. ) ;
#30994 = CARTESIAN_POINT ( 'NONE',  ( 5.000000000000000000, 55.16347631943131802, -60.67117009219075641 ) ) ;
#30995 = ORIENTED_EDGE ( 'NONE', *, *, #45283, .T. ) ;
#30996 = ORIENTED_EDGE ( 'NONE', *, *, #839, .T. ) ;
#30997 = CIRCLE ( 'NONE', #10601, 62.50000000000000000 ) ;
#30998 = AXIS2_PLACEMENT_3D ( 'NONE', #42619, #36973, #37726 ) ;
#30999 = CARTESIAN_POINT ( 'NONE',  ( 11.99999999999999822, 24.73286445877808148, -73.44644590900034586 ) ) ;
#31000 = EDGE_CURVE ( 'NONE', #61584, #64608, #70725, .T. ) ;
#31001 = DIRECTION ( 'NONE',  ( -1.000000000000000000, 0.000000000000000000, 0.000000000000000000 ) ) ;
#31002 = CARTESIAN_POINT ( 'NONE',  ( 92.69370383062501162, -209.9999999999999716, 89.64281250086713726 ) ) ;
#31003 = CYLINDRICAL_SURFACE ( 'NONE', #7488, 42.00000000000000000 ) ;
#31004 = CYLINDRICAL_SURFACE ( 'NONE', #57715, 31.99999999999998579 ) ;
#31005 = CARTESIAN_POINT ( 'NONE',  ( 92.34999999999999432, 90.00000000000002842, 84.28499999999999659 ) ) ;
#31006 = AXIS2_PLACEMENT_3D ( 'NONE', #42509, #56005, #39469 ) ;
#31007 = ORIENTED_EDGE ( 'NONE', *, *, #32664, .T. ) ;
#31008 = DIRECTION ( 'NONE',  ( 1.000000000000000000, 0.000000000000000000, 0.000000000000000000 ) ) ;
#31009 = LINE ( 'NONE', #71227, #61877 ) ;
#31010 = LINE ( 'NONE', #6616, #70609 ) ;
#31011 = CARTESIAN_POINT ( 'NONE',  ( 11.99999999999999822, 76.66974797899837313, 11.30684508768366747 ) ) ;
#31012 = FACE_OUTER_BOUND ( 'NONE', #15907, .T. ) ;
#31013 = CYLINDRICAL_SURFACE ( 'NONE', #64904, 77.49899999999999523 ) ;
#31014 = PRODUCT_DEFINITION_CONTEXT ( 'detailed design', #72439, 'design' ) ;
#31015 = CARTESIAN_POINT ( 'NONE',  ( -92.34999999999999432, -209.9999999999999716, 90.00000000000000000 ) ) ;
#31016 = CYLINDRICAL_SURFACE ( 'NONE', #1663, 16.00000000000000000 ) ;
#31017 = FACE_OUTER_BOUND ( 'NONE', #17906, .T. ) ;
#31018 = AXIS2_PLACEMENT_3D ( 'NONE', #48357, #53264, #14888 ) ;
#31019 = CARTESIAN_POINT ( 'NONE',  ( 96.15314808468748708, 88.00268892867053694, 84.93322916753382401 ) ) ;
#31020 = AXIS2_PLACEMENT_3D ( 'NONE', #45957, #35032, #68881 ) ;
#31021 = AXIS2_PLACEMENT_3D ( 'NONE', #57584, #74111, #46295 ) ;
#31022 = CARTESIAN_POINT ( 'NONE',  ( -96.15314808468747287, -208.0026889286704943, 87.79072916753381151 ) ) ;
#31023 = CARTESIAN_POINT ( 'NONE',  ( 10.00000000000000000, -41.91543099594819921, 2.663952781846001816 ) ) ;
#31024 = ORIENTED_EDGE ( 'NONE', *, *, #69365, .T. ) ;
#31025 = CYLINDRICAL_SURFACE ( 'NONE', #36496, 77.49899999999999523 ) ;
#31026 = CARTESIAN_POINT ( 'NONE',  ( -92.34999999999999432, -208.4700217866474645, 80.84541666666666515 ) ) ;
#31027 = CARTESIAN_POINT ( 'NONE',  ( -97.30629616937501680, 91.33154071421968467, 76.88989583420047325 ) ) ;
#31028 = VECTOR ( 'NONE', #52655, 1000.000000000000000 ) ;
#31029 = VECTOR ( 'NONE', #3141, 1000.000000000000000 ) ;
#31030 = CARTESIAN_POINT ( 'NONE',  ( 92.69370383062501162, -208.6684592857803011, 85.14489583420048291 ) ) ;
#31031 = VERTEX_POINT ( 'NONE', #20466 ) ;
#31032 =( NAMED_UNIT ( * ) PLANE_ANGLE_UNIT ( ) SI_UNIT ( $, .RADIAN. ) );
#31033 = VERTEX_POINT ( 'NONE', #71580 ) ;
#31034 = VERTEX_POINT ( 'NONE', #2481 ) ;
#31035 = CIRCLE ( 'NONE', #73057, 42.00000000000000000 ) ;
#31036 = ADVANCED_FACE ( 'NONE', ( #31360 ), #59579, .T. ) ;
#31037 = DIRECTION ( 'NONE',  ( 0.000000000000000000, 0.000000000000000000, 1.000000000000000000 ) ) ;
#31038 = CARTESIAN_POINT ( 'NONE',  ( 10.00000000000000000, 30.84782396557218931, 21.32104025579126017 ) ) ;
#31039 = EDGE_CURVE ( 'NONE', #46252, #16557, #48294, .T. ) ;
#31040 = EDGE_LOOP ( 'NONE', ( #57841, #46453, #65928, #58421, #66875, #20141, #50015, #67618 ) ) ;
#31041 = VECTOR ( 'NONE', #62048, 1000.000000000000000 ) ;
#31042 = PLANE ( 'NONE',  #69609 ) ;
#31043 = CIRCLE ( 'NONE', #73065, 77.49899999999999523 ) ;
#31044 = ADVANCED_FACE ( 'NONE', ( #25367 ), #65974, .F. ) ;
#31045 = CARTESIAN_POINT ( 'NONE',  ( 92.69370383062501162, -208.6684592857803295, 78.31864583420050963 ) ) ;
#31046 = DIRECTION ( 'NONE',  ( -1.000000000000000000, -0.000000000000000000, -0.000000000000000000 ) ) ;
#31047 = DIRECTION ( 'NONE',  ( 1.000000000000000000, -0.000000000000000000, 0.000000000000000000 ) ) ;
#31048 = CIRCLE ( 'NONE', #8251, 37.49900000000000233 ) ;
#31049 = DIRECTION ( 'NONE',  ( 0.000000000000000000, 0.000000000000000000, -1.000000000000000000 ) ) ;
#31050 = EDGE_CURVE ( 'NONE', #10635, #66514, #7698, .T. ) ;
#31051 = LINE ( 'NONE', #61125, #9369 ) ;
#31052 = CARTESIAN_POINT ( 'NONE',  ( 93.67500000000001137, -207.7050326799711968, 81.00416666666666288 ) ) ;
#31053 = VERTEX_POINT ( 'NONE', #14445 ) ;
#31054 = ORIENTED_EDGE ( 'NONE', *, *, #67931, .T. ) ;
#31055 = ORIENTED_EDGE ( 'NONE', *, *, #30110, .T. ) ;
#31056 = ORIENTED_EDGE ( 'NONE', *, *, #20392, .F. ) ;
#31057 = DIRECTION ( 'NONE',  ( -1.000000000000000000, 0.000000000000000000, 0.000000000000000000 ) ) ;
#31058 = CARTESIAN_POINT ( 'NONE',  ( -93.84685191531254134, 91.99731107132950569, 84.50989583420049200 ) ) ;
#31059 = LINE ( 'NONE', #20147, #72249 ) ;
#31060 = CARTESIAN_POINT ( 'NONE',  ( 0.000000000000000000, -35.95386929396248377, -10.96151621346525751 ) ) ;
#31061 = CARTESIAN_POINT ( 'NONE',  ( 92.34999999999999432, 90.00000000000002842, 76.66499999999999204 ) ) ;
#31062 = EDGE_CURVE ( 'NONE', #57306, #1695, #24619, .T. ) ;
#31063 = ORIENTED_EDGE ( 'NONE', *, *, #74327, .T. ) ;
#31064 = CIRCLE ( 'NONE', #73084, 31.99999999999999645 ) ;
#31065 = CARTESIAN_POINT ( 'NONE',  ( -92.34999999999999432, -208.4700217866474645, 85.36979166840096411 ) ) ;
#31066 = ORIENTED_EDGE ( 'NONE', *, *, #67721, .T. ) ;
#31067 = EDGE_CURVE ( 'NONE', #35173, #48383, #11034, .T. ) ;
#31068 = DIRECTION ( 'NONE',  ( 0.000000000000000000, -0.4067366430757881068, -0.9135454576426063067 ) ) ;
#31069 = ORIENTED_EDGE ( 'NONE', *, *, #73348, .F. ) ;
#31070 = CARTESIAN_POINT ( 'NONE',  ( -95.00000000000002842, 93.05995642670501411, 86.11062500173430578 ) ) ;
#31071 = CARTESIAN_POINT ( 'NONE',  ( 97.30629616937498838, 90.00000000000002842, 87.57906250086715261 ) ) ;
#31072 = DIRECTION ( 'NONE',  ( 0.000000000000000000, -0.3826834323650969427, 0.9238795325112838519 ) ) ;
#31073 = CIRCLE ( 'NONE', #4708, 15.39727592608509177 ) ;
#31074 = VECTOR ( 'NONE', #45481, 1000.000000000000000 ) ;
#31075 = CARTESIAN_POINT ( 'NONE',  ( -16.07206065793331007, -141.0698568150738197, 2.500000000000000000 ) ) ;
#31076 = CARTESIAN_POINT ( 'NONE',  ( 12.00000000000000000, -4.261787119645322974, -26.19803753235774479 ) ) ;
#31077 = DIRECTION ( 'NONE',  ( 0.000000000000000000, 0.000000000000000000, 1.000000000000000000 ) ) ;
#31078 = ORIENTED_EDGE ( 'NONE', *, *, #61542, .F. ) ;
#31079 = CARTESIAN_POINT ( 'NONE',  ( -92.35000000000003695, 90.00000000000004263, 82.06250000000000000 ) ) ;
#31080 = ADVANCED_FACE ( 'NONE', ( #30614 ), #47923, .T. ) ;
#31081 = ADVANCED_FACE ( 'NONE', ( #26091 ), #13699, .F. ) ;
#31082 = PLANE ( 'NONE',  #8296 ) ;
#31083 = ORIENTED_EDGE ( 'NONE', *, *, #66895, .T. ) ;
#31084 = AXIS2_PLACEMENT_3D ( 'NONE', #21776, #44725, #27407 ) ;
#31085 = VERTEX_POINT ( 'NONE', #65594 ) ;
#31086 = CIRCLE ( 'NONE', #14225, 82.00000000000000000 ) ;
#31087 = CARTESIAN_POINT ( 'NONE',  ( 23.49916127795269460, -121.5130826919798039, -5.500000000000000000 ) ) ;
#31088 = CARTESIAN_POINT ( 'NONE',  ( 12.00000000000000000, -18.13022148937262656, -15.02647892043543898 ) ) ;
#31089 = LINE ( 'NONE', #64573, #8911 ) ;
#31090 = CARTESIAN_POINT ( 'NONE',  ( -92.69370383062498320, -209.9999999999999716, 85.03906250086714635 ) ) ;
#31091 = ORIENTED_EDGE ( 'NONE', *, *, #71115, .F. ) ;
#31092 = ORIENTED_EDGE ( 'NONE', *, *, #68374, .F. ) ;
#31093 = CIRCLE ( 'NONE', #53913, 15.99999999999999822 ) ;
#31094 = AXIS2_PLACEMENT_3D ( 'NONE', #14259, #37577, #20648 ) ;
#31095 = VERTEX_POINT ( 'NONE', #14062 ) ;
#31096 = DIRECTION ( 'NONE',  ( 0.000000000000000000, 0.000000000000000000, 1.000000000000000000 ) ) ;
#31097 = VECTOR ( 'NONE', #12818, 1000.000000000000000 ) ;
#31098 = VECTOR ( 'NONE', #49120, 1000.000000000000000 ) ;
#31099 = DIRECTION ( 'NONE',  ( -1.000000000000000000, -0.000000000000000000, -0.000000000000000000 ) ) ;
#31100 = SURFACE_SIDE_STYLE ('',( #13803 ) ) ;
#31101 = CARTESIAN_POINT ( 'NONE',  ( 92.69370383062498320, 88.66845928578035796, 82.07572916753382231 ) ) ;
#31102 = DIRECTION ( 'NONE',  ( 0.000000000000000000, 0.000000000000000000, 1.000000000000000000 ) ) ;
#31103 = CARTESIAN_POINT ( 'NONE',  ( 10.00000000000000000, 0.000000000000000000, 0.000000000000000000 ) ) ;
#31104 = DIRECTION ( 'NONE',  ( 0.000000000000000000, 0.3090169943749411785, 0.9510565162951556406 ) ) ;
#31105 = CIRCLE ( 'NONE', #32276, 31.99999999999998579 ) ;
#31106 = CYLINDRICAL_SURFACE ( 'NONE', #61588, 11.59999999999999787 ) ;
#31107 = VECTOR ( 'NONE', #60549, 1000.000000000000000 ) ;
#31108 = CARTESIAN_POINT ( 'NONE',  ( 23.49916127795269460, -121.5130826919798039, 5.500000000000000000 ) ) ;
#31109 = LINE ( 'NONE', #24010, #27489 ) ;
#31110 = CARTESIAN_POINT ( 'NONE',  ( -6.782329983125270800, 10.49999999999999467, -145.0000000000000000 ) ) ;
#31111 = PRODUCT_DEFINITION_CONTEXT ( 'detailed design', #48408, 'design' ) ;
#31112 = DIRECTION ( 'NONE',  ( -1.000000000000000000, -0.000000000000000000, -0.000000000000000000 ) ) ;
#31113 = VERTEX_POINT ( 'NONE', #59965 ) ;
#31114 = CARTESIAN_POINT ( 'NONE',  ( -95.00000000000002842, 92.66308142843932671, 86.30906250086714238 ) ) ;
#31115 = DIRECTION ( 'NONE',  ( -1.000000000000000000, 0.000000000000000000, 0.000000000000000000 ) ) ;
#31116 = EDGE_CURVE ( 'NONE', #42164, #4487, #38382, .T. ) ;
#31117 = SHAPE_REPRESENTATION ( 'BR-542', ( #31596, #44828, #26769, #18356, #35204, #14758, #47190, #13568, #48412, #17185, #54423, #32778, #23200, #5180, #56796, #2841, #52005, #8814, #33982, #9977, #53198, #22006, #37586, #67633, #62823, #72385, #24376, #59209, #68817, #50815, #29183, #40003, #1605, #55609, #66401, #65229, #426, #42408, #43607, #20767, #11171 ), #49585 ) ;
#31118 = ADVANCED_FACE ( 'NONE', ( #3567 ), #27579, .F. ) ;
#31119 = LINE ( 'NONE', #53688, #65675 ) ;
#31120 = EDGE_CURVE ( 'NONE', #3329, #13842, #26465, .T. ) ;
#31121 = ORIENTED_EDGE ( 'NONE', *, *, #27146, .F. ) ;
#31122 = CARTESIAN_POINT ( 'NONE',  ( 97.64999999999999147, -209.9999999999999716, 83.33250000000001023 ) ) ;
#31123 = CARTESIAN_POINT ( 'NONE',  ( 97.64999999999999147, 90.00000000000002842, 85.23749999999999716 ) ) ;
#31124 = CARTESIAN_POINT ( 'NONE',  ( -100.0000000000000142, 95.00000000000002842, 90.00000000000000000 ) ) ;
#31125 = CIRCLE ( 'NONE', #64741, 3.299999999999969624 ) ;
#31126 = EDGE_CURVE ( 'NONE', #4312, #63015, #40815, .T. ) ;
#31127 = AXIS2_PLACEMENT_3D ( 'NONE', #32114, #55053, #3582 ) ;
#31128 = CARTESIAN_POINT ( 'NONE',  ( 96.15314808468750130, -211.9973110713294489, 82.39322916753381776 ) ) ;
#31129 = EDGE_CURVE ( 'NONE', #60548, #62864, #8386, .T. ) ;
#31130 = AXIS2_PLACEMENT_3D ( 'NONE', #2236, #25129, #72088 ) ;
#31131 = VERTEX_POINT ( 'NONE', #50878 ) ;
#31132 = ORIENTED_EDGE ( 'NONE', *, *, #64527, .T. ) ;
#31133 = DIRECTION ( 'NONE',  ( 0.000000000000000000, -0.000000000000000000, 1.000000000000000000 ) ) ;
#31134 = ORIENTED_EDGE ( 'NONE', *, *, #11388, .T. ) ;
#31135 = CARTESIAN_POINT ( 'NONE',  ( 11.99999999999999822, -70.52718814184277107, 26.02418014898285037 ) ) ;
#31136 = LINE ( 'NONE', #37903, #22011 ) ;
#31137 = EDGE_CURVE ( 'NONE', #64009, #48915, #72014, .T. ) ;
#31138 = ORIENTED_EDGE ( 'NONE', *, *, #10877, .F. ) ;
#31139 = SURFACE_STYLE_USAGE ( .BOTH. , #72101 ) ;
#31140 = CARTESIAN_POINT ( 'NONE',  ( 97.30629616937498838, -208.6684592857803011, 76.20197916753382117 ) ) ;
#31141 = AXIS2_PLACEMENT_3D ( 'NONE', #41721, #30796, #53380 ) ;
#31142 = ORIENTED_EDGE ( 'NONE', *, *, #4247, .F. ) ;
#31143 = DIRECTION ( 'NONE',  ( 1.000000000000000000, -0.000000000000000000, 0.000000000000000000 ) ) ;
#31144 = ORIENTED_EDGE ( 'NONE', *, *, #2783, .F. ) ;
#31145 = ORIENTED_EDGE ( 'NONE', *, *, #58215, .F. ) ;
#31146 = DIRECTION ( 'NONE',  ( 0.000000000000000000, 0.000000000000000000, 1.000000000000000000 ) ) ;
#31147 = CIRCLE ( 'NONE', #25153, 31.99999999999999645 ) ;
#31148 = CARTESIAN_POINT ( 'NONE',  ( 10.00000000000000000, 71.91182617369189245, 28.89263327155772743 ) ) ;
#31149 = VECTOR ( 'NONE', #62338, 1000.000000000000000 ) ;
#31150 = ORIENTED_EDGE ( 'NONE', *, *, #51354, .F. ) ;
#31151 = DIRECTION ( 'NONE',  ( 0.8225049752423786442, 0.5687579148473752566, -0.000000000000000000 ) ) ;
#31152 = CARTESIAN_POINT ( 'NONE',  ( 97.64999999999997726, -208.4700217866474645, 84.09979166840095388 ) ) ;
#31154 = AXIS2_PLACEMENT_3D ( 'NONE', #68321, #44657, #57405 ) ;
#31153 = CARTESIAN_POINT ( 'NONE',  ( 96.32499999999998863, 87.70503267997126784, 83.86166666666666458 ) ) ;
#31155 = EDGE_CURVE ( 'NONE', #47765, #34388, #26395, .T. ) ;
#31156 = VERTEX_POINT ( 'NONE', #67807 ) ;
#31157 = DIRECTION ( 'NONE',  ( -1.000000000000000000, 0.000000000000000000, 0.000000000000000000 ) ) ;
#31158 = ADVANCED_FACE ( 'NONE', ( #33583 ), #61808, .F. ) ;
#31159 = CYLINDRICAL_SURFACE ( 'NONE', #42934, 11.59999999999999787 ) ;
#31160 = ORIENTED_EDGE ( 'NONE', *, *, #73847, .F. ) ;
#31161 = ORIENTED_EDGE ( 'NONE', *, *, #15009, .T. ) ;
#31162 = CARTESIAN_POINT ( 'NONE',  ( -92.69370383062505425, 91.33154071421968467, 88.26697916753381890 ) ) ;
#31163 = CARTESIAN_POINT ( 'NONE',  ( 92.69370383062498320, 90.00000000000002842, 81.38781250086714181 ) ) ;
#31164 = ORIENTED_EDGE ( 'NONE', *, *, #578, .T. ) ;
#31165 = CARTESIAN_POINT ( 'NONE',  ( 92.34999999999999432, 91.52997821335252127, 83.67645833506762187 ) ) ;
#31166 = CARTESIAN_POINT ( 'NONE',  ( 0.000000000000000000, 0.000000000000000000, 0.000000000000000000 ) ) ;
#31167 = ORIENTED_EDGE ( 'NONE', *, *, #62949, .F. ) ;
#31168 = CARTESIAN_POINT ( 'NONE',  ( 0.000000000000000000, -18.89407956138203204, -75.16055320797050854 ) ) ;
#31169 = ORIENTED_EDGE ( 'NONE', *, *, #38347, .T. ) ;
#31170 = ORIENTED_EDGE ( 'NONE', *, *, #18984, .F. ) ;
#31171 = ORIENTED_EDGE ( 'NONE', *, *, #31324, .T. ) ;
#31172 = CARTESIAN_POINT ( 'NONE',  ( 97.64999999999999147, -209.9999999999999716, 90.00000000000000000 ) ) ;
#31173 = CARTESIAN_POINT ( 'NONE',  ( -10.00000000000000000, 0.000000000000000000, 0.000000000000000000 ) ) ;
#31174 = CARTESIAN_POINT ( 'NONE',  ( -96.32500000000001705, 92.29496732002878900, 84.17916666666666003 ) ) ;
#31175 = EDGE_LOOP ( 'NONE', ( #44581, #6578, #23406, #3541, #65734 ) ) ;
#31176 = CARTESIAN_POINT ( 'NONE',  ( 92.34999999999999432, 90.00000000000002842, 90.00000000000000000 ) ) ;
#31177 = DIRECTION ( 'NONE',  ( -1.000000000000000000, -0.000000000000000000, -0.000000000000000000 ) ) ;
#31178 = ORIENTED_EDGE ( 'NONE', *, *, #19272, .T. ) ;
#31179 = CARTESIAN_POINT ( 'NONE',  ( -95.00000000002611955, 90.00000000000007105, -75.00000000000000000 ) ) ;
#31180 = CARTESIAN_POINT ( 'NONE',  ( -96.15314808468747287, -208.0026889286704943, 81.28197916753380525 ) ) ;
#31181 = ORIENTED_EDGE ( 'NONE', *, *, #5456, .F. ) ;
#31182 = CIRCLE ( 'NONE', #29937, 26.50000000000000355 ) ;
#31183 = CARTESIAN_POINT ( 'NONE',  ( -43.60332556124591719, -117.0000000000000000, 2.500000000000000000 ) ) ;
#31184 = CARTESIAN_POINT ( 'NONE',  ( 10.00000000000000000, -34.44570377933649041, 69.42325613327427902 ) ) ;
#31185 = CARTESIAN_POINT ( 'NONE',  ( -97.65000000002615366, -210.0000000000000284, -64.99999999999356248 ) ) ;
#31186 = DIRECTION ( 'NONE',  ( 0.000000000000000000, 0.9135454576426060846, -0.4067366430757888285 ) ) ;
#31187 = AXIS2_PLACEMENT_3D ( 'NONE', #9176, #38863, #32099 ) ;
#31188 = CIRCLE ( 'NONE', #9619, 42.00000000000000000 ) ;
#31189 = LINE ( 'NONE', #37950, #71553 ) ;
#31190 = DIRECTION ( 'NONE',  ( 0.000000000000000000, -0.7431448254773954654, 0.6691306063588569053 ) ) ;
#31192 = AXIS2_PLACEMENT_3D ( 'NONE', #16069, #44274, #33729 ) ;
#31191 = DIRECTION ( 'NONE',  ( -1.000000000000000000, -0.000000000000000000, -0.000000000000000000 ) ) ;
#31193 = DIRECTION ( 'NONE',  ( 0.000000000000000000, 0.6494480483301849905, -0.7604059656000298206 ) ) ;
#31194 = CARTESIAN_POINT ( 'NONE',  ( 11.99999999999999822, -21.60688246758642705, 79.10210256391358996 ) ) ;
#31195 = DIRECTION ( 'NONE',  ( 0.000000000000000000, -0.2334453638559128297, 0.9723699203976748917 ) ) ;
#31196 = EDGE_CURVE ( 'NONE', #35036, #32855, #55786, .T. ) ;
#31197 = CARTESIAN_POINT ( 'NONE',  ( -96.15314808468751551, 88.00268892867056536, 75.14364583420046984 ) ) ;
#31198 = CYLINDRICAL_SURFACE ( 'NONE', #31084, 2.649999999999985700 ) ;
#31199 = LINE ( 'NONE', #65434, #18203 ) ;
#31200 = CARTESIAN_POINT ( 'NONE',  ( 10.00000000000000000, 0.000000000000000000, 0.000000000000000000 ) ) ;
#31201 = DIRECTION ( 'NONE',  ( 1.000000000000000000, 0.000000000000000000, 0.000000000000000000 ) ) ;
#31202 = AXIS2_PLACEMENT_3D ( 'NONE', #7053, #25087, #12688 ) ;
#31203 = CIRCLE ( 'NONE', #4834, 37.49900000000000944 ) ;
#31204 = DIRECTION ( 'NONE',  ( -1.000000000000000000, 0.000000000000000000, 0.000000000000000000 ) ) ;
#31206 = CARTESIAN_POINT ( 'NONE',  ( 93.84685191531248449, 88.00268892867053694, 89.27239583420049485 ) ) ;
#31205 = AXIS2_PLACEMENT_3D ( 'NONE', #37749, #32821, #21931 ) ;
#31207 = AXIS2_PLACEMENT_3D ( 'NONE', #53949, #9180, #60336 ) ;
#31208 = DIRECTION ( 'NONE',  ( 0.000000000000000000, 0.8526401643540897357, 0.5224985647159531288 ) ) ;
#31209 = CARTESIAN_POINT ( 'NONE',  ( 97.65000000000000568, -211.5299782133524502, 78.83458333333334167 ) ) ;
#31210 = DIRECTION ( 'NONE',  ( 0.000000000000000000, 0.9876883405951371042, 0.1564344650402346715 ) ) ;
#31211 = CARTESIAN_POINT ( 'NONE',  ( -93.67499999999998295, -212.2949673200287179, 89.57666666666666799 ) ) ;
#31212 = EDGE_CURVE ( 'NONE', #26602, #2572, #61196, .T. ) ;
#31213 = CIRCLE ( 'NONE', #62478, 82.00000000000000000 ) ;
#31214 = VECTOR ( 'NONE', #35027, 1000.000000000000000 ) ;
#31215 = EDGE_CURVE ( 'NONE', #45970, #57911, #44398, .T. ) ;
#31216 = CARTESIAN_POINT ( 'NONE',  ( -97.64999999999996305, -209.9999999999999716, 84.92000000000000171 ) ) ;
#31217 =( BOUNDED_CURVE ( )  B_SPLINE_CURVE ( 2, ( #49881, #31853, #72801, #55908, #6273, #12262, #17171 ),
 .UNSPECIFIED., .F., .F. ) 
 B_SPLINE_CURVE_WITH_KNOTS ( ( 3, 2, 2, 3 ),
 ( 0.9101937466136234001, 0.9172495203192131408, 0.9243052858601306099, 0.9313609857438962525 ),
 .UNSPECIFIED. ) 
 CURVE ( )  GEOMETRIC_REPRESENTATION_ITEM ( )  RATIONAL_B_SPLINE_CURVE ( ( 1.000000000000000000, 0.8660254037844387076, 1.000000000000000000, 0.8660254037844387076, 1.000000000000000000, 0.8660266504798329601, 0.9999975066324136019 ) ) 
 REPRESENTATION_ITEM ( '' )  );
#31218 = VERTEX_POINT ( 'NONE', #61056 ) ;
#31219 = DIRECTION ( 'NONE',  ( 0.000000000000000000, -1.065814103640136079E-14, -1.000000000000000000 ) ) ;
#31220 = DIRECTION ( 'NONE',  ( -1.000000000000000000, -0.000000000000000000, -0.000000000000000000 ) ) ;
#31221 = ADVANCED_FACE ( 'NONE', ( #44133 ), #21561, .T. ) ;
#31222 = DIRECTION ( 'NONE',  ( -1.000000000000000000, -0.000000000000000000, 0.000000000000000000 ) ) ;
#31223 = EDGE_CURVE ( 'NONE', #64494, #51571, #52832, .T. ) ;
#31224 = ORIENTED_EDGE ( 'NONE', *, *, #63437, .T. ) ;
#31225 = DIRECTION ( 'NONE',  ( -1.000000000000000000, -0.000000000000000000, -0.000000000000000000 ) ) ;
#31226 = CARTESIAN_POINT ( 'NONE',  ( 10.00000000000000000, 40.68715046381928602, 10.41901085202092503 ) ) ;
#31227 = VERTEX_POINT ( 'NONE', #49758 ) ;
#31228 = CARTESIAN_POINT ( 'NONE',  ( 92.69370383062501162, -209.9999999999999716, 81.38781250086714181 ) ) ;
#31229 = DIRECTION ( 'NONE',  ( -1.000000000000000000, 0.000000000000000000, 0.000000000000000000 ) ) ;
#31230 = EDGE_CURVE ( 'NONE', #20377, #15161, #24014, .T. ) ;
#31231 = VERTEX_POINT ( 'NONE', #38495 ) ;
#31232 = DIRECTION ( 'NONE',  ( -1.000000000000000000, 0.000000000000000000, 0.000000000000000000 ) ) ;
#31233 = AXIS2_PLACEMENT_3D ( 'NONE', #1846, #7449, #12340 ) ;
#31234 = ORIENTED_EDGE ( 'NONE', *, *, #42684, .T. ) ;
#31235 = DIRECTION ( 'NONE',  ( -1.000000000000000000, 0.000000000000000000, 0.000000000000000000 ) ) ;
#31236 = EDGE_LOOP ( 'NONE', ( #45589, #44953, #15365, #34762 ) ) ;
#31237 = VECTOR ( 'NONE', #47214, 1000.000000000000000 ) ;
#31238 = CARTESIAN_POINT ( 'NONE',  ( -95.00000000000002842, 92.66308142843932671, 75.67281250086716682 ) ) ;
#31239 = ORIENTED_EDGE ( 'NONE', *, *, #5565, .F. ) ;
#31240 = EDGE_LOOP ( 'NONE', ( #5659, #27377, #24071, #49726 ) ) ;
#31241 = VECTOR ( 'NONE', #13535, 1000.000000000000000 ) ;
#31242 = LINE ( 'NONE', #64727, #65285 ) ;
#31243 = ORIENTED_EDGE ( 'NONE', *, *, #27484, .T. ) ;
#31244 = CARTESIAN_POINT ( 'NONE',  ( 0.000000000000000000, 10.30890764327382847, 81.34940948281339956 ) ) ;
#31245 = DIRECTION ( 'NONE',  ( -1.000000000000000000, -0.000000000000000000, 0.000000000000000000 ) ) ;
#31246 = EDGE_CURVE ( 'NONE', #62092, #14951, #61435, .T. ) ;
#31247 = ORIENTED_EDGE ( 'NONE', *, *, #72110, .T. ) ;
#31248 = DIRECTION ( 'NONE',  ( -1.000000000000000000, -0.000000000000000000, 0.000000000000000000 ) ) ;
#31249 = ORIENTED_EDGE ( 'NONE', *, *, #66628, .T. ) ;
#31250 = CARTESIAN_POINT ( 'NONE',  ( 93.67500000000001137, -212.2949673200287179, 86.29583333333333428 ) ) ;
#31251 = EDGE_CURVE ( 'NONE', #16009, #19127, #28780, .T. ) ;
#31252 = VERTEX_POINT ( 'NONE', #55038 ) ;
#31253 = ORIENTED_EDGE ( 'NONE', *, *, #13300, .T. ) ;
#31254 = ORIENTED_EDGE ( 'NONE', *, *, #5727, .F. ) ;
#31255 = CARTESIAN_POINT ( 'NONE',  ( 93.84685191531249870, -208.0026889286704943, 79.37697916753380412 ) ) ;
#31256 = VECTOR ( 'NONE', #15447, 1000.000000000000000 ) ;
#31257 = DIRECTION ( 'NONE',  ( -0.7273375899149793211, 0.6862798483830554463, 0.000000000000000000 ) ) ;
#31258 = CYLINDRICAL_SURFACE ( 'NONE', #63056, 2.649999999999985700 ) ;
#31259 = ORIENTED_EDGE ( 'NONE', *, *, #51550, .T. ) ;
#31260 = DIRECTION ( 'NONE',  ( 1.000000000000000000, 0.000000000000000000, -0.000000000000000000 ) ) ;
#31261 = EDGE_LOOP ( 'NONE', ( #24145, #38755 ) ) ;
#31262 = FACE_OUTER_BOUND ( 'NONE', #64185, .T. ) ;
#31263 = DIRECTION ( 'NONE',  ( -1.000000000000000000, -0.000000000000000000, -0.000000000000000000 ) ) ;
#31264 = DIRECTION ( 'NONE',  ( 0.000000000000000000, -0.4067366430758009854, 0.9135454576426004225 ) ) ;
#31265 = CIRCLE ( 'NONE', #46898, 31.99999999999998934 ) ;
#31266 = DIRECTION ( 'NONE',  ( -0.000000000000000000, 1.000000000000000000, -0.000000000000000000 ) ) ;
#31267 = CARTESIAN_POINT ( 'NONE',  ( -94.99999999999997158, -207.3369185715606307, 82.49906250086714010 ) ) ;
#31268 = CARTESIAN_POINT ( 'NONE',  ( -97.30629616937501680, 88.66845928578038638, 77.78947916753381264 ) ) ;
#31269 = ORIENTED_EDGE ( 'NONE', *, *, #62510, .T. ) ;
#31270 = CARTESIAN_POINT ( 'NONE',  ( 97.30629616937498838, 90.00000000000002842, 80.43531250086714124 ) ) ;
#31271 = ORIENTED_EDGE ( 'NONE', *, *, #10291, .T. ) ;
#31272 = CARTESIAN_POINT ( 'NONE',  ( 21.85433023846371370, -135.0628101570779620, 5.500000000000000000 ) ) ;
#31273 = DIRECTION ( 'NONE',  ( -0.000000000000000000, 0.8090169943749498938, -0.5877852522924696954 ) ) ;
#31274 = CARTESIAN_POINT ( 'NONE',  ( 10.00000000000000000, 66.50666863322000211, 39.78640506895629869 ) ) ;
#31275 = CARTESIAN_POINT ( 'NONE',  ( 10.00000000000000000, -14.66109333815410487, -73.73191006444587003 ) ) ;
#31276 = CARTESIAN_POINT ( 'NONE',  ( 10.00000000000000000, 0.000000000000000000, 0.000000000000000000 ) ) ;
#31277 = CARTESIAN_POINT ( 'NONE',  ( -96.15314808468745866, -211.9973110713294489, 81.49364583420047836 ) ) ;
#31278 = CARTESIAN_POINT ( 'NONE',  ( 94.99999999999998579, 86.94004357329502852, 86.98374999999998636 ) ) ;
#31279 = CARTESIAN_POINT ( 'NONE',  ( 11.99999999999999822, 58.39081064771822582, -50.95692526931267707 ) ) ;
#31280 = FACE_OUTER_BOUND ( 'NONE', #57463, .T. ) ;
#31281 = EDGE_LOOP ( 'NONE', ( #15439, #47407, #74060, #35837, #5469, #28886 ) ) ;
#31282 = ORIENTED_EDGE ( 'NONE', *, *, #40194, .T. ) ;
#31283 = CARTESIAN_POINT ( 'NONE',  ( 10.00000000000000000, -15.48615015657610883, 39.04073710021339139 ) ) ;
#31284 = CARTESIAN_POINT ( 'NONE',  ( -92.35000000000005116, 88.47002178664754979, 75.65958333333333030 ) ) ;
#31285 = LINE ( 'NONE', #26391, #73974 ) ;
#31286 = CARTESIAN_POINT ( 'NONE',  ( -93.84685191531254134, 91.99731107132950569, 85.62114583420046188 ) ) ;
#31287 = DIRECTION ( 'NONE',  ( -1.000000000000000000, 0.000000000000000000, 0.000000000000000000 ) ) ;
#31288 = DIRECTION ( 'NONE',  ( -1.000000000000000000, 0.000000000000000000, 0.000000000000000000 ) ) ;
#31289 = DIRECTION ( 'NONE',  ( 1.000000000000000000, -0.000000000000000000, 0.000000000000000000 ) ) ;
#31290 = ORIENTED_EDGE ( 'NONE', *, *, #40419, .T. ) ;
#31291 = CARTESIAN_POINT ( 'NONE',  ( -92.69370383062502583, 88.66845928578038638, 75.30239583420048177 ) ) ;
#31292 = EDGE_CURVE ( 'NONE', #60557, #45142, #50390, .T. ) ;
#31293 = VECTOR ( 'NONE', #73549, 1000.000000000000000 ) ;
#31294 = CIRCLE ( 'NONE', #6159, 82.00000000000000000 ) ;
#31295 = CARTESIAN_POINT ( 'NONE',  ( 10.00000000000000000, 16.45098606841173705, -33.79645857604496229 ) ) ;
#31296 = DIRECTION ( 'NONE',  ( -1.000000000000000000, 0.000000000000000000, 0.000000000000000000 ) ) ;
#31297 = DIRECTION ( 'NONE',  ( 1.000000000000000000, 0.000000000000000000, 0.000000000000000000 ) ) ;
#31298 = CARTESIAN_POINT ( 'NONE',  ( 92.35000000000000853, -209.9999999999999716, 84.92000000000000171 ) ) ;
#31299 = CARTESIAN_POINT ( 'NONE',  ( -92.69370383062498320, -208.6684592857803011, 81.28197916753381946 ) ) ;
#31300 = EDGE_CURVE ( 'NONE', #50488, #39943, #34796, .T. ) ;
#31301 = EDGE_CURVE ( 'NONE', #39300, #59025, #37220, .T. ) ;
#31302 = CARTESIAN_POINT ( 'NONE',  ( 5.999999999999999112, -67.80270845531921964, 46.11716303203162681 ) ) ;
#31303 = DIRECTION ( 'NONE',  ( 0.000000000000000000, 0.000000000000000000, 1.000000000000000000 ) ) ;
#31304 = CARTESIAN_POINT ( 'NONE',  ( 0.000000000000000000, 0.6853352020795618893, -37.58145647212453611 ) ) ;
#31305 = CARTESIAN_POINT ( 'NONE',  ( 16.30584220631899228, -140.9432449716519784, 5.500000000000000000 ) ) ;
#31306 = VECTOR ( 'NONE', #34911, 1000.000000000000000 ) ;
#31307 = VERTEX_POINT ( 'NONE', #61753 ) ;
#31308 = EDGE_CURVE ( 'NONE', #55937, #67975, #33526, .T. ) ;
#31309 = DIRECTION ( 'NONE',  ( -1.000000000000000000, -0.000000000000000000, -0.000000000000000000 ) ) ;
#31310 = CARTESIAN_POINT ( 'NONE',  ( 11.99999999999999822, 59.46389618802034960, -49.70050353004825894 ) ) ;
#31311 = DIRECTION ( 'NONE',  ( -1.000000000000000000, 0.000000000000000000, 0.000000000000000000 ) ) ;
#31312 = AXIS2_PLACEMENT_3D ( 'NONE', #31364, #8815, #14450 ) ;
#31313 = CIRCLE ( 'NONE', #37347, 77.49899999999999523 ) ;
#31314 = AXIS2_PLACEMENT_3D ( 'NONE', #44731, #3134, #38711 ) ;
#31315 = CARTESIAN_POINT ( 'NONE',  ( 10.00000000000000000, 0.000000000000000000, 0.000000000000000000 ) ) ;
#31316 = CARTESIAN_POINT ( 'NONE',  ( 92.69370383062501162, -208.6684592857803011, 87.84364583420048689 ) ) ;
#31317 = ORIENTED_EDGE ( 'NONE', *, *, #59623, .F. ) ;
#31318 = CARTESIAN_POINT ( 'NONE',  ( 92.35000000000000853, -209.9999999999999716, 87.45999999999999375 ) ) ;
#31319 = CARTESIAN_POINT ( 'NONE',  ( 0.000000000000000000, 16.00000000000000000, 2.500000000000000000 ) ) ;
#31320 = EDGE_CURVE ( 'NONE', #70347, #5816, #10231, .T. ) ;
#31321 = ORIENTED_EDGE ( 'NONE', *, *, #23041, .F. ) ;
#31322 = LINE ( 'NONE', #33913, #32781 ) ;
#31323 = EDGE_CURVE ( 'NONE', #32002, #20059, #15503, .T. ) ;
#31324 = EDGE_CURVE ( 'NONE', #14688, #17922, #26418, .T. ) ;
#31325 = ORIENTED_EDGE ( 'NONE', *, *, #29535, .T. ) ;
#31326 = DIRECTION ( 'NONE',  ( 0.000000000000000000, 0.8090169943749486725, -0.5877852522924714718 ) ) ;
#31327 = ORIENTED_EDGE ( 'NONE', *, *, #8646, .T. ) ;
#31328 = ORIENTED_EDGE ( 'NONE', *, *, #23923, .T. ) ;
#31329 = ORIENTED_EDGE ( 'NONE', *, *, #59831, .T. ) ;
#31330 = CARTESIAN_POINT ( 'NONE',  ( -95.00000000002611955, 90.00000000000007105, -75.00000000000000000 ) ) ;
#31331 = EDGE_CURVE ( 'NONE', #28882, #65467, #33605, .T. ) ;
#31332 = VERTEX_POINT ( 'NONE', #73751 ) ;
#31333 = PRODUCT_DEFINITION_SHAPE ( 'NONE', 'NONE',  #6784 ) ;
#31334 = ORIENTED_EDGE ( 'NONE', *, *, #71868, .T. ) ;
#31335 = CARTESIAN_POINT ( 'NONE',  ( 97.30629616937498838, 91.33154071421968467, 80.01197916753380923 ) ) ;
#31336 = DIRECTION ( 'NONE',  ( -1.000000000000000000, -0.000000000000000000, -0.000000000000000000 ) ) ;
#31337 = ORIENTED_EDGE ( 'NONE', *, *, #5800, .T. ) ;
#31338 = ORIENTED_EDGE ( 'NONE', *, *, #17898, .T. ) ;
#31339 = VECTOR ( 'NONE', #61082, 1000.000000000000000 ) ;
#31340 = CIRCLE ( 'NONE', #32521, 82.00000000000000000 ) ;
#31341 = VERTEX_POINT ( 'NONE', #72272 ) ;
#31342 = DIRECTION ( 'NONE',  ( -1.000000000000000000, 0.000000000000000000, 0.000000000000000000 ) ) ;
#31343 = AXIS2_PLACEMENT_3D ( 'NONE', #42770, #35279, #30729 ) ;
#31344 = ORIENTED_EDGE ( 'NONE', *, *, #4159, .T. ) ;
#31345 = DIRECTION ( 'NONE',  ( 0.000000000000000000, 0.000000000000000000, 1.000000000000000000 ) ) ;
#31346 = DIRECTION ( 'NONE',  ( 0.000000000000000000, 0.000000000000000000, 1.000000000000000000 ) ) ;
#31347 = CARTESIAN_POINT ( 'NONE',  ( 11.99999999999999822, -51.02545421589285723, -55.20638768913812555 ) ) ;
#31348 = FACE_OUTER_BOUND ( 'NONE', #38576, .T. ) ;
#31349 = CARTESIAN_POINT ( 'NONE',  ( -3.000000000000000000, -19.89357724624987256, -12.59942793731086041 ) ) ;
#31350 = CARTESIAN_POINT ( 'NONE',  ( -22.53294031248082163, -134.0273518838794757, -5.500000000000000000 ) ) ;
#31351 = CARTESIAN_POINT ( 'NONE',  ( 10.00000000000000000, 33.80338159004307386, -16.23288003029461279 ) ) ;
#31352 = CARTESIAN_POINT ( 'NONE',  ( -92.34999999999999432, -211.5299782133524502, 75.73895833506765030 ) ) ;
#31353 = CARTESIAN_POINT ( 'NONE',  ( -95.00000000000002842, 92.66308142843932671, 87.73781250086715033 ) ) ;
#31355 = CARTESIAN_POINT ( 'NONE',  ( -97.65000000000001990, 88.47002178664754979, 77.43229166840096411 ) ) ;
#31354 = CARTESIAN_POINT ( 'NONE',  ( 97.64999999999997726, 88.47002178664753558, 76.37395833506761278 ) ) ;
#31356 = EDGE_LOOP ( 'NONE', ( #60593, #47788 ) ) ;
#31357 = CARTESIAN_POINT ( 'NONE',  ( 92.69370383062498320, 88.66845928578037217, 77.15447916753382174 ) ) ;
#31358 = FACE_OUTER_BOUND ( 'NONE', #35056, .T. ) ;
#31359 = DIRECTION ( 'NONE',  ( -0.000000000000000000, 0.9510565162951539753, -0.3090169943749460635 ) ) ;
#31360 = FACE_OUTER_BOUND ( 'NONE', #128, .T. ) ;
#31361 = FACE_OUTER_BOUND ( 'NONE', #38289, .T. ) ;
#31362 = CARTESIAN_POINT ( 'NONE',  ( 5.000000000000000000, 60.67117009219135326, 55.16347631943062169 ) ) ;
#31363 = ORIENTED_EDGE ( 'NONE', *, *, #9273, .F. ) ;
#31364 = CARTESIAN_POINT ( 'NONE',  ( 11.99999999999999822, 0.000000000000000000, 0.000000000000000000 ) ) ;
#31365 = CIRCLE ( 'NONE', #71013, 12.50000000000000000 ) ;
#31366 = FACE_OUTER_BOUND ( 'NONE', #45339, .T. ) ;
#31367 = VERTEX_POINT ( 'NONE', #27893 ) ;
#31368 = CIRCLE ( 'NONE', #6178, 77.49899999999999523 ) ;
#31369 = VERTEX_POINT ( 'NONE', #61384 ) ;
#31370 = AXIS2_PLACEMENT_3D ( 'NONE', #37799, #8481, #31394 ) ;
#31371 = CARTESIAN_POINT ( 'NONE',  ( 0.000000000000000000, 0.000000000000000000, -43.79999999999998295 ) ) ;
#31372 = CARTESIAN_POINT ( 'NONE',  ( 0.000000000000000000, 0.000000000000000000, 0.000000000000000000 ) ) ;
#31373 = CARTESIAN_POINT ( 'NONE',  ( -10.00000000000000000, 0.000000000000000000, 0.000000000000000000 ) ) ;
#31374 = DIRECTION ( 'NONE',  ( -0.000000000000000000, -0.000000000000000000, -1.000000000000000000 ) ) ;
#31375 = DIRECTION ( 'NONE',  ( -1.000000000000000000, 0.000000000000000000, -0.000000000000000000 ) ) ;
#31376 = DIRECTION ( 'NONE',  ( 1.000000000000000000, -7.677074106448950501E-15, -2.598394312951952234E-14 ) ) ;
#31377 = ORIENTED_EDGE ( 'NONE', *, *, #11205, .F. ) ;
#31378 = EDGE_CURVE ( 'NONE', #35409, #30682, #38813, .T. ) ;
#31379 = LINE ( 'NONE', #54329, #6735 ) ;
#31380 = CARTESIAN_POINT ( 'NONE',  ( 0.000000000000000000, -0.8261519478425669583, -77.49459641780886443 ) ) ;
#31381 = EDGE_CURVE ( 'NONE', #55085, #10768, #68125, .T. ) ;
#31382 = DIRECTION ( 'NONE',  ( 0.000000000000000000, 0.2079116908177664758, 0.9781476007338042455 ) ) ;
#31383 = FACE_OUTER_BOUND ( 'NONE', #6244, .T. ) ;
#31384 = ADVANCED_FACE ( 'NONE', ( #33156 ), #73001, .F. ) ;
#31385 = DIRECTION ( 'NONE',  ( 0.000000000000000000, 0.000000000000000000, 1.000000000000000000 ) ) ;
#31386 = CARTESIAN_POINT ( 'NONE',  ( 92.35000000009274856, -209.9999861897330788, 80.55392363656960697 ) ) ;
#31387 = LINE ( 'NONE', #9204, #10964 ) ;
#31388 = EDGE_CURVE ( 'NONE', #71815, #53141, #4992, .T. ) ;
#31389 = LINE ( 'NONE', #54338, #8858 ) ;
#31390 = CARTESIAN_POINT ( 'NONE',  ( 10.00000000000000000, -20.40083707022935400, 72.35432306680478121 ) ) ;
#31391 = EDGE_CURVE ( 'NONE', #15350, #47006, #22265, .T. ) ;
#31392 = CARTESIAN_POINT ( 'NONE',  ( 93.84685191531248449, 91.99731107132950569, 83.34572916753383254 ) ) ;
#31393 = CARTESIAN_POINT ( 'NONE',  ( -97.30629616937497417, -211.3315407142195852, 84.77447916753381207 ) ) ;
#31394 = DIRECTION ( 'NONE',  ( -0.7273375899149793211, 0.6862798483830554463, 0.000000000000000000 ) ) ;
#31395 = ORIENTED_EDGE ( 'NONE', *, *, #52474, .F. ) ;
#31396 = EDGE_CURVE ( 'NONE', #18486, #28736, #29525, .T. ) ;
#31397 =( GEOMETRIC_REPRESENTATION_CONTEXT ( 3 ) GLOBAL_UNCERTAINTY_ASSIGNED_CONTEXT ( ( #39185 ) ) GLOBAL_UNIT_ASSIGNED_CONTEXT ( ( #30786, #19513, #13133 ) ) REPRESENTATION_CONTEXT ( 'NONE', 'WORKASPACE' ) );
#31398 = DIRECTION ( 'NONE',  ( 1.000000000000000000, 1.427937372958405461E-15, 7.962523111839130290E-16 ) ) ;
#31399 = AXIS2_PLACEMENT_3D ( 'NONE', #47826, #19620, #48928 ) ;
#31400 = CARTESIAN_POINT ( 'NONE',  ( -94.99999999999997158, -213.0599564267049857, 78.09374999999998579 ) ) ;
#31401 = CARTESIAN_POINT ( 'NONE',  ( 92.35000000000000853, -209.9999999999999716, 78.57000000000000739 ) ) ;
#31402 = AXIS2_PLACEMENT_3D ( 'NONE', #58959, #7448, #30362 ) ;
#31403 = AXIS2_PLACEMENT_3D ( 'NONE', #69216, #46285, #24458 ) ;
#31404 = CARTESIAN_POINT ( 'NONE',  ( 96.15314808468748708, -208.0026889286704943, 83.08114583420048405 ) ) ;
#31405 = ORIENTED_EDGE ( 'NONE', *, *, #14241, .F. ) ;
#31406 = CIRCLE ( 'NONE', #61427, 16.00000000000000000 ) ;
#31407 = CARTESIAN_POINT ( 'NONE',  ( 10.00000000000000000, -20.40083707022829174, -72.35432306680507963 ) ) ;
#31408 = ORIENTED_EDGE ( 'NONE', *, *, #41607, .T. ) ;
#31409 = EDGE_CURVE ( 'NONE', #23719, #68440, #20774, .T. ) ;
#31410 = ADVANCED_FACE ( 'NONE', ( #21502 ), #33124, .T. ) ;
#31411 = ORIENTED_EDGE ( 'NONE', *, *, #58858, .F. ) ;
#31412 = VECTOR ( 'NONE', #33489, 1000.000000000000000 ) ;
#31413 = DIRECTION ( 'NONE',  ( 0.000000000000000000, -0.8090169943749403458, -0.5877852522924830181 ) ) ;
#31414 = EDGE_CURVE ( 'NONE', #1375, #49986, #28295, .T. ) ;
#31415 = ADVANCED_FACE ( 'NONE', ( #49705 ), #4623, .T. ) ;
#31416 = VECTOR ( 'NONE', #2915, 1000.000000000000000 ) ;
#31417 = VECTOR ( 'NONE', #938, 1000.000000000000000 ) ;
#31418 = EDGE_LOOP ( 'NONE', ( #73230, #66321, #55777, #67952 ) ) ;
#31419 = CARTESIAN_POINT ( 'NONE',  ( -97.65000000002672209, -209.9999999999999147, -74.99999999999342037 ) ) ;
#31420 = CARTESIAN_POINT ( 'NONE',  ( 93.84685191531251292, -211.9973110713294489, 78.47739583420049314 ) ) ;
#31421 = DIRECTION ( 'NONE',  ( 0.000000000000000000, -0.7071067811865535679, 0.7071067811865413555 ) ) ;
#31422 = EDGE_CURVE ( 'NONE', #14697, #16651, #42749, .T. ) ;
#31423 = CARTESIAN_POINT ( 'NONE',  ( 11.99999999999999822, -6.903761155837269570, -77.19088730480530103 ) ) ;
#31424 =( BOUNDED_CURVE ( )  B_SPLINE_CURVE ( 2, ( #34302, #36426, #71366, #35681, #65390 ),
 .UNSPECIFIED., .F., .F. ) 
 B_SPLINE_CURVE_WITH_KNOTS ( ( 3, 2, 3 ),
 ( 0.9525283480321510288, 0.9595841135600021721, 0.9629953541049918186 ),
 .UNSPECIFIED. ) 
 CURVE ( )  GEOMETRIC_REPRESENTATION_ITEM ( )  RATIONAL_B_SPLINE_CURVE ( ( 1.000000000000000000, 0.8660254037844387076, 1.000000000000000000, 0.9352274998423498742, 0.9330859296547722170 ) ) 
 REPRESENTATION_ITEM ( '' )  );
#31425 = DIRECTION ( 'NONE',  ( -1.000000000000000000, 0.000000000000000000, -0.000000000000000000 ) ) ;
#31426 = FACE_OUTER_BOUND ( 'NONE', #57434, .T. ) ;
#31427 = CARTESIAN_POINT ( 'NONE',  ( -7.893099573151324044, -11.68370571044642503, -1.199999999999999956 ) ) ;
#31428 = CARTESIAN_POINT ( 'NONE',  ( 96.32499999999998863, -212.2949673200287179, 81.32166666666667254 ) ) ;
#31429 = EDGE_LOOP ( 'NONE', ( #59548, #14489, #68687, #6605 ) ) ;
#31430 = ORIENTED_EDGE ( 'NONE', *, *, #24602, .T. ) ;
#31431 = VERTEX_POINT ( 'NONE', #40669 ) ;
#31432 = ORIENTED_EDGE ( 'NONE', *, *, #23516, .T. ) ;
#31433 = DIRECTION ( 'NONE',  ( 1.000000000000000000, -0.000000000000000000, -0.000000000000000000 ) ) ;
#31434 = CARTESIAN_POINT ( 'NONE',  ( -92.69370383062504004, 90.00000000000004263, 83.13406250086715943 ) ) ;
#31435 = CARTESIAN_POINT ( 'NONE',  ( 0.000000000000000000, 3.894527615419058009, -81.90746397400384637 ) ) ;
#31436 = LINE ( 'NONE', #53635, #48626 ) ;
#31437 = CARTESIAN_POINT ( 'NONE',  ( 96.32499999999997442, 92.29496732002878900, 75.18333333333332291 ) ) ;
#31438 = CARTESIAN_POINT ( 'NONE',  ( 6.782329983125270800, 10.49999999999999467, -20.00000000000000000 ) ) ;
#31439 = ORIENTED_EDGE ( 'NONE', *, *, #48718, .T. ) ;
#31440 = CARTESIAN_POINT ( 'NONE',  ( -97.64999999999996305, -209.9999999999999716, 84.36437500173430237 ) ) ;
#31441 = VERTEX_POINT ( 'NONE', #16998 ) ;
#31442 = CYLINDRICAL_SURFACE ( 'NONE', #1476, 82.00000000000000000 ) ;
#31443 = EDGE_LOOP ( 'NONE', ( #59961, #42989, #15970, #353 ) ) ;
#31444 = CARTESIAN_POINT ( 'NONE',  ( -96.32500000000001705, 87.70503267997129626, 85.10520833506762983 ) ) ;
#31445 = EDGE_LOOP ( 'NONE', ( #71914, #49519 ) ) ;
#31446 = CARTESIAN_POINT ( 'NONE',  ( 92.69370383062498320, 91.33154071421968467, 85.93864583420048575 ) ) ;
#31447 = DIRECTION ( 'NONE',  ( -1.000000000000000000, -0.000000000000000000, 0.000000000000000000 ) ) ;
#31448 = PLANE ( 'NONE',  #19387 ) ;
#31449 = CARTESIAN_POINT ( 'NONE',  ( 0.000000000000000000, 0.000000000000000000, 0.000000000000000000 ) ) ;
#31450 = STYLED_ITEM ( 'NONE', ( #13638 ), #64162 ) ;
#31451 = AXIS2_PLACEMENT_3D ( 'NONE', #8258, #14264, #36455 ) ;
#31452 = DIRECTION ( 'NONE',  ( -1.000000000000000000, -0.000000000000000000, -0.000000000000000000 ) ) ;
#31453 = ORIENTED_EDGE ( 'NONE', *, *, #5534, .F. ) ;
#31454 = FACE_OUTER_BOUND ( 'NONE', #38542, .T. ) ;
#31455 = FACE_OUTER_BOUND ( 'NONE', #34266, .T. ) ;
#31456 = ORIENTED_EDGE ( 'NONE', *, *, #32048, .F. ) ;
#31457 = AXIS2_PLACEMENT_3D ( 'NONE', #21777, #43977, #49230 ) ;
#31458 = VERTEX_POINT ( 'NONE', #51195 ) ;
#31459 = DIRECTION ( 'NONE',  ( 0.000000000000000000, 0.000000000000000000, 1.000000000000000000 ) ) ;
#31460 = AXIS2_PLACEMENT_3D ( 'NONE', #12598, #58101, #63378 ) ;
#31461 = DIRECTION ( 'NONE',  ( 0.000000000000000000, 0.000000000000000000, 1.000000000000000000 ) ) ;
#31462 = CARTESIAN_POINT ( 'NONE',  ( -92.34999999999986642, -211.5299782133523649, 83.27958333333332064 ) ) ;
#31463 = AXIS2_PLACEMENT_3D ( 'NONE', #1717, #46811, #36253 ) ;
#31464 = CARTESIAN_POINT ( 'NONE',  ( -92.69370383062498320, -211.3315407142195852, 84.98614583420047097 ) ) ;
#31465 = ORIENTED_EDGE ( 'NONE', *, *, #37118, .F. ) ;
#31466 = ORIENTED_EDGE ( 'NONE', *, *, #52819, .T. ) ;
#31467 = ORIENTED_EDGE ( 'NONE', *, *, #28793, .F. ) ;
#31468 = ADVANCED_FACE ( 'NONE', ( #45585 ), #69959, .F. ) ;
#31469 = DIRECTION ( 'NONE',  ( 0.000000000000000000, 0.000000000000000000, 1.000000000000000000 ) ) ;
#31470 = AXIS2_PLACEMENT_3D ( 'NONE', #14827, #53956, #43436 ) ;
#31471 = CIRCLE ( 'NONE', #7443, 32.50000000000000000 ) ;
#31472 = CARTESIAN_POINT ( 'NONE',  ( 97.64999999999999147, 90.00000000000002842, 86.50750000000000739 ) ) ;
#31473 = EDGE_CURVE ( 'NONE', #23551, #65491, #5525, .T. ) ;
#31474 = CARTESIAN_POINT ( 'NONE',  ( 97.64999999999999147, -209.9999999999999716, 82.77687500173431090 ) ) ;
#31475 = CARTESIAN_POINT ( 'NONE',  ( 93.84685191531248449, 91.99731107132950569, 78.10697916753380809 ) ) ;
#31476 = DIRECTION ( 'NONE',  ( 1.000000000000000000, 0.000000000000000000, 0.000000000000000000 ) ) ;
#31477 = DIRECTION ( 'NONE',  ( 0.000000000000000000, 0.000000000000000000, 1.000000000000000000 ) ) ;
#31478 = DIRECTION ( 'NONE',  ( 0.000000000000000000, -0.7604059656000368150, 0.6494480483301767748 ) ) ;
#31479 = DIRECTION ( 'NONE',  ( 0.000000000000000000, -0.9969173337331287410, 0.07845909572783489605 ) ) ;
#31480 = EDGE_CURVE ( 'NONE', #7284, #27292, #21099, .T. ) ;
#31482 = EDGE_CURVE ( 'NONE', #49792, #15852, #15097, .T. ) ;
#31481 = CARTESIAN_POINT ( 'NONE',  ( -97.65000000000001990, 90.00000000000004263, 76.74437500173429783 ) ) ;
#31483 = DIRECTION ( 'NONE',  ( 1.000000000000000000, 0.000000000000000000, 0.000000000000000000 ) ) ;
#31484 = CYLINDRICAL_SURFACE ( 'NONE', #58862, 31.99999999999999289 ) ;
#31485 = DIRECTION ( 'NONE',  ( 0.000000000000000000, -0.4539904997395541875, 0.8910065241883642351 ) ) ;
#31486 = ORIENTED_EDGE ( 'NONE', *, *, #14749, .T. ) ;
#31487 = CARTESIAN_POINT ( 'NONE',  ( -97.30629616937501680, 91.33154071421968467, 81.96989583420047154 ) ) ;
#31488 = DIRECTION ( 'NONE',  ( -1.000000000000000000, 0.000000000000000000, 0.000000000000000000 ) ) ;
#31489 = ADVANCED_FACE ( 'NONE', ( #34275 ), #18106, .T. ) ;
#31490 = DIRECTION ( 'NONE',  ( 0.1850432970638656860, -0.9827303690289285187, 0.000000000000000000 ) ) ;
#31491 = ORIENTED_EDGE ( 'NONE', *, *, #53048, .T. ) ;
#31492 = CARTESIAN_POINT ( 'NONE',  ( 0.000000000000000000, -2.543863470248944214, 81.96053171279901051 ) ) ;
#31493 = DIRECTION ( 'NONE',  ( -1.000000000000000000, -0.000000000000000000, 0.000000000000000000 ) ) ;
#31494 = DIRECTION ( 'NONE',  ( -1.000000000000000000, 0.000000000000000000, 0.000000000000000000 ) ) ;
#31495 = ADVANCED_FACE ( 'NONE', ( #64345 ), #63239, .T. ) ;
#31496 = EDGE_CURVE ( 'NONE', #24127, #67018, #4339, .T. ) ;
#31497 = CARTESIAN_POINT ( 'NONE',  ( 92.69370383062501162, -209.9999999999999716, 79.64156250086715261 ) ) ;
#31498 = VECTOR ( 'NONE', #70576, 1000.000000000000000 ) ;
#31499 = ORIENTED_EDGE ( 'NONE', *, *, #67253, .T. ) ;
#31500 = ORIENTED_EDGE ( 'NONE', *, *, #45860, .T. ) ;
#31501 = CIRCLE ( 'NONE', #8715, 15.70000000000326956 ) ;
#31502 = DIRECTION ( 'NONE',  ( 0.000000000000000000, 0.7071067811865437980, 0.7071067811865512365 ) ) ;
#31503 = DIRECTION ( 'NONE',  ( 0.000000000000000000, 0.000000000000000000, 1.000000000000000000 ) ) ;
#31504 = AXIS2_PLACEMENT_3D ( 'NONE', #47642, #19062, #59671 ) ;
#31505 = DIRECTION ( 'NONE',  ( -1.000000000000000000, -0.000000000000000000, -0.000000000000000000 ) ) ;
#31506 = ORIENTED_EDGE ( 'NONE', *, *, #17470, .F. ) ;
#31507 =( LENGTH_UNIT ( ) NAMED_UNIT ( * ) SI_UNIT ( .MILLI., .METRE. ) );
#31508 = CARTESIAN_POINT ( 'NONE',  ( 96.15314808468748708, -208.0026889286704943, 76.25489583420049655 ) ) ;
#31509 = ORIENTED_EDGE ( 'NONE', *, *, #81, .F. ) ;
#31510 = CARTESIAN_POINT ( 'NONE',  ( 10.00000000000000000, 0.000000000000000000, 0.000000000000000000 ) ) ;
#31511 = ORIENTED_EDGE ( 'NONE', *, *, #26702, .F. ) ;
#31512 = CIRCLE ( 'NONE', #51968, 12.49999999999999645 ) ;
#31513 = ORIENTED_EDGE ( 'NONE', *, *, #40778, .T. ) ;
#31514 = CARTESIAN_POINT ( 'NONE',  ( -95.00000000000002842, 86.94004357329504273, 83.17374999999999829 ) ) ;
#31515 = AXIS2_PLACEMENT_3D ( 'NONE', #63587, #73720, #29339 ) ;
#31516 =( LENGTH_UNIT ( ) NAMED_UNIT ( * ) SI_UNIT ( .MILLI., .METRE. ) );
#31517 = CARTESIAN_POINT ( 'NONE',  ( -15.44521549751111422, -137.7748507232956001, 5.500000000000000000 ) ) ;
#31518 = ORIENTED_EDGE ( 'NONE', *, *, #27903, .F. ) ;
#31519 = DIRECTION ( 'NONE',  ( 0.000000000000000000, 0.3090169943749482839, -0.9510565162951533091 ) ) ;
#31520 = CARTESIAN_POINT ( 'NONE',  ( 97.64999999999999147, -209.9999999999999716, 82.14187500173429157 ) ) ;
#31521 = CARTESIAN_POINT ( 'NONE',  ( 97.64999999999997726, 91.52997821335252127, 85.29041666666665833 ) ) ;
#31522 = VERTEX_POINT ( 'NONE', #57957 ) ;
#31523 = CARTESIAN_POINT ( 'NONE',  ( -0.0004442498512760095037, 0.001194404164628348752, -49.00000000000000000 ) ) ;
#31524 = CARTESIAN_POINT ( 'NONE',  ( -100.0000000000000142, 95.00000000000002842, 90.00000000000000000 ) ) ;
#31525 = ORIENTED_EDGE ( 'NONE', *, *, #23762, .T. ) ;
#31526 = ORIENTED_EDGE ( 'NONE', *, *, #2992, .T. ) ;
#31527 = CARTESIAN_POINT ( 'NONE',  ( -96.15314808468751551, 88.00268892867056536, 87.36739583420049371 ) ) ;
#31528 = CARTESIAN_POINT ( 'NONE',  ( 94.99999999999998579, 92.66308142843935514, 83.13406250086714522 ) ) ;
#31529 = VERTEX_POINT ( 'NONE', #28631 ) ;
#31530 = CARTESIAN_POINT ( 'NONE',  ( 94.99999999999998579, 86.94004357329500010, 81.34812500173430294 ) ) ;
#31531 = DIRECTION ( 'NONE',  ( -1.000000000000000000, -0.000000000000000000, -0.000000000000000000 ) ) ;
#31532 = ORIENTED_EDGE ( 'NONE', *, *, #24472, .F. ) ;
#31533 = CARTESIAN_POINT ( 'NONE',  ( 92.35000000000000853, -209.9999999999999716, 77.93499999999998806 ) ) ;
#31534 = VERTEX_POINT ( 'NONE', #56852 ) ;
#31535 = ORIENTED_EDGE ( 'NONE', *, *, #70936, .F. ) ;
#31536 = EDGE_LOOP ( 'NONE', ( #27907, #9237, #2966, #68148 ) ) ;
#31537 = DIRECTION ( 'NONE',  ( 0.000000000000000000, 0.000000000000000000, 1.000000000000000000 ) ) ;
#31538 = CARTESIAN_POINT ( 'NONE',  ( 0.000000000000000000, 0.000000000000000000, 0.000000000000000000 ) ) ;
#31539 = CARTESIAN_POINT ( 'NONE',  ( -96.32500000000001705, 87.70503267997129626, 83.12083333333332291 ) ) ;
#31540 = ORIENTED_EDGE ( 'NONE', *, *, #16968, .F. ) ;
#31541 = CARTESIAN_POINT ( 'NONE',  ( 10.00000000000000000, -26.02418014898359289, 70.52718814184250107 ) ) ;
#31542 = FACE_OUTER_BOUND ( 'NONE', #55315, .T. ) ;
#31543 = VERTEX_POINT ( 'NONE', #34648 ) ;
#31544 = CARTESIAN_POINT ( 'NONE',  ( 11.99999999999999822, 62.20884554314085335, -46.21855187248562657 ) ) ;
#31545 = CARTESIAN_POINT ( 'NONE',  ( -94.99999999999997158, -212.6630814284392557, 79.00656250086713328 ) ) ;
#31546 = ORIENTED_EDGE ( 'NONE', *, *, #36170, .F. ) ;
#31547 = CARTESIAN_POINT ( 'NONE',  ( 10.00000000000000000, -55.20638768913724448, -51.02545421589383068 ) ) ;
#31548 = CARTESIAN_POINT ( 'NONE',  ( -0.2999999999999947153, 0.000000000000000000, -12.50000000000000000 ) ) ;
#31549 = DIRECTION ( 'NONE',  ( -1.000000000000000000, 0.000000000000000000, 0.000000000000000000 ) ) ;
#31550 = CARTESIAN_POINT ( 'NONE',  ( 0.000000000000000000, 60.67117009219215618, -55.16347631942977614 ) ) ;
#31551 = PRODUCT_DEFINITION ( 'UNKNOWN', '', #58026, #31850 ) ;
#31552 = ADVANCED_FACE ( 'NONE', ( #12451 ), #24125, .T. ) ;
#31553 = DIRECTION ( 'NONE',  ( -0.000000000000000000, 0.9781476007338069101, -0.2079116908177532363 ) ) ;
#31554 = AXIS2_PLACEMENT_3D ( 'NONE', #7684, #48649, #8435 ) ;
#31555 = EDGE_CURVE ( 'NONE', #2973, #2485, #57220, .T. ) ;
#31556 = PRESENTATION_STYLE_ASSIGNMENT (( #41377 ) ) ;
#31557 = LINE ( 'NONE', #1931, #68458 ) ;
#31558 = DIRECTION ( 'NONE',  ( -0.3853207896976523772, 0.9227826878668550226, 0.000000000000000000 ) ) ;
#31559 = SHAPE_REPRESENTATION ( 'small gear_ISO - Spur gear 2M 40T 20PA 10FW ---S40A75H50L20.0N', ( #43395 ), #59053 ) ;
#31560 = CARTESIAN_POINT ( 'NONE',  ( -93.67500000000003979, 92.29496732002878900, 88.59770833506763665 ) ) ;
#31562 = ADVANCED_FACE ( 'NONE', ( #5731 ), #69604, .T. ) ;
#31561 = DIRECTION ( 'NONE',  ( -1.000000000000000000, 0.000000000000000000, -0.000000000000000000 ) ) ;
#31563 = CARTESIAN_POINT ( 'NONE',  ( -92.69370383062504004, 90.00000000000004263, 76.62531250086713897 ) ) ;
#31564 = DIRECTION ( 'NONE',  ( 0.000000000000000000, 0.8660254037844432595, 0.4999999999999919509 ) ) ;
#31565 = LINE ( 'NONE', #1939, #38657 ) ;
#31566 = CIRCLE ( 'NONE', #59168, 12.49999999999999645 ) ;
#31567 = LINE ( 'NONE', #15019, #16342 ) ;
#31568 = EDGE_CURVE ( 'NONE', #45157, #65293, #66739, .T. ) ;
#31569 = CARTESIAN_POINT ( 'NONE',  ( -2.499999999999973355, 65.00000000000000000, -290.0000000000000568 ) ) ;
#31570 = AXIS2_PLACEMENT_3D ( 'NONE', #71406, #43971, #54504 ) ;
#31571 = CARTESIAN_POINT ( 'NONE',  ( 0.000000000000000000, -75.11764819372145041, 29.05362095685286050 ) ) ;
#31572 = DIRECTION ( 'NONE',  ( 0.000000000000000000, 0.000000000000000000, 1.000000000000000000 ) ) ;
#31573 = AXIS2_PLACEMENT_3D ( 'NONE', #24371, #69852, #41294 ) ;
#31574 = CYLINDRICAL_SURFACE ( 'NONE', #25075, 31.99999999999999289 ) ;
#31575 = CARTESIAN_POINT ( 'NONE',  ( 11.99999999999999822, 20.40083707022882820, 72.35432306680490910 ) ) ;
#31576 = CARTESIAN_POINT ( 'NONE',  ( -93.67499999999998295, -207.7050326799711968, 89.15333333333333599 ) ) ;
#31577 = ADVANCED_FACE ( 'NONE', ( #6101 ), #22300, .F. ) ;
#31578 = DIRECTION ( 'NONE',  ( 0.000000000000000000, -0.5000000000000046629, 0.8660254037844359321 ) ) ;
#31579 = EDGE_CURVE ( 'NONE', #32561, #1816, #72718, .T. ) ;
#31580 = ORIENTED_EDGE ( 'NONE', *, *, #1333, .T. ) ;
#31581 = CYLINDRICAL_SURFACE ( 'NONE', #29920, 31.99999999999999289 ) ;
#31582 = CARTESIAN_POINT ( 'NONE',  ( -2.500000000000017319, -80.00000000000001421, -189.9999999999999147 ) ) ;
#31583 = CARTESIAN_POINT ( 'NONE',  ( 10.00000000000000000, -16.23288003029521320, 33.80338159004277543 ) ) ;
#31584 = LINE ( 'NONE', #59434, #64160 ) ;
#31585 = ADVANCED_FACE ( 'NONE', ( #46308 ), #69235, .F. ) ;
#31586 = ORIENTED_EDGE ( 'NONE', *, *, #1341, .T. ) ;
#31587 = CARTESIAN_POINT ( 'NONE',  ( 10.00000000000000000, -27.13269053701078448, -25.88420570971428702 ) ) ;
#31588 = CYLINDRICAL_SURFACE ( 'NONE', #13921, 77.49899999999999523 ) ;
#31589 = ORIENTED_EDGE ( 'NONE', *, *, #17479, .T. ) ;
#31590 =( REPRESENTATION_RELATIONSHIP ('NONE','NONE', #31117, #23457 ) REPRESENTATION_RELATIONSHIP_WITH_TRANSFORMATION ( #26358 )SHAPE_REPRESENTATION_RELATIONSHIP( ) );
#31591 = CIRCLE ( 'NONE', #42405, 2.650000000000540812 ) ;
#31592 = CARTESIAN_POINT ( 'NONE',  ( 92.69370383062501162, -208.6684592857803295, 81.96989583420047154 ) ) ;
#31593 = CARTESIAN_POINT ( 'NONE',  ( 97.30629616937498838, -211.3315407142195852, 87.52614583420049144 ) ) ;
#31594 = VERTEX_POINT ( 'NONE', #7563 ) ;
#31595 = CARTESIAN_POINT ( 'NONE',  ( 95.00000000000000000, -212.6630814284392557, 86.15031250086714465 ) ) ;
#31596 = AXIS2_PLACEMENT_3D ( 'NONE', #67791, #15163, #38480 ) ;
#31597 = ORIENTED_EDGE ( 'NONE', *, *, #63766, .F. ) ;
#31598 = DIRECTION ( 'NONE',  ( 0.000000000000000000, 0.000000000000000000, -1.000000000000000000 ) ) ;
#31599 = ORIENTED_EDGE ( 'NONE', *, *, #34150, .F. ) ;
#31600 = CARTESIAN_POINT ( 'NONE',  ( -92.69370383062504004, 90.00000000000004263, 78.68906250086715204 ) ) ;
#31601 = AXIS2_PLACEMENT_3D ( 'NONE', #72465, #8205, #14588 ) ;
#31602 = ORIENTED_EDGE ( 'NONE', *, *, #65911, .F. ) ;
#31603 = ORIENTED_EDGE ( 'NONE', *, *, #43251, .F. ) ;
#31604 = PLANE ( 'NONE',  #47312 ) ;
#31605 = ORIENTED_EDGE ( 'NONE', *, *, #64082, .F. ) ;
#31606 = DIRECTION ( 'NONE',  ( -1.000000000000000000, 0.000000000000000000, -0.000000000000000000 ) ) ;
#31607 = FILL_AREA_STYLE_COLOUR ( '', #8014 ) ;
#31608 = VERTEX_POINT ( 'NONE', #49896 ) ;
#31609 = CARTESIAN_POINT ( 'NONE',  ( -2.499999999999997780, 8.494897427831771708, 0.000000000000000000 ) ) ;
#31610 = AXIS2_PLACEMENT_3D ( 'NONE', #72009, #55474, #55095 ) ;
#31611 = ORIENTED_EDGE ( 'NONE', *, *, #5129, .F. ) ;
#31612 = DIRECTION ( 'NONE',  ( -0.000000000000000000, -0.000000000000000000, 1.000000000000000000 ) ) ;
#31613 = VECTOR ( 'NONE', #46118, 1000.000000000000000 ) ;
#31614 = ORIENTED_EDGE ( 'NONE', *, *, #35043, .T. ) ;
#31615 = ADVANCED_FACE ( 'NONE', ( #3704 ), #21317, .F. ) ;
#31616 = ORIENTED_EDGE ( 'NONE', *, *, #22568, .F. ) ;
#31617 = CIRCLE ( 'NONE', #14835, 37.49900000000001654 ) ;
#31618 = ORIENTED_EDGE ( 'NONE', *, *, #50081, .F. ) ;
#31619 = CARTESIAN_POINT ( 'NONE',  ( 92.69370383062501162, -211.3315407142195852, 78.90072916753381094 ) ) ;
#31620 = DIRECTION ( 'NONE',  ( -0.3311129884571281101, -0.9435911131814402886, 0.000000000000000000 ) ) ;
#31621 = VECTOR ( 'NONE', #49683, 1000.000000000000000 ) ;
#31622 = CARTESIAN_POINT ( 'NONE',  ( -92.34999999999999432, -210.0000000198591295, 85.95187500101400246 ) ) ;
#31623 = ORIENTED_EDGE ( 'NONE', *, *, #63134, .F. ) ;
#31624 = ORIENTED_EDGE ( 'NONE', *, *, #3434, .F. ) ;
#31625 = CARTESIAN_POINT ( 'NONE',  ( -3.000000000000000000, 0.000000000000000000, 0.000000000000000000 ) ) ;
#31626 = DIRECTION ( 'NONE',  ( -1.000000000000000000, -0.000000000000000000, -0.000000000000000000 ) ) ;
#31628 = ADVANCED_FACE ( 'NONE', ( #24480 ), #70320, .T. ) ;
#31627 = ORIENTED_EDGE ( 'NONE', *, *, #41029, .F. ) ;
#31629 = CARTESIAN_POINT ( 'NONE',  ( -97.64999999980591383, 89.99998015720542810, 86.27002759516649633 ) ) ;
#31630 = CARTESIAN_POINT ( 'NONE',  ( 10.00000000000000000, 0.000000000000000000, 0.000000000000000000 ) ) ;
#31631 = CARTESIAN_POINT ( 'NONE',  ( -97.30629616937497417, -208.6684592857803011, 79.42989583420046529 ) ) ;
#31632 = EDGE_CURVE ( 'NONE', #44223, #61399, #41505, .T. ) ;
#31633 = CARTESIAN_POINT ( 'NONE',  ( -92.69370383062502583, 88.66845928578038638, 77.36614583420048064 ) ) ;
#31634 = ORIENTED_EDGE ( 'NONE', *, *, #12280, .T. ) ;
#31635 = CARTESIAN_POINT ( 'NONE',  ( 96.15314808468748708, 88.00268892867053694, 79.05947916753380866 ) ) ;
#31636 = EDGE_LOOP ( 'NONE', ( #53365, #16729, #5320, #13114 ) ) ;
#31637 = LINE ( 'NONE', #54580, #8324 ) ;
#31638 = CARTESIAN_POINT ( 'NONE',  ( -94.99999999999997158, -212.6630814284392557, 88.53156250086713897 ) ) ;
#31639 = CARTESIAN_POINT ( 'NONE',  ( -97.64999999999996305, -209.9999999999999716, 76.66499999999999204 ) ) ;
#31640 = CARTESIAN_POINT ( 'NONE',  ( -3.000000000000000000, -25.60904388321925396, 6.976881207771172377 ) ) ;
#31641 = CARTESIAN_POINT ( 'NONE',  ( 10.00000000000000000, -16.23288003029521320, 33.80338159004277543 ) ) ;
#31642 = CARTESIAN_POINT ( 'NONE',  ( -94.99999999999997158, -207.3369185715606307, 83.13406250086714522 ) ) ;
#31643 = ADVANCED_FACE ( 'NONE', ( #43912 ), #22356, .F. ) ;
#31644 = DIRECTION ( 'NONE',  ( -0.000000000000000000, 0.9781476007338067991, 0.2079116908177533474 ) ) ;
#31645 = LINE ( 'NONE', #20375, #42702 ) ;
#31646 = PLANE ( 'NONE',  #5906 ) ;
#31647 = ORIENTED_EDGE ( 'NONE', *, *, #44257, .F. ) ;
#31648 = EDGE_LOOP ( 'NONE', ( #6404, #13062, #18858, #42146 ) ) ;
#31649 = PLANE ( 'NONE',  #14465 ) ;
#31650 = CARTESIAN_POINT ( 'NONE',  ( 26.09152095774781799, -124.8716048804687375, 5.500000000000000000 ) ) ;
#31651 = CARTESIAN_POINT ( 'NONE',  ( 0.000000000000000000, 0.000000000000000000, 0.000000000000000000 ) ) ;
#31652 = CARTESIAN_POINT ( 'NONE',  ( -96.15314808468752972, 91.99731107132950569, 85.72697916753379843 ) ) ;
#31653 = CARTESIAN_POINT ( 'NONE',  ( 10.00000000000000000, 33.79645857604513992, 16.45098606841138178 ) ) ;
#31654 = FACE_OUTER_BOUND ( 'NONE', #45974, .T. ) ;
#31655 = CARTESIAN_POINT ( 'NONE',  ( 10.00000000000000000, 0.000000000000000000, 0.000000000000000000 ) ) ;
#31656 =( BOUNDED_CURVE ( )  B_SPLINE_CURVE ( 2, ( #65985, #24999, #32482, #47933, #59593, #66712, #8462, #19356, #31742 ),
 .UNSPECIFIED., .F., .F. ) 
 B_SPLINE_CURVE_WITH_KNOTS ( ( 3, 2, 2, 2, 3 ),
 ( 0.08466915177892291033, 0.08466918649058885471, 0.09172495203147111587, 0.09878071757235337702, 0.1058364832022827828 ),
 .UNSPECIFIED. ) 
 CURVE ( )  GEOMETRIC_REPRESENTATION_ITEM ( )  RATIONAL_B_SPLINE_CURVE ( ( 0.9999986817990127452, 0.9999993408962638552, 1.000000000000000000, 0.8660254037844387076, 1.000000000000000000, 0.8660254037844387076, 1.000000000000000000, 0.8660254037844387076, 1.000000000000000000 ) ) 
 REPRESENTATION_ITEM ( '' )  );
#31657 = ADVANCED_FACE ( 'NONE', ( #43552 ), #30476, .T. ) ;
#31658 = ORIENTED_EDGE ( 'NONE', *, *, #35712, .T. ) ;
#31659 = CYLINDRICAL_SURFACE ( 'NONE', #65411, 15.80000000000028315 ) ;
#31660 = PRODUCT_DEFINITION_FORMATION_WITH_SPECIFIED_SOURCE ( 'ANY', '', #3780, .NOT_KNOWN. ) ;
#31661 = DIRECTION ( 'NONE',  ( -1.000000000000000000, 0.000000000000000000, -0.000000000000000000 ) ) ;
#31662 = AXIS2_PLACEMENT_3D ( 'NONE', #46142, #35217, #40126 ) ;
#31663 = DIRECTION ( 'NONE',  ( 0.000000000000000000, -0.7604059656000369261, 0.6494480483301766638 ) ) ;
#31664 = DIRECTION ( 'NONE',  ( 2.603472992746261562E-14, 2.546204323184492723E-14, -1.000000000000000000 ) ) ;
#31665 = CARTESIAN_POINT ( 'NONE',  ( 10.00000000000000000, 0.000000000000000000, 0.000000000000000000 ) ) ;
#31666 = DIRECTION ( 'NONE',  ( 0.000000000000000000, 0.000000000000000000, 1.000000000000000000 ) ) ;
#31667 = CARTESIAN_POINT ( 'NONE',  ( -96.15314808468747287, -208.0026889286704943, 83.98072916753382344 ) ) ;
#31668 = EDGE_CURVE ( 'NONE', #17876, #50235, #9093, .T. ) ;
#31669 = CARTESIAN_POINT ( 'NONE',  ( 0.000000000000000000, 0.000000000000000000, 0.000000000000000000 ) ) ;
#31670 = EDGE_CURVE ( 'NONE', #53075, #56256, #36727, .T. ) ;
#31671 = AXIS2_PLACEMENT_3D ( 'NONE', #42909, #36509, #30859 ) ;
#31672 = EDGE_CURVE ( 'NONE', #26258, #70972, #21112, .T. ) ;
#31673 = CIRCLE ( 'NONE', #26891, 2.500000000000000444 ) ;
#31674 = DIRECTION ( 'NONE',  ( 0.000000000000000000, 0.000000000000000000, 1.000000000000000000 ) ) ;
#31675 = DIRECTION ( 'NONE',  ( -1.000000000000000000, 0.000000000000000000, 0.000000000000000000 ) ) ;
#31676 = DIRECTION ( 'NONE',  ( 0.000000000000000000, -0.000000000000000000, 1.000000000000000000 ) ) ;
#31677 = ORIENTED_EDGE ( 'NONE', *, *, #55750, .T. ) ;
#31678 = CARTESIAN_POINT ( 'NONE',  ( 95.00000000000000000, -209.9999999999999716, 90.00000000000000000 ) ) ;
#31679 = DIRECTION ( 'NONE',  ( -0.000000000000000000, -0.000000000000000000, 1.000000000000000000 ) ) ;
#31680 = CARTESIAN_POINT ( 'NONE',  ( -12.75000000000000000, -120.0000000000000000, -80.00000000000001421 ) ) ;
#31681 = CIRCLE ( 'NONE', #29309, 82.00000000000000000 ) ;
#31682 = CIRCLE ( 'NONE', #19659, 15.99999999999999822 ) ;
#31683 = DIRECTION ( 'NONE',  ( -0.000000000000000000, -0.000000000000000000, 1.000000000000000000 ) ) ;
#31684 = ORIENTED_EDGE ( 'NONE', *, *, #35099, .T. ) ;
#31685 = CARTESIAN_POINT ( 'NONE',  ( 92.35000000003284981, 90.00000839192529156, 86.90410584365271518 ) ) ;
#31686 = CARTESIAN_POINT ( 'NONE',  ( 10.00000000000000000, 59.46389618801964616, 49.70050353004912580 ) ) ;
#31687 = EDGE_LOOP ( 'NONE', ( #35689, #43999, #15895, #39129, #16348 ) ) ;
#31688 = CARTESIAN_POINT ( 'NONE',  ( -97.64999999978461176, -209.9999789922612479, 79.91868729551984529 ) ) ;
#31689 = ORIENTED_EDGE ( 'NONE', *, *, #24306, .F. ) ;
#31690 = AXIS2_PLACEMENT_3D ( 'NONE', #6138, #40707, #69996 ) ;
#31691 = CARTESIAN_POINT ( 'NONE',  ( 4.999999999999999112, 36.13751322684449008, -21.40280677340332716 ) ) ;
#31692 = ORIENTED_EDGE ( 'NONE', *, *, #72608, .F. ) ;
#31693 = ORIENTED_EDGE ( 'NONE', *, *, #74029, .T. ) ;
#31694 = ORIENTED_EDGE ( 'NONE', *, *, #52022, .F. ) ;
#31695 = ORIENTED_EDGE ( 'NONE', *, *, #69035, .T. ) ;
#31696 = DIRECTION ( 'NONE',  ( -0.000000000000000000, -0.000000000000000000, 1.000000000000000000 ) ) ;
#31697 = ORIENTED_EDGE ( 'NONE', *, *, #30623, .F. ) ;
#31698 = AXIS2_PLACEMENT_3D ( 'NONE', #13437, #41635, #18335 ) ;
#31699 = ORIENTED_EDGE ( 'NONE', *, *, #15515, .F. ) ;
#31700 = CARTESIAN_POINT ( 'NONE',  ( 92.69370383062498320, 90.00000000000002842, 79.00656250086716170 ) ) ;
#31701 = DIRECTION ( 'NONE',  ( -1.000000000000000000, 0.000000000000000000, 0.000000000000000000 ) ) ;
#31702 = DIRECTION ( 'NONE',  ( 0.000000000000000000, 0.000000000000000000, 1.000000000000000000 ) ) ;
#31703 = ORIENTED_EDGE ( 'NONE', *, *, #6562, .F. ) ;
#31704 = ORIENTED_EDGE ( 'NONE', *, *, #33536, .F. ) ;
#31705 = ADVANCED_FACE ( 'NONE', ( #42154 ), #26599, .T. ) ;
#31706 = ORIENTED_EDGE ( 'NONE', *, *, #38596, .T. ) ;
#31707 = DIRECTION ( 'NONE',  ( 0.000000000000000000, 0.000000000000000000, 1.000000000000000000 ) ) ;
#31708 = VERTEX_POINT ( 'NONE', #47414 ) ;
#31709 = AXIS2_PLACEMENT_3D ( 'NONE', #38373, #21429, #3080 ) ;
#31710 = DIRECTION ( 'NONE',  ( 0.000000000000000000, 0.000000000000000000, 0.9999999999999998890 ) ) ;
#31711 = DIRECTION ( 'NONE',  ( -0.000000000000000000, -0.6691306063588570163, 0.7431448254773953543 ) ) ;
#31712 = CARTESIAN_POINT ( 'NONE',  ( -3.000000000000000000, 23.50000000000000000, -1.500000000000001332 ) ) ;
#31713 = CARTESIAN_POINT ( 'NONE',  ( -12.49999999999999645, 1.530808498934191127E-15, -175.0000000000000000 ) ) ;
#31714 = CARTESIAN_POINT ( 'NONE',  ( 0.000000000000000000, 0.000000000000000000, 0.000000000000000000 ) ) ;
#31715 = EDGE_CURVE ( 'NONE', #1727, #1450, #60737, .T. ) ;
#31716 = DIRECTION ( 'NONE',  ( 0.000000000000000000, 0.000000000000000000, 1.000000000000000000 ) ) ;
#31717 = DIRECTION ( 'NONE',  ( -1.000000000000000000, 0.000000000000000000, 0.000000000000000000 ) ) ;
#31718 = CARTESIAN_POINT ( 'NONE',  ( -94.99999999999997158, -213.0599564267049857, 76.26812500173430465 ) ) ;
#31719 = EDGE_CURVE ( 'NONE', #40423, #44983, #63157, .T. ) ;
#31720 = CARTESIAN_POINT ( 'NONE',  ( -97.30629616937501680, 91.33154071421968467, 89.74864583420048803 ) ) ;
#31721 = EDGE_LOOP ( 'NONE', ( #46454, #25586, #32783, #6204 ) ) ;
#31723 = CARTESIAN_POINT ( 'NONE',  ( -97.30629616937501680, 91.33154071421968467, 87.68489583420047495 ) ) ;
#31722 = CARTESIAN_POINT ( 'NONE',  ( 96.32499999999997442, 92.29496732002878900, 74.62770833506762358 ) ) ;
#31724 = AXIS2_PLACEMENT_3D ( 'NONE', #7493, #30403, #1887 ) ;
#31725 = ORIENTED_EDGE ( 'NONE', *, *, #46196, .T. ) ;
#31726 = CARTESIAN_POINT ( 'NONE',  ( 93.84685191531248449, 88.00268892867053694, 75.93739583420048689 ) ) ;
#31727 = VECTOR ( 'NONE', #30472, 1000.000000000000000 ) ;
#31728 = DIRECTION ( 'NONE',  ( -1.000000000000000000, -0.000000000000000000, -0.000000000000000000 ) ) ;
#31729 = CARTESIAN_POINT ( 'NONE',  ( 97.64999999999997726, -211.5299782133524218, 87.72458333333332803 ) ) ;
#31730 = CARTESIAN_POINT ( 'NONE',  ( 10.00000000000000000, 0.000000000000000000, 0.000000000000000000 ) ) ;
#31731 = CARTESIAN_POINT ( 'NONE',  ( -95.00000000000002842, 93.05995642670504253, 78.49062500173430124 ) ) ;
#31732 = CARTESIAN_POINT ( 'NONE',  ( -10.00000000000000000, 0.000000000000000000, 0.000000000000000000 ) ) ;
#31733 = EDGE_CURVE ( 'NONE', #48642, #30113, #11505, .T. ) ;
#31735 = LINE ( 'NONE', #8071, #1377 ) ;
#31734 = VECTOR ( 'NONE', #26760, 1000.000000000000114 ) ;
#31736 = CYLINDRICAL_SURFACE ( 'NONE', #68309, 16.00000000000000000 ) ;
#31737 = ORIENTED_EDGE ( 'NONE', *, *, #13085, .T. ) ;
#31738 = ORIENTED_EDGE ( 'NONE', *, *, #25485, .T. ) ;
#31739 = CIRCLE ( 'NONE', #68847, 10.00000000000000178 ) ;
#31740 = DIRECTION ( 'NONE',  ( -1.000000000000000000, 0.000000000000000000, 0.000000000000000000 ) ) ;
#31741 = DIRECTION ( 'NONE',  ( -1.000000000000000000, 0.000000000000000000, 0.000000000000000000 ) ) ;
#31742 = CARTESIAN_POINT ( 'NONE',  ( 97.64999999999999147, -210.0000000334413244, 87.85687500050293863 ) ) ;
#31743 = AXIS2_PLACEMENT_3D ( 'NONE', #31135, #55557, #20968 ) ;
#31744 = LINE ( 'NONE', #47934, #36356 ) ;
#31745 = CARTESIAN_POINT ( 'NONE',  ( 0.000000000000000000, 0.000000000000000000, -54.99999999999998579 ) ) ;
#31746 = CARTESIAN_POINT ( 'NONE',  ( -92.69370383062498320, -208.6684592857803011, 75.56697916753383026 ) ) ;
#31747 = ADVANCED_FACE ( 'NONE', ( #7192 ), #30108, .F. ) ;
#31748 = ORIENTED_EDGE ( 'NONE', *, *, #58478, .T. ) ;
#31749 = CARTESIAN_POINT ( 'NONE',  ( -93.84685191531252713, 88.00268892867056536, 82.86947916753379673 ) ) ;
#31750 = DIRECTION ( 'NONE',  ( -8.326672684688524170E-16, -1.065814103640131188E-14, -1.000000000000000000 ) ) ;
#31751 = CYLINDRICAL_SURFACE ( 'NONE', #51083, 2.649999999999985700 ) ;
#31752 = CARTESIAN_POINT ( 'NONE',  ( 0.000000000000000000, 29.81001611431041098, -22.74946021919100403 ) ) ;
#31753 = DIRECTION ( 'NONE',  ( -1.000000000000000000, -0.000000000000000000, 0.000000000000000000 ) ) ;
#31754 = DIRECTION ( 'NONE',  ( -1.000000000000000000, 0.000000000000000000, 0.000000000000000000 ) ) ;
#31755 = CARTESIAN_POINT ( 'NONE',  ( -94.99999999999997158, -206.9400435732949575, 87.30124999999999602 ) ) ;
#31756 = LINE ( 'NONE', #60723, #73358 ) ;
#31757 = DIRECTION ( 'NONE',  ( -1.000000000000000000, -7.616308197389468785E-15, 2.603472992745757322E-14 ) ) ;
#31758 = CARTESIAN_POINT ( 'NONE',  ( 0.000000000000000000, 0.000000000000000000, 0.000000000000000000 ) ) ;
#31759 = EDGE_CURVE ( 'NONE', #46309, #31608, #49166, .T. ) ;
#31760 = EDGE_CURVE ( 'NONE', #5511, #58272, #49918, .T. ) ;
#31761 = CARTESIAN_POINT ( 'NONE',  ( 94.99999999999998579, 87.33691857156068750, 85.51531250086715374 ) ) ;
#31762 = CARTESIAN_POINT ( 'NONE',  ( -92.69370383062498320, -208.6684592857803295, 83.18697916753382060 ) ) ;
#31763 = CARTESIAN_POINT ( 'NONE',  ( 94.99999999999998579, 90.00000000000002842, 90.00000000000000000 ) ) ;
#31764 = VERTEX_POINT ( 'NONE', #28829 ) ;
#31765 = CARTESIAN_POINT ( 'NONE',  ( -6.719258119307966126, -15.35072898742050462, -1.199999999999999956 ) ) ;
#31766 = CARTESIAN_POINT ( 'NONE',  ( -92.34999999999999432, -211.5299782133524502, 78.19958333333332234 ) ) ;
#31767 = CYLINDRICAL_SURFACE ( 'NONE', #61752, 11.59999999999999964 ) ;
#31768 = AXIS2_PLACEMENT_3D ( 'NONE', #32254, #14603, #26621 ) ;
#31769 = CARTESIAN_POINT ( 'NONE',  ( 93.84685191531251292, -211.9973110713294489, 82.76364583420047438 ) ) ;
#31770 = ORIENTED_EDGE ( 'NONE', *, *, #74103, .F. ) ;
#31771 = DIRECTION ( 'NONE',  ( 0.000000000000000000, -0.8090169943749531134, 0.5877852522924653655 ) ) ;
#31772 = VERTEX_POINT ( 'NONE', #310 ) ;
#31773 = AXIS2_PLACEMENT_3D ( 'NONE', #6012, #11994, #34188 ) ;
#31774 = CARTESIAN_POINT ( 'NONE',  ( 11.99999999999999822, 0.000000000000000000, 0.000000000000000000 ) ) ;
#31775 = AXIS2_PLACEMENT_3D ( 'NONE', #22676, #1269, #56892 ) ;
#31776 = VERTEX_POINT ( 'NONE', #5181 ) ;
#31777 = DIRECTION ( 'NONE',  ( -0.4415113423096792000, 0.000000000000000000, -0.8972556684757725387 ) ) ;
#31778 = ORIENTED_EDGE ( 'NONE', *, *, #28020, .T. ) ;
#31779 = CARTESIAN_POINT ( 'NONE',  ( 95.00000000000000000, -207.3369185715606307, 76.94281250086714863 ) ) ;
#31780 = CARTESIAN_POINT ( 'NONE',  ( 10.00000000000000000, -35.38097989696503021, -12.42422080174676147 ) ) ;
#31782 = CARTESIAN_POINT ( 'NONE',  ( 20.85212586905262100, -130.9402397935870965, -5.500000000000000000 ) ) ;
#31781 = AXIS2_PLACEMENT_3D ( 'NONE', #3552, #27176, #38103 ) ;
#31783 = EDGE_CURVE ( 'NONE', #44748, #25853, #43751, .T. ) ;
#31784 = DIRECTION ( 'NONE',  ( -1.000000000000000000, -0.000000000000000000, 0.000000000000000000 ) ) ;
#31785 = CARTESIAN_POINT ( 'NONE',  ( 0.000000000000000000, -37.22597642581153821, -5.202137450156795850 ) ) ;
#31786 = CARTESIAN_POINT ( 'NONE',  ( -92.35000000000005116, 88.47002178664754979, 83.35895833506764063 ) ) ;
#31787 = CARTESIAN_POINT ( 'NONE',  ( 95.00000000000000000, -213.0599564267049857, 82.53874999999999318 ) ) ;
#31788 = AXIS2_PLACEMENT_3D ( 'NONE', #28034, #50975, #68276 ) ;
#31789 = EDGE_CURVE ( 'NONE', #26822, #52685, #27720, .T. ) ;
#31790 = ORIENTED_EDGE ( 'NONE', *, *, #30298, .T. ) ;
#31791 = ORIENTED_EDGE ( 'NONE', *, *, #15651, .F. ) ;
#31792 = ORIENTED_EDGE ( 'NONE', *, *, #31067, .T. ) ;
#31793 = ORIENTED_EDGE ( 'NONE', *, *, #43736, .F. ) ;
#31794 = CARTESIAN_POINT ( 'NONE',  ( -92.34999999999999432, -211.5299782133524218, 86.53395833506763779 ) ) ;
#31795 = EDGE_CURVE ( 'NONE', #2080, #3079, #59120, .T. ) ;
#31796 =( NAMED_UNIT ( * ) PLANE_ANGLE_UNIT ( ) SI_UNIT ( $, .RADIAN. ) );
#31797 = CARTESIAN_POINT ( 'NONE',  ( -93.84685191531254134, 91.99731107132950569, 85.14489583420048291 ) ) ;
#31798 = CARTESIAN_POINT ( 'NONE',  ( 11.99999999999999822, 46.21855187248719687, -62.20884554313968806 ) ) ;
#31799 = CARTESIAN_POINT ( 'NONE',  ( -3.000000000000000000, 0.000000000000000000, 0.000000000000000000 ) ) ;
#31800 = ADVANCED_FACE ( 'NONE', ( #17186, #11172 ), #10423, .F. ) ;
#31801 = DIRECTION ( 'NONE',  ( 0.000000000000000000, -0.6691306063588661202, -0.7431448254773871387 ) ) ;
#31802 = CARTESIAN_POINT ( 'NONE',  ( -93.67499999999998295, -212.2949673200287179, 83.94104166840097037 ) ) ;
#31803 = ORIENTED_EDGE ( 'NONE', *, *, #69333, .T. ) ;
#31804 = CARTESIAN_POINT ( 'NONE',  ( -94.99999999999997158, -213.0599564267049857, 85.79312500173431033 ) ) ;
#31805 = ORIENTED_EDGE ( 'NONE', *, *, #68449, .T. ) ;
#31806 = CARTESIAN_POINT ( 'NONE',  ( 0.000000000000000000, 16.23288003029543347, -33.80338159004267595 ) ) ;
#31807 = ORIENTED_EDGE ( 'NONE', *, *, #43066, .T. ) ;
#31808 = CARTESIAN_POINT ( 'NONE',  ( -97.65000000000001990, 90.00000000000004263, 84.36437500173430237 ) ) ;
#31809 = ORIENTED_EDGE ( 'NONE', *, *, #56706, .F. ) ;
#31810 = CARTESIAN_POINT ( 'NONE',  ( 92.69370383062498320, 88.66845928578037217, 87.94947916753382344 ) ) ;
#31811 = DIRECTION ( 'NONE',  ( -0.000000000000000000, -0.000000000000000000, 1.000000000000000000 ) ) ;
#31812 = CARTESIAN_POINT ( 'NONE',  ( 10.00000000000000000, -55.38113227695743745, -54.21277698773734244 ) ) ;
#31813 = DIRECTION ( 'NONE',  ( 1.000000000000000000, 0.000000000000000000, 0.000000000000000000 ) ) ;
#31814 = LINE ( 'NONE', #65678, #49822 ) ;
#31815 = EDGE_CURVE ( 'NONE', #69665, #6591, #38638, .T. ) ;
#31816 = DIRECTION ( 'NONE',  ( -1.000000000000000000, 0.000000000000000000, 0.000000000000000000 ) ) ;
#31817 = ORIENTED_EDGE ( 'NONE', *, *, #19629, .F. ) ;
#31818 = CARTESIAN_POINT ( 'NONE',  ( -95.00000000000002842, 93.05995642670504253, 81.03062500173430749 ) ) ;
#31819 = CARTESIAN_POINT ( 'NONE',  ( 0.000000000000000000, 0.8660254037844389297, -1.500000000000000000 ) ) ;
#31820 = AXIS2_PLACEMENT_3D ( 'NONE', #20149, #2908, #43851 ) ;
#31821 = VERTEX_POINT ( 'NONE', #73568 ) ;
#31822 = EDGE_LOOP ( 'NONE', ( #29977, #15480, #29775, #25034 ) ) ;
#31823 = CARTESIAN_POINT ( 'NONE',  ( 2.500000000000034639, 90.00000000000000000, -310.0000000000000000 ) ) ;
#31824 = FACE_OUTER_BOUND ( 'NONE', #26345, .T. ) ;
#31825 = EDGE_CURVE ( 'NONE', #19590, #60096, #28085, .T. ) ;
#31826 = DIRECTION ( 'NONE',  ( -1.000000000000000000, 0.000000000000000000, 0.000000000000000000 ) ) ;
#31827 = CARTESIAN_POINT ( 'NONE',  ( -97.30629616937497417, -208.6684592857803011, 83.39864583420050792 ) ) ;
#31828 = VERTEX_POINT ( 'NONE', #22836 ) ;
#31829 = VECTOR ( 'NONE', #19020, 1000.000000000000000 ) ;
#31830 = CARTESIAN_POINT ( 'NONE',  ( 97.65000000000004832, -211.5299782133523934, 81.37458333333333371 ) ) ;
#31831 = EDGE_CURVE ( 'NONE', #61902, #56093, #17916, .T. ) ;
#31832 = CIRCLE ( 'NONE', #34256, 12.49999999999999645 ) ;
#31833 = EDGE_LOOP ( 'NONE', ( #29327, #49092, #19847, #862 ) ) ;
#31834 = EDGE_CURVE ( 'NONE', #14575, #49911, #65789, .T. ) ;
#31835 = CARTESIAN_POINT ( 'NONE',  ( 97.64999999964362587, 89.99995654222556141, 89.12687334326064104 ) ) ;
#31836 = EDGE_CURVE ( 'NONE', #48671, #59850, #52574, .T. ) ;
#31837 = AXIS2_PLACEMENT_3D ( 'NONE', #24385, #70222, #13465 ) ;
#31838 = CARTESIAN_POINT ( 'NONE',  ( 94.99999999999998579, 92.66308142843935514, 89.64281250086715147 ) ) ;
#31839 = DIRECTION ( 'NONE',  ( 0.000000000000000000, 0.000000000000000000, 1.000000000000000000 ) ) ;
#31840 = CARTESIAN_POINT ( 'NONE',  ( 96.15314808468748708, 88.00268892867053694, 79.69447916753379957 ) ) ;
#31841 = CARTESIAN_POINT ( 'NONE',  ( 1.250000000000000444, -16.78109714094927085, -1.199999999999999956 ) ) ;
#31842 = CARTESIAN_POINT ( 'NONE',  ( 11.99999999999999822, 71.91182617369230456, -28.89263327155667938 ) ) ;
#31843 = CIRCLE ( 'NONE', #27009, 77.49900000000000944 ) ;
#31844 = CARTESIAN_POINT ( 'NONE',  ( 15.00000000000000000, -14.54903810567644484, 22.19967320028775504 ) ) ;
#31845 = CARTESIAN_POINT ( 'NONE',  ( 0.000000000000000000, 0.000000000000000000, 0.000000000000000000 ) ) ;
#31846 = CARTESIAN_POINT ( 'NONE',  ( 100.0000000000260201, 95.00000000000001421, 74.99999999999998579 ) ) ;
#31847 = FACE_OUTER_BOUND ( 'NONE', #1073, .T. ) ;
#31848 = EDGE_CURVE ( 'NONE', #73707, #55862, #44660, .T. ) ;
#31849 = CARTESIAN_POINT ( 'NONE',  ( -92.69370383062494057, -209.7238243954290340, 74.79348190356849102 ) ) ;
#31850 = PRODUCT_DEFINITION_CONTEXT ( 'detailed design', #53241, 'design' ) ;
#31851 = AXIS2_PLACEMENT_3D ( 'NONE', #9916, #32837, #5419 ) ;
#31852 = EDGE_CURVE ( 'NONE', #31895, #26439, #8304, .T. ) ;
#31853 = CARTESIAN_POINT ( 'NONE',  ( -92.34999999999999432, -211.5299782133524218, 75.73895833506765030 ) ) ;
#31854 = ORIENTED_EDGE ( 'NONE', *, *, #24459, .F. ) ;
#31855 = CARTESIAN_POINT ( 'NONE',  ( -93.84685191531254134, 91.99731107132950569, 83.08114583420048405 ) ) ;
#31856 = DIRECTION ( 'NONE',  ( 0.000000000000000000, 0.9781476007338045786, -0.2079116908177641720 ) ) ;
#31857 = CIRCLE ( 'NONE', #73878, 16.00000000000000000 ) ;
#31858 = CYLINDRICAL_SURFACE ( 'NONE', #22271, 77.49899999999999523 ) ;
#31859 = CIRCLE ( 'NONE', #73462, 16.00000000000000355 ) ;
#31860 = ORIENTED_EDGE ( 'NONE', *, *, #17516, .T. ) ;
#31861 =( BOUNDED_CURVE ( )  B_SPLINE_CURVE ( 2, ( #71178, #48994, #60669, #24961, #59936, #8424, #70818, #66314, #8787 ),
 .UNSPECIFIED., .F., .F. ) 
 B_SPLINE_CURVE_WITH_KNOTS ( ( 3, 2, 2, 2, 3 ),
 ( 0.08466915177892317401, 0.08466918649058881308, 0.09172495203147107423, 0.09878071757235333539, 0.1058364832022826857 ),
 .UNSPECIFIED. ) 
 CURVE ( )  GEOMETRIC_REPRESENTATION_ITEM ( )  RATIONAL_B_SPLINE_CURVE ( ( 0.9999986817990245136, 0.9999993408962697394, 1.000000000000000000, 0.8660254037844387076, 1.000000000000000000, 0.8660254037844387076, 1.000000000000000000, 0.8660254037844387076, 1.000000000000000000 ) ) 
 REPRESENTATION_ITEM ( '' )  );
#31862 = DIRECTION ( 'NONE',  ( 0.000000000000000000, 0.000000000000000000, -1.000000000000000000 ) ) ;
#31863 = CARTESIAN_POINT ( 'NONE',  ( 92.35000000045006630, -210.0000310946952595, 88.81037122969986797 ) ) ;
#31864 = CARTESIAN_POINT ( 'NONE',  ( 96.90829729882861443, 88.16127723153182671, 74.99954709728268654 ) ) ;
#31865 = CARTESIAN_POINT ( 'NONE',  ( -997.5739745962155212, 0.000000000000000000, 0.000000000000000000 ) ) ;
#31866 = AXIS2_PLACEMENT_3D ( 'NONE', #28763, #24250, #1359 ) ;
#31867 = CARTESIAN_POINT ( 'NONE',  ( 95.00000000000000000, -207.3369185715606307, 78.21281250086717307 ) ) ;
#31868 = ORIENTED_EDGE ( 'NONE', *, *, #9734, .F. ) ;
#31869 = ORIENTED_EDGE ( 'NONE', *, *, #48323, .T. ) ;
#31870 = CYLINDRICAL_SURFACE ( 'NONE', #48870, 15.70000000000326956 ) ;
#31871 = DIRECTION ( 'NONE',  ( 0.000000000000000000, 0.000000000000000000, 1.000000000000000000 ) ) ;
#31872 = CARTESIAN_POINT ( 'NONE',  ( 10.00000000000000000, 0.000000000000000000, 0.000000000000000000 ) ) ;
#31873 = EDGE_LOOP ( 'NONE', ( #74281, #14129, #74, #4350 ) ) ;
#31874 = CIRCLE ( 'NONE', #64322, 77.49899999999999523 ) ;
#31875 = FACE_OUTER_BOUND ( 'NONE', #53263, .T. ) ;
#31876 = CARTESIAN_POINT ( 'NONE',  ( 96.15314808468750130, -211.9973110713294489, 76.04322916753382344 ) ) ;
#31877 = EDGE_LOOP ( 'NONE', ( #52211, #56713, #52410, #33786 ) ) ;
#31878 = EDGE_CURVE ( 'NONE', #35308, #21754, #3393, .T. ) ;
#31879 = CARTESIAN_POINT ( 'NONE',  ( 10.00000000000000000, -73.72996012237449293, 14.67089635893687571 ) ) ;
#31880 = EDGE_LOOP ( 'NONE', ( #47272, #68982, #33931 ) ) ;
#31881 = CIRCLE ( 'NONE', #42746, 31.99999999999998579 ) ;
#31882 = ORIENTED_EDGE ( 'NONE', *, *, #30992, .T. ) ;
#31883 = DIRECTION ( 'NONE',  ( 0.000000000000000000, 0.000000000000000000, 1.000000000000000000 ) ) ;
#31884 = EDGE_CURVE ( 'NONE', #1062, #64295, #36963, .T. ) ;
#31885 = SHAPE_REPRESENTATION_RELATIONSHIP ( 'NONE' , 'NONE' ,  #65179, #59777 ) ;
#31886 = AXIS2_PLACEMENT_3D ( 'NONE', #29367, #58322, #29006 ) ;
#31887 = DIRECTION ( 'NONE',  ( 0.000000000000000000, 0.000000000000000000, -1.000000000000000000 ) ) ;
#31888 = AXIS2_PLACEMENT_3D ( 'NONE', #61543, #73541, #4041 ) ;
#31889 = VERTEX_POINT ( 'NONE', #61940 ) ;
#31890 = CARTESIAN_POINT ( 'NONE',  ( 97.64999999999999147, 90.00000000000002842, 90.00000000000000000 ) ) ;
#31891 = CARTESIAN_POINT ( 'NONE',  ( 96.32499999999998863, -207.7050326799711968, 81.61270833506763722 ) ) ;
#31892 = EDGE_CURVE ( 'NONE', #54291, #56237, #33339, .T. ) ;
#31893 = CARTESIAN_POINT ( 'NONE',  ( 97.64999999999997726, 91.52997821335252127, 84.02041666666667652 ) ) ;
#31894 = EDGE_CURVE ( 'NONE', #54114, #23922, #52878, .T. ) ;
#31895 = VERTEX_POINT ( 'NONE', #59254 ) ;
#31896 = DIRECTION ( 'NONE',  ( 0.000000000000000000, 0.000000000000000000, 1.000000000000000000 ) ) ;
#31897 = CARTESIAN_POINT ( 'NONE',  ( 5.999999999999999112, 63.97538442413498672, -51.29473840253155004 ) ) ;
#31898 = AXIS2_PLACEMENT_3D ( 'NONE', #73813, #11053, #68192 ) ;
#31899 = ORIENTED_EDGE ( 'NONE', *, *, #37262, .F. ) ;
#31900 = AXIS2_PLACEMENT_3D ( 'NONE', #45919, #27104, #28598 ) ;
#31901 = ORIENTED_EDGE ( 'NONE', *, *, #62059, .T. ) ;
#31902 = CARTESIAN_POINT ( 'NONE',  ( -96.15314808468752972, 91.99731107132950569, 88.42572916753381662 ) ) ;
#31903 = CARTESIAN_POINT ( 'NONE',  ( 93.84685191531248449, 88.00268892867053694, 80.22364583420046813 ) ) ;
#31904 = VERTEX_POINT ( 'NONE', #12640 ) ;
#31905 = CARTESIAN_POINT ( 'NONE',  ( 96.32499999999998863, 87.70503267997126784, 83.30604166840096525 ) ) ;
#31906 = DIRECTION ( 'NONE',  ( 1.000000000000000000, -3.961972362386988449E-13, -2.612289469705706555E-14 ) ) ;
#31907 = EDGE_LOOP ( 'NONE', ( #20616, #38012, #67391, #52096 ) ) ;
#31908 = FACE_BOUND ( 'NONE', #60208, .T. ) ;
#31909 = ORIENTED_EDGE ( 'NONE', *, *, #65343, .F. ) ;
#31910 = ORIENTED_EDGE ( 'NONE', *, *, #61726, .T. ) ;
#31911 = EDGE_CURVE ( 'NONE', #13389, #23740, #33180, .T. ) ;
#31912 = ORIENTED_EDGE ( 'NONE', *, *, #43550, .T. ) ;
#31913 = DIRECTION ( 'NONE',  ( 1.000000000000000000, 0.000000000000000000, 0.000000000000000000 ) ) ;
#31914 = EDGE_CURVE ( 'NONE', #64387, #49393, #56185, .T. ) ;
#31915 = VERTEX_POINT ( 'NONE', #64165 ) ;
#31916 = CARTESIAN_POINT ( 'NONE',  ( -94.99999999999997158, -206.9400435732949575, 81.03062500173430749 ) ) ;
#31917 = CARTESIAN_POINT ( 'NONE',  ( 97.64999999999997726, 91.52997821335252127, 87.90979166840095615 ) ) ;
#31918 = ORIENTED_EDGE ( 'NONE', *, *, #45505, .T. ) ;
#31919 = DIRECTION ( 'NONE',  ( -1.000000000000000000, 0.000000000000000000, 0.000000000000000000 ) ) ;
#31920 = CARTESIAN_POINT ( 'NONE',  ( -94.99999999999997158, -207.3369185715606307, 80.59406250086715318 ) ) ;
#31921 = VERTEX_POINT ( 'NONE', #70506 ) ;
#31922 = LINE ( 'NONE', #55974, #15846 ) ;
#31923 = CARTESIAN_POINT ( 'NONE',  ( -3.000000000000000000, -0.9646360437372163421, -23.52805723605591126 ) ) ;
#31924 = CYLINDRICAL_SURFACE ( 'NONE', #68188, 2.649999999999999467 ) ;
#31925 = FACE_OUTER_BOUND ( 'NONE', #40209, .T. ) ;
#31926 = FACE_OUTER_BOUND ( 'NONE', #25181, .T. ) ;
#31927 = ADVANCED_FACE ( 'NONE', ( #1783 ), #7001, .T. ) ;
#31928 = ADVANCED_FACE ( 'NONE', ( #58890 ), #19017, .T. ) ;
#31929 = CARTESIAN_POINT ( 'NONE',  ( 10.00000000000000000, 12.26510123303308752, -35.53030884539072787 ) ) ;
#31930 = CARTESIAN_POINT ( 'NONE',  ( 92.69370383062498320, 91.33154071421968467, 88.31989583420048007 ) ) ;
#31931 = CARTESIAN_POINT ( 'NONE',  ( -92.34999999999999432, -209.9999999999999716, 85.87249999999998806 ) ) ;
#31932 = FACE_OUTER_BOUND ( 'NONE', #30502, .T. ) ;
#31933 = FACE_OUTER_BOUND ( 'NONE', #24523, .T. ) ;
#31934 = CARTESIAN_POINT ( 'NONE',  ( 0.000000000000000000, 0.000000000000000000, 0.000000000000000000 ) ) ;
#31935 = LINE ( 'NONE', #3397, #53900 ) ;
#31936 = CARTESIAN_POINT ( 'NONE',  ( 10.00000000000000000, 0.000000000000000000, 0.000000000000000000 ) ) ;
#31937 = FACE_BOUND ( 'NONE', #19882, .T. ) ;
#31938 = CIRCLE ( 'NONE', #47570, 26.50000000000552092 ) ;
#31939 = CARTESIAN_POINT ( 'NONE',  ( 10.00000000000000000, -75.11764819372145041, 29.05362095685286761 ) ) ;
#31940 = DIRECTION ( 'NONE',  ( 1.000000000000000000, 0.000000000000000000, 0.000000000000000000 ) ) ;
#31941 = CARTESIAN_POINT ( 'NONE',  ( 96.15314808468748708, 91.99731107132950569, 89.58989583420049030 ) ) ;
#31942 = DIRECTION ( 'NONE',  ( 1.000000000000000000, 0.000000000000000000, 0.000000000000000000 ) ) ;
#31943 = AXIS2_PLACEMENT_3D ( 'NONE', #36032, #69871, #34554 ) ;
#31944 = CARTESIAN_POINT ( 'NONE',  ( 11.99999999999999822, -62.50884508063453637, 41.76106447765467777 ) ) ;
#31945 = CARTESIAN_POINT ( 'NONE',  ( -92.34999999999999432, -208.4700217866474645, 88.46541666666665549 ) ) ;
#31946 = AXIS2_PLACEMENT_3D ( 'NONE', #73826, #15205, #38888 ) ;
#31947 = CARTESIAN_POINT ( 'NONE',  ( 97.64999999999601243, 89.99999541993086893, 76.42687486206342840 ) ) ;
#31948 = PRODUCT ( 'housing', 'housing', '', ( #45623 ) ) ;
#31949 = VECTOR ( 'NONE', #64316, 1000.000000000000000 ) ;
#31950 = AXIS2_PLACEMENT_3D ( 'NONE', #73716, #4960, #5696 ) ;
#31951 = EDGE_LOOP ( 'NONE', ( #39650, #15630, #66416, #68252 ) ) ;
#31952 = CARTESIAN_POINT ( 'NONE',  ( 0.000000000000000000, 12.42422080174638310, 35.38097989696515810 ) ) ;
#31953 = CARTESIAN_POINT ( 'NONE',  ( 0.000000000000000000, 0.000000000000000000, 0.000000000000000000 ) ) ;
#31954 = FACE_OUTER_BOUND ( 'NONE', #17843, .T. ) ;
#31955 = FACE_OUTER_BOUND ( 'NONE', #44019, .T. ) ;
#31956 = ORIENTED_EDGE ( 'NONE', *, *, #49725, .F. ) ;
#31957 = ORIENTED_EDGE ( 'NONE', *, *, #41430, .F. ) ;
#31958 = CARTESIAN_POINT ( 'NONE',  ( 15.00000000000000000, -11.95096189432345746, -23.69967320028757030 ) ) ;
#31959 = DIRECTION ( 'NONE',  ( 0.000000000000000000, 0.000000000000000000, 1.000000000000000000 ) ) ;
#31960 = VERTEX_POINT ( 'NONE', #29926 ) ;
#31961 = CARTESIAN_POINT ( 'NONE',  ( 93.84685191531251292, -211.9973110713294489, 80.85864583420047325 ) ) ;
#31962 = CARTESIAN_POINT ( 'NONE',  ( 92.69370383062501162, -208.6684592857803295, 84.03364583420049883 ) ) ;
#31963 = VERTEX_POINT ( 'NONE', #41972 ) ;
#31964 = CARTESIAN_POINT ( 'NONE',  ( 96.15314808468750130, -211.9973110713294489, 86.20322916753382003 ) ) ;
#31965 = ORIENTED_EDGE ( 'NONE', *, *, #47630, .T. ) ;
#31966 = ADVANCED_FACE ( 'NONE', ( #24309 ), #69417, .F. ) ;
#31967 = FACE_OUTER_BOUND ( 'NONE', #43744, .T. ) ;
#31968 = ORIENTED_EDGE ( 'NONE', *, *, #39635, .F. ) ;
#31969 = CARTESIAN_POINT ( 'NONE',  ( -95.00000000000002842, 92.66308142843932671, 77.57781250086715374 ) ) ;
#31970 = VERTEX_POINT ( 'NONE', #41222 ) ;
#31971 = EDGE_CURVE ( 'NONE', #41695, #57350, #63388, .T. ) ;
#31972 = ORIENTED_EDGE ( 'NONE', *, *, #16288, .F. ) ;
#31973 = DIRECTION ( 'NONE',  ( -1.000000000000000000, 0.000000000000000000, -0.000000000000000000 ) ) ;
#31974 = ORIENTED_EDGE ( 'NONE', *, *, #673, .F. ) ;
#31975 = CARTESIAN_POINT ( 'NONE',  ( 93.67499999999998295, 92.29496732002878900, 88.06854166840095388 ) ) ;
#31976 = DIRECTION ( 'NONE',  ( 1.000000000000000000, 0.000000000000000000, 0.000000000000000000 ) ) ;
#31977 = EDGE_CURVE ( 'NONE', #27109, #46417, #63549, .T. ) ;
#31978 = EDGE_LOOP ( 'NONE', ( #5980, #71031, #30903, #65295 ) ) ;
#31979 = CARTESIAN_POINT ( 'NONE',  ( 11.99999999999999822, 0.000000000000000000, 0.000000000000000000 ) ) ;
#31980 = VERTEX_POINT ( 'NONE', #18646 ) ;
#31981 = CARTESIAN_POINT ( 'NONE',  ( 11.99999999999999822, 80.28980883073758434, 16.65972982744962749 ) ) ;
#31982 = ADVANCED_FACE ( 'NONE', ( #64525 ), #46132, .T. ) ;
#31983 = CONICAL_SURFACE ( 'NONE', #74019, 5.000000000000000888, 1.047197551196596299 ) ;
#31984 = ORIENTED_EDGE ( 'NONE', *, *, #8735, .T. ) ;
#31985 = EDGE_CURVE ( 'NONE', #19363, #31543, #37143, .T. ) ;
#31986 = ORIENTED_EDGE ( 'NONE', *, *, #48740, .F. ) ;
#31987 = ORIENTED_EDGE ( 'NONE', *, *, #37091, .T. ) ;
#31988 = CARTESIAN_POINT ( 'NONE',  ( 97.30629616937498838, -208.6684592857803011, 78.58322916753381548 ) ) ;
#31989 = CARTESIAN_POINT ( 'NONE',  ( 11.99999999999999822, 0.000000000000000000, 0.000000000000000000 ) ) ;
#31990 = CONTEXT_DEPENDENT_SHAPE_REPRESENTATION ( #9546, #67401 ) ;
#31991 = DIRECTION ( 'NONE',  ( 0.000000000000000000, 0.000000000000000000, 1.000000000000000000 ) ) ;
#31992 = VERTEX_POINT ( 'NONE', #17547 ) ;
#31993 = VERTEX_POINT ( 'NONE', #35943 ) ;
#31994 = CIRCLE ( 'NONE', #58410, 31.99999999999998579 ) ;
#31995 = VERTEX_POINT ( 'NONE', #2148 ) ;
#31996 = CIRCLE ( 'NONE', #40381, 16.00000000000000000 ) ;
#31997 = CARTESIAN_POINT ( 'NONE',  ( 12.74955575014913833, 0.001194404169505926478, -64.99999999999967315 ) ) ;
#31998 = DIRECTION ( 'NONE',  ( 1.000000000000000000, -3.061616997868382648E-16, -0.000000000000000000 ) ) ;
#31999 = EDGE_CURVE ( 'NONE', #42708, #29316, #14139, .T. ) ;
#32000 = CARTESIAN_POINT ( 'NONE',  ( -92.69370383062504004, 90.00000000000004263, 80.59406250086715318 ) ) ;
#32001 = EDGE_CURVE ( 'NONE', #5496, #46961, #40480, .T. ) ;
#32002 = VERTEX_POINT ( 'NONE', #63428 ) ;
#32003 = CARTESIAN_POINT ( 'NONE',  ( 97.30629616937498838, 88.66845928578037217, 77.84239583420045960 ) ) ;
#32004 = VERTEX_POINT ( 'NONE', #11902 ) ;
#32005 = CARTESIAN_POINT ( 'NONE',  ( 10.00000000000000000, -39.04073710021356192, 15.48615015657568250 ) ) ;
#32006 = CARTESIAN_POINT ( 'NONE',  ( -97.30629616937497417, -208.6684592857803011, 88.95489583420048518 ) ) ;
#32007 = CARTESIAN_POINT ( 'NONE',  ( 0.000000000000000000, 74.65374052328648702, 8.840884882375350529 ) ) ;
#32008 = DIRECTION ( 'NONE',  ( -1.000000000000000000, -0.000000000000000000, 0.000000000000000000 ) ) ;
#32009 = CYLINDRICAL_SURFACE ( 'NONE', #48896, 31.99999999999999289 ) ;
#32010 = CARTESIAN_POINT ( 'NONE',  ( -96.15314808468747287, -208.0026889286704943, 83.18697916753382060 ) ) ;
#32011 = CARTESIAN_POINT ( 'NONE',  ( 2.499999999999981348, -79.99999999999998579, -280.0000000000000000 ) ) ;
#32012 = CARTESIAN_POINT ( 'NONE',  ( 5.999999999999999112, -27.74655509720726698, 77.16300072079651784 ) ) ;
#32013 = CARTESIAN_POINT ( 'NONE',  ( 11.99999999999999822, -46.21855187248585395, -62.20884554314068993 ) ) ;
#32014 = VERTEX_POINT ( 'NONE', #35206 ) ;
#32015 = EDGE_CURVE ( 'NONE', #52268, #61765, #49450, .T. ) ;
#32016 = EDGE_CURVE ( 'NONE', #47415, #26822, #9222, .T. ) ;
#32017 = PRESENTATION_LAYER_ASSIGNMENT (  '', '', ( #28426 ) ) ;
#32018 = EDGE_LOOP ( 'NONE', ( #42066, #15619, #9251, #68570 ) ) ;
#32019 = FACE_OUTER_BOUND ( 'NONE', #63396, .T. ) ;
#32020 = DIRECTION ( 'NONE',  ( -1.000000000000000000, 0.000000000000000000, 0.000000000000000000 ) ) ;
#32021 = DIRECTION ( 'NONE',  ( -1.000000000000000000, 0.000000000000000000, 0.000000000000000000 ) ) ;
#32022 = CARTESIAN_POINT ( 'NONE',  ( -92.69370383062504004, 90.00000000000004263, 86.78531250086714977 ) ) ;
#32023 = FACE_OUTER_BOUND ( 'NONE', #33371, .T. ) ;
#32024 = CARTESIAN_POINT ( 'NONE',  ( 0.000000000000000000, 8.840884882376133902, -74.65374052328640175 ) ) ;
#32025 = VERTEX_POINT ( 'NONE', #48709 ) ;
#32026 = CARTESIAN_POINT ( 'NONE',  ( 10.00000000000000000, 29.81001611431041098, -22.74946021919100403 ) ) ;
#32027 = CARTESIAN_POINT ( 'NONE',  ( -30.50000000000000000, -120.0000000000000000, -2.500000000000000000 ) ) ;
#32028 = DIRECTION ( 'NONE',  ( -1.000000000000000000, -0.000000000000000000, -0.000000000000000000 ) ) ;
#32029 = CARTESIAN_POINT ( 'NONE',  ( 0.000000000000000000, 1.732050807568878747, 7.017607234860990640E-28 ) ) ;
#32030 = DIRECTION ( 'NONE',  ( -1.000000000000000000, 0.000000000000000000, 0.000000000000000000 ) ) ;
#32031 = CARTESIAN_POINT ( 'NONE',  ( -32.50000000000000000, -120.0000000000000000, -2.500000000000000000 ) ) ;
#32032 = CARTESIAN_POINT ( 'NONE',  ( -96.15314808468747287, -208.0026889286704943, 81.44072916753381719 ) ) ;
#32033 = CARTESIAN_POINT ( 'NONE',  ( 10.00000000000000000, 0.000000000000000000, 0.000000000000000000 ) ) ;
#32034 = AXIS2_PLACEMENT_3D ( 'NONE', #45459, #35269, #52547 ) ;
#32035 = DIRECTION ( 'NONE',  ( -1.000000000000000000, -0.000000000000000000, -0.000000000000000000 ) ) ;
#32036 = CARTESIAN_POINT ( 'NONE',  ( 0.000000000000000000, 0.000000000000000000, 0.000000000000000000 ) ) ;
#32037 = DIRECTION ( 'NONE',  ( -0.000000000000000000, -0.000000000000000000, -1.000000000000000000 ) ) ;
#32038 = CIRCLE ( 'NONE', #39263, 31.99999999999999645 ) ;
#32039 = ORIENTED_EDGE ( 'NONE', *, *, #35209, .T. ) ;
#32040 = DIRECTION ( 'NONE',  ( 1.000000000000000000, 0.000000000000000000, 0.000000000000000000 ) ) ;
#32041 = DIRECTION ( 'NONE',  ( -1.000000000000000000, 0.000000000000000000, 0.000000000000000000 ) ) ;
#32042 = CARTESIAN_POINT ( 'NONE',  ( -13.05994868825747446, -139.5943292883446532, 5.500000000000000000 ) ) ;
#32043 = AXIS2_PLACEMENT_3D ( 'NONE', #44561, #1867, #49806 ) ;
#32044 = EDGE_CURVE ( 'NONE', #61944, #36401, #61111, .T. ) ;
#32045 = CIRCLE ( 'NONE', #68075, 31.99999999999999289 ) ;
#32046 = CYLINDRICAL_SURFACE ( 'NONE', #1326, 2.649999999999985700 ) ;
#32047 = EDGE_LOOP ( 'NONE', ( #610, #413, #39056, #43593 ) ) ;
#32048 = EDGE_CURVE ( 'NONE', #24152, #40400, #37815, .T. ) ;
#32049 = DIRECTION ( 'NONE',  ( -1.000000000000000000, 0.000000000000000000, 0.000000000000000000 ) ) ;
#32050 = AXIS2_PLACEMENT_3D ( 'NONE', #42774, #64976, #70574 ) ;
#32051 = DIRECTION ( 'NONE',  ( 1.000000000000000000, 0.000000000000000000, 0.000000000000000000 ) ) ;
#32052 = VERTEX_POINT ( 'NONE', #43831 ) ;
#32053 = EDGE_CURVE ( 'NONE', #49911, #34884, #32522, .T. ) ;
#32054 = DIRECTION ( 'NONE',  ( -1.000000000000000000, 0.000000000000000000, 0.000000000000000000 ) ) ;
#32055 = CIRCLE ( 'NONE', #74089, 42.00000000000000000 ) ;
#32056 = VERTEX_POINT ( 'NONE', #43469 ) ;
#32057 = EDGE_CURVE ( 'NONE', #47514, #17108, #10574, .T. ) ;
#32058 = ORIENTED_EDGE ( 'NONE', *, *, #62470, .F. ) ;
#32059 = LINE ( 'NONE', #59922, #74211 ) ;
#32060 = CIRCLE ( 'NONE', #53656, 82.00000000000000000 ) ;
#32061 = ORIENTED_EDGE ( 'NONE', *, *, #21277, .T. ) ;
#32062 = ADVANCED_FACE ( 'NONE', ( #37449 ), #3620, .T. ) ;
#32063 = EDGE_LOOP ( 'NONE', ( #7872, #53541, #7838, #32447, #55659 ) ) ;
#32064 = EDGE_LOOP ( 'NONE', ( #45502, #69336 ) ) ;
#32065 = ORIENTED_EDGE ( 'NONE', *, *, #34026, .T. ) ;
#32066 = CARTESIAN_POINT ( 'NONE',  ( 0.000000000000000000, -22.74946021919153694, 29.81001611431000597 ) ) ;
#32067 = VECTOR ( 'NONE', #52414, 1000.000000000000000 ) ;
#32068 = ORIENTED_EDGE ( 'NONE', *, *, #56082, .T. ) ;
#32069 = ORIENTED_EDGE ( 'NONE', *, *, #58489, .T. ) ;
#32070 = CARTESIAN_POINT ( 'NONE',  ( 92.69370383062498320, 91.33154071421968467, 75.14364583420049826 ) ) ;
#32071 = DIRECTION ( 'NONE',  ( 0.000000000000000000, 0.000000000000000000, 1.000000000000000000 ) ) ;
#32072 = ADVANCED_FACE ( 'NONE', ( #55088 ), #38168, .F. ) ;
#32073 = DIRECTION ( 'NONE',  ( -1.000000000000000000, -0.000000000000000000, 0.000000000000000000 ) ) ;
#32074 = VERTEX_POINT ( 'NONE', #59629 ) ;
#32075 = ORIENTED_EDGE ( 'NONE', *, *, #17334, .T. ) ;
#32076 = ORIENTED_EDGE ( 'NONE', *, *, #23583, .T. ) ;
#32077 = CARTESIAN_POINT ( 'NONE',  ( 92.69370383062498320, 91.33154071421968467, 88.31989583420046586 ) ) ;
#32078 = ORIENTED_EDGE ( 'NONE', *, *, #36099, .T. ) ;
#32079 = CARTESIAN_POINT ( 'NONE',  ( 97.30629616937498838, -208.6684592857803011, 89.37822916753381719 ) ) ;
#32080 = DIRECTION ( 'NONE',  ( -0.6912384115093119785, 0.7226267767347698268, 0.000000000000000000 ) ) ;
#32081 = DIRECTION ( 'NONE',  ( 0.000000000000000000, 0.000000000000000000, 1.000000000000000000 ) ) ;
#32082 = DIRECTION ( 'NONE',  ( 0.000000000000000000, 0.000000000000000000, 1.000000000000000000 ) ) ;
#32083 = CARTESIAN_POINT ( 'NONE',  ( 96.32499999999997442, 92.29496732002878900, 77.80270833506763495 ) ) ;
#32084 = DIRECTION ( 'NONE',  ( -1.000000000000000000, -0.000000000000000000, -0.000000000000000000 ) ) ;
#32085 = CYLINDRICAL_SURFACE ( 'NONE', #7228, 15.77977592589476608 ) ;
#32086 = FACE_OUTER_BOUND ( 'NONE', #34753, .T. ) ;
#32087 = CARTESIAN_POINT ( 'NONE',  ( -96.32499999999996021, -207.7050326799711968, 75.36854166840096525 ) ) ;
#32088 = EDGE_CURVE ( 'NONE', #18817, #3169, #38468, .T. ) ;
#32089 = CARTESIAN_POINT ( 'NONE',  ( 0.000000000000000000, -65.59268652807237743, 36.72794159290217664 ) ) ;
#32090 = ADVANCED_FACE ( 'NONE', ( #70892 ), #49078, .T. ) ;
#32091 = ORIENTED_EDGE ( 'NONE', *, *, #2331, .F. ) ;
#32093 = CARTESIAN_POINT ( 'NONE',  ( -96.15314808468752972, 91.99731107132950569, 87.63197916753379957 ) ) ;
#32092 = CARTESIAN_POINT ( 'NONE',  ( 97.30629616937498838, 90.00000000000002842, 86.78531250086714977 ) ) ;
#32094 =( BOUNDED_CURVE ( )  B_SPLINE_CURVE ( 2, ( #22951, #61677, #23313, #10164, #67689, #56028, #4550 ),
 .UNSPECIFIED., .F., .F. ) 
 B_SPLINE_CURVE_WITH_KNOTS ( ( 3, 2, 2, 3 ),
 ( 0.8125000000000002220, 0.8194444444444446418, 0.8263888888888889506, 0.8333333333333334814 ),
 .UNSPECIFIED. ) 
 CURVE ( )  GEOMETRIC_REPRESENTATION_ITEM ( )  RATIONAL_B_SPLINE_CURVE ( ( 0.9999999999999956701, 0.8660254037844430375, 1.000000000000000000, 0.8660254037844387076, 1.000000000000000000, 0.8660254037844365982, 1.000000000000002220 ) ) 
 REPRESENTATION_ITEM ( '' )  );
#32095 = ORIENTED_EDGE ( 'NONE', *, *, #38991, .T. ) ;
#32096 = CARTESIAN_POINT ( 'NONE',  ( 96.15314808468748708, 91.99731107132950569, 77.52489583420047836 ) ) ;
#32097 = DIRECTION ( 'NONE',  ( 0.000000000000000000, 0.000000000000000000, 1.000000000000000000 ) ) ;
#32098 = DIRECTION ( 'NONE',  ( -0.000000000000000000, -0.000000000000000000, 1.000000000000000000 ) ) ;
#32099 = DIRECTION ( 'NONE',  ( 1.000000000000000000, 0.000000000000000000, 0.000000000000000000 ) ) ;
#32100 = CARTESIAN_POINT ( 'NONE',  ( 95.00000000000000000, -213.0599564267049857, 77.53812500173428646 ) ) ;
#32101 = CARTESIAN_POINT ( 'NONE',  ( -97.65000000000001990, 90.00000000000004263, 89.36499999999999488 ) ) ;
#32102 = CARTESIAN_POINT ( 'NONE',  ( 11.99999999999999822, -72.35160999960831418, 20.41045688087797672 ) ) ;
#32103 = PLANE ( 'NONE',  #7230 ) ;
#32104 = ORIENTED_EDGE ( 'NONE', *, *, #61943, .T. ) ;
#32105 = AXIS2_PLACEMENT_3D ( 'NONE', #24092, #59402, #64671 ) ;
#32106 = VERTEX_POINT ( 'NONE', #20127 ) ;
#32107 = AXIS2_PLACEMENT_3D ( 'NONE', #56936, #44914, #17440 ) ;
#32108 = CARTESIAN_POINT ( 'NONE',  ( -95.00000000000002842, 93.05995642670501411, 80.31624999999998238 ) ) ;
#32109 = CYLINDRICAL_SURFACE ( 'NONE', #49928, 42.00000000000000000 ) ;
#32110 = CARTESIAN_POINT ( 'NONE',  ( 92.35000000000007958, -208.4700217866474361, 82.96208333333332519 ) ) ;
#32111 = DIRECTION ( 'NONE',  ( -0.000000000000000000, -0.000000000000000000, 1.000000000000000000 ) ) ;
#32112 = CARTESIAN_POINT ( 'NONE',  ( 0.000000000000000000, 46.53671651294032330, -59.03961581697353012 ) ) ;
#32113 = CARTESIAN_POINT ( 'NONE',  ( 0.000000000000000000, 73.72996012237460661, -14.67089635893632504 ) ) ;
#32114 = CARTESIAN_POINT ( 'NONE',  ( 16.84844760790522855, -103.5491698323862124, 5.500000000000000000 ) ) ;
#32115 = VERTEX_POINT ( 'NONE', #37063 ) ;
#32116 = CARTESIAN_POINT ( 'NONE',  ( -93.84685191531252713, 88.00268892867056536, 80.96447916753380980 ) ) ;
#32117 = CARTESIAN_POINT ( 'NONE',  ( 19.12409105625795291, -101.5943176906707919, 5.500000000000000000 ) ) ;
#32118 = DIRECTION ( 'NONE',  ( -0.000000000000000000, -0.000000000000000000, 1.000000000000000000 ) ) ;
#32119 = LINE ( 'NONE', #61079, #58512 ) ;
#32120 = FACE_OUTER_BOUND ( 'NONE', #40038, .T. ) ;
#32121 = DIRECTION ( 'NONE',  ( 0.000000000000000000, 0.9723699203976756689, 0.2334453638559093602 ) ) ;
#32122 = DIRECTION ( 'NONE',  ( -1.000000000000000000, -0.000000000000000000, -0.000000000000000000 ) ) ;
#32123 = CARTESIAN_POINT ( 'NONE',  ( 10.00000000000000000, 76.66974797899837313, 11.30684508768368524 ) ) ;
#32124 = AXIS2_PLACEMENT_3D ( 'NONE', #4468, #15731, #54462 ) ;
#32125 = EDGE_CURVE ( 'NONE', #22556, #64812, #58588, .T. ) ;
#32126 = CARTESIAN_POINT ( 'NONE',  ( 96.15314808468748708, 91.99731107132950569, 80.06489583420048461 ) ) ;
#32127 = CARTESIAN_POINT ( 'NONE',  ( -94.99999999999997158, -212.6630814284392557, 84.24531250086717193 ) ) ;
#32128 = CARTESIAN_POINT ( 'NONE',  ( 0.000000000000000000, -120.0000000000000000, 2.500000000000000000 ) ) ;
#32129 = VERTEX_POINT ( 'NONE', #2532 ) ;
#32130 = CARTESIAN_POINT ( 'NONE',  ( -96.32499999999996021, -212.2949673200287179, 81.21583333333333599 ) ) ;
#32131 = CARTESIAN_POINT ( 'NONE',  ( -93.67499999999998295, -207.7050326799711968, 77.72333333333332916 ) ) ;
#32132 = DIRECTION ( 'NONE',  ( -1.000000000000000000, -0.000000000000000000, -0.000000000000000000 ) ) ;
#32133 = EDGE_CURVE ( 'NONE', #53810, #38967, #26163, .T. ) ;
#32134 = CARTESIAN_POINT ( 'NONE',  ( 97.30629616937498838, -209.9999999999999716, 82.34031250086714238 ) ) ;
#32135 = VERTEX_POINT ( 'NONE', #19759 ) ;
#32136 = ADVANCED_FACE ( 'NONE', ( #54359, #2883 ), #5466, .T. ) ;
#32137 = CYLINDRICAL_SURFACE ( 'NONE', #17865, 15.70000000000326956 ) ;
#32138 = ORIENTED_EDGE ( 'NONE', *, *, #20865, .T. ) ;
#32139 = CARTESIAN_POINT ( 'NONE',  ( 5.000000000000000000, -27.75498641678720446, -31.52238457039628727 ) ) ;
#32140 = VERTEX_POINT ( 'NONE', #38548 ) ;
#32141 = MECHANICAL_DESIGN_GEOMETRIC_PRESENTATION_REPRESENTATION (  '', ( #50121 ), #41761 ) ;
#32142 = AXIS2_PLACEMENT_3D ( 'NONE', #7367, #30645, #2132 ) ;
#32143 = EDGE_CURVE ( 'NONE', #65173, #68158, #15617, .T. ) ;
#32144 = ADVANCED_FACE ( 'NONE', ( #61853 ), #73485, .T. ) ;
#32145 = CARTESIAN_POINT ( 'NONE',  ( -95.00000000000002842, 86.94004357329504273, 79.44312500173430180 ) ) ;
#32146 = AXIS2_PLACEMENT_3D ( 'NONE', #2493, #14460, #42667 ) ;
#32147 = VECTOR ( 'NONE', #63967, 1000.000000000000000 ) ;
#32148 = CARTESIAN_POINT ( 'NONE',  ( 92.69370383062501162, -211.3315407142195852, 77.78947916753381264 ) ) ;
#32149 = CYLINDRICAL_SURFACE ( 'NONE', #14088, 2.649999999999985700 ) ;
#32150 = LINE ( 'NONE', #61120, #50827 ) ;
#32151 = CARTESIAN_POINT ( 'NONE',  ( -97.01659045497900991, 88.39448418669211094, 74.95309847082319266 ) ) ;
#32152 = CARTESIAN_POINT ( 'NONE',  ( 96.15314808468748708, 88.00268892867053694, 85.56822916753381492 ) ) ;
#32153 = EDGE_CURVE ( 'NONE', #41196, #63433, #40565, .T. ) ;
#32154 = DIRECTION ( 'NONE',  ( 0.000000000000000000, 0.000000000000000000, 1.000000000000000000 ) ) ;
#32155 = CARTESIAN_POINT ( 'NONE',  ( 93.67500000000001137, -207.7050326799711968, 80.36916666666665776 ) ) ;
#32156 = VERTEX_POINT ( 'NONE', #67860 ) ;
#32157 = VERTEX_POINT ( 'NONE', #67488 ) ;
#32158 = ORIENTED_EDGE ( 'NONE', *, *, #66207, .F. ) ;
#32159 = EDGE_LOOP ( 'NONE', ( #67225, #63741, #26384, #7768 ) ) ;
#32160 = CIRCLE ( 'NONE', #54982, 82.00000000000000000 ) ;
#32161 =( LENGTH_UNIT ( ) NAMED_UNIT ( * ) SI_UNIT ( .MILLI., .METRE. ) );
#32162 = CARTESIAN_POINT ( 'NONE',  ( -92.69370383062502583, 91.33154071421968467, 84.45697916753383083 ) ) ;
#32163 = CARTESIAN_POINT ( 'NONE',  ( 4.999999999999999112, 41.81611651403861885, 3.925862922256313503 ) ) ;
#32164 = VECTOR ( 'NONE', #18683, 1000.000000000000000 ) ;
#32165 = DIRECTION ( 'NONE',  ( -1.000000000000000000, 0.000000000000000000, -0.000000000000000000 ) ) ;
#32166 = CARTESIAN_POINT ( 'NONE',  ( 10.00000000000000000, -49.70050353004933896, 59.46389618801946852 ) ) ;
#32167 = CIRCLE ( 'NONE', #15383, 42.00000000000000000 ) ;
#32168 = CARTESIAN_POINT ( 'NONE',  ( 10.00000000000000000, 0.000000000000000000, 0.000000000000000000 ) ) ;
#32169 = CIRCLE ( 'NONE', #6965, 16.00000000000000000 ) ;
#32170 = ORIENTED_EDGE ( 'NONE', *, *, #39639, .F. ) ;
#32171 = CARTESIAN_POINT ( 'NONE',  ( -97.64999999999994884, -211.5299782133524502, 86.95729166840096980 ) ) ;
#32173 = ORIENTED_EDGE ( 'NONE', *, *, #40593, .T. ) ;
#32172 = EDGE_CURVE ( 'NONE', #65748, #9715, #62609, .T. ) ;
#32174 = FACE_OUTER_BOUND ( 'NONE', #27118, .T. ) ;
#32175 = EDGE_LOOP ( 'NONE', ( #3275, #64817, #8584, #73597 ) ) ;
#32176 = CARTESIAN_POINT ( 'NONE',  ( -96.32500000000001705, 87.70503267997129626, 81.93020833506763267 ) ) ;
#32177 = STYLED_ITEM ( 'NONE', ( #51934 ), #36653 ) ;
#32179 = EDGE_CURVE ( 'NONE', #18340, #23470, #26879, .T. ) ;
#32178 = ORIENTED_EDGE ( 'NONE', *, *, #28273, .F. ) ;
#32180 = CARTESIAN_POINT ( 'NONE',  ( 97.30629616937498838, 91.33154071421968467, 88.26697916753381890 ) ) ;
#32181 = LINE ( 'NONE', #48743, #4621 ) ;
#32182 = DIRECTION ( 'NONE',  ( -0.000000000000000000, -0.000000000000000000, -1.000000000000000000 ) ) ;
#32183 = CARTESIAN_POINT ( 'NONE',  ( -97.64999999950686060, 89.99996796133669363, 83.73041644179562581 ) ) ;
#32184 = DIRECTION ( 'NONE',  ( 1.000000000000000000, -0.000000000000000000, -0.000000000000000000 ) ) ;
#32185 = CARTESIAN_POINT ( 'NONE',  ( 10.00000000000000000, -65.64334221924882229, -41.19522573413803457 ) ) ;
#32186 = VERTEX_POINT ( 'NONE', #56959 ) ;
#32187 = CARTESIAN_POINT ( 'NONE',  ( -10.00000000000000000, 0.000000000000000000, 0.000000000000000000 ) ) ;
#32188 = CARTESIAN_POINT ( 'NONE',  ( 0.000000000000000000, 0.000000000000000000, 20.00000000000000000 ) ) ;
#32189 = ORIENTED_EDGE ( 'NONE', *, *, #24270, .F. ) ;
#32190 = VERTEX_POINT ( 'NONE', #39669 ) ;
#32191 = LINE ( 'NONE', #27585, #22311 ) ;
#32192 = CARTESIAN_POINT ( 'NONE',  ( 4.250000000000000000, -13.95926121303099343, -1.199999999999999956 ) ) ;
#32193 = DIRECTION ( 'NONE',  ( -1.000000000000000000, 0.000000000000000000, 0.000000000000000000 ) ) ;
#32194 = CARTESIAN_POINT ( 'NONE',  ( -93.84685191531247028, -211.9973110713294489, 84.29822916753381890 ) ) ;
#32195 = VERTEX_POINT ( 'NONE', #28365 ) ;
#32196 = VECTOR ( 'NONE', #69803, 1000.000000000000000 ) ;
#32197 = DIRECTION ( 'NONE',  ( 0.000000000000000000, 0.000000000000000000, 1.000000000000000000 ) ) ;
#32198 = ORIENTED_EDGE ( 'NONE', *, *, #68354, .T. ) ;
#32199 = AXIS2_PLACEMENT_3D ( 'NONE', #64501, #12976, #35915 ) ;
#32200 = AXIS2_PLACEMENT_3D ( 'NONE', #62103, #69589, #23001 ) ;
#32201 = FACE_OUTER_BOUND ( 'NONE', #57694, .T. ) ;
#32202 = CARTESIAN_POINT ( 'NONE',  ( 11.99999999999999822, 2.946379043146343246, 75.11764819372150725 ) ) ;
#32203 = CIRCLE ( 'NONE', #49004, 31.99999999999998934 ) ;
#32204 = CARTESIAN_POINT ( 'NONE',  ( 93.84685191531248449, 88.00268892867053694, 77.68364583420047609 ) ) ;
#32205 = CIRCLE ( 'NONE', #9398, 32.00000000000000000 ) ;
#32206 = DIRECTION ( 'NONE',  ( 0.000000000000000000, 0.000000000000000000, 1.000000000000000000 ) ) ;
#32207 = DIRECTION ( 'NONE',  ( -1.000000000000000000, 0.000000000000000000, 0.000000000000000000 ) ) ;
#32208 = DIRECTION ( 'NONE',  ( -1.000000000000000000, 0.000000000000000000, -0.000000000000000000 ) ) ;
#32209 = CARTESIAN_POINT ( 'NONE',  ( 10.00000000000000000, -35.95386929396248377, -10.96151621346525751 ) ) ;
#32210 = FACE_OUTER_BOUND ( 'NONE', #21368, .T. ) ;
#32211 = DIRECTION ( 'NONE',  ( -1.000000000000000000, -0.000000000000000000, -0.000000000000000000 ) ) ;
#32212 = CARTESIAN_POINT ( 'NONE',  ( 93.67499999999999716, 87.70503267997126784, 76.85020833506763438 ) ) ;
#32213 = ORIENTED_EDGE ( 'NONE', *, *, #35030, .T. ) ;
#32214 = CARTESIAN_POINT ( 'NONE',  ( -93.84685191531254134, 91.99731107132950569, 81.81114583420047381 ) ) ;
#32215 = FACE_OUTER_BOUND ( 'NONE', #46247, .T. ) ;
#32216 = EDGE_CURVE ( 'NONE', #41287, #58363, #62226, .T. ) ;
#32217 = AXIS2_PLACEMENT_3D ( 'NONE', #31979, #56032, #44391 ) ;
#32218 = EDGE_CURVE ( 'NONE', #26486, #35261, #27340, .T. ) ;
#32219 = AXIS2_PLACEMENT_3D ( 'NONE', #5741, #69970, #28642 ) ;
#32220 = VECTOR ( 'NONE', #48140, 1000.000000000000000 ) ;
#32221 = DIRECTION ( 'NONE',  ( 1.000000000000000000, -0.000000000000000000, -0.000000000000000000 ) ) ;
#32222 = VERTEX_POINT ( 'NONE', #45312 ) ;
#32223 = CIRCLE ( 'NONE', #13017, 42.00000000000000000 ) ;
#32224 = CARTESIAN_POINT ( 'NONE',  ( 5.000000000000000000, 15.48615015657581750, 39.04073710021349797 ) ) ;
#32225 = CYLINDRICAL_SURFACE ( 'NONE', #2400, 37.49900000000000233 ) ;
#32226 = CARTESIAN_POINT ( 'NONE',  ( 11.99999999999999822, -78.73519480814938731, -22.90783923731713045 ) ) ;
#32227 = ADVANCED_FACE ( 'NONE', ( #10713 ), #62986, .F. ) ;
#32228 = DIRECTION ( 'NONE',  ( -1.000000000000000000, -0.000000000000000000, -0.000000000000000000 ) ) ;
#32229 = CARTESIAN_POINT ( 'NONE',  ( 92.69370383062501162, -208.6684592857803011, 77.68364583420047609 ) ) ;
#32230 = EDGE_LOOP ( 'NONE', ( #31337, #19346, #25430, #13926 ) ) ;
#32231 = ORIENTED_EDGE ( 'NONE', *, *, #25693, .F. ) ;
#32232 = CARTESIAN_POINT ( 'NONE',  ( 0.000000000000000000, 0.000000000000000000, 0.000000000000000000 ) ) ;
#32233 = EDGE_CURVE ( 'NONE', #72308, #18859, #40032, .T. ) ;
#32234 = FACE_OUTER_BOUND ( 'NONE', #1595, .T. ) ;
#32235 = CARTESIAN_POINT ( 'NONE',  ( 0.000000000000000000, -31.46837873494930093, -68.27212725128309501 ) ) ;
#32236 = VECTOR ( 'NONE', #13680, 1000.000000000000000 ) ;
#32237 = EDGE_CURVE ( 'NONE', #6493, #54754, #33641, .T. ) ;
#32238 = DIRECTION ( 'NONE',  ( -1.000000000000000000, 0.000000000000000000, 0.000000000000000000 ) ) ;
#32239 = EDGE_CURVE ( 'NONE', #18753, #47168, #45690, .T. ) ;
#32240 = CARTESIAN_POINT ( 'NONE',  ( 93.84685191531251292, -211.9973110713294489, 77.84239583420048803 ) ) ;
#32241 = CIRCLE ( 'NONE', #50236, 31.99999999999999289 ) ;
#32242 = AXIS2_PLACEMENT_3D ( 'NONE', #60180, #37239, #71417 ) ;
#32243 = ORIENTED_EDGE ( 'NONE', *, *, #70365, .T. ) ;
#32244 = FACE_OUTER_BOUND ( 'NONE', #54524, .T. ) ;
#32245 = ORIENTED_EDGE ( 'NONE', *, *, #72952, .T. ) ;
#32246 = EDGE_CURVE ( 'NONE', #48302, #16851, #66799, .T. ) ;
#32247 = EDGE_LOOP ( 'NONE', ( #49370, #74235, #60941, #53665 ) ) ;
#32248 = CARTESIAN_POINT ( 'NONE',  ( -3.000000000000000000, -22.67460108101774807, -6.353146135318215038 ) ) ;
#32249 = AXIS2_PLACEMENT_3D ( 'NONE', #6081, #462, #47028 ) ;
#32250 =( NAMED_UNIT ( * ) SI_UNIT ( $, .STERADIAN. ) SOLID_ANGLE_UNIT ( ) );
#32251 = DIRECTION ( 'NONE',  ( 1.000000000000000000, -0.000000000000000000, 0.000000000000000000 ) ) ;
#32252 = VECTOR ( 'NONE', #25224, 1000.000000000000000 ) ;
#32253 = ORIENTED_EDGE ( 'NONE', *, *, #37086, .F. ) ;
#32254 = CARTESIAN_POINT ( 'NONE',  ( 0.000000000000000000, 30.80686688397010542, 21.53537804866092387 ) ) ;
#32255 = CARTESIAN_POINT ( 'NONE',  ( 96.32499999999998863, -212.2949673200287179, 80.76604166840097321 ) ) ;
#32256 = CARTESIAN_POINT ( 'NONE',  ( 96.32499999999997442, 92.29496732002878900, 86.61333333333332973 ) ) ;
#32257 = ORIENTED_EDGE ( 'NONE', *, *, #60798, .F. ) ;
#32258 = CARTESIAN_POINT ( 'NONE',  ( 0.000000000000000000, 65.59268652807210742, 36.72794159290264560 ) ) ;
#32259 = ADVANCED_FACE ( 'NONE', ( #4349 ), #27632, .F. ) ;
#32260 = LINE ( 'NONE', #72486, #51347 ) ;
#32261 = ORIENTED_EDGE ( 'NONE', *, *, #17546, .F. ) ;
#32262 = VERTEX_POINT ( 'NONE', #56592 ) ;
#32263 = CARTESIAN_POINT ( 'NONE',  ( -93.84685191531252713, 88.00268892867056536, 84.93322916753382401 ) ) ;
#32264 = CARTESIAN_POINT ( 'NONE',  ( 92.69370383062498320, 91.33154071421968467, 82.60489583420047666 ) ) ;
#32265 = ORIENTED_EDGE ( 'NONE', *, *, #21102, .T. ) ;
#32266 = AXIS2_PLACEMENT_3D ( 'NONE', #55792, #10297, #62945 ) ;
#32267 = AXIS2_PLACEMENT_3D ( 'NONE', #64806, #59158, #7648 ) ;
#32268 = CARTESIAN_POINT ( 'NONE',  ( 2.600855584879231068E-12, -120.0000000000000000, -65.00000000000000000 ) ) ;
#32269 = VERTEX_POINT ( 'NONE', #5095 ) ;
#32270 = CARTESIAN_POINT ( 'NONE',  ( 0.000000000000000000, 5.256550761633969060, -77.32052557432835727 ) ) ;
#32271 = VECTOR ( 'NONE', #9036, 1000.000000000000000 ) ;
#32272 = CIRCLE ( 'NONE', #73062, 3.300000000000000711 ) ;
#32273 = EDGE_LOOP ( 'NONE', ( #28198, #20142, #51582, #27926 ) ) ;
#32274 = ORIENTED_EDGE ( 'NONE', *, *, #40910, .F. ) ;
#32275 = DIRECTION ( 'NONE',  ( -1.000000000000000000, -0.000000000000000000, 0.000000000000000000 ) ) ;
#32276 = AXIS2_PLACEMENT_3D ( 'NONE', #7112, #18751, #25875 ) ;
#32277 = AXIS2_PLACEMENT_3D ( 'NONE', #27131, #55349, #3140 ) ;
#32278 = ORIENTED_EDGE ( 'NONE', *, *, #41522, .T. ) ;
#32279 = LINE ( 'NONE', #55221, #1212 ) ;
#32280 = VECTOR ( 'NONE', #34374, 1000.000000000000114 ) ;
#32281 = CARTESIAN_POINT ( 'NONE',  ( -22.67106064244953245, -113.6342314410295842, -5.500000000000000000 ) ) ;
#32282 = ORIENTED_EDGE ( 'NONE', *, *, #43474, .T. ) ;
#32283 = PLANE ( 'NONE',  #19 ) ;
#32284 = CARTESIAN_POINT ( 'NONE',  ( -92.69370383062498320, -208.6684592857803011, 79.85322916753379729 ) ) ;
#32285 = ORIENTED_EDGE ( 'NONE', *, *, #42140, .F. ) ;
#32286 = CARTESIAN_POINT ( 'NONE',  ( 11.99999999999999822, -30.41916302227062019, -71.27951684758059514 ) ) ;
#32287 = DIRECTION ( 'NONE',  ( 0.000000000000000000, 1.000000000000000000, 3.469446951953616555E-15 ) ) ;
#32288 = LINE ( 'NONE', #61258, #27323 ) ;
#32289 = CARTESIAN_POINT ( 'NONE',  ( -43.60332556124591719, -117.0000000000000000, -2.500000000000000000 ) ) ;
#32290 = CARTESIAN_POINT ( 'NONE',  ( 96.32499999999998863, -207.7050326799711968, 83.51770833506763836 ) ) ;
#32291 = LINE ( 'NONE', #43245, #48120 ) ;
#32292 = CARTESIAN_POINT ( 'NONE',  ( 94.99999999999998579, 87.33691857156068750, 87.26156250086714294 ) ) ;
#32293 = CARTESIAN_POINT ( 'NONE',  ( 0.000000000000000000, -74.65491531819111515, -8.830959090343204920 ) ) ;
#32294 = FACE_OUTER_BOUND ( 'NONE', #14818, .T. ) ;
#32295 = CARTESIAN_POINT ( 'NONE',  ( 92.35000000000000853, -209.9999999999999716, 88.09499999999999886 ) ) ;
#32296 = DIRECTION ( 'NONE',  ( 0.000000000000000000, 0.000000000000000000, -1.000000000000000000 ) ) ;
#32297 = CIRCLE ( 'NONE', #64732, 2.055000000000000160 ) ;
#32298 = CARTESIAN_POINT ( 'NONE',  ( 95.00000000002596323, -209.9999999999999147, -74.99999999999349143 ) ) ;
#32299 = CARTESIAN_POINT ( 'NONE',  ( -92.35000000000005116, 88.47002178664754979, 87.80395833506766223 ) ) ;
#32300 =( BOUNDED_CURVE ( )  B_SPLINE_CURVE ( 2, ( #39713, #45735, #50600, #48834, #27676, #50979, #10759, #38965, #22410 ),
 .UNSPECIFIED., .F., .F. ) 
 B_SPLINE_CURVE_WITH_KNOTS ( ( 3, 2, 2, 2, 3 ),
 ( 0.4445132602971387792, 0.4515689946164713753, 0.4586247601573538724, 0.4656805256982363139, 0.4656806970056963091 ),
 .UNSPECIFIED. ) 
 CURVE ( )  GEOMETRIC_REPRESENTATION_ITEM ( )  RATIONAL_B_SPLINE_CURVE ( ( 0.9999988143381453032, 0.8660259966179892910, 1.000000000000000000, 0.8660254037844387076, 1.000000000000000000, 0.8660254037844387076, 1.000000000000000000, 0.9999967472207444974, 0.9999934945994379820 ) ) 
 REPRESENTATION_ITEM ( '' )  );
#32301 = DIRECTION ( 'NONE',  ( -7.705842312279274921E-15, 1.000000000000000000, -2.546204323184492723E-14 ) ) ;
#32302 = AXIS2_PLACEMENT_3D ( 'NONE', #54945, #3465, #9820 ) ;
#32303 = CARTESIAN_POINT ( 'NONE',  ( 92.35000000006144205, 90.00001182178868930, 76.10900611559256390 ) ) ;
#32304 = CIRCLE ( 'NONE', #74338, 37.49900000000000233 ) ;
#32305 = AXIS2_PLACEMENT_3D ( 'NONE', #5630, #56759, #5265 ) ;
#32306 = EDGE_CURVE ( 'NONE', #68440, #69078, #27994, .T. ) ;
#32307 = VECTOR ( 'NONE', #43509, 1000.000000000000114 ) ;
#32308 = FACE_OUTER_BOUND ( 'NONE', #42819, .T. ) ;
#32310 = VECTOR ( 'NONE', #6713, 1000.000000000000000 ) ;
#32309 = DIRECTION ( 'NONE',  ( -1.000000000000000000, 3.061616997868383141E-16, -0.000000000000000000 ) ) ;
#32311 = EDGE_CURVE ( 'NONE', #17108, #56237, #25502, .T. ) ;
#32312 = DIRECTION ( 'NONE',  ( -0.000000000000000000, -0.000000000000000000, 1.000000000000000000 ) ) ;
#32313 = CARTESIAN_POINT ( 'NONE',  ( -97.64999999999996305, -209.9999999999999716, 88.73000000000000398 ) ) ;
#32314 = CIRCLE ( 'NONE', #52721, 42.00000000000000000 ) ;
#32315 = ADVANCED_FACE ( 'NONE', ( #40393 ), #63341, .T. ) ;
#32316 = DIRECTION ( 'NONE',  ( 1.000000000000000000, 0.000000000000000000, 0.000000000000000000 ) ) ;
#32317 = EDGE_CURVE ( 'NONE', #59483, #26699, #41144, .T. ) ;
#32318 = CARTESIAN_POINT ( 'NONE',  ( -97.30629616937495996, -209.9999999999999716, 89.64281250086713726 ) ) ;
#32319 = DIRECTION ( 'NONE',  ( -1.000000000000000000, -0.000000000000000000, 0.000000000000000000 ) ) ;
#32320 = DIRECTION ( 'NONE',  ( -1.000000000000000000, -0.000000000000000000, -0.000000000000000000 ) ) ;
#32321 = CARTESIAN_POINT ( 'NONE',  ( 10.00000000000000000, 29.01471420065564644, 76.69515212746024702 ) ) ;
#32322 = AXIS2_PLACEMENT_3D ( 'NONE', #25912, #43955, #55597 ) ;
#32323 = VECTOR ( 'NONE', #23144, 1000.000000000000000 ) ;
#32324 = VECTOR ( 'NONE', #49854, 1000.000000000000000 ) ;
#32325 = ORIENTED_EDGE ( 'NONE', *, *, #53911, .T. ) ;
#32326 = AXIS2_PLACEMENT_3D ( 'NONE', #64268, #39862, #6746 ) ;
#32327 = VERTEX_POINT ( 'NONE', #68974 ) ;
#32328 = AXIS2_PLACEMENT_3D ( 'NONE', #25579, #42507, #54167 ) ;
#32329 = DIRECTION ( 'NONE',  ( 0.000000000000000000, -0.8090169943749433434, 0.5877852522924787992 ) ) ;
#32330 = CYLINDRICAL_SURFACE ( 'NONE', #67993, 77.49899999999999523 ) ;
#32331 = VERTEX_POINT ( 'NONE', #29464 ) ;
#32332 = CARTESIAN_POINT ( 'NONE',  ( 93.84685191531251292, -211.9973110713294489, 82.76364583420047438 ) ) ;
#32333 = CARTESIAN_POINT ( 'NONE',  ( 92.69370383062501162, -209.9999999999999716, 84.72156250086715090 ) ) ;
#32335 = ORIENTED_EDGE ( 'NONE', *, *, #47392, .F. ) ;
#32334 = EDGE_CURVE ( 'NONE', #54634, #50408, #52631, .T. ) ;
#32336 = CARTESIAN_POINT ( 'NONE',  ( 92.69370383062501162, -209.9999999999999716, 87.26156250086715715 ) ) ;
#32337 = ORIENTED_EDGE ( 'NONE', *, *, #3686, .F. ) ;
#32338 = LINE ( 'NONE', #55283, #31041 ) ;
#32339 = ORIENTED_EDGE ( 'NONE', *, *, #54896, .T. ) ;
#32340 = ADVANCED_FACE ( 'NONE', ( #40776 ), #7302, .T. ) ;
#32341 = EDGE_CURVE ( 'NONE', #5845, #54097, #56234, .T. ) ;
#32342 = CARTESIAN_POINT ( 'NONE',  ( -92.69370383062502583, 88.66845928578038638, 78.00114583420049996 ) ) ;
#32343 = ORIENTED_EDGE ( 'NONE', *, *, #6809, .F. ) ;
#32344 = VERTEX_POINT ( 'NONE', #70062 ) ;
#32345 = DIRECTION ( 'NONE',  ( -0.000000000000000000, -0.000000000000000000, -1.000000000000000000 ) ) ;
#32346 = ORIENTED_EDGE ( 'NONE', *, *, #7201, .F. ) ;
#32347 = DIRECTION ( 'NONE',  ( -1.000000000000000000, -0.000000000000000000, -0.000000000000000000 ) ) ;
#32348 = CYLINDRICAL_SURFACE ( 'NONE', #926, 31.99999999999998579 ) ;
#32349 = ORIENTED_EDGE ( 'NONE', *, *, #48147, .F. ) ;
#32350 = CARTESIAN_POINT ( 'NONE',  ( 0.000000000000000000, -14.66109333815513160, 73.73191006444567108 ) ) ;
#32351 = EDGE_CURVE ( 'NONE', #8457, #30109, #51388, .T. ) ;
#32352 = VERTEX_POINT ( 'NONE', #24582 ) ;
#32353 = DIRECTION ( 'NONE',  ( -1.000000000000000000, 0.000000000000000000, 0.000000000000000000 ) ) ;
#32354 = CIRCLE ( 'NONE', #47989, 82.00000000000000000 ) ;
#32355 = VERTEX_POINT ( 'NONE', #13297 ) ;
#32356 = AXIS2_PLACEMENT_3D ( 'NONE', #73435, #10289, #33209 ) ;
#32357 = CIRCLE ( 'NONE', #68407, 77.49899999999999523 ) ;
#32358 = VERTEX_POINT ( 'NONE', #46786 ) ;
#32359 = ORIENTED_EDGE ( 'NONE', *, *, #64968, .T. ) ;
#32360 = CARTESIAN_POINT ( 'NONE',  ( 93.84685191531251292, -211.9973110713294489, 76.41364583420048007 ) ) ;
#32361 = ITEM_DEFINED_TRANSFORMATION ( 'NONE', 'NONE', #53198,  #43395 ) ;
#32362 = FACE_BOUND ( 'NONE', #71344, .T. ) ;
#32363 = ORIENTED_EDGE ( 'NONE', *, *, #65266, .T. ) ;
#32364 = VERTEX_POINT ( 'NONE', #64081 ) ;
#32365 = AXIS2_PLACEMENT_3D ( 'NONE', #35369, #58294, #67821 ) ;
#32366 = ORIENTED_EDGE ( 'NONE', *, *, #7336, .T. ) ;
#32367 = FACE_OUTER_BOUND ( 'NONE', #19498, .T. ) ;
#32368 = LINE ( 'NONE', #3460, #11906 ) ;
#32369 = CARTESIAN_POINT ( 'NONE',  ( -96.15314808468751551, 88.00268892867056536, 79.74739583420048916 ) ) ;
#32370 = EDGE_LOOP ( 'NONE', ( #55421, #20775, #31509, #50923 ) ) ;
#32371 = CARTESIAN_POINT ( 'NONE',  ( 93.84685191531248449, 88.00268892867053694, 77.04864583420047097 ) ) ;
#32372 = ORIENTED_EDGE ( 'NONE', *, *, #64797, .F. ) ;
#32373 = CARTESIAN_POINT ( 'NONE',  ( -10.00000000000000000, 0.000000000000000000, 0.000000000000000000 ) ) ;
#32374 = CARTESIAN_POINT ( 'NONE',  ( -96.15314808468747287, -208.0026889286704943, 88.26697916753380468 ) ) ;
#32375 = CARTESIAN_POINT ( 'NONE',  ( -1.084202172485504434E-14, -5.773502691896260863, -2.080000000000000071 ) ) ;
#32376 = CARTESIAN_POINT ( 'NONE',  ( 10.00000000000000000, -21.53537804866103045, 30.80686688397002371 ) ) ;
#32377 = DIRECTION ( 'NONE',  ( 1.000000000000000000, -0.000000000000000000, 0.000000000000000000 ) ) ;
#32378 = CARTESIAN_POINT ( 'NONE',  ( -94.99999999999997158, -207.3369185715606307, 79.95906250086713385 ) ) ;
#32379 = VECTOR ( 'NONE', #14915, 1000.000000000000000 ) ;
#32380 = CARTESIAN_POINT ( 'NONE',  ( 0.000000000000000000, 0.000000000000000000, 42.00000000000001421 ) ) ;
#32381 = CARTESIAN_POINT ( 'NONE',  ( 4.999999999999999112, -9.188173127307592836, 40.98264845739746676 ) ) ;
#32382 = LINE ( 'NONE', #14365, #44309 ) ;
#32383 = VERTEX_POINT ( 'NONE', #63714 ) ;
#32384 = AXIS2_PLACEMENT_3D ( 'NONE', #64468, #12942, #17853 ) ;
#32385 = AXIS2_PLACEMENT_3D ( 'NONE', #5877, #74279, #56255 ) ;
#32386 = ORIENTED_EDGE ( 'NONE', *, *, #42339, .T. ) ;
#32387 = DIRECTION ( 'NONE',  ( -1.000000000000000000, 0.000000000000000000, -0.000000000000000000 ) ) ;
#32388 = AXIS2_PLACEMENT_3D ( 'NONE', #14788, #71556, #26066 ) ;
#32389 = AXIS2_PLACEMENT_3D ( 'NONE', #24388, #35299, #58976 ) ;
#32390 = DIRECTION ( 'NONE',  ( -8.783410004945701396E-16, -1.065814103640131188E-14, -1.000000000000000000 ) ) ;
#32391 = CARTESIAN_POINT ( 'NONE',  ( 93.98225765065697601, -207.8046129959941197, 74.85985921673515975 ) ) ;
#32392 = CARTESIAN_POINT ( 'NONE',  ( -96.15314808468751551, 88.00268892867056536, 83.39864583420047950 ) ) ;
#32393 = DIRECTION ( 'NONE',  ( -0.000000000000000000, -0.000000000000000000, -1.000000000000000000 ) ) ;
#32394 = DIRECTION ( 'NONE',  ( 0.000000000000000000, -0.1564344650402170744, -0.9876883405951398798 ) ) ;
#32395 = ORIENTED_EDGE ( 'NONE', *, *, #52804, .T. ) ;
#32396 = LINE ( 'NONE', #32026, #29366 ) ;
#32397 = LINE ( 'NONE', #9107, #60468 ) ;
#32398 = PLANE ( 'NONE',  #61001 ) ;
#32399 = EDGE_CURVE ( 'NONE', #66021, #56438, #41876, .T. ) ;
#32400 = DIRECTION ( 'NONE',  ( 0.5200609990132993854, 0.8541291221503275466, -0.000000000000000000 ) ) ;
#32401 = CARTESIAN_POINT ( 'NONE',  ( -20.30386590532152979, -102.9045904027214959, -5.500000000000000000 ) ) ;
#32402 = CARTESIAN_POINT ( 'NONE',  ( -93.84685191531247028, -211.9973110713294489, 84.29822916753381890 ) ) ;
#32403 = ADVANCED_FACE ( 'NONE', ( #47516 ), #584, .T. ) ;
#32404 = CARTESIAN_POINT ( 'NONE',  ( -97.64999999996709334, -209.9999916080759306, 86.90410584369134028 ) ) ;
#32405 = ADVANCED_FACE ( 'NONE', ( #69705 ), #18929, .F. ) ;
#32406 = VECTOR ( 'NONE', #43409, 1000.000000000000000 ) ;
#32407 = ORIENTED_EDGE ( 'NONE', *, *, #53499, .T. ) ;
#32408 = DIRECTION ( 'NONE',  ( 0.000000000000000000, 0.000000000000000000, -1.000000000000000000 ) ) ;
#32409 = LINE ( 'NONE', #2785, #31029 ) ;
#32410 = FACE_OUTER_BOUND ( 'NONE', #52330, .T. ) ;
#32411 = VERTEX_POINT ( 'NONE', #28738 ) ;
#32412 = CARTESIAN_POINT ( 'NONE',  ( 97.64999999999689351, 89.99999595380309358, 77.06187486178042434 ) ) ;
#32413 = CARTESIAN_POINT ( 'NONE',  ( 11.99999999999999822, -77.19088730480518734, -6.903761155838607166 ) ) ;
#32414 = AXIS2_PLACEMENT_3D ( 'NONE', #38511, #4691, #21577 ) ;
#32415 = CARTESIAN_POINT ( 'NONE',  ( 15.00000000000000000, -22.67460108101782978, -6.353146135317906840 ) ) ;
#32416 = CIRCLE ( 'NONE', #22737, 4.750000000000000000 ) ;
#32417 = CARTESIAN_POINT ( 'NONE',  ( 0.000000000000000000, 26.08949754953062694, -27.05870788708203989 ) ) ;
#32418 = EDGE_CURVE ( 'NONE', #52788, #69505, #18975, .T. ) ;
#32419 = VERTEX_POINT ( 'NONE', #46047 ) ;
#32420 = EDGE_CURVE ( 'NONE', #30682, #15051, #11782, .T. ) ;
#32421 = CARTESIAN_POINT ( 'NONE',  ( 0.000000000000000000, 0.000000000000000000, 0.000000000000000000 ) ) ;
#32422 = DIRECTION ( 'NONE',  ( 0.000000000000000000, 0.000000000000000000, 1.000000000000000000 ) ) ;
#32423 = EDGE_LOOP ( 'NONE', ( #30739, #7139 ) ) ;
#32424 = CYLINDRICAL_SURFACE ( 'NONE', #62831, 82.00000000000000000 ) ;
#32425 = CYLINDRICAL_SURFACE ( 'NONE', #60411, 42.00000000000000000 ) ;
#32426 = ORIENTED_EDGE ( 'NONE', *, *, #49204, .T. ) ;
#32427 = DIRECTION ( 'NONE',  ( -1.000000000000000000, -0.000000000000000000, -0.000000000000000000 ) ) ;
#32428 = AXIS2_PLACEMENT_3D ( 'NONE', #48937, #19264, #2764 ) ;
#32429 = EDGE_LOOP ( 'NONE', ( #23397, #28848, #25084, #34706 ) ) ;
#32430 = CARTESIAN_POINT ( 'NONE',  ( 3.000000000000000000, 2.201436576420041202, 1.270999999999998575 ) ) ;
#32431 = CIRCLE ( 'NONE', #2447, 42.00000000000000000 ) ;
#32432 = AXIS2_PLACEMENT_3D ( 'NONE', #7326, #70829, #65584 ) ;
#32433 = EDGE_CURVE ( 'NONE', #18122, #38079, #35491, .T. ) ;
#32434 = EDGE_CURVE ( 'NONE', #53274, #2804, #32059, .T. ) ;
#32435 = AXIS2_PLACEMENT_3D ( 'NONE', #38501, #72334, #43786 ) ;
#32436 = ORIENTED_EDGE ( 'NONE', *, *, #64614, .T. ) ;
#32437 = ORIENTED_EDGE ( 'NONE', *, *, #7982, .T. ) ;
#32438 = AXIS2_PLACEMENT_3D ( 'NONE', #4930, #51136, #74061 ) ;
#32439 = VERTEX_POINT ( 'NONE', #20040 ) ;
#32440 = ORIENTED_EDGE ( 'NONE', *, *, #3118, .F. ) ;
#32441 = CARTESIAN_POINT ( 'NONE',  ( 10.00000000000000000, -4.992566952385247170, 37.16516213103275845 ) ) ;
#32442 = VERTEX_POINT ( 'NONE', #9133 ) ;
#32443 = VERTEX_POINT ( 'NONE', #43378 ) ;
#32444 = CARTESIAN_POINT ( 'NONE',  ( 93.84685191531248449, 91.99731107132950569, 75.72572916753382799 ) ) ;
#32445 = CARTESIAN_POINT ( 'NONE',  ( 11.99999999999999822, -39.47590169984896846, 71.87247863392398983 ) ) ;
#32446 = CARTESIAN_POINT ( 'NONE',  ( 10.00000000000000000, 0.000000000000000000, 0.000000000000000000 ) ) ;
#32447 = ORIENTED_EDGE ( 'NONE', *, *, #43635, .F. ) ;
#32448 = VERTEX_POINT ( 'NONE', #71911 ) ;
#32449 = ORIENTED_EDGE ( 'NONE', *, *, #49056, .F. ) ;
#32450 = CARTESIAN_POINT ( 'NONE',  ( 96.15314808468748708, 88.00268892867053694, 87.31447916753380412 ) ) ;
#32451 = ORIENTED_EDGE ( 'NONE', *, *, #73476, .T. ) ;
#32452 = CARTESIAN_POINT ( 'NONE',  ( 96.15314808468748708, -208.0026889286704943, 88.16114583420046813 ) ) ;
#32453 = DIRECTION ( 'NONE',  ( 1.000000000000000000, -0.000000000000000000, -0.000000000000000000 ) ) ;
#32454 = CARTESIAN_POINT ( 'NONE',  ( -92.35000000000005116, 91.52997821335253548, 77.11479166840095445 ) ) ;
#32455 = DIRECTION ( 'NONE',  ( 0.000000000000000000, 0.1564344650402313408, -0.9876883405951376593 ) ) ;
#32456 = CARTESIAN_POINT ( 'NONE',  ( 5.000000000000000000, 2.886751345948125991, -6.000000000000000000 ) ) ;
#32457 = CARTESIAN_POINT ( 'NONE',  ( -97.64999999999996305, -209.9999999999999716, 83.01499999999998636 ) ) ;
#32458 = LINE ( 'NONE', #31351, #51469 ) ;
#32459 = CARTESIAN_POINT ( 'NONE',  ( -93.67499999999998295, -207.7050326799711968, 75.26270833506764291 ) ) ;
#32460 = CARTESIAN_POINT ( 'NONE',  ( -93.84685191531252713, 88.00268892867056536, 89.37822916753381719 ) ) ;
#32461 = ORIENTED_EDGE ( 'NONE', *, *, #30383, .T. ) ;
#32462 = UNCERTAINTY_MEASURE_WITH_UNIT (LENGTH_MEASURE( 1.000000000000000082E-05 ), #17078, 'distance_accuracy_value', 'NONE');
#32464 = CARTESIAN_POINT ( 'NONE',  ( -96.15314808468751551, 88.00268892867056536, 86.57364583420047666 ) ) ;
#32463 = CARTESIAN_POINT ( 'NONE',  ( 94.99999999999998579, 92.66308142843935514, 88.84906250086713442 ) ) ;
#32465 = ORIENTED_EDGE ( 'NONE', *, *, #12545, .T. ) ;
#32466 = CARTESIAN_POINT ( 'NONE',  ( 10.00000000000000000, -68.67312586195023982, 35.91791733033450384 ) ) ;
#32467 = CARTESIAN_POINT ( 'NONE',  ( 0.000000000000000000, -120.0000000000000000, 2.500000000000000000 ) ) ;
#32468 = DIRECTION ( 'NONE',  ( 1.000000000000000000, 1.427937372958405461E-15, 7.962523111839130290E-16 ) ) ;
#32469 = DIRECTION ( 'NONE',  ( -0.000000000000000000, -0.000000000000000000, 1.000000000000000000 ) ) ;
#32470 = DIRECTION ( 'NONE',  ( 0.000000000000000000, 0.000000000000000000, 1.000000000000000000 ) ) ;
#32471 = AXIS2_PLACEMENT_3D ( 'NONE', #63497, #62773, #34171 ) ;
#32472 = DIRECTION ( 'NONE',  ( -1.000000000000000000, 0.000000000000000000, 0.000000000000000000 ) ) ;
#32473 = CIRCLE ( 'NONE', #68506, 14.53333333333331545 ) ;
#32474 = CARTESIAN_POINT ( 'NONE',  ( 10.00000000000000000, -21.32104025579135964, 30.84782396557210760 ) ) ;
#32475 = VERTEX_POINT ( 'NONE', #65191 ) ;
#32476 = EDGE_LOOP ( 'NONE', ( #36483, #72569, #31738, #62814 ) ) ;
#32477 = CIRCLE ( 'NONE', #28895, 16.00000000000000355 ) ;
#32478 = B_SPLINE_CURVE_WITH_KNOTS ( 'NONE', 3,
 ( #36474, #14656, #7910, #47402, #48868, #71052 ),
 .UNSPECIFIED., .F., .F.,
 ( 4, 2, 4 ),
 ( 0.7528176110416423539, 0.8153862273022710605, 0.8779548435628997671 ),
 .UNSPECIFIED. ) ;
#32479 = CARTESIAN_POINT ( 'NONE',  ( -97.65000000000001990, 90.00000000000004263, 82.37999999999999545 ) ) ;
#32480 = LINE ( 'NONE', #42307, #59552 ) ;
#32481 = CARTESIAN_POINT ( 'NONE',  ( 10.00000000000000000, 0.000000000000000000, 0.000000000000000000 ) ) ;
#32482 = CARTESIAN_POINT ( 'NONE',  ( 92.35000000000000853, -209.9999999999999716, 88.17437500173430465 ) ) ;
#32483 = ADVANCED_FACE ( 'NONE', ( #54276, #20425, #8408 ), #53899, .F. ) ;
#32484 = DIRECTION ( 'NONE',  ( 1.000000000000000000, 0.000000000000000000, 0.000000000000000000 ) ) ;
#32485 = CARTESIAN_POINT ( 'NONE',  ( 0.000000000000000000, 16.45098606841126454, 33.79645857604518966 ) ) ;
#32486 = DIRECTION ( 'NONE',  ( 0.000000000000000000, -0.4539904997395541875, 0.8910065241883641241 ) ) ;
#32487 = ORIENTED_EDGE ( 'NONE', *, *, #8054, .F. ) ;
#32488 = CARTESIAN_POINT ( 'NONE',  ( -95.00000000000002842, 87.33691857156074434, 81.54656250086715374 ) ) ;
#32489 = EDGE_CURVE ( 'NONE', #17385, #24964, #37359, .T. ) ;
#32490 = AXIS2_PLACEMENT_3D ( 'NONE', #31929, #9370, #15761 ) ;
#32491 = CARTESIAN_POINT ( 'NONE',  ( 97.64999999997402824, 89.99998827382246702, 82.77687459617033028 ) ) ;
#32492 = AXIS2_PLACEMENT_3D ( 'NONE', #50773, #62835, #11656 ) ;
#32493 = LINE ( 'NONE', #26491, #54681 ) ;
#32494 = AXIS2_PLACEMENT_3D ( 'NONE', #58277, #28961, #69557 ) ;
#32495 = CARTESIAN_POINT ( 'NONE',  ( -95.00000000000002842, 93.05995642670504253, 79.04624999999997215 ) ) ;
#32496 = EDGE_CURVE ( 'NONE', #70917, #51144, #53805, .T. ) ;
#32497 = CARTESIAN_POINT ( 'NONE',  ( 26.28306158492127764, -123.3838844133976522, -2.500000000000000000 ) ) ;
#32498 = CARTESIAN_POINT ( 'NONE',  ( -95.00000000000002842, 93.05995642670504253, 82.22124999999999773 ) ) ;
#32499 = CARTESIAN_POINT ( 'NONE',  ( 10.00000000000000000, 22.74946021919175720, -29.81001611430984255 ) ) ;
#32500 = CARTESIAN_POINT ( 'NONE',  ( 11.99999999999999822, 0.000000000000000000, 0.000000000000000000 ) ) ;
#32501 = AXIS2_PLACEMENT_3D ( 'NONE', #43368, #36962, #66289 ) ;
#32502 = DIRECTION ( 'NONE',  ( 1.000000000000000000, 0.000000000000000000, -0.000000000000000000 ) ) ;
#32503 = EDGE_CURVE ( 'NONE', #69736, #68378, #17801, .T. ) ;
#32504 = ADVANCED_FACE ( 'NONE', ( #66299 ), #30580, .T. ) ;
#32505 = CARTESIAN_POINT ( 'NONE',  ( 96.15314808468748708, 91.99731107132950569, 81.96989583420048575 ) ) ;
#32506 = CARTESIAN_POINT ( 'NONE',  ( -93.84685191531248449, -208.0026889286704943, 83.23989583420049598 ) ) ;
#32507 = CARTESIAN_POINT ( 'NONE',  ( 10.00000000000000000, 26.01480285779837232, 70.53064760720326376 ) ) ;
#32508 = ORIENTED_EDGE ( 'NONE', *, *, #4684, .F. ) ;
#32509 = LINE ( 'NONE', #14482, #5305 ) ;
#32510 = CARTESIAN_POINT ( 'NONE',  ( -96.32499999999996021, -212.2949673200287179, 77.40583333333331950 ) ) ;
#32511 = DIRECTION ( 'NONE',  ( 1.000000000000000000, 0.000000000000000000, 0.000000000000000000 ) ) ;
#32512 = CARTESIAN_POINT ( 'NONE',  ( -96.15314808468751551, 88.00268892867056536, 79.11239583420048405 ) ) ;
#32514 = EDGE_CURVE ( 'NONE', #31776, #64448, #3527, .T. ) ;
#32513 = CARTESIAN_POINT ( 'NONE',  ( 95.00000000000000000, -212.6630814284392557, 82.18156250086714465 ) ) ;
#32515 = ORIENTED_EDGE ( 'NONE', *, *, #71300, .F. ) ;
#32516 = EDGE_CURVE ( 'NONE', #9438, #26686, #20205, .T. ) ;
#32517 = EDGE_LOOP ( 'NONE', ( #65671, #17286, #68154, #42242 ) ) ;
#32518 = CARTESIAN_POINT ( 'NONE',  ( 4.999999999999999112, -16.65560815589383381, -38.55633173627028754 ) ) ;
#32519 = ORIENTED_EDGE ( 'NONE', *, *, #58091, .T. ) ;
#32520 = VECTOR ( 'NONE', #32208, 1000.000000000000000 ) ;
#32521 = AXIS2_PLACEMENT_3D ( 'NONE', #62170, #10655, #73433 ) ;
#32523 = VECTOR ( 'NONE', #20480, 1000.000000000000000 ) ;
#32522 = LINE ( 'NONE', #8863, #46573 ) ;
#32524 = ORIENTED_EDGE ( 'NONE', *, *, #14749, .F. ) ;
#32525 = VERTEX_POINT ( 'NONE', #14776 ) ;
#32526 = CARTESIAN_POINT ( 'NONE',  ( 96.66079198124941740, -211.6002412367799934, 74.80065669543249385 ) ) ;
#32527 = LINE ( 'NONE', #43835, #11673 ) ;
#32528 = CARTESIAN_POINT ( 'NONE',  ( 0.000000000000000000, 73.44644590900092851, -24.73286445877629092 ) ) ;
#32529 = DIRECTION ( 'NONE',  ( 0.000000000000000000, 0.000000000000000000, 1.000000000000000000 ) ) ;
#32530 =( BOUNDED_CURVE ( )  B_SPLINE_CURVE ( 2, ( #26833, #50879, #49759, #27580, #67435, #50120, #32836, #56911, #55787, #39615, #4306, #15930, #33210, #56155, #72681, #21182, #73804, #15184, #4673, #38119, #62557, #61057, #73436, #39243, #44886, #62173, #22317, #11040, #45260, #33963, #46733, #1287, #11399, #29060, #52738, #63666, #6154, #12507, #18151, #34332, #23431, #6512, #23070, #35444, #57273, #51627, #58373, #24173, #5780, #62940, #34700, #51987, #45998, #28686, #17776, #22697, #30164, #45643, #178, #64398, #535, #68926, #47107, #17415, #29785, #40348, #29412, #46362, #69290, #63293, #35798, #57652, #18514, #11753, #40722, #12135, #35078, #58008, #52360, #6872, #7252, #907, #70012, #23793, #69658, #41099, #17049, #41456, #64031, #12868, #58754, #53110, #68561, #39984, #59490, #7981, #1647, #18880, #43331, #8726, #37311, #54587, #66248, #59127, #9087, #30898, #14361, #36543, #26006, #25282, #13251, #42208, #60246, #70750, #71119, #37674, #2389, #24901, #48931, #53842, #48206, #7614, #32010, #31642, #24533, #47469, #36920, #30528, #13616, #54226, #3112, #14724, #19623, #48577, #65877, #2014, #59868, #60608, #70375, #71489, #8355, #53478, #71855, #20371, #41819, #19257, #42569, #64765, #47829, #25641, #65509, #65143, #36179, #13976, #31277, #2757, #19989, #42944, #43689, #61347, #10564, #67345, #38032, #56066, #44050, #10950, #44424, #38775, #55321, #67719, #66609, #9454, #16209, #33486, #15090, #20738, #66966, #38406, #3839, #60962, #50034, #62469, #54950, #32378, #22225, #9826, #49305, #61711, #39149, #16583, #21093, #56449, #26739, #4582, #72591, #3471, #15845, #10196, #33118, #73713, #62088, #32744, #49667, #15462, #4958, #39526, #55695, #27481, #4211, #50416, #45167, #27102, #72961, #21463, #21849, #73342, #26375, #44797, #27858, #50786, #68092, #72231, #51157, #1197, #41011, #69569, #52275, #45915, #40634, #11311, #35365, #6783, #29697, #28227, #34244, #41374, #34993, #450, #46641, #28975, #52646, #34610, #57188, #58289, #63209, #57560, #74091, #5693, #28595, #6431, #51907, #6069, #12051, #92, #24093, #62851, #5329, #23347, #68472, #18429, #63574, #17696, #69927, #64310, #29331, #57928, #63944, #18068, #47017, #68841, #33875, #51536, #17328, #40260, #11670, #39900, #22984, #12421, #56821, #46274, #819, #16963, #23705 ),
 .UNSPECIFIED., .F., .F. ) 
 B_SPLINE_CURVE_WITH_KNOTS ( ( 3, 2, 2, 2, 2, 2, 2, 2, 2, 2, 2, 2, 2, 2, 2, 2, 2, 2, 2, 2, 2, 2, 2, 2, 2, 2, 2, 2, 2, 2, 2, 2, 2, 2, 2, 2, 2, 2, 2, 2, 2, 2, 2, 2, 2, 2, 2, 2, 2, 2, 2, 2, 2, 2, 2, 2, 2, 2, 2, 2, 2, 2, 2, 2, 2, 2, 2, 2, 2, 2, 2, 2, 2, 2, 2, 2, 2, 2, 2, 2, 2, 2, 2, 2, 2, 2, 2, 2, 2, 2, 2, 2, 2, 2, 2, 2, 2, 2, 2, 2, 2, 2, 2, 2, 2, 2, 2, 2, 2, 2, 2, 2, 2, 2, 2, 2, 2, 2, 2, 2, 2, 2, 2, 2, 2, 2, 2, 2, 2, 2, 2, 2, 2, 2, 2, 2, 2, 2, 2, 2, 2, 3 ),
 ( 0.000000000000000000, 0.007055765384978172905, 0.01411153076995634581, 0.02116729615493451871, 0.02822306153991269162, 0.03527882692489087146, 0.04233459230986903743, 0.04939035769484721727, 0.05644612307982538324, 0.06350188846480356308, 0.07055765384978174293, 0.07761341923475992277, 0.08466918461973807486, 0.09172495000471626858, 0.09878071538969443455, 0.1058364807746726144, 0.1128922461596507665, 0.1199480115446289602, 0.1270037769296071262, 0.1340595423145853060, 0.1411153076995634859, 0.1481710730845416657, 0.1552268384695198455, 0.1622826038544979699, 0.1693383692394761497, 0.1763941346244543296, 0.1834499000094325372, 0.1905056653944106893, 0.1975614307793888691, 0.2046171961643670489, 0.2116729615493452288, 0.2187287269343233809, 0.2257844923193015330, 0.2328402577042797406, 0.2398960230892579204, 0.2469517884742360725, 0.2540075538592142523, 0.2610633192441924044, 0.2681190846291706120, 0.2751748500141487641, 0.2822306153991269717, 0.2892863807841050683, 0.2963421461690833314, 0.3033979115540614280, 0.3104536769390396911, 0.3175094423240178432, 0.3245652077089959398, 0.3316209730939742029, 0.3386767384789522994, 0.3457325038639305625, 0.3527882692489086591, 0.3598440346338868667, 0.3668998000188650743, 0.3739555654038432264, 0.3810113307888213785, 0.3880670961737995306, 0.3951228615587777382, 0.4021786269437558903, 0.4092343923287340979, 0.4162901577137122500, 0.4233459230986904576, 0.4304016884836686097, 0.4374574538686467617, 0.4445132192536249693, 0.4515689846386030659, 0.4586247500235813290, 0.4656805154085594811, 0.4727362807935376332, 0.4797920461785158408, 0.4868478115634939929, 0.4939035769484721450, 0.5009593423334502971, 0.5080151077184285047, 0.5150708731034067123, 0.5221266384883848088, 0.5291824038733630164, 0.5362381692583412240, 0.5432939346433194316, 0.5503497000282975282, 0.5574054654132757358, 0.5644612307982539434, 0.5715169961832320400, 0.5785727615682101366, 0.5856285269531884552, 0.5926842923381666628, 0.5997400577231447594, 0.6067958231081228559, 0.6138515884931010635, 0.6209073538780793822, 0.6279631192630574787, 0.6350188846480356863, 0.6420746500330137829, 0.6491304154179918795, 0.6561861808029701981, 0.6632419461879484057, 0.6702977115729265023, 0.6773534769579045989, 0.6844092423428829175, 0.6914650077278611251, 0.6985207731128392217, 0.7055765384978173183, 0.7126323038827955259, 0.7196880692677737335, 0.7267438346527518300, 0.7337996000377301486, 0.7408553654227082452, 0.7479111308076864528, 0.7549668961926645494, 0.7620226615776427570, 0.7690784269626209646, 0.7761341923475990612, 0.7831899577325773798, 0.7902457231175554764, 0.7973014885025335730, 0.8043572538875117806, 0.8114130192724900992, 0.8184687846574681958, 0.8255245500424462923, 0.8325803154274244999, 0.8396360808124025965, 0.8466918461973809151, 0.8537476115823590117, 0.8608033769673372193, 0.8678591423523153159, 0.8749149077372935235, 0.8819706731222718421, 0.8890264385072499387, 0.8960822038922280353, 0.9031379692772061318, 0.9101937346621844505, 0.9172495000471626581, 0.9243052654321407546, 0.9313610308171189622, 0.9384167962020971698, 0.9454725615870752664, 0.9525283269720534740, 0.9595840923570316816, 0.9666398577420097782, 0.9736956231269879858, 0.9807513885119661934, 0.9878071538969442900, 0.9900635123082156541 ),
 .UNSPECIFIED. ) 
 CURVE ( )  GEOMETRIC_REPRESENTATION_ITEM ( )  RATIONAL_B_SPLINE_CURVE ( ( 1.000000000000000000, 0.8660254037844387076, 1.000000000000000000, 0.8660254037844387076, 1.000000000000000000, 0.8660254037844387076, 1.000000000000000000, 0.8660254037844387076, 1.000000000000000000, 0.8660254037844387076, 1.000000000000000000, 0.8660254037844387076, 1.000000000000000000, 0.8660254037844387076, 1.000000000000000000, 0.8660254037844387076, 1.000000000000000000, 0.8660254037844387076, 1.000000000000000000, 0.8660254037844387076, 1.000000000000000000, 0.8660254037844387076, 1.000000000000000000, 0.8660254037844387076, 1.000000000000000000, 0.8660254037844387076, 1.000000000000000000, 0.8660254037844387076, 1.000000000000000000, 0.8660254037844387076, 1.000000000000000000, 0.8660254037844387076, 1.000000000000000000, 0.8660254037844387076, 1.000000000000000000, 0.8660254037844387076, 1.000000000000000000, 0.8660254037844387076, 1.000000000000000000, 0.8660254037844387076, 1.000000000000000000, 0.8660254037844387076, 1.000000000000000000, 0.8660254037844387076, 1.000000000000000000, 0.8660254037844387076, 1.000000000000000000, 0.8660254037844387076, 1.000000000000000000, 0.8660254037844387076, 1.000000000000000000, 0.8660254037844387076, 1.000000000000000000, 0.8660254037844387076, 1.000000000000000000, 0.8660254037844387076, 1.000000000000000000, 0.8660254037844387076, 1.000000000000000000, 0.8660254037844387076, 1.000000000000000000, 0.8660254037844387076, 1.000000000000000000, 0.8660254037844387076, 1.000000000000000000, 0.8660254037844387076, 1.000000000000000000, 0.8660254037844387076, 1.000000000000000000, 0.8660254037844387076, 1.000000000000000000, 0.8660254037844387076, 1.000000000000000000, 0.8660254037844387076, 1.000000000000000000, 0.8660254037844387076, 1.000000000000000000, 0.8660254037844387076, 1.000000000000000000, 0.8660254037844387076, 1.000000000000000000, 0.8660254037844387076, 1.000000000000000000, 0.8660254037844387076, 1.000000000000000000, 0.8660254037844387076, 1.000000000000000000, 0.8660254037844387076, 1.000000000000000000, 0.8660254037844387076, 1.000000000000000000, 0.8660254037844387076, 1.000000000000000000, 0.8660254037844387076, 1.000000000000000000, 0.8660254037844387076, 1.000000000000000000, 0.8660254037844387076, 1.000000000000000000, 0.8660254037844387076, 1.000000000000000000, 0.8660254037844387076, 1.000000000000000000, 0.8660254037844387076, 1.000000000000000000, 0.8660254037844387076, 1.000000000000000000, 0.8660254037844387076, 1.000000000000000000, 0.8660254037844387076, 1.000000000000000000, 0.8660254037844387076, 1.000000000000000000, 0.8660254037844387076, 1.000000000000000000, 0.8660254037844387076, 1.000000000000000000, 0.8660254037844387076, 1.000000000000000000, 0.8660254037844387076, 1.000000000000000000, 0.8660254037844387076, 1.000000000000000000, 0.8660254037844387076, 1.000000000000000000, 0.8660254037844387076, 1.000000000000000000, 0.8660254037844387076, 1.000000000000000000, 0.8660254037844387076, 1.000000000000000000, 0.8660254037844387076, 1.000000000000000000, 0.8660254037844387076, 1.000000000000000000, 0.8660254037844387076, 1.000000000000000000, 0.8660254037844387076, 1.000000000000000000, 0.8660254037844387076, 1.000000000000000000, 0.8660254037844387076, 1.000000000000000000, 0.8660254037844387076, 1.000000000000000000, 0.8660254037844387076, 1.000000000000000000, 0.8660254037844387076, 1.000000000000000000, 0.8660254037844387076, 1.000000000000000000, 0.8660254037844387076, 1.000000000000000000, 0.8660254037844387076, 1.000000000000000000, 0.8660254037844387076, 1.000000000000000000, 0.8660254037844387076, 1.000000000000000000, 0.8660254037844387076, 1.000000000000000000, 0.8660254037844387076, 1.000000000000000000, 0.8660254037844387076, 1.000000000000000000, 0.8660254037844387076, 1.000000000000000000, 0.8660254037844387076, 1.000000000000000000, 0.8660254037844387076, 1.000000000000000000, 0.8660254037844387076, 1.000000000000000000, 0.8660254037844387076, 1.000000000000000000, 0.8660254037844387076, 1.000000000000000000, 0.8660254037844387076, 1.000000000000000000, 0.8660254037844387076, 1.000000000000000000, 0.8660254037844387076, 1.000000000000000000, 0.8660254037844387076, 1.000000000000000000, 0.8660254037844387076, 1.000000000000000000, 0.8660254037844387076, 1.000000000000000000, 0.8660254037844387076, 1.000000000000000000, 0.8660254037844387076, 1.000000000000000000, 0.8660254037844387076, 1.000000000000000000, 0.8660254037844387076, 1.000000000000000000, 0.8660254037844387076, 1.000000000000000000, 0.8660254037844387076, 1.000000000000000000, 0.8660254037844387076, 1.000000000000000000, 0.8660254037844387076, 1.000000000000000000, 0.8660254037844387076, 1.000000000000000000, 0.8660254037844387076, 1.000000000000000000, 0.8660254037844387076, 1.000000000000000000, 0.8660254037844387076, 1.000000000000000000, 0.8660254037844387076, 1.000000000000000000, 0.8660254037844387076, 1.000000000000000000, 0.8660254037844387076, 1.000000000000000000, 0.8660254037844387076, 1.000000000000000000, 0.8660254037844387076, 1.000000000000000000, 0.8660254037844387076, 1.000000000000000000, 0.8660254037844387076, 1.000000000000000000, 0.8660254037844387076, 1.000000000000000000, 0.8660254037844387076, 1.000000000000000000, 0.8660254037844387076, 1.000000000000000000, 0.8660254037844387076, 1.000000000000000000, 0.8660254037844387076, 1.000000000000000000, 0.8660254037844387076, 1.000000000000000000, 0.8660254037844387076, 1.000000000000000000, 0.8660254037844387076, 1.000000000000000000, 0.8660254037844387076, 1.000000000000000000, 0.8660254037844387076, 1.000000000000000000, 0.8660254037844387076, 1.000000000000000000, 0.8660254037844387076, 1.000000000000000000, 0.8660254037844387076, 1.000000000000000000, 0.8660254037844387076, 1.000000000000000000, 0.8660254037844387076, 1.000000000000000000, 0.8660254037844387076, 1.000000000000000000, 0.8660254037844387076, 1.000000000000000000, 0.8660254037844387076, 1.000000000000000000, 0.8660254037844387076, 1.000000000000000000, 0.8660254037844387076, 1.000000000000000000, 0.8660254037844387076, 1.000000000000000000, 0.8660254037844387076, 1.000000000000000000, 0.8660254037844387076, 1.000000000000000000, 0.8660254037844387076, 1.000000000000000000, 0.8660254037844387076, 1.000000000000000000, 0.8660254037844387076, 1.000000000000000000, 0.8660254037844387076, 1.000000000000000000, 0.9571563550410487897, 0.9417145902178700734 ) ) 
 REPRESENTATION_ITEM ( '' )  );
#32531 = CARTESIAN_POINT ( 'NONE',  ( 93.84685191531248449, 91.99731107132950569, 87.15572916753382060 ) ) ;
#32532 = CARTESIAN_POINT ( 'NONE',  ( 96.32499999999998863, 87.70503267997126784, 75.05104166840095559 ) ) ;
#32533 = CARTESIAN_POINT ( 'NONE',  ( 93.67500000000001137, -212.2949673200287179, 83.12083333333332291 ) ) ;
#32534 = VERTEX_POINT ( 'NONE', #20788 ) ;
#32535 = ORIENTED_EDGE ( 'NONE', *, *, #51, .T. ) ;
#32536 = VERTEX_POINT ( 'NONE', #26429 ) ;
#32537 = ORIENTED_EDGE ( 'NONE', *, *, #38320, .T. ) ;
#32538 = CARTESIAN_POINT ( 'NONE',  ( -12.49999999999999645, 0.000000000000000000, 125.0000000000000000 ) ) ;
#32539 = AXIS2_PLACEMENT_3D ( 'NONE', #46832, #12601, #18245 ) ;
#32540 = CIRCLE ( 'NONE', #42169, 77.49899999999999523 ) ;
#32541 =( NAMED_UNIT ( * ) PLANE_ANGLE_UNIT ( ) SI_UNIT ( $, .RADIAN. ) );
#32542 = CARTESIAN_POINT ( 'NONE',  ( 92.35000000001610942, 89.99999393654047708, 88.17456390440148084 ) ) ;
#32543 = VECTOR ( 'NONE', #16147, 1000.000000000000114 ) ;
#32544 = DIRECTION ( 'NONE',  ( 2.603472992746261562E-14, 2.546204323184492723E-14, -1.000000000000000000 ) ) ;
#32545 = DIRECTION ( 'NONE',  ( -1.000000000000000000, 0.000000000000000000, 0.000000000000000000 ) ) ;
#32546 = ORIENTED_EDGE ( 'NONE', *, *, #48734, .T. ) ;
#32547 = CARTESIAN_POINT ( 'NONE',  ( -97.64999999999994884, -208.4700217866474645, 86.85145833506763324 ) ) ;
#32548 = ORIENTED_EDGE ( 'NONE', *, *, #8498, .T. ) ;
#32549 = DIRECTION ( 'NONE',  ( 0.000000000000000000, 0.000000000000000000, 1.000000000000000000 ) ) ;
#32550 = ORIENTED_EDGE ( 'NONE', *, *, #68532, .T. ) ;
#32551 = CARTESIAN_POINT ( 'NONE',  ( -92.35000000000003695, 90.00000000000004263, 84.04687500173430692 ) ) ;
#32552 = AXIS2_PLACEMENT_3D ( 'NONE', #66184, #49245, #49606 ) ;
#32553 = VERTEX_POINT ( 'NONE', #49358 ) ;
#32554 = CARTESIAN_POINT ( 'NONE',  ( 92.69370383062498320, 88.66845928578037217, 82.23447916753383424 ) ) ;
#32555 = DIRECTION ( 'NONE',  ( 1.000000000000000000, 0.000000000000000000, 0.000000000000000000 ) ) ;
#32557 = EDGE_CURVE ( 'NONE', #19049, #29007, #48981, .T. ) ;
#32556 = DIRECTION ( 'NONE',  ( -1.000000000000000000, -0.000000000000000000, 0.000000000000000000 ) ) ;
#32558 = DIRECTION ( 'NONE',  ( 0.000000000000000000, 0.5877852522924689183, 0.8090169943749504489 ) ) ;
#32559 = CYLINDRICAL_SURFACE ( 'NONE', #19827, 31.99999999999998579 ) ;
#32560 = CARTESIAN_POINT ( 'NONE',  ( 92.35000000001610942, 89.99999393654047708, 88.17456390440148084 ) ) ;
#32561 = VERTEX_POINT ( 'NONE', #25690 ) ;
#32562 = DIRECTION ( 'NONE',  ( -1.000000000000000000, 0.000000000000000000, 0.000000000000000000 ) ) ;
#32563 = FACE_OUTER_BOUND ( 'NONE', #18026, .T. ) ;
#32564 = ORIENTED_EDGE ( 'NONE', *, *, #2727, .T. ) ;
#32565 = ORIENTED_EDGE ( 'NONE', *, *, #4006, .F. ) ;
#32566 = EDGE_CURVE ( 'NONE', #53902, #20797, #10602, .T. ) ;
#32567 = ADVANCED_FACE ( 'NONE', ( #36229 ), #48257, .T. ) ;
#32568 = CARTESIAN_POINT ( 'NONE',  ( 11.99999999999999822, -69.42325613327415113, -34.44570377933671779 ) ) ;
#32569 = CARTESIAN_POINT ( 'NONE',  ( 23.49955575014914189, 0.001194404164656991856, -64.99999999999938893 ) ) ;
#32570 = DIRECTION ( 'NONE',  ( 0.000000000000000000, 0.000000000000000000, 1.000000000000000000 ) ) ;
#32571 = CARTESIAN_POINT ( 'NONE',  ( -93.84685191531248449, -208.0026889286704943, 84.50989583420049200 ) ) ;
#32572 = ORIENTED_EDGE ( 'NONE', *, *, #71288, .F. ) ;
#32573 = CYLINDRICAL_SURFACE ( 'NONE', #15303, 16.00000000000000000 ) ;
#32574 = ORIENTED_EDGE ( 'NONE', *, *, #53831, .T. ) ;
#32575 = ADVANCED_FACE ( 'NONE', ( #42258 ), #36596, .T. ) ;
#32576 = STYLED_ITEM ( 'NONE', ( #35470 ), #28332 ) ;
#32577 = VECTOR ( 'NONE', #12132, 1000.000000000000000 ) ;
#32578 = FACE_OUTER_BOUND ( 'NONE', #70728, .T. ) ;
#32579 = VECTOR ( 'NONE', #18529, 1000.000000000000000 ) ;
#32580 = CARTESIAN_POINT ( 'NONE',  ( 11.99999999999999822, 59.75363087400075557, 56.15606465354979093 ) ) ;
#32581 = AXIS2_PLACEMENT_3D ( 'NONE', #29071, #58019, #28702 ) ;
#32582 = DIRECTION ( 'NONE',  ( -1.000000000000000000, -1.224646799147354193E-16, 0.000000000000000000 ) ) ;
#32583 = CARTESIAN_POINT ( 'NONE',  ( 94.99999999999998579, 87.33691857156068750, 78.37156250086714238 ) ) ;
#32584 = CARTESIAN_POINT ( 'NONE',  ( 10.00000000000000000, -30.84782396557233142, 21.32104025579104345 ) ) ;
#32585 = DIRECTION ( 'NONE',  ( -0.000000000000000000, 0.9781476007338064660, 0.2079116908177554846 ) ) ;
#32586 = LINE ( 'NONE', #2949, #48153 ) ;
#32587 = DIRECTION ( 'NONE',  ( 1.000000000000000000, 0.000000000000000000, 0.000000000000000000 ) ) ;
#32588 = DIRECTION ( 'NONE',  ( 0.000000000000000000, 0.000000000000000000, 1.000000000000000000 ) ) ;
#32589 = FACE_OUTER_BOUND ( 'NONE', #59374, .T. ) ;
#32590 = AXIS2_PLACEMENT_3D ( 'NONE', #33677, #50215, #55504 ) ;
#32591 =( REPRESENTATION_RELATIONSHIP ('NONE','NONE', #31117, #51769 ) REPRESENTATION_RELATIONSHIP_WITH_TRANSFORMATION ( #48913 )SHAPE_REPRESENTATION_RELATIONSHIP( ) );
#32592 = EDGE_CURVE ( 'NONE', #31980, #74050, #65555, .T. ) ;
#32593 = LINE ( 'NONE', #20586, #36033 ) ;
#32594 = LINE ( 'NONE', #4054, #6995 ) ;
#32595 = CARTESIAN_POINT ( 'NONE',  ( 92.34999999999999432, 90.00000000000002842, 76.74437500173429783 ) ) ;
#32596 = VERTEX_POINT ( 'NONE', #71539 ) ;
#32597 = CARTESIAN_POINT ( 'NONE',  ( -95.00000000000002842, 87.33691857156074434, 83.45156250086714067 ) ) ;
#32598 = AXIS2_PLACEMENT_3D ( 'NONE', #21564, #62562, #62176 ) ;
#32599 = DIRECTION ( 'NONE',  ( 0.000000000000000000, 0.8090169943749487835, -0.5877852522924712497 ) ) ;
#32600 = CIRCLE ( 'NONE', #8575, 37.49900000000000233 ) ;
#32602 = EDGE_CURVE ( 'NONE', #15417, #8203, #14408, .T. ) ;
#32601 = CARTESIAN_POINT ( 'NONE',  ( 0.000000000000000000, -35.47612816024539484, 22.48208911017487921 ) ) ;
#32603 = EDGE_CURVE ( 'NONE', #1809, #24727, #3160, .T. ) ;
#32604 = ORIENTED_EDGE ( 'NONE', *, *, #8088, .T. ) ;
#32605 = CARTESIAN_POINT ( 'NONE',  ( 0.000000000000000000, 1.732050807568878747, 7.017607234860990640E-28 ) ) ;
#32606 = ADVANCED_FACE ( 'NONE', ( #5004 ), #74138, .F. ) ;
#32607 = DIRECTION ( 'NONE',  ( -1.000000000000000000, -0.000000000000000000, -0.000000000000000000 ) ) ;
#32608 = FACE_OUTER_BOUND ( 'NONE', #43757, .T. ) ;
#32609 = CARTESIAN_POINT ( 'NONE',  ( 92.35004028547584198, 88.46999852781718232, 83.14729327728632313 ) ) ;
#32610 = CARTESIAN_POINT ( 'NONE',  ( 92.69370383062501162, -211.3315407142195852, 77.78947916753381264 ) ) ;
#32611 = EDGE_LOOP ( 'NONE', ( #20804, #58060, #8043, #10341 ) ) ;
#32612 = ORIENTED_EDGE ( 'NONE', *, *, #14868, .F. ) ;
#32613 = CARTESIAN_POINT ( 'NONE',  ( 10.00000000000000000, -69.42325613327415113, -34.44570377933673910 ) ) ;
#32614 = DIRECTION ( 'NONE',  ( -1.000000000000000000, 0.000000000000000000, 0.000000000000000000 ) ) ;
#32615 = DIRECTION ( 'NONE',  ( 1.000000000000000000, -0.000000000000000000, 0.000000000000000000 ) ) ;
#32616 = DIRECTION ( 'NONE',  ( 0.000000000000000000, 0.000000000000000000, 1.000000000000000000 ) ) ;
#32617 = CARTESIAN_POINT ( 'NONE',  ( 97.30629616937498838, -209.9999999999999716, 77.41906250086715602 ) ) ;
#32618 = COLOUR_RGB ( '', 0.08235294, 0.09019608, 0.10196078) ;
#32619 = ORIENTED_EDGE ( 'NONE', *, *, #40158, .F. ) ;
#32620 = DIRECTION ( 'NONE',  ( 0.000000000000000000, -1.000000000000000000, 0.000000000000000000 ) ) ;
#32621 = EDGE_LOOP ( 'NONE', ( #10576, #33100, #65847, #12761 ) ) ;
#32622 = VERTEX_POINT ( 'NONE', #56501 ) ;
#32623 = CARTESIAN_POINT ( 'NONE',  ( 10.00000000000000000, -2.946379043145784582, -75.11764819372150725 ) ) ;
#32624 = AXIS2_PLACEMENT_3D ( 'NONE', #60534, #36109, #7541 ) ;
#32625 = FILL_AREA_STYLE ('',( #61223 ) ) ;
#32626 = CARTESIAN_POINT ( 'NONE',  ( 0.000000000000000000, 26.08949754953062694, -27.05870788708203989 ) ) ;
#32627 = ORIENTED_EDGE ( 'NONE', *, *, #39463, .F. ) ;
#32628 = DIRECTION ( 'NONE',  ( -1.000000000000000000, 0.000000000000000000, 0.000000000000000000 ) ) ;
#32629 = CARTESIAN_POINT ( 'NONE',  ( 95.00000000000000000, -213.0599564267049857, 81.34812500173430294 ) ) ;
#32630 = CARTESIAN_POINT ( 'NONE',  ( 92.34999999999999432, 91.52997821335252127, 80.42208333333331893 ) ) ;
#32631 = VERTEX_POINT ( 'NONE', #10616 ) ;
#32632 = DIRECTION ( 'NONE',  ( -1.000000000000000000, 0.000000000000000000, 0.000000000000000000 ) ) ;
#32633 = CIRCLE ( 'NONE', #291, 15.99999999999999645 ) ;
#32634 = ORIENTED_EDGE ( 'NONE', *, *, #51021, .F. ) ;
#32635 = CARTESIAN_POINT ( 'NONE',  ( -92.69370383062498320, -210.0000000000000568, 74.79348190356851944 ) ) ;
#32636 = ORIENTED_EDGE ( 'NONE', *, *, #10502, .T. ) ;
#32637 = CYLINDRICAL_SURFACE ( 'NONE', #74052, 82.00000000000000000 ) ;
#32638 = CARTESIAN_POINT ( 'NONE',  ( -96.15314808468751551, 88.00268892867056536, 85.46239583420047836 ) ) ;
#32639 = CARTESIAN_POINT ( 'NONE',  ( 93.84685191531248449, 91.99731107132950569, 81.91697916753381037 ) ) ;
#32640 = ORIENTED_EDGE ( 'NONE', *, *, #28342, .T. ) ;
#32641 = DIRECTION ( 'NONE',  ( 0.000000000000000000, 0.5224985647159500202, -0.8526401643540915121 ) ) ;
#32642 = EDGE_CURVE ( 'NONE', #39400, #28422, #58643, .T. ) ;
#32643 = CARTESIAN_POINT ( 'NONE',  ( 10.00000000000000000, 0.000000000000000000, 0.000000000000000000 ) ) ;
#32644 = ORIENTED_EDGE ( 'NONE', *, *, #24969, .T. ) ;
#32645 = CYLINDRICAL_SURFACE ( 'NONE', #8068, 16.00000000000000000 ) ;
#32646 = AXIS2_PLACEMENT_3D ( 'NONE', #57565, #51540, #11671 ) ;
#32647 = AXIS2_PLACEMENT_3D ( 'NONE', #46437, #47548, #30247 ) ;
#32648 = ORIENTED_EDGE ( 'NONE', *, *, #25291, .T. ) ;
#32649 = ORIENTED_EDGE ( 'NONE', *, *, #54582, .F. ) ;
#32650 = ADVANCED_FACE ( 'NONE', ( #61766, #33920, #22649 ), #10996, .F. ) ;
#32651 = CARTESIAN_POINT ( 'NONE',  ( 97.64999999999999147, 89.99999999755287661, 75.15687493081163950 ) ) ;
#32652 = EDGE_CURVE ( 'NONE', #13516, #6672, #26218, .T. ) ;
#32653 = ORIENTED_EDGE ( 'NONE', *, *, #29799, .F. ) ;
#32654 = DIRECTION ( 'NONE',  ( -1.000000000000000000, 0.000000000000000000, 0.000000000000000000 ) ) ;
#32655 = CYLINDRICAL_SURFACE ( 'NONE', #3488, 16.00000000000000000 ) ;
#32656 = VERTEX_POINT ( 'NONE', #21518 ) ;
#32657 = CARTESIAN_POINT ( 'NONE',  ( -94.26819495033781493, -212.6374485842881938, 75.02735117824597921 ) ) ;
#32658 = CARTESIAN_POINT ( 'NONE',  ( -97.30629616937497417, -208.6684592857803011, 80.06489583420047040 ) ) ;
#32659 = EDGE_LOOP ( 'NONE', ( #42823, #49464, #6878, #57801 ) ) ;
#32660 = CARTESIAN_POINT ( 'NONE',  ( 10.00000000000000000, 0.000000000000000000, 0.000000000000000000 ) ) ;
#32661 = DIRECTION ( 'NONE',  ( -0.000000000000000000, -0.000000000000000000, -1.000000000000000000 ) ) ;
#32662 = CARTESIAN_POINT ( 'NONE',  ( 0.000000000000000000, -26.02418014898359289, 70.52718814184250107 ) ) ;
#32663 = CARTESIAN_POINT ( 'NONE',  ( 6.000000000000000000, 81.90746397400387480, 3.894527615418180044 ) ) ;
#32664 = EDGE_CURVE ( 'NONE', #58390, #8233, #10136, .T. ) ;
#32665 = LINE ( 'NONE', #22143, #10221 ) ;
#32666 = CARTESIAN_POINT ( 'NONE',  ( 11.99999999999999822, 0.000000000000000000, 0.000000000000000000 ) ) ;
#32667 = CARTESIAN_POINT ( 'NONE',  ( 97.30629616937498838, 90.00000000000002842, 89.32531250086714181 ) ) ;
#32668 = DIRECTION ( 'NONE',  ( -1.000000000000000000, 0.000000000000000000, 0.000000000000000000 ) ) ;
#32669 = DIRECTION ( 'NONE',  ( 1.000000000000000000, 0.000000000000000000, 0.000000000000000000 ) ) ;
#32670 = CYLINDRICAL_SURFACE ( 'NONE', #53218, 37.49900000000000233 ) ;
#32671 = DIRECTION ( 'NONE',  ( 0.000000000000000000, 0.000000000000000000, 1.000000000000000000 ) ) ;
#32672 = DIRECTION ( 'NONE',  ( -1.000000000000000000, 0.000000000000000000, 0.000000000000000000 ) ) ;
#32673 = CARTESIAN_POINT ( 'NONE',  ( 11.99999999999999822, 39.78640506895604290, 66.50666863322015843 ) ) ;
#32674 = DIRECTION ( 'NONE',  ( -0.000000000000000000, 0.7431448254773946882, -0.6691306063588577935 ) ) ;
#32675 = ADVANCED_FACE ( 'NONE', ( #67016 ), #38080, .T. ) ;
#32676 = DIRECTION ( 'NONE',  ( -1.000000000000000000, 0.000000000000000000, 0.000000000000000000 ) ) ;
#32677 = CARTESIAN_POINT ( 'NONE',  ( 0.000000000000000000, -10.74501242461307982, 35.92658777277507198 ) ) ;
#32678 = DIRECTION ( 'NONE',  ( 0.000000000000000000, 0.000000000000000000, 1.000000000000000000 ) ) ;
#32679 = CIRCLE ( 'NONE', #1505, 14.09999999999999964 ) ;
#32680 = CARTESIAN_POINT ( 'NONE',  ( -97.64999999999996305, -209.9999999999999716, 83.65000000000000568 ) ) ;
#32681 = CIRCLE ( 'NONE', #15899, 16.00000000000000355 ) ;
#32682 = CARTESIAN_POINT ( 'NONE',  ( 97.64999999999999147, -210.0000000334413244, 87.85687500050293863 ) ) ;
#32683 = EDGE_CURVE ( 'NONE', #23343, #58541, #50836, .T. ) ;
#32684 = EDGE_CURVE ( 'NONE', #73246, #26822, #9510, .T. ) ;
#32685 = AXIS2_PLACEMENT_3D ( 'NONE', #73526, #15660, #66784 ) ;
#32686 = CYLINDRICAL_SURFACE ( 'NONE', #9543, 31.99999999999998579 ) ;
#32687 = DIRECTION ( 'NONE',  ( -1.000000000000000000, 0.000000000000000000, 0.000000000000000000 ) ) ;
#32688 = FACE_OUTER_BOUND ( 'NONE', #64645, .T. ) ;
#32689 = CARTESIAN_POINT ( 'NONE',  ( 10.00000000000000000, 0.000000000000000000, 0.000000000000000000 ) ) ;
#32690 = AXIS2_PLACEMENT_3D ( 'NONE', #20970, #56310, #22093 ) ;
#32691 = CIRCLE ( 'NONE', #356, 82.00000000000000000 ) ;
#32692 = CARTESIAN_POINT ( 'NONE',  ( 96.15314808468750130, -211.9973110713294489, 88.10822916753382117 ) ) ;
#32693 = ORIENTED_EDGE ( 'NONE', *, *, #25058, .T. ) ;
#32694 = VERTEX_POINT ( 'NONE', #32430 ) ;
#32695 = CARTESIAN_POINT ( 'NONE',  ( 15.00000000000000000, -18.13022148937242761, 15.02647892043569122 ) ) ;
#32696 = LINE ( 'NONE', #26330, #52367 ) ;
#32697 = ORIENTED_EDGE ( 'NONE', *, *, #18849, .T. ) ;
#32698 = CARTESIAN_POINT ( 'NONE',  ( 96.15314808468750130, -211.9973110713294489, 80.96447916753380980 ) ) ;
#32699 = CARTESIAN_POINT ( 'NONE',  ( 95.00000000000000000, -207.3369185715606307, 84.56281250086716739 ) ) ;
#32700 = EDGE_LOOP ( 'NONE', ( #45541, #35509, #70548, #39098 ) ) ;
#32701 = CARTESIAN_POINT ( 'NONE',  ( 96.15314808468748708, -208.0026889286704943, 85.77989583420048803 ) ) ;
#32702 = VERTEX_POINT ( 'NONE', #50085 ) ;
#32703 = DIRECTION ( 'NONE',  ( -1.000000000000000000, 0.000000000000000000, 0.000000000000000000 ) ) ;
#32704 = ORIENTED_EDGE ( 'NONE', *, *, #57887, .T. ) ;
#32705 = PLANE ( 'NONE',  #54904 ) ;
#32706 = ORIENTED_EDGE ( 'NONE', *, *, #66406, .F. ) ;
#32707 = VERTEX_POINT ( 'NONE', #38456 ) ;
#32708 = DIRECTION ( 'NONE',  ( -0.1045284632676436315, -0.9945218953682742891, 0.000000000000000000 ) ) ;
#32709 = VERTEX_POINT ( 'NONE', #44477 ) ;
#32710 = DIRECTION ( 'NONE',  ( -0.000000000000000000, -0.000000000000000000, -1.000000000000000000 ) ) ;
#32711 = CARTESIAN_POINT ( 'NONE',  ( 10.00000000000000000, 0.000000000000000000, 0.000000000000000000 ) ) ;
#32712 = ORIENTED_EDGE ( 'NONE', *, *, #17370, .F. ) ;
#32713 = DIRECTION ( 'NONE',  ( 0.000000000000000000, 0.6494480483301848794, -0.7604059656000299317 ) ) ;
#32714 = ORIENTED_EDGE ( 'NONE', *, *, #65201, .F. ) ;
#32715 = DIRECTION ( 'NONE',  ( 1.000000000000000000, -0.000000000000000000, -0.000000000000000000 ) ) ;
#32716 = ORIENTED_EDGE ( 'NONE', *, *, #13261, .T. ) ;
#32717 = ADVANCED_FACE ( 'NONE', ( #61395 ), #73013, .T. ) ;
#32718 =( GEOMETRIC_REPRESENTATION_CONTEXT ( 3 ) GLOBAL_UNCERTAINTY_ASSIGNED_CONTEXT ( ( #43455 ) ) GLOBAL_UNIT_ASSIGNED_CONTEXT ( ( #29209, #30684, #35231 ) ) REPRESENTATION_CONTEXT ( 'NONE', 'WORKASPACE' ) );
#32719 = VERTEX_POINT ( 'NONE', #33543 ) ;
#32720 = VERTEX_POINT ( 'NONE', #62133 ) ;
#32721 = DIRECTION ( 'NONE',  ( -1.000000000000000000, 0.000000000000000000, 0.000000000000000000 ) ) ;
#32722 = CONTEXT_DEPENDENT_SHAPE_REPRESENTATION ( #39301, #30263 ) ;
#32723 = CARTESIAN_POINT ( 'NONE',  ( 11.99999999999999822, 0.000000000000000000, 0.000000000000000000 ) ) ;
#32725 = EDGE_CURVE ( 'NONE', #55313, #24224, #32167, .T. ) ;
#32724 = EDGE_LOOP ( 'NONE', ( #70521, #3453, #27430, #27361 ) ) ;
#32726 = AXIS2_PLACEMENT_3D ( 'NONE', #27629, #23474, #56203 ) ;
#32727 = ORIENTED_EDGE ( 'NONE', *, *, #44819, .F. ) ;
#32728 = VERTEX_POINT ( 'NONE', #38827 ) ;
#32729 = CARTESIAN_POINT ( 'NONE',  ( 10.00000000000000000, 62.50884508063487033, -41.76106447765422303 ) ) ;
#32730 = EDGE_CURVE ( 'NONE', #14729, #2397, #56116, .T. ) ;
#32731 = DIRECTION ( 'NONE',  ( 0.000000000000000000, 0.4539904997395414754, 0.8910065241883706744 ) ) ;
#32732 = CARTESIAN_POINT ( 'NONE',  ( -92.35000000000003695, 90.00000000000004263, 89.68250000000000455 ) ) ;
#32733 = ORIENTED_EDGE ( 'NONE', *, *, #31496, .F. ) ;
#32734 = CARTESIAN_POINT ( 'NONE',  ( 92.69370383062498320, 91.33154071421968467, 76.88989583420047325 ) ) ;
#32735 = AXIS2_PLACEMENT_3D ( 'NONE', #72278, #45211, #61760 ) ;
#32736 =( BOUNDED_CURVE ( )  B_SPLINE_CURVE ( 2, ( #48953, #71883, #54611, #3135, #65532, #42592, #20012 ),
 .UNSPECIFIED., .F., .F. ) 
 B_SPLINE_CURVE_WITH_KNOTS ( ( 3, 2, 2, 3 ),
 ( 0.2291666666666663521, 0.2361111111111107719, 0.2430555555555551639, 0.2499999999999995837 ),
 .UNSPECIFIED. ) 
 CURVE ( )  GEOMETRIC_REPRESENTATION_ITEM ( )  RATIONAL_B_SPLINE_CURVE ( ( 1.000000000000005995, 0.8660254037844328234, 1.000000000000000000, 0.8660254037844387076, 1.000000000000000000, 0.8660254037844467012, 0.9999999999999920064 ) ) 
 REPRESENTATION_ITEM ( '' )  );
#32737 = ORIENTED_EDGE ( 'NONE', *, *, #61397, .T. ) ;
#32738 = FACE_OUTER_BOUND ( 'NONE', #18936, .T. ) ;
#32739 = CARTESIAN_POINT ( 'NONE',  ( -94.99999999999997158, -212.6630814284392557, 89.16656250086712987 ) ) ;
#32740 = VERTEX_POINT ( 'NONE', #73392 ) ;
#32741 = DIRECTION ( 'NONE',  ( -1.000000000000000000, -0.000000000000000000, 0.000000000000000000 ) ) ;
#32742 = CARTESIAN_POINT ( 'NONE',  ( -92.34999999999999432, -209.9999999999999716, 90.00000000000000000 ) ) ;
#32743 = DIRECTION ( 'NONE',  ( 0.000000000000000000, 0.000000000000000000, 1.000000000000000000 ) ) ;
#32744 = CARTESIAN_POINT ( 'NONE',  ( -94.99999999999997158, -212.6630814284392557, 79.00656250086714749 ) ) ;
#32745 = ADVANCED_FACE ( 'NONE', ( #44846 ), #67002, .T. ) ;
#32746 = DIRECTION ( 'NONE',  ( 0.000000000000000000, 0.000000000000000000, 1.000000000000000000 ) ) ;
#32747 = LINE ( 'NONE', #65511, #49930 ) ;
#32748 = VECTOR ( 'NONE', #13165, 1000.000000000000000 ) ;
#32749 = DIRECTION ( 'NONE',  ( -0.000000000000000000, -0.000000000000000000, 1.000000000000000000 ) ) ;
#32750 = ORIENTED_EDGE ( 'NONE', *, *, #68176, .F. ) ;
#32751 = CIRCLE ( 'NONE', #69992, 30.50000000000000000 ) ;
#32752 = VERTEX_POINT ( 'NONE', #39198 ) ;
#32753 = DIRECTION ( 'NONE',  ( -1.000000000000000000, 3.061616997868383141E-16, -0.000000000000000000 ) ) ;
#32754 = CARTESIAN_POINT ( 'NONE',  ( 0.000000000000000000, -38.55633173627022359, 16.65560815589396526 ) ) ;
#32755 = CARTESIAN_POINT ( 'NONE',  ( 96.58546442478372285, -208.2943803060620667, 74.79912739178800507 ) ) ;
#32756 = CARTESIAN_POINT ( 'NONE',  ( -93.84685191531254134, 91.99731107132950569, 80.54114583420046358 ) ) ;
#32757 = CARTESIAN_POINT ( 'NONE',  ( 10.00000000000000000, 0.000000000000000000, 0.000000000000000000 ) ) ;
#32758 = CARTESIAN_POINT ( 'NONE',  ( 0.000000000000000000, 0.000000000000000000, 0.000000000000000000 ) ) ;
#32759 = EDGE_CURVE ( 'NONE', #59559, #37734, #5855, .T. ) ;
#32760 = EDGE_LOOP ( 'NONE', ( #66912, #57402, #22205, #48470 ) ) ;
#32761 = EDGE_CURVE ( 'NONE', #43377, #72913, #57612, .T. ) ;
#32762 = CARTESIAN_POINT ( 'NONE',  ( 3.000000000000000000, -2.935248768560059673, 2.602085213965210642E-15 ) ) ;
#32763 = EDGE_CURVE ( 'NONE', #56683, #32364, #73064, .T. ) ;
#32765 = EDGE_CURVE ( 'NONE', #26530, #58950, #24492, .T. ) ;
#32764 = DIRECTION ( 'NONE',  ( -1.000000000000000000, 0.000000000000000000, 0.000000000000000000 ) ) ;
#32766 = CARTESIAN_POINT ( 'NONE',  ( -10.00000000000000000, 0.000000000000000000, 0.000000000000000000 ) ) ;
#32767 = CARTESIAN_POINT ( 'NONE',  ( -93.67500000000003979, 92.29496732002878900, 89.78833333333332689 ) ) ;
#32768 = CARTESIAN_POINT ( 'NONE',  ( -94.99999999999997158, -209.9999999999999716, 90.00000000000000000 ) ) ;
#32769 = CARTESIAN_POINT ( 'NONE',  ( -93.84685191531248449, -208.0026889286704943, 78.15989583420049769 ) ) ;
#32770 = CARTESIAN_POINT ( 'NONE',  ( 92.35000000006144205, 90.00001182178868930, 76.10900611559256390 ) ) ;
#32771 = EDGE_CURVE ( 'NONE', #74080, #55829, #28816, .T. ) ;
#32772 = ORIENTED_EDGE ( 'NONE', *, *, #29982, .F. ) ;
#32773 = DIRECTION ( 'NONE',  ( 0.000000000000000000, 0.000000000000000000, 1.000000000000000000 ) ) ;
#32774 = DIRECTION ( 'NONE',  ( 0.000000000000000000, -0.9723699203976789995, 0.2334453638558957322 ) ) ;
#32775 = DIRECTION ( 'NONE',  ( 0.000000000000000000, -0.5877852522924801315, 0.8090169943749421222 ) ) ;
#32776 = ORIENTED_EDGE ( 'NONE', *, *, #2499, .T. ) ;
#32777 = ADVANCED_FACE ( 'NONE', ( #51949 ), #11356, .T. ) ;
#32778 = AXIS2_PLACEMENT_3D ( 'NONE', #68994, #17848, #35143 ) ;
#32779 = DIRECTION ( 'NONE',  ( -1.000000000000000000, 0.000000000000000000, -0.000000000000000000 ) ) ;
#32780 = DIRECTION ( 'NONE',  ( -1.000000000000000000, 0.000000000000000000, 0.000000000000000000 ) ) ;
#32781 = VECTOR ( 'NONE', #40298, 1000.000000000000000 ) ;
#32782 = CARTESIAN_POINT ( 'NONE',  ( 5.000000000000000000, 22.48208911017551870, -35.47612816024499693 ) ) ;
#32783 = ORIENTED_EDGE ( 'NONE', *, *, #29514, .T. ) ;
#32784 = CARTESIAN_POINT ( 'NONE',  ( 10.00000000000000000, -35.95386929396264009, 10.96151621346475658 ) ) ;
#32785 = FILL_AREA_STYLE ('',( #27142 ) ) ;
#32786 = ORIENTED_EDGE ( 'NONE', *, *, #10127, .F. ) ;
#32787 = VECTOR ( 'NONE', #36694, 1000.000000000000000 ) ;
#32788 = DIRECTION ( 'NONE',  ( 0.000000000000000000, -0.9876883405951393247, 0.1564344650402204329 ) ) ;
#32789 = CARTESIAN_POINT ( 'NONE',  ( -3.000000000000000000, -4.261787119644969479, -26.19803753235780519 ) ) ;
#32790 = TOROIDAL_SURFACE ( 'NONE', #24442, 13.10000000000000142, 0.5999999999999998668 ) ;
#32791 = ORIENTED_EDGE ( 'NONE', *, *, #56433, .F. ) ;
#32792 = LINE ( 'NONE', #31038, #39039 ) ;
#32793 = VERTEX_POINT ( 'NONE', #41056 ) ;
#32794 = AXIS2_PLACEMENT_3D ( 'NONE', #8265, #8647, #31558 ) ;
#32795 = DIRECTION ( 'NONE',  ( 0.000000000000000000, -0.5224985647159561264, 0.8526401643540878483 ) ) ;
#32796 = VECTOR ( 'NONE', #48501, 1000.000000000000114 ) ;
#32797 = VECTOR ( 'NONE', #33507, 1000.000000000000000 ) ;
#32798 = DIRECTION ( 'NONE',  ( -1.000000000000000000, 0.000000000000000000, 0.000000000000000000 ) ) ;
#32799 = ORIENTED_EDGE ( 'NONE', *, *, #20978, .T. ) ;
#32800 = ORIENTED_EDGE ( 'NONE', *, *, #8663, .T. ) ;
#32801 = ORIENTED_EDGE ( 'NONE', *, *, #65443, .F. ) ;
#32802 = CARTESIAN_POINT ( 'NONE',  ( -5.000000000000000000, 2.886751345948126879, -2.079999999999992077 ) ) ;
#32803 = VERTEX_POINT ( 'NONE', #6828 ) ;
#32804 = ORIENTED_EDGE ( 'NONE', *, *, #49327, .T. ) ;
#32805 = CARTESIAN_POINT ( 'NONE',  ( 96.15314808468748708, 91.99731107132950569, 74.98489583420048632 ) ) ;
#32806 = LINE ( 'NONE', #73404, #44368 ) ;
#32807 = CARTESIAN_POINT ( 'NONE',  ( 15.00000000000000000, -3.948201729842032215, 23.21447184625297666 ) ) ;
#32808 = ORIENTED_EDGE ( 'NONE', *, *, #45182, .F. ) ;
#32809 = ORIENTED_EDGE ( 'NONE', *, *, #57740, .T. ) ;
#32810 = EDGE_CURVE ( 'NONE', #33855, #51707, #33454, .T. ) ;
#32811 = ORIENTED_EDGE ( 'NONE', *, *, #7066, .T. ) ;
#32812 = CARTESIAN_POINT ( 'NONE',  ( 96.15314808468748708, 91.99731107132950569, 87.52614583420047722 ) ) ;
#32813 = VERTEX_POINT ( 'NONE', #68887 ) ;
#32814 = CARTESIAN_POINT ( 'NONE',  ( 93.84685191531251292, -211.9973110713294489, 84.03364583420047040 ) ) ;
#32815 = DIRECTION ( 'NONE',  ( 0.000000000000000000, 0.000000000000000000, -1.000000000000000000 ) ) ;
#32816 = CARTESIAN_POINT ( 'NONE',  ( -95.00000000000002842, 90.00000000000004263, 90.00000000000000000 ) ) ;
#32817 = EDGE_CURVE ( 'NONE', #74032, #40680, #47068, .T. ) ;
#32818 = CARTESIAN_POINT ( 'NONE',  ( -92.35000000000312070, 89.99999595380251094, 77.06187486178039592 ) ) ;
#32819 = FACE_OUTER_BOUND ( 'NONE', #46974, .T. ) ;
#32820 = DIRECTION ( 'NONE',  ( 0.000000000000000000, 0.000000000000000000, 1.000000000000000000 ) ) ;
#32821 = DIRECTION ( 'NONE',  ( -1.000000000000000000, 0.000000000000000000, -0.000000000000000000 ) ) ;
#32822 = EDGE_CURVE ( 'NONE', #19761, #57988, #12830, .T. ) ;
#32823 = CARTESIAN_POINT ( 'NONE',  ( 94.99999999999998579, 86.94004357329502852, 85.15812500173429100 ) ) ;
#32824 = EDGE_CURVE ( 'NONE', #33925, #37934, #6476, .T. ) ;
#32825 = CARTESIAN_POINT ( 'NONE',  ( -92.69370383062498320, -211.3315407142195852, 87.36739583420047950 ) ) ;
#32826 = CARTESIAN_POINT ( 'NONE',  ( -92.69370383062504004, 90.00000000000004263, 84.40406250086715545 ) ) ;
#32827 = VERTEX_POINT ( 'NONE', #40305 ) ;
#32828 = AXIS2_PLACEMENT_3D ( 'NONE', #59470, #36160, #18861 ) ;
#32830 = CARTESIAN_POINT ( 'NONE',  ( -96.15314808468752972, 91.99731107132950569, 89.53697916753381492 ) ) ;
#32829 = CARTESIAN_POINT ( 'NONE',  ( 94.99999999999998579, 92.66308142843935514, 86.94406250086714749 ) ) ;
#32831 = ORIENTED_EDGE ( 'NONE', *, *, #39291, .T. ) ;
#32832 = DIRECTION ( 'NONE',  ( 0.000000000000000000, -0.8910065241883721177, 0.4539904997395382003 ) ) ;
#32833 = CARTESIAN_POINT ( 'NONE',  ( 10.00000000000000000, 0.000000000000000000, 0.000000000000000000 ) ) ;
#32834 = FACE_OUTER_BOUND ( 'NONE', #15897, .T. ) ;
#32835 = DIRECTION ( 'NONE',  ( 1.000000000000000000, 0.000000000000000000, 0.000000000000000000 ) ) ;
#32836 = CARTESIAN_POINT ( 'NONE',  ( -92.69370383062498320, -209.9999999999999716, 89.32531250086714181 ) ) ;
#32837 = DIRECTION ( 'NONE',  ( -1.000000000000000000, 0.000000000000000000, 0.000000000000000000 ) ) ;
#32838 = PRODUCT_DEFINITION_FORMATION_WITH_SPECIFIED_SOURCE ( 'ANY', '', #73401, .NOT_KNOWN. ) ;
#32839 = DIRECTION ( 'NONE',  ( -1.000000000000000000, 0.000000000000000000, 0.000000000000000000 ) ) ;
#32840 = CARTESIAN_POINT ( 'NONE',  ( 0.000000000000000000, -32.34446384429989507, 26.79245525562703278 ) ) ;
#32841 = ORIENTED_EDGE ( 'NONE', *, *, #18997, .F. ) ;
#32842 = AXIS2_PLACEMENT_3D ( 'NONE', #3986, #10726, #32529 ) ;
#32843 = ADVANCED_FACE ( 'NONE', ( #63988 ), #17373, .T. ) ;
#32844 = EDGE_LOOP ( 'NONE', ( #21658, #73874, #73216, #49461 ) ) ;
#32845 = EDGE_CURVE ( 'NONE', #1093, #12587, #29865, .T. ) ;
#32846 = CARTESIAN_POINT ( 'NONE',  ( -92.35000000000003695, 90.00000000000004263, 82.69749999999999091 ) ) ;
#32847 = CARTESIAN_POINT ( 'NONE',  ( 10.00000000000000000, -31.52238457039619490, 27.75498641678731104 ) ) ;
#32848 = DIRECTION ( 'NONE',  ( -1.000000000000000000, -0.000000000000000000, -0.000000000000000000 ) ) ;
#32849 = CARTESIAN_POINT ( 'NONE',  ( 11.99999999999999822, 70.53064760720316428, -26.01480285779861035 ) ) ;
#32850 = FACE_BOUND ( 'NONE', #69127, .T. ) ;
#32851 = CARTESIAN_POINT ( 'NONE',  ( 92.35003236756685396, 91.52999690077596995, 87.48645704240065868 ) ) ;
#32852 = CARTESIAN_POINT ( 'NONE',  ( -92.35000000000005116, 88.47002178664754979, 86.53395833506763779 ) ) ;
#32853 = CIRCLE ( 'NONE', #61682, 42.00000000000000000 ) ;
#32854 = DIRECTION ( 'NONE',  ( 0.000000000000000000, -0.9510565162951565288, 0.3090169943749383474 ) ) ;
#32855 = VERTEX_POINT ( 'NONE', #34288 ) ;
#32856 = CARTESIAN_POINT ( 'NONE',  ( -97.30629616937501680, 90.00000000000004263, 83.29281250086714294 ) ) ;
#32857 = CARTESIAN_POINT ( 'NONE',  ( 10.00000000000000000, 0.000000000000000000, 0.000000000000000000 ) ) ;
#32858 = CIRCLE ( 'NONE', #498, 31.99999999999998934 ) ;
#32859 = ADVANCED_FACE ( 'NONE', ( #63253 ), #11714, .T. ) ;
#32860 = ADVANCED_FACE ( 'NONE', ( #24137 ), #23749, .F. ) ;
#32861 = FACE_OUTER_BOUND ( 'NONE', #47445, .T. ) ;
#32862 = CARTESIAN_POINT ( 'NONE',  ( 10.00000000000000000, -35.95386929396248377, -10.96151621346525751 ) ) ;
#32863 = DIRECTION ( 'NONE',  ( 0.000000000000000000, -0.8090169943749422332, -0.5877852522924803536 ) ) ;
#32864 = DIRECTION ( 'NONE',  ( -0.9038112904824853189, 0.4279312458752977943, 0.000000000000000000 ) ) ;
#32865 = DIRECTION ( 'NONE',  ( 0.000000000000000000, 0.000000000000000000, 1.000000000000000000 ) ) ;
#32866 = DIRECTION ( 'NONE',  ( 0.000000000000000000, 0.8090169943749447867, 0.5877852522924769119 ) ) ;
#32867 = CARTESIAN_POINT ( 'NONE',  ( 92.69370383062498320, 90.00000000000002842, 79.00656250086716170 ) ) ;
#32868 = AXIS2_PLACEMENT_3D ( 'NONE', #42552, #61241, #48556 ) ;
#32869 = CARTESIAN_POINT ( 'NONE',  ( -94.99999999999997158, -212.6630814284392557, 81.70531250086715147 ) ) ;
#32870 = CYLINDRICAL_SURFACE ( 'NONE', #44591, 2.649999999999999467 ) ;
#32871 = ORIENTED_EDGE ( 'NONE', *, *, #7562, .T. ) ;
#32872 = CARTESIAN_POINT ( 'NONE',  ( -97.65000000000001990, 89.99996511148930267, 83.09437620840749616 ) ) ;
#32873 = CARTESIAN_POINT ( 'NONE',  ( -93.67499999999998295, -212.2949673200287179, 78.14666666666667538 ) ) ;
#32874 = CARTESIAN_POINT ( 'NONE',  ( -92.69370383062504004, 90.00000000000004263, 79.32406250086715715 ) ) ;
#32875 = CARTESIAN_POINT ( 'NONE',  ( 97.30629616937498838, -208.6684592857803011, 81.12322916753382174 ) ) ;
#32876 = ORIENTED_EDGE ( 'NONE', *, *, #31223, .T. ) ;
#32877 = VECTOR ( 'NONE', #12327, 1000.000000000000000 ) ;
#32878 = CARTESIAN_POINT ( 'NONE',  ( 10.00000000000000000, -25.88420570971381807, -27.13269053701123212 ) ) ;
#32879 = ORIENTED_EDGE ( 'NONE', *, *, #4776, .T. ) ;
#32880 = LINE ( 'NONE', #66387, #58466 ) ;
#32881 = ORIENTED_EDGE ( 'NONE', *, *, #42354, .T. ) ;
#32882 = DIRECTION ( 'NONE',  ( -1.000000000000000000, 0.000000000000000000, -0.000000000000000000 ) ) ;
#32883 = VECTOR ( 'NONE', #52703, 1000.000000000000000 ) ;
#32884 = ORIENTED_EDGE ( 'NONE', *, *, #70802, .T. ) ;
#32885 = ORIENTED_EDGE ( 'NONE', *, *, #46782, .F. ) ;
#32886 = ORIENTED_EDGE ( 'NONE', *, *, #16519, .T. ) ;
#32887 = CARTESIAN_POINT ( 'NONE',  ( 0.000000000000000000, 29.81001611431009479, 22.74946021919143391 ) ) ;
#32888 = CARTESIAN_POINT ( 'NONE',  ( 10.00000000000000000, 0.000000000000000000, 2.500000000000000000 ) ) ;
#32889 = DIRECTION ( 'NONE',  ( -1.000000000000000000, 7.619177619974977057E-15, 2.612289469705706555E-14 ) ) ;
#32890 = CONICAL_SURFACE ( 'NONE', #29301, 5.000000000000000888, 1.047197551196596299 ) ;
#32891 = DIRECTION ( 'NONE',  ( -1.000000000000000000, 0.000000000000000000, 0.000000000000000000 ) ) ;
#32892 = CARTESIAN_POINT ( 'NONE',  ( 94.99999999999998579, 92.66308142843935514, 87.10281250086715943 ) ) ;
#32893 = VECTOR ( 'NONE', #48330, 1000.000000000000000 ) ;
#32894 = DIRECTION ( 'NONE',  ( -0.02332147558787674158, -0.9997280174009349762, 0.000000000000000000 ) ) ;
#32895 = CARTESIAN_POINT ( 'NONE',  ( 96.32499999999998863, -212.2949673200287179, 76.87666666666666515 ) ) ;
#32896 = ADVANCED_FACE ( 'NONE', ( #70707, #9046, #42526, #59822, #64722, #24858, #13934, #20327, #66209, #41778, #65468, #8311, #3431, #30852, #36137, #59085, #19578 ), #14684, .T. ) ;
#32897 = ORIENTED_EDGE ( 'NONE', *, *, #40999, .F. ) ;
#32898 = ORIENTED_EDGE ( 'NONE', *, *, #40584, .T. ) ;
#32899 = EDGE_CURVE ( 'NONE', #65222, #13949, #7074, .T. ) ;
#32900 = ORIENTED_EDGE ( 'NONE', *, *, #38636, .T. ) ;
#32901 = VECTOR ( 'NONE', #31754, 1000.000000000000000 ) ;
#32902 = EDGE_LOOP ( 'NONE', ( #59916, #36723, #6163, #63248, #9146 ) ) ;
#32903 = CARTESIAN_POINT ( 'NONE',  ( 11.99999999999999822, -46.53671651293991118, 59.03961581697383565 ) ) ;
#32904 = ADVANCED_FACE ( 'NONE', ( #47787 ), #48530, .T. ) ;
#32905 = CARTESIAN_POINT ( 'NONE',  ( 5.999999999999999112, 60.67117009219215618, -55.16347631942977614 ) ) ;
#32906 = CARTESIAN_POINT ( 'NONE',  ( 96.32499999999998863, -212.2949673200287179, 82.67104166840096013 ) ) ;
#32907 = DIRECTION ( 'NONE',  ( -2.603472992746261562E-14, -2.546204323184492723E-14, 1.000000000000000000 ) ) ;
#32908 = CARTESIAN_POINT ( 'NONE',  ( 0.000000000000000000, -60.67117009219176538, 55.16347631943019536 ) ) ;
#32910 = ORIENTED_EDGE ( 'NONE', *, *, #69605, .F. ) ;
#32909 = EDGE_CURVE ( 'NONE', #4807, #38459, #49081, .T. ) ;
#32911 = CARTESIAN_POINT ( 'NONE',  ( -92.34999999999999432, -211.5299782133524502, 81.45395833506763950 ) ) ;
#32912 = ORIENTED_EDGE ( 'NONE', *, *, #47115, .T. ) ;
#32913 = CARTESIAN_POINT ( 'NONE',  ( 11.99999999999999822, 0.000000000000000000, 0.000000000000000000 ) ) ;
#32914 = CIRCLE ( 'NONE', #564, 82.00000000000000000 ) ;
#32915 = EDGE_LOOP ( 'NONE', ( #34638, #56070, #33438, #66186 ) ) ;
#32916 = CARTESIAN_POINT ( 'NONE',  ( -95.00000000000002842, 86.94004357329504273, 81.98312500173430806 ) ) ;
#32917 = EDGE_CURVE ( 'NONE', #44329, #26982, #61065, .T. ) ;
#32918 = ORIENTED_EDGE ( 'NONE', *, *, #69124, .F. ) ;
#32919 = CARTESIAN_POINT ( 'NONE',  ( 97.30629616937498838, 88.66845928578037217, 83.71614583420050337 ) ) ;
#32920 = DIRECTION ( 'NONE',  ( 1.000000000000000000, 0.000000000000000000, -0.000000000000000000 ) ) ;
#32921 = CARTESIAN_POINT ( 'NONE',  ( -92.35000677009857384, -211.5299821220706917, 82.72395806468945523 ) ) ;
#32922 = CIRCLE ( 'NONE', #59345, 82.00000000000000000 ) ;
#32923 = FACE_OUTER_BOUND ( 'NONE', #131, .T. ) ;
#32924 = CARTESIAN_POINT ( 'NONE',  ( -3.360000000000002096, 0.000000000000000000, 0.000000000000000000 ) ) ;
#32925 = CARTESIAN_POINT ( 'NONE',  ( 97.65000000000000568, 91.52997821335250705, 87.83041666666669300 ) ) ;
#32926 = ORIENTED_EDGE ( 'NONE', *, *, #19362, .F. ) ;
#32927 = PLANE ( 'NONE',  #26678 ) ;
#32928 = DIRECTION ( 'NONE',  ( -1.000000000000000000, -0.000000000000000000, 0.000000000000000000 ) ) ;
#32929 = DIRECTION ( 'NONE',  ( 1.000000000000000000, 0.000000000000000000, 0.000000000000000000 ) ) ;
#32930 = ORIENTED_EDGE ( 'NONE', *, *, #20796, .T. ) ;
#32931 = ORIENTED_EDGE ( 'NONE', *, *, #33528, .T. ) ;
#32932 = EDGE_CURVE ( 'NONE', #54637, #26934, #43092, .T. ) ;
#32933 = ADVANCED_FACE ( 'NONE', ( #31967 ), #30491, .F. ) ;
#32934 = DIRECTION ( 'NONE',  ( -1.000000000000000000, -0.000000000000000000, 0.000000000000000000 ) ) ;
#32935 = CARTESIAN_POINT ( 'NONE',  ( -3.000000000000000000, 18.84667830672579925, 18.68964196561269020 ) ) ;
#32936 = DIRECTION ( 'NONE',  ( 0.000000000000000000, 0.000000000000000000, 1.000000000000000000 ) ) ;
#32937 = CARTESIAN_POINT ( 'NONE',  ( -96.15314808468745866, -211.9973110713294489, 79.74739583420048916 ) ) ;
#32938 = ORIENTED_EDGE ( 'NONE', *, *, #66617, .F. ) ;
#32939 = DIRECTION ( 'NONE',  ( 0.000000000000000000, 0.000000000000000000, -1.000000000000000000 ) ) ;
#32940 = ORIENTED_EDGE ( 'NONE', *, *, #66656, .F. ) ;
#32941 = DIRECTION ( 'NONE',  ( -0.000000000000000000, -0.000000000000000000, 1.000000000000000000 ) ) ;
#32942 = EDGE_CURVE ( 'NONE', #32025, #12008, #36501, .T. ) ;
#32943 = EDGE_CURVE ( 'NONE', #15838, #29293, #70332, .T. ) ;
#32944 = CIRCLE ( 'NONE', #42574, 77.49899999999999523 ) ;
#32945 = DIRECTION ( 'NONE',  ( 1.000000000000000000, 0.000000000000000000, 0.000000000000000000 ) ) ;
#32946 = CARTESIAN_POINT ( 'NONE',  ( -92.34999999999999432, -211.5299782133524218, 76.37395833506761278 ) ) ;
#32947 = CARTESIAN_POINT ( 'NONE',  ( 97.30629616937498838, 88.66845928578035796, 78.47739583420047893 ) ) ;
#32948 = DIRECTION ( 'NONE',  ( -1.000000000000000000, 0.000000000000000000, 0.000000000000000000 ) ) ;
#32949 = FACE_OUTER_BOUND ( 'NONE', #25245, .T. ) ;
#32950 = DIRECTION ( 'NONE',  ( 0.000000000000000000, 0.000000000000000000, 1.000000000000000000 ) ) ;
#32951 = DIRECTION ( 'NONE',  ( -1.000000000000000000, -0.000000000000000000, 0.000000000000000000 ) ) ;
#32952 = CARTESIAN_POINT ( 'NONE',  ( 0.000000000000000000, 0.000000000000000000, -54.99999999999998579 ) ) ;
#32953 = DIRECTION ( 'NONE',  ( 0.000000000000000000, 0.000000000000000000, 1.000000000000000000 ) ) ;
#32954 = CIRCLE ( 'NONE', #40169, 16.00000000000000000 ) ;
#32955 = CIRCLE ( 'NONE', #22138, 12.50000000000022560 ) ;
#32956 = CYLINDRICAL_SURFACE ( 'NONE', #42014, 23.50000000000489919 ) ;
#32957 = AXIS2_PLACEMENT_3D ( 'NONE', #59473, #35780, #71838 ) ;
#32958 = CARTESIAN_POINT ( 'NONE',  ( -31.74999999999995737, 0.000000000000000000, 0.000000000000000000 ) ) ;
#32959 = CARTESIAN_POINT ( 'NONE',  ( -15.70044424985398557, 0.001194404164747221980, -70.59999999999959641 ) ) ;
#32960 = ORIENTED_EDGE ( 'NONE', *, *, #23667, .F. ) ;
#32961 = CARTESIAN_POINT ( 'NONE',  ( -97.30629616937501680, 88.66845928578038638, 83.34572916753381833 ) ) ;
#32962 = VECTOR ( 'NONE', #42245, 1000.000000000000000 ) ;
#32963 = DIRECTION ( 'NONE',  ( -1.000000000000000000, -0.000000000000000000, -0.000000000000000000 ) ) ;
#32964 = CIRCLE ( 'NONE', #607, 16.00000000000000000 ) ;
#32965 = FACE_OUTER_BOUND ( 'NONE', #7503, .T. ) ;
#32966 = VECTOR ( 'NONE', #35664, 1000.000000000000000 ) ;
#32967 = ORIENTED_EDGE ( 'NONE', *, *, #46713, .T. ) ;
#32968 =( BOUNDED_CURVE ( )  B_SPLINE_CURVE ( 2, ( #44150, #32852, #11412, #68577, #5431, #62575, #56170 ),
 .UNSPECIFIED., .F., .F. ) 
 B_SPLINE_CURVE_WITH_KNOTS ( ( 3, 2, 2, 3 ),
 ( 0.1905056698837213069, 0.1975614351447063655, 0.2046172006855886960, 0.2116728463006670724 ),
 .UNSPECIFIED. ) 
 CURVE ( )  GEOMETRIC_REPRESENTATION_ITEM ( )  RATIONAL_B_SPLINE_CURVE ( ( 1.000000000000000000, 0.8660254037844387076, 1.000000000000000000, 0.8660254037844387076, 1.000000000000000000, 0.8660276809308478096, 0.9999954457845905420 ) ) 
 REPRESENTATION_ITEM ( '' )  );
#32969 = LINE ( 'NONE', #50639, #36676 ) ;
#32970 = CARTESIAN_POINT ( 'NONE',  ( 12.50000000000000000, -107.5000000000000000, 2.500000000000000000 ) ) ;
#32971 = DIRECTION ( 'NONE',  ( -1.000000000000000000, 0.000000000000000000, 0.000000000000000000 ) ) ;
#32972 = VECTOR ( 'NONE', #63839, 1000.000000000000000 ) ;
#32973 = DIRECTION ( 'NONE',  ( 0.000000000000000000, 1.000000000000000000, -1.625241993126352398E-15 ) ) ;
#32974 = CARTESIAN_POINT ( 'NONE',  ( 97.30629616937498838, -209.9999999999999716, 79.95906250086714806 ) ) ;
#32975 = ORIENTED_EDGE ( 'NONE', *, *, #45798, .T. ) ;
#32976 = EDGE_CURVE ( 'NONE', #16651, #27107, #18838, .T. ) ;
#32977 = ORIENTED_EDGE ( 'NONE', *, *, #37621, .F. ) ;
#32978 = EDGE_CURVE ( 'NONE', #3617, #72633, #18272, .T. ) ;
#32979 = DIRECTION ( 'NONE',  ( 0.000000000000000000, 0.000000000000000000, 1.000000000000000000 ) ) ;
#32980 = CARTESIAN_POINT ( 'NONE',  ( 11.99999999999999822, 74.65491531819105830, 8.830959090343693418 ) ) ;
#32981 = EDGE_CURVE ( 'NONE', #34710, #21157, #15427, .T. ) ;
#32982 = CARTESIAN_POINT ( 'NONE',  ( -12.50000000000000000, -132.5000000000000000, 2.500000000000000000 ) ) ;
#32983 = DIRECTION ( 'NONE',  ( -1.000000000000000000, -0.000000000000000000, 0.000000000000000000 ) ) ;
#32984 = B_SPLINE_CURVE_WITH_KNOTS ( 'NONE', 3,
 ( #11503, #34435, #5157, #45375, #64138, #50995, #58117, #6614, #11867, #46103, #68297, #5523, #34820, #62675, #11150, #34072, #57017, #28425 ),
 .UNSPECIFIED., .F., .F.,
 ( 4, 2, 2, 2, 2, 2, 2, 2, 4 ),
 ( -0.004093595876927202080, -0.003575961939746029588, -0.003058328002564857095, -0.002540694065383684603, -0.002023060128202512110, -0.001505426191021339618, -0.0009877922538401671254, -0.0004701583166589946329, 4.747562052217785961E-05 ),
 .UNSPECIFIED. ) ;
#32985 = DIRECTION ( 'NONE',  ( -1.000000000000000000, 0.000000000000000000, 0.000000000000000000 ) ) ;
#32986 = CARTESIAN_POINT ( 'NONE',  ( 95.00000000000000000, -213.0599564267049857, 87.61875000000000568 ) ) ;
#32987 = EDGE_CURVE ( 'NONE', #20918, #39053, #57479, .T. ) ;
#32988 = ORIENTED_EDGE ( 'NONE', *, *, #58810, .F. ) ;
#32989 = DIRECTION ( 'NONE',  ( -1.000000000000000000, 0.000000000000000000, -0.000000000000000000 ) ) ;
#32990 = ORIENTED_EDGE ( 'NONE', *, *, #5792, .F. ) ;
#32991 = ORIENTED_EDGE ( 'NONE', *, *, #47047, .F. ) ;
#32992 = CARTESIAN_POINT ( 'NONE',  ( 0.000000000000000000, 26.01480285779933510, -70.53064760720289428 ) ) ;
#32993 = VECTOR ( 'NONE', #72393, 1000.000000000000000 ) ;
#32994 = SURFACE_STYLE_FILL_AREA ( #63093 ) ;
#32995 = EDGE_CURVE ( 'NONE', #54409, #26601, #9420, .T. ) ;
#32996 = LINE ( 'NONE', #9708, #68942 ) ;
#32997 = VERTEX_POINT ( 'NONE', #73299 ) ;
#32998 = CYLINDRICAL_SURFACE ( 'NONE', #18564, 21.00000000000000000 ) ;
#32999 = CARTESIAN_POINT ( 'NONE',  ( 97.64999999999997726, -211.5299782133524502, 78.91395833506763324 ) ) ;
#33000 = CARTESIAN_POINT ( 'NONE',  ( 97.64999999999999147, 90.00000000000002842, 82.06250000000000000 ) ) ;
#33001 = ORIENTED_EDGE ( 'NONE', *, *, #56527, .F. ) ;
#33002 = DIRECTION ( 'NONE',  ( 0.000000000000000000, 0.000000000000000000, -1.000000000000000000 ) ) ;
#33003 = ORIENTED_EDGE ( 'NONE', *, *, #24936, .F. ) ;
#33004 = CARTESIAN_POINT ( 'NONE',  ( 90.00000000000001421, -204.9999999999999716, -80.00000000000000000 ) ) ;
#33005 = ORIENTED_EDGE ( 'NONE', *, *, #7958, .F. ) ;
#33006 = CARTESIAN_POINT ( 'NONE',  ( 15.00000000000000000, 16.83928648764922542, -16.46020748918050458 ) ) ;
#33007 = CARTESIAN_POINT ( 'NONE',  ( -96.15314808468751551, 88.00268892867056536, 82.92239583420048632 ) ) ;
#33008 = CIRCLE ( 'NONE', #41394, 16.00000000000000000 ) ;
#33009 = EDGE_CURVE ( 'NONE', #45064, #68267, #38740, .T. ) ;
#33010 = CARTESIAN_POINT ( 'NONE',  ( 94.99999999999998579, 92.66308142843935514, 78.68906250086713783 ) ) ;
#33011 = AXIS2_PLACEMENT_3D ( 'NONE', #66946, #9068, #39131 ) ;
#33012 = ORIENTED_EDGE ( 'NONE', *, *, #4812, .T. ) ;
#33013 = CARTESIAN_POINT ( 'NONE',  ( 5.999999999999999112, -56.15606465355000410, 59.75363087400056372 ) ) ;
#33014 = CYLINDRICAL_SURFACE ( 'NONE', #60585, 77.49899999999999523 ) ;
#33015 = DIRECTION ( 'NONE',  ( -1.000000000000000000, 0.000000000000000000, 0.000000000000000000 ) ) ;
#33016 = ORIENTED_EDGE ( 'NONE', *, *, #54175, .T. ) ;
#33017 = CARTESIAN_POINT ( 'NONE',  ( 10.00000000000000000, 11.30684508768452545, -76.66974797899825944 ) ) ;
#33018 = CARTESIAN_POINT ( 'NONE',  ( -93.84685191531248449, -208.0026889286704943, 82.44614583420046472 ) ) ;
#33019 = EDGE_LOOP ( 'NONE', ( #10836, #68610, #10901, #21903 ) ) ;
#33020 = VERTEX_POINT ( 'NONE', #66924 ) ;
#33022 = CARTESIAN_POINT ( 'NONE',  ( 97.64999999999999147, 90.00000000000002842, 78.88750000000000284 ) ) ;
#33021 = CIRCLE ( 'NONE', #49813, 31.99999999999998579 ) ;
#33023 = ADVANCED_FACE ( 'NONE', ( #22188 ), #44009, .T. ) ;
#33024 = ORIENTED_EDGE ( 'NONE', *, *, #3529, .F. ) ;
#33025 = EDGE_CURVE ( 'NONE', #44604, #46613, #27440, .T. ) ;
#33026 = DIRECTION ( 'NONE',  ( 0.000000000000000000, 0.6494480483301848794, -0.7604059656000299317 ) ) ;
#33027 = APPLICATION_CONTEXT ( 'automotive_design' ) ;
#33028 = CARTESIAN_POINT ( 'NONE',  ( 93.67499999999999716, 87.70503267997126784, 88.91520833506763211 ) ) ;
#33029 = ORIENTED_EDGE ( 'NONE', *, *, #10021, .F. ) ;
#33030 = CARTESIAN_POINT ( 'NONE',  ( -94.99999999999997158, -207.3369185715606307, 78.68906250086713783 ) ) ;
#33031 = ORIENTED_EDGE ( 'NONE', *, *, #32943, .T. ) ;
#33032 = CARTESIAN_POINT ( 'NONE',  ( 13.83832728059186046, -142.6495187161941089, 5.500000000000000000 ) ) ;
#33033 = FACE_OUTER_BOUND ( 'NONE', #55387, .T. ) ;
#33034 = CARTESIAN_POINT ( 'NONE',  ( 11.99999999999999822, -50.23322058963393744, 64.81221759200325039 ) ) ;
#33035 = CARTESIAN_POINT ( 'NONE',  ( 0.000000000000000000, -67.80270845531855173, -46.11716303203260736 ) ) ;
#33036 = LINE ( 'NONE', #4496, #36623 ) ;
#33037 = CIRCLE ( 'NONE', #70219, 31.99999999999999645 ) ;
#33038 = CARTESIAN_POINT ( 'NONE',  ( -95.00000000000002842, 86.94004357329504273, 89.52374999999999261 ) ) ;
#33039 = CARTESIAN_POINT ( 'NONE',  ( 92.69370383062498320, 90.00000000000002842, 89.64281250086713726 ) ) ;
#33040 = DIRECTION ( 'NONE',  ( -0.000000000000000000, -0.000000000000000000, 1.000000000000000000 ) ) ;
#33041 = CARTESIAN_POINT ( 'NONE',  ( 2.500000000000015987, 65.00000000000000000, -290.0000000000000568 ) ) ;
#33042 = DIRECTION ( 'NONE',  ( -1.000000000000000000, -0.000000000000000000, -0.000000000000000000 ) ) ;
#33043 = CARTESIAN_POINT ( 'NONE',  ( 10.00000000000000000, 0.000000000000000000, 0.000000000000000000 ) ) ;
#33044 = CARTESIAN_POINT ( 'NONE',  ( 11.99999999999999822, 51.29473840253317007, -63.97538442413369353 ) ) ;
#33045 = DIRECTION ( 'NONE',  ( -1.000000000000000000, 0.000000000000000000, 0.000000000000000000 ) ) ;
#33046 = DIRECTION ( 'NONE',  ( 1.000000000000000000, 0.000000000000000000, 0.000000000000000000 ) ) ;
#33047 = CARTESIAN_POINT ( 'NONE',  ( -96.32500000000001705, 92.29496732002878900, 75.92416666666666458 ) ) ;
#33048 = DIRECTION ( 'NONE',  ( 0.000000000000000000, 0.000000000000000000, 1.000000000000000000 ) ) ;
#33049 = LINE ( 'NONE', #43353, #63765 ) ;
#33050 = FACE_OUTER_BOUND ( 'NONE', #40527, .T. ) ;
#33051 = CARTESIAN_POINT ( 'NONE',  ( 10.00000000000000000, 0.000000000000000000, 0.000000000000000000 ) ) ;
#33052 = CARTESIAN_POINT ( 'NONE',  ( -94.99999999999997158, -206.9400435732949575, 85.39624999999998067 ) ) ;
#33053 = ADVANCED_FACE ( 'NONE', ( #68049 ), #26696, .T. ) ;
#33054 = LINE ( 'NONE', #60545, #51775 ) ;
#33055 = AXIS2_PLACEMENT_3D ( 'NONE', #46492, #40867, #35207 ) ;
#33056 = CARTESIAN_POINT ( 'NONE',  ( 10.00000000000000000, 62.50329211542494789, -41.76937507738723099 ) ) ;
#33057 = CIRCLE ( 'NONE', #71486, 3.000000000000000444 ) ;
#33058 = CARTESIAN_POINT ( 'NONE',  ( 3.000000000000000000, 0.000000000000000000, -25.03750572909317285 ) ) ;
#33059 = CARTESIAN_POINT ( 'NONE',  ( 11.99999999999999822, -76.41127070299262414, -12.93880638057396304 ) ) ;
#33060 = LINE ( 'NONE', #39472, #17409 ) ;
#33061 = AXIS2_PLACEMENT_3D ( 'NONE', #51757, #67946, #45773 ) ;
#33062 = CARTESIAN_POINT ( 'NONE',  ( 97.30629616937498838, -211.3315407142195852, 88.16114583420048234 ) ) ;
#33063 = ORIENTED_EDGE ( 'NONE', *, *, #63252, .T. ) ;
#33064 = ADVANCED_FACE ( 'NONE', ( #50747, #3801 ), #67682, .T. ) ;
#33065 = AXIS2_PLACEMENT_3D ( 'NONE', #12610, #17886, #6974 ) ;
#33066 = VERTEX_POINT ( 'NONE', #26339 ) ;
#33068 = ADVANCED_FACE ( 'NONE', ( #43649 ), #39488, .T. ) ;
#33067 = CARTESIAN_POINT ( 'NONE',  ( 0.000000000000000000, -80.00000000000000000, -90.00000000000000000 ) ) ;
#33069 = DIRECTION ( 'NONE',  ( -1.000000000000000000, -0.000000000000000000, 0.000000000000000000 ) ) ;
#33070 = ORIENTED_EDGE ( 'NONE', *, *, #52602, .T. ) ;
#33071 = CIRCLE ( 'NONE', #55905, 15.99999999999999645 ) ;
#33072 = CARTESIAN_POINT ( 'NONE',  ( 92.69370383062501162, -209.9999999999999716, 78.21281250086714465 ) ) ;
#33073 = CARTESIAN_POINT ( 'NONE',  ( 95.00000000000000000, -207.3369185715606307, 86.46781250086714010 ) ) ;
#33074 = ORIENTED_EDGE ( 'NONE', *, *, #43975, .T. ) ;
#33075 = VECTOR ( 'NONE', #29413, 1000.000000000000000 ) ;
#33076 = CARTESIAN_POINT ( 'NONE',  ( 96.15314808468750130, -211.9973110713294489, 85.56822916753381492 ) ) ;
#33077 = EDGE_CURVE ( 'NONE', #11494, #73475, #56780, .T. ) ;
#33078 = EDGE_CURVE ( 'NONE', #72957, #17127, #49997, .T. ) ;
#33079 = EDGE_LOOP ( 'NONE', ( #59974, #9657, #48074, #18372 ) ) ;
#33080 = DIRECTION ( 'NONE',  ( -1.000000000000000000, 0.000000000000000000, -0.000000000000000000 ) ) ;
#33081 = ORIENTED_EDGE ( 'NONE', *, *, #72815, .F. ) ;
#33082 =( NAMED_UNIT ( * ) PLANE_ANGLE_UNIT ( ) SI_UNIT ( $, .RADIAN. ) );
#33083 = PRESENTATION_LAYER_ASSIGNMENT (  '', '', ( #28319 ) ) ;
#33084 = ORIENTED_EDGE ( 'NONE', *, *, #6972, .T. ) ;
#33085 = DIRECTION ( 'NONE',  ( -1.000000000000000000, 0.000000000000000000, 0.000000000000000000 ) ) ;
#33086 = ORIENTED_EDGE ( 'NONE', *, *, #50737, .T. ) ;
#33087 = CARTESIAN_POINT ( 'NONE',  ( 0.000000000000000000, -41.76106447765443619, -62.50884508063471401 ) ) ;
#33088 = CARTESIAN_POINT ( 'NONE',  ( 92.35000000000000853, -209.9999999999999716, 89.44437500173430067 ) ) ;
#33089 = VERTEX_POINT ( 'NONE', #61303 ) ;
#33090 = CARTESIAN_POINT ( 'NONE',  ( 10.00000000000000000, -31.46837873494930093, -68.27212725128309501 ) ) ;
#33091 = VERTEX_POINT ( 'NONE', #55651 ) ;
#33092 = LINE ( 'NONE', #16554, #30021 ) ;
#33093 = EDGE_CURVE ( 'NONE', #59084, #23150, #8244, .T. ) ;
#33094 = ORIENTED_EDGE ( 'NONE', *, *, #26387, .T. ) ;
#33095 = VERTEX_POINT ( 'NONE', #62433 ) ;
#33096 = EDGE_LOOP ( 'NONE', ( #11627, #43788, #9280, #8788 ) ) ;
#33097 = CARTESIAN_POINT ( 'NONE',  ( 0.000000000000000000, 0.000000000000000000, 0.000000000000000000 ) ) ;
#33098 = DIRECTION ( 'NONE',  ( 1.000000000000000000, 0.000000000000000000, 0.000000000000000000 ) ) ;
#33099 = ORIENTED_EDGE ( 'NONE', *, *, #49204, .F. ) ;
#33100 = ORIENTED_EDGE ( 'NONE', *, *, #43379, .F. ) ;
#33101 = ORIENTED_EDGE ( 'NONE', *, *, #40151, .F. ) ;
#33102 = CARTESIAN_POINT ( 'NONE',  ( -92.35000000000003695, 90.00000000000004263, 87.14249999999999829 ) ) ;
#33103 = CARTESIAN_POINT ( 'NONE',  ( 15.00000000000000000, 16.61724383029390140, 20.69703378468902955 ) ) ;
#33104 = CARTESIAN_POINT ( 'NONE',  ( -97.30629616937501680, 88.66845928578038638, 77.15447916753382174 ) ) ;
#33105 = EDGE_CURVE ( 'NONE', #41779, #19829, #46674, .T. ) ;
#33106 = EDGE_CURVE ( 'NONE', #3442, #12401, #39110, .T. ) ;
#33107 = VERTEX_POINT ( 'NONE', #9412 ) ;
#33108 = CARTESIAN_POINT ( 'NONE',  ( 97.30629616937498838, 91.33154071421968467, 77.31322916753380525 ) ) ;
#33109 = ORIENTED_EDGE ( 'NONE', *, *, #26124, .T. ) ;
#33110 = DIRECTION ( 'NONE',  ( -0.000000000000000000, 0.000000000000000000, 1.000000000000000000 ) ) ;
#33111 = CARTESIAN_POINT ( 'NONE',  ( -96.15314808468745866, -211.9973110713294489, 89.11364583420048291 ) ) ;
#33112 = VERTEX_POINT ( 'NONE', #44380 ) ;
#33113 = EDGE_CURVE ( 'NONE', #37924, #21174, #32338, .T. ) ;
#33114 = CARTESIAN_POINT ( 'NONE',  ( 3.453178355211938388, -3.779809238954861428, -0.7375898304884541679 ) ) ;
#33115 = CIRCLE ( 'NONE', #60777, 37.49900000000000944 ) ;
#33116 = DIRECTION ( 'NONE',  ( 0.000000000000000000, 0.000000000000000000, 1.000000000000000000 ) ) ;
#33117 = CARTESIAN_POINT ( 'NONE',  ( 15.70000000000602114, -120.0000000000001137, -70.60000000000039222 ) ) ;
#33118 = CARTESIAN_POINT ( 'NONE',  ( -92.69370383062498320, -209.9999999999999716, 79.16531250086714522 ) ) ;
#33119 = CYLINDRICAL_SURFACE ( 'NONE', #66267, 11.59999999999999787 ) ;
#33120 = DIRECTION ( 'NONE',  ( -1.000000000000000000, 0.000000000000000000, -0.000000000000000000 ) ) ;
#33121 = AXIS2_PLACEMENT_3D ( 'NONE', #41898, #48278, #24601 ) ;
#33122 = CARTESIAN_POINT ( 'NONE',  ( -3.000000000000000000, 14.60985201121704513, 18.46759930825707841 ) ) ;
#33123 = EDGE_LOOP ( 'NONE', ( #12485, #36346, #53558, #40979 ) ) ;
#33124 = TOROIDAL_SURFACE ( 'NONE', #39155, 13.10000000000000142, 0.5999999999999998668 ) ;
#33125 = ORIENTED_EDGE ( 'NONE', *, *, #31301, .T. ) ;
#33126 = FACE_OUTER_BOUND ( 'NONE', #47139, .T. ) ;
#33127 = VECTOR ( 'NONE', #35463, 1000.000000000000000 ) ;
#33128 = DIRECTION ( 'NONE',  ( 0.000000000000000000, 1.000000000000000000, 3.491481338843133750E-15 ) ) ;
#33129 = DIRECTION ( 'NONE',  ( 0.000000000000000000, 0.000000000000000000, -1.000000000000000000 ) ) ;
#33130 = CARTESIAN_POINT ( 'NONE',  ( -97.30629616937501680, 90.00000000000004263, 82.65781250086713783 ) ) ;
#33131 = CARTESIAN_POINT ( 'NONE',  ( 97.64999999999999147, 90.00000000000002842, 76.98250000000000171 ) ) ;
#33132 = PLANE ( 'NONE',  #62676 ) ;
#33133 = AXIS2_PLACEMENT_3D ( 'NONE', #6881, #35810, #58766 ) ;
#33134 = AXIS2_PLACEMENT_3D ( 'NONE', #28977, #63947, #29335 ) ;
#33135 = ORIENTED_EDGE ( 'NONE', *, *, #18241, .T. ) ;
#33136 = DIRECTION ( 'NONE',  ( 0.000000000000000000, 0.000000000000000000, -1.000000000000000000 ) ) ;
#33137 = FACE_OUTER_BOUND ( 'NONE', #43323, .T. ) ;
#33138 = CARTESIAN_POINT ( 'NONE',  ( -95.00000000000002842, 90.00000000000004263, 90.00000000000000000 ) ) ;
#33139 = CARTESIAN_POINT ( 'NONE',  ( 10.00000000000000000, 6.903761155838878061, -77.19088730480517313 ) ) ;
#33140 = CARTESIAN_POINT ( 'NONE',  ( 11.99999999999999822, 0.000000000000000000, 0.000000000000000000 ) ) ;
#33141 = AXIS2_PLACEMENT_3D ( 'NONE', #8679, #72544, #25958 ) ;
#33142 = CARTESIAN_POINT ( 'NONE',  ( 0.000000000000000000, 51.02545421589324803, 55.20638768913779870 ) ) ;
#33143 = CARTESIAN_POINT ( 'NONE',  ( -92.69370383062498320, -209.9999999999999716, 78.68906250086715204 ) ) ;
#33144 = DIRECTION ( 'NONE',  ( 1.000000000000000000, 0.000000000000000000, 0.000000000000000000 ) ) ;
#33145 = EDGE_CURVE ( 'NONE', #61936, #16380, #50260, .T. ) ;
#33146 = VERTEX_POINT ( 'NONE', #4542 ) ;
#33147 = DIRECTION ( 'NONE',  ( -1.000000000000000000, -0.000000000000000000, -0.000000000000000000 ) ) ;
#33148 = DIRECTION ( 'NONE',  ( 0.02332147558787671729, 0.9997280174009349762, -0.000000000000000000 ) ) ;
#33149 = DIRECTION ( 'NONE',  ( -1.000000000000000000, 7.955419762439749020E-15, 2.563413034563919251E-14 ) ) ;
#33150 = ORIENTED_EDGE ( 'NONE', *, *, #23673, .F. ) ;
#33151 = CARTESIAN_POINT ( 'NONE',  ( 12.00000000000000000, 23.59884966291538433, 12.14883922797231186 ) ) ;
#33152 = DIRECTION ( 'NONE',  ( -0.000000000000000000, -0.000000000000000000, 1.000000000000000000 ) ) ;
#33153 = EDGE_CURVE ( 'NONE', #8129, #12189, #8163, .T. ) ;
#33154 = AXIS2_PLACEMENT_3D ( 'NONE', #4851, #49561, #4101 ) ;
#33155 = ADVANCED_FACE ( 'NONE', ( #41328 ), #69489, .T. ) ;
#33156 = FACE_OUTER_BOUND ( 'NONE', #62800, .T. ) ;
#33157 = ORIENTED_EDGE ( 'NONE', *, *, #3907, .F. ) ;
#33158 = CARTESIAN_POINT ( 'NONE',  ( 92.34999999999999432, 90.00000000000002842, 78.57000000000000739 ) ) ;
#33159 = CARTESIAN_POINT ( 'NONE',  ( 15.00000000000000000, 22.07842321921480888, -8.187992925817425771 ) ) ;
#33160 = ORIENTED_EDGE ( 'NONE', *, *, #72729, .T. ) ;
#33161 = CARTESIAN_POINT ( 'NONE',  ( 97.30629616937498838, -208.6684592857803295, 88.74322916753382628 ) ) ;
#33162 = CARTESIAN_POINT ( 'NONE',  ( 92.35000000000000853, -209.9999999999999716, 86.18999999999999773 ) ) ;
#33163 = AXIS2_PLACEMENT_3D ( 'NONE', #50032, #67717, #4580 ) ;
#33164 = EDGE_LOOP ( 'NONE', ( #2880, #37270, #49357, #56055 ) ) ;
#33165 = CARTESIAN_POINT ( 'NONE',  ( 10.00000000000000000, 65.64334221924966073, -41.19522573413664190 ) ) ;
#33166 = ADVANCED_FACE ( 'NONE', ( #40219 ), #40968, .T. ) ;
#33167 = ORIENTED_EDGE ( 'NONE', *, *, #40011, .F. ) ;
#33168 = DIRECTION ( 'NONE',  ( 1.000000000000000000, -3.035766082959412415E-16, 0.000000000000000000 ) ) ;
#33169 = ORIENTED_EDGE ( 'NONE', *, *, #57389, .T. ) ;
#33170 = CARTESIAN_POINT ( 'NONE',  ( -90.00000000000000000, -116.0000000000000142, 39.99999999999996447 ) ) ;
#33171 = ORIENTED_EDGE ( 'NONE', *, *, #3599, .T. ) ;
#33172 = ORIENTED_EDGE ( 'NONE', *, *, #66617, .T. ) ;
#33173 = CIRCLE ( 'NONE', #39206, 82.00000000000000000 ) ;
#33174 = ORIENTED_EDGE ( 'NONE', *, *, #61681, .T. ) ;
#33175 = CARTESIAN_POINT ( 'NONE',  ( -95.00000000000002842, 90.00000000000004263, 73.40771935957695860 ) ) ;
#33176 = VERTEX_POINT ( 'NONE', #35319 ) ;
#33177 = PRODUCT_DEFINITION_SHAPE ( 'NONE', 'NONE',  #74345 ) ;
#33178 = ADVANCED_FACE ( 'NONE', ( #63904 ), #57517, .F. ) ;
#33179 = ORIENTED_EDGE ( 'NONE', *, *, #28336, .T. ) ;
#33180 =( BOUNDED_CURVE ( )  B_SPLINE_CURVE ( 2, ( #7751, #30300, #47597, #30665, #53245, #41587, #29552 ),
 .UNSPECIFIED., .F., .F. ) 
 B_SPLINE_CURVE_WITH_KNOTS ( ( 3, 2, 2, 3 ),
 ( 0.9374999999999995559, 0.9444444444444441977, 0.9513888888888889506, 0.9583333333333337034 ),
 .UNSPECIFIED. ) 
 CURVE ( )  GEOMETRIC_REPRESENTATION_ITEM ( )  RATIONAL_B_SPLINE_CURVE ( ( 1.000000000000008660, 0.8660254037844301589, 1.000000000000000000, 0.8660254037844387076, 1.000000000000000000, 0.8660254037844322683, 1.000000000000006439 ) ) 
 REPRESENTATION_ITEM ( '' )  );
#33181 = CARTESIAN_POINT ( 'NONE',  ( 96.15314808468748708, 88.00268892867053694, 77.31322916753381946 ) ) ;
#33182 = CARTESIAN_POINT ( 'NONE',  ( 5.000000000000002665, 29.01471420065564644, 76.69515212746026123 ) ) ;
#33183 = EDGE_CURVE ( 'NONE', #74032, #69905, #35937, .T. ) ;
#33184 = CARTESIAN_POINT ( 'NONE',  ( -26.49999999999781863, -119.9999999999996021, -49.00000000000066080 ) ) ;
#33185 = VERTEX_POINT ( 'NONE', #6030 ) ;
#33186 = ORIENTED_EDGE ( 'NONE', *, *, #44913, .F. ) ;
#33187 = EDGE_LOOP ( 'NONE', ( #3424, #30477, #48445, #42001 ) ) ;
#33188 = CARTESIAN_POINT ( 'NONE',  ( 97.30629616937498838, 90.00000000000002842, 87.42031250086714067 ) ) ;
#33190 = ORIENTED_EDGE ( 'NONE', *, *, #12021, .F. ) ;
#33189 = EDGE_CURVE ( 'NONE', #43729, #20222, #49145, .T. ) ;
#33191 = CARTESIAN_POINT ( 'NONE',  ( 92.69370383062501162, -209.9999999999999716, 83.92781250086714806 ) ) ;
#33192 = APPLICATION_PROTOCOL_DEFINITION ( 'draft international standard', 'automotive_design', 1998, #62377 ) ;
#33193 = LINE ( 'NONE', #3551, #24711 ) ;
#33194 = DIRECTION ( 'NONE',  ( 0.000000000000000000, 0.5877852522924743583, -0.8090169943749466741 ) ) ;
#33195 = CARTESIAN_POINT ( 'NONE',  ( 10.00000000000000000, 33.80338159004283938, 16.23288003029508886 ) ) ;
#33196 = CARTESIAN_POINT ( 'NONE',  ( 10.00000000000000000, 37.22597642581158084, -5.202137450156524068 ) ) ;
#33197 = LINE ( 'NONE', #44504, #34818 ) ;
#33198 = FACE_OUTER_BOUND ( 'NONE', #17125, .T. ) ;
#33199 = CARTESIAN_POINT ( 'NONE',  ( -94.99999999999997158, -212.6630814284392557, 87.26156250086714294 ) ) ;
#33200 = CARTESIAN_POINT ( 'NONE',  ( -95.00000000000002842, 92.66308142843932671, 86.46781250086716852 ) ) ;
#33201 = EDGE_CURVE ( 'NONE', #69905, #45064, #3556, .T. ) ;
#33202 = ORIENTED_EDGE ( 'NONE', *, *, #27744, .F. ) ;
#33204 = CARTESIAN_POINT ( 'NONE',  ( -92.69370383062502583, 91.33154071421968467, 88.10822916753380696 ) ) ;
#33203 = CARTESIAN_POINT ( 'NONE',  ( 97.30629616937498838, 90.00000000000002842, 89.32531250086714181 ) ) ;
#33205 = ORIENTED_EDGE ( 'NONE', *, *, #664, .T. ) ;
#33206 = PLANE ( 'NONE',  #7035 ) ;
#33207 = FACE_OUTER_BOUND ( 'NONE', #18774, .T. ) ;
#33208 = DIRECTION ( 'NONE',  ( 1.000000000000000000, 0.000000000000000000, 0.000000000000000000 ) ) ;
#33209 = DIRECTION ( 'NONE',  ( 0.000000000000000000, 0.7071067811865487940, -0.7071067811865462405 ) ) ;
#33210 = CARTESIAN_POINT ( 'NONE',  ( -97.30629616937495996, -209.9999999999999716, 89.00781250086714635 ) ) ;
#33211 = LINE ( 'NONE', #34333, #5480 ) ;
#33212 = LINE ( 'NONE', #27584, #37406 ) ;
#33213 = DIRECTION ( 'NONE',  ( 0.000000000000000000, 0.000000000000000000, 1.000000000000000000 ) ) ;
#33214 = ORIENTED_EDGE ( 'NONE', *, *, #59252, .F. ) ;
#33215 = CIRCLE ( 'NONE', #71629, 32.00000000000000000 ) ;
#33216 = ORIENTED_EDGE ( 'NONE', *, *, #38442, .T. ) ;
#33217 = CARTESIAN_POINT ( 'NONE',  ( -92.35000000000005116, 91.52997821335253548, 80.21041666666666003 ) ) ;
#33218 = LINE ( 'NONE', #5427, #71503 ) ;
#33219 = FACE_OUTER_BOUND ( 'NONE', #26152, .T. ) ;
#33220 = CARTESIAN_POINT ( 'NONE',  ( 0.000000000000000000, -120.0000000000000000, 2.500000000000000000 ) ) ;
#33221 = CARTESIAN_POINT ( 'NONE',  ( 12.00000000000000000, -14.54903810567676636, -22.19967320028756674 ) ) ;
#33222 = CARTESIAN_POINT ( 'NONE',  ( 92.35000000003358878, -210.0000076551254153, 78.01464417100928017 ) ) ;
#33223 = CYLINDRICAL_SURFACE ( 'NONE', #49220, 31.99999999999998579 ) ;
#33224 = AXIS2_PLACEMENT_3D ( 'NONE', #30805, #53753, #25187 ) ;
#33225 = ORIENTED_EDGE ( 'NONE', *, *, #72806, .T. ) ;
#33226 = CARTESIAN_POINT ( 'NONE',  ( -92.69370383062502583, 88.66845928578038638, 81.01739583420048518 ) ) ;
#33227 = AXIS2_PLACEMENT_3D ( 'NONE', #17018, #11724, #57620 ) ;
#33228 = CARTESIAN_POINT ( 'NONE',  ( 0.000000000000000000, -89.50000000000000000, -5.500000000000000000 ) ) ;
#33229 = LINE ( 'NONE', #55809, #12642 ) ;
#33230 = DIRECTION ( 'NONE',  ( 0.000000000000000000, 0.9510565162951544194, -0.3090169943749446757 ) ) ;
#33231 = CIRCLE ( 'NONE', #30810, 37.49900000000000233 ) ;
#33232 = DIRECTION ( 'NONE',  ( -0.000000000000000000, -0.000000000000000000, 1.000000000000000000 ) ) ;
#33233 = CARTESIAN_POINT ( 'NONE',  ( -96.32500000000001705, 92.29496732002878900, 82.27416666666665890 ) ) ;
#33234 = VECTOR ( 'NONE', #35916, 1000.000000000000000 ) ;
#33235 = VECTOR ( 'NONE', #1934, 1000.000000000000000 ) ;
#33236 = CARTESIAN_POINT ( 'NONE',  ( 94.99999999999998579, 92.66308142843932671, 82.02281250086714692 ) ) ;
#33237 = CARTESIAN_POINT ( 'NONE',  ( -94.99999999999997158, -212.6630814284392557, 79.80031250086715033 ) ) ;
#33238 = DIRECTION ( 'NONE',  ( 0.000000000000000000, 0.000000000000000000, 1.000000000000000000 ) ) ;
#33239 = ORIENTED_EDGE ( 'NONE', *, *, #7877, .F. ) ;
#33240 = CARTESIAN_POINT ( 'NONE',  ( -0.0004442498508594591917, 0.001194404164628348752, -65.00000000000000000 ) ) ;
#33241 = CARTESIAN_POINT ( 'NONE',  ( -97.64999999999994884, -211.5299782133524502, 75.44791666666667140 ) ) ;
#33242 = EDGE_CURVE ( 'NONE', #70028, #39032, #17657, .T. ) ;
#33243 = EDGE_CURVE ( 'NONE', #64733, #74246, #64709, .T. ) ;
#33244 = AXIS2_PLACEMENT_3D ( 'NONE', #62711, #16076, #15707 ) ;
#33245 = ADVANCED_FACE ( 'NONE', ( #22562 ), #45507, .F. ) ;
#33246 = CARTESIAN_POINT ( 'NONE',  ( -92.69370383062505425, 91.33154071421968467, 78.10697916753383652 ) ) ;
#33247 = CARTESIAN_POINT ( 'NONE',  ( 93.84685191531249870, -208.0026889286704943, 81.28197916753380525 ) ) ;
#33248 = ORIENTED_EDGE ( 'NONE', *, *, #53324, .T. ) ;
#33249 = VECTOR ( 'NONE', #860, 1000.000000000000000 ) ;
#33250 = DIRECTION ( 'NONE',  ( -1.000000000000000000, 7.571543891232750625E-15, 2.563413034563919882E-14 ) ) ;
#33251 = EDGE_LOOP ( 'NONE', ( #27741, #32776, #74201, #16266 ) ) ;
#33252 = EDGE_CURVE ( 'NONE', #36430, #21993, #777, .T. ) ;
#33253 = DIRECTION ( 'NONE',  ( -1.000000000000000000, 0.000000000000000000, 0.000000000000000000 ) ) ;
#33254 = ORIENTED_EDGE ( 'NONE', *, *, #37794, .T. ) ;
#33255 = DIRECTION ( 'NONE',  ( 0.000000000000000000, 0.000000000000000000, 1.000000000000000000 ) ) ;
#33256 = ORIENTED_EDGE ( 'NONE', *, *, #24029, .F. ) ;
#33257 = ORIENTED_EDGE ( 'NONE', *, *, #59430, .F. ) ;
#33258 = ORIENTED_EDGE ( 'NONE', *, *, #12900, .F. ) ;
#33259 = DIRECTION ( 'NONE',  ( -1.000000000000000000, -0.000000000000000000, 0.000000000000000000 ) ) ;
#33260 = ORIENTED_EDGE ( 'NONE', *, *, #52344, .T. ) ;
#33261 = CARTESIAN_POINT ( 'NONE',  ( 0.000000000000000000, -26.02418014898359289, 70.52718814184250107 ) ) ;
#33262 = DIRECTION ( 'NONE',  ( -1.000000000000000000, 0.000000000000000000, -0.000000000000000000 ) ) ;
#33263 = CARTESIAN_POINT ( 'NONE',  ( 93.84685191531248449, 91.99731107132950569, 85.88572916753381037 ) ) ;
#33264 = CARTESIAN_POINT ( 'NONE',  ( -26.50044424985255276, 0.001194404164626844313, -80.00000000000000000 ) ) ;
#33265 = CARTESIAN_POINT ( 'NONE',  ( 93.67500000000001137, -207.7050326799711968, 79.09916666666666174 ) ) ;
#33266 = CIRCLE ( 'NONE', #10482, 11.59999999999999787 ) ;
#33267 = ORIENTED_EDGE ( 'NONE', *, *, #31155, .F. ) ;
#33268 = ORIENTED_EDGE ( 'NONE', *, *, #70165, .T. ) ;
#33269 = ORIENTED_EDGE ( 'NONE', *, *, #7478, .T. ) ;
#33270 = ORIENTED_EDGE ( 'NONE', *, *, #8818, .F. ) ;
#33271 = PRESENTATION_STYLE_ASSIGNMENT (( #61131 ) ) ;
#33272 = EDGE_CURVE ( 'NONE', #28934, #68126, #412, .T. ) ;
#33273 = EDGE_CURVE ( 'NONE', #21836, #19615, #53835, .T. ) ;
#33274 =( LENGTH_UNIT ( ) NAMED_UNIT ( * ) SI_UNIT ( .MILLI., .METRE. ) );
#33275 = DIRECTION ( 'NONE',  ( 0.000000000000000000, -0.8090169943749402348, -0.5877852522924830181 ) ) ;
#33276 = CIRCLE ( 'NONE', #54913, 37.49900000000000233 ) ;
#33277 = DIRECTION ( 'NONE',  ( 0.000000000000000000, 0.000000000000000000, 1.000000000000000000 ) ) ;
#33278 = VECTOR ( 'NONE', #46023, 1000.000000000000000 ) ;
#33279 = DIRECTION ( 'NONE',  ( 0.000000000000000000, 0.000000000000000000, 1.000000000000000000 ) ) ;
#33280 = CYLINDRICAL_SURFACE ( 'NONE', #70756, 2.649999999999999467 ) ;
#33281 = DIRECTION ( 'NONE',  ( 1.000000000000000000, 0.000000000000000000, 0.000000000000000000 ) ) ;
#33282 = ORIENTED_EDGE ( 'NONE', *, *, #15871, .T. ) ;
#33283 = CARTESIAN_POINT ( 'NONE',  ( -96.32499999999996021, -207.7050326799711968, 84.25854166840096582 ) ) ;
#33284 = EDGE_LOOP ( 'NONE', ( #35495, #65230, #25506, #35086 ) ) ;
#33285 = DIRECTION ( 'NONE',  ( 1.000000000000000000, 0.000000000000000000, 0.000000000000000000 ) ) ;
#33286 = EDGE_CURVE ( 'NONE', #20440, #20082, #34950, .T. ) ;
#33287 = ORIENTED_EDGE ( 'NONE', *, *, #22533, .F. ) ;
#33289 = CARTESIAN_POINT ( 'NONE',  ( -97.65000000000001990, 88.47002178664754979, 82.51229166840094820 ) ) ;
#33288 = CARTESIAN_POINT ( 'NONE',  ( 93.67499999999998295, 92.29496732002878900, 82.98854166840096980 ) ) ;
#33290 = EDGE_LOOP ( 'NONE', ( #46779, #65233, #43568, #30299 ) ) ;
#33291 = CARTESIAN_POINT ( 'NONE',  ( 96.15314808468748708, 88.00268892867053694, 84.93322916753382401 ) ) ;
#33292 = DIRECTION ( 'NONE',  ( 0.000000000000000000, 0.5877852522924744694, -0.8090169943749465631 ) ) ;
#33293 = DIRECTION ( 'NONE',  ( 0.000000000000000000, 0.000000000000000000, 1.000000000000000000 ) ) ;
#33294 = CARTESIAN_POINT ( 'NONE',  ( 11.99999999999999822, -71.87247863392441616, 39.47590169984818687 ) ) ;
#33295 = DIRECTION ( 'NONE',  ( 0.000000000000000000, -0.7071067811865389130, -0.7071067811865561215 ) ) ;
#33296 = ORIENTED_EDGE ( 'NONE', *, *, #19104, .F. ) ;
#33297 = FACE_OUTER_BOUND ( 'NONE', #6023, .T. ) ;
#33298 = LINE ( 'NONE', #56254, #24139 ) ;
#33299 = CARTESIAN_POINT ( 'NONE',  ( 13.36666666666666536, 1.636944554860295198E-15, -1.466666666666671670 ) ) ;
#33300 = VERTEX_POINT ( 'NONE', #23663 ) ;
#33301 = ORIENTED_EDGE ( 'NONE', *, *, #14574, .F. ) ;
#33302 = AXIS2_PLACEMENT_3D ( 'NONE', #4275, #27923, #39586 ) ;
#33303 = CARTESIAN_POINT ( 'NONE',  ( 0.000000000000000000, 36.72794159290241822, 65.59268652807223532 ) ) ;
#33304 = CARTESIAN_POINT ( 'NONE',  ( 10.00000000000000000, 0.8828120875900632436, 37.48860685352291000 ) ) ;
#33305 = LINE ( 'NONE', #4783, #48510 ) ;
#33306 = CARTESIAN_POINT ( 'NONE',  ( -93.84685191531248449, -208.0026889286704943, 82.60489583420049087 ) ) ;
#33307 = ORIENTED_EDGE ( 'NONE', *, *, #19345, .F. ) ;
#33308 = CARTESIAN_POINT ( 'NONE',  ( 12.49999999999999645, 1.530808498934191127E-15, 42.00000000000001421 ) ) ;
#33309 = EDGE_LOOP ( 'NONE', ( #42615, #49766, #5380, #22543 ) ) ;
#33310 = DIRECTION ( 'NONE',  ( -1.000000000000000000, -0.000000000000000000, -0.000000000000000000 ) ) ;
#33311 = CARTESIAN_POINT ( 'NONE',  ( 0.000000000000000000, -68.55367621811173251, 44.99326035066031437 ) ) ;
#33312 = DIRECTION ( 'NONE',  ( -1.000000000000000000, 0.000000000000000000, 0.000000000000000000 ) ) ;
#33313 = CARTESIAN_POINT ( 'NONE',  ( 10.00000000000000000, 35.92658777277525672, -10.74501242461245809 ) ) ;
#33314 = LINE ( 'NONE', #51360, #16070 ) ;
#33315 = CARTESIAN_POINT ( 'NONE',  ( 10.00000000000000000, 71.27951684758069462, -30.41916302227035729 ) ) ;
#33316 = DIRECTION ( 'NONE',  ( 0.000000000000000000, 0.000000000000000000, 1.000000000000000000 ) ) ;
#33317 = DIRECTION ( 'NONE',  ( 1.343011723336883198E-16, -1.000000000000000000, 0.000000000000000000 ) ) ;
#33318 = FACE_BOUND ( 'NONE', #27053, .T. ) ;
#33319 = DIRECTION ( 'NONE',  ( -0.000000000000000000, -0.000000000000000000, -1.000000000000000000 ) ) ;
#33320 = AXIS2_PLACEMENT_3D ( 'NONE', #32623, #10441, #22477 ) ;
#33321 = CARTESIAN_POINT ( 'NONE',  ( 10.00000000000000000, 75.16055320797059380, -18.89407956138177269 ) ) ;
#33322 = CARTESIAN_POINT ( 'NONE',  ( 96.15314808468748708, 88.00268892867053694, 89.37822916753381719 ) ) ;
#33323 = CIRCLE ( 'NONE', #62174, 31.99999999999999289 ) ;
#33324 = FACE_OUTER_BOUND ( 'NONE', #44675, .T. ) ;
#33325 = CARTESIAN_POINT ( 'NONE',  ( 10.00000000000000000, -81.90746397400386059, -3.894527615418773347 ) ) ;
#33326 = ORIENTED_EDGE ( 'NONE', *, *, #13419, .F. ) ;
#33327 = EDGE_CURVE ( 'NONE', #30842, #52479, #15397, .T. ) ;
#33328 = CARTESIAN_POINT ( 'NONE',  ( -97.30629616937501680, 91.33154071421968467, 80.69989583420046131 ) ) ;
#33329 = EDGE_CURVE ( 'NONE', #23304, #24152, #13118, .T. ) ;
#33330 = VECTOR ( 'NONE', #12438, 1000.000000000000000 ) ;
#33331 = ADVANCED_FACE ( 'NONE', ( #7486, #20228 ), #71354, .T. ) ;
#33332 = DIRECTION ( 'NONE',  ( -0.000000000000000000, -0.000000000000000000, 1.000000000000000000 ) ) ;
#33333 = ORIENTED_EDGE ( 'NONE', *, *, #2167, .F. ) ;
#33334 = EDGE_CURVE ( 'NONE', #50088, #31458, #41688, .T. ) ;
#33335 = CARTESIAN_POINT ( 'NONE',  ( 0.000000000000000000, 30.84782396557248418, -21.32104025579081252 ) ) ;
#33336 = CARTESIAN_POINT ( 'NONE',  ( -14.53333333333331545, 1.779820014760817565E-15, -1.466666666666671670 ) ) ;
#33337 = DIRECTION ( 'NONE',  ( 0.000000000000000000, 0.5877852522924744694, -0.8090169943749465631 ) ) ;
#33338 = EDGE_CURVE ( 'NONE', #13514, #57170, #71940, .T. ) ;
#33339 = LINE ( 'NONE', #56300, #34722 ) ;
#33340 = CARTESIAN_POINT ( 'NONE',  ( 95.00000000000000000, -212.6630814284392557, 76.62531250086715318 ) ) ;
#33341 = AXIS2_PLACEMENT_3D ( 'NONE', #69073, #53257, #13397 ) ;
#33342 = AXIS2_PLACEMENT_3D ( 'NONE', #12311, #69457, #24705 ) ;
#33343 = ORIENTED_EDGE ( 'NONE', *, *, #29268, .T. ) ;
#33344 = VERTEX_POINT ( 'NONE', #2628 ) ;
#33345 = VECTOR ( 'NONE', #69063, 1000.000000000000000 ) ;
#33346 = EDGE_CURVE ( 'NONE', #4389, #34691, #1882, .T. ) ;
#33347 = CIRCLE ( 'NONE', #62201, 42.00000000000000000 ) ;
#33348 = ADVANCED_FACE ( 'NONE', ( #70243 ), #13843, .T. ) ;
#33349 = DIRECTION ( 'NONE',  ( -1.000000000000000000, 0.000000000000000000, -0.000000000000000000 ) ) ;
#33350 = CYLINDRICAL_SURFACE ( 'NONE', #56764, 77.49899999999999523 ) ;
#33351 = AXIS2_PLACEMENT_3D ( 'NONE', #14391, #21128, #31676 ) ;
#33352 = CARTESIAN_POINT ( 'NONE',  ( 15.00000000000000000, 23.49999999999999645, 1.499999999999995337 ) ) ;
#33353 = FACE_OUTER_BOUND ( 'NONE', #16155, .T. ) ;
#33354 = CARTESIAN_POINT ( 'NONE',  ( 10.00000000000000000, -55.38113227695743745, -54.21277698773734244 ) ) ;
#33355 = CARTESIAN_POINT ( 'NONE',  ( 93.67500000000001137, -207.7050326799711968, 88.62416666666665321 ) ) ;
#33356 = EDGE_LOOP ( 'NONE', ( #68968, #48555, #38768, #54937 ) ) ;
#33357 = CARTESIAN_POINT ( 'NONE',  ( -97.64999999999990621, -208.4700217866474077, 88.04208333333330927 ) ) ;
#33358 = ORIENTED_EDGE ( 'NONE', *, *, #71967, .T. ) ;
#33359 = ORIENTED_EDGE ( 'NONE', *, *, #31783, .T. ) ;
#33360 = LINE ( 'NONE', #50662, #26135 ) ;
#33361 = EDGE_CURVE ( 'NONE', #366, #70501, #31105, .T. ) ;
#33362 = EDGE_CURVE ( 'NONE', #1463, #7305, #25507, .T. ) ;
#33363 = FACE_OUTER_BOUND ( 'NONE', #60914, .T. ) ;
#33364 = ORIENTED_EDGE ( 'NONE', *, *, #72728, .F. ) ;
#33365 = CARTESIAN_POINT ( 'NONE',  ( 97.64999999999997726, -208.4700217866474645, 79.65479166840096070 ) ) ;
#33366 = CARTESIAN_POINT ( 'NONE',  ( 97.64999999999997726, 88.47002178664753558, 81.37458333333333371 ) ) ;
#33367 = ORIENTED_EDGE ( 'NONE', *, *, #50751, .T. ) ;
#33368 = CARTESIAN_POINT ( 'NONE',  ( 92.35000000000000853, -209.9999999999999716, 75.47437500173430180 ) ) ;
#33369 = ORIENTED_EDGE ( 'NONE', *, *, #8395, .F. ) ;
#33370 = DIRECTION ( 'NONE',  ( -1.000000000000000000, 0.000000000000000000, -0.000000000000000000 ) ) ;
#33371 = EDGE_LOOP ( 'NONE', ( #26995, #44384, #24704, #71663 ) ) ;
#33372 = CARTESIAN_POINT ( 'NONE',  ( 10.00000000000000000, -22.74946021919110706, -29.81001611431033282 ) ) ;
#33373 = CARTESIAN_POINT ( 'NONE',  ( -97.30629616937501680, 90.00000000000004263, 84.72156250086715090 ) ) ;
#33374 = AXIS2_PLACEMENT_3D ( 'NONE', #10735, #45329, #67506 ) ;
#33375 = CARTESIAN_POINT ( 'NONE',  ( 96.15314808468748708, 88.00268892867053694, 78.42447916753381776 ) ) ;
#33376 = ORIENTED_EDGE ( 'NONE', *, *, #51631, .T. ) ;
#33377 = CYLINDRICAL_SURFACE ( 'NONE', #10548, 31.99999999999998579 ) ;
#33378 = CIRCLE ( 'NONE', #16596, 15.99999999999999822 ) ;
#33379 = AXIS2_PLACEMENT_3D ( 'NONE', #43162, #3314, #14936 ) ;
#33380 = DIRECTION ( 'NONE',  ( 0.000000000000000000, 0.000000000000000000, 1.000000000000000000 ) ) ;
#33381 = DIRECTION ( 'NONE',  ( -0.3311129884571281101, -0.9435911131814402886, 0.000000000000000000 ) ) ;
#33382 = FACE_OUTER_BOUND ( 'NONE', #37169, .T. ) ;
#33383 = EDGE_LOOP ( 'NONE', ( #38366, #73615, #33558, #34125 ) ) ;
#33384 = CARTESIAN_POINT ( 'NONE',  ( 10.00000000000000000, -18.89407956138310496, 75.16055320797023853 ) ) ;
#33385 = CARTESIAN_POINT ( 'NONE',  ( -96.15314808468745866, -211.9973110713294489, 78.95364583420047211 ) ) ;
#33386 = ORIENTED_EDGE ( 'NONE', *, *, #25861, .F. ) ;
#33387 = ORIENTED_EDGE ( 'NONE', *, *, #44665, .T. ) ;
#33388 = AXIS2_PLACEMENT_3D ( 'NONE', #4242, #71147, #19652 ) ;
#33389 = CARTESIAN_POINT ( 'NONE',  ( 96.32499999999997442, 92.29496732002878900, 78.99333333333332519 ) ) ;
#33390 = VERTEX_POINT ( 'NONE', #37174 ) ;
#33391 = CARTESIAN_POINT ( 'NONE',  ( 1.560000000000000053, -0.8660254037844384856, -1.500000000000000000 ) ) ;
#33392 = CARTESIAN_POINT ( 'NONE',  ( -3.000000000000000000, -11.95096189432345390, 23.69967320028757385 ) ) ;
#33393 = ORIENTED_EDGE ( 'NONE', *, *, #69910, .T. ) ;
#33394 = CARTESIAN_POINT ( 'NONE',  ( -92.69370383062498320, -208.6684592857803011, 75.40822916753381833 ) ) ;
#33395 = ORIENTED_EDGE ( 'NONE', *, *, #25572, .F. ) ;
#33396 = DIRECTION ( 'NONE',  ( 1.000000000000000000, 0.000000000000000000, 0.000000000000000000 ) ) ;
#33397 = CARTESIAN_POINT ( 'NONE',  ( 15.00000000000000000, -11.95096189432345746, -23.69967320028757030 ) ) ;
#33398 = CARTESIAN_POINT ( 'NONE',  ( 15.00000000000000000, -25.60904388321925040, -6.976881207771165272 ) ) ;
#33399 = CARTESIAN_POINT ( 'NONE',  ( -97.64999999999996305, -209.9999999999999716, 89.44437500173430067 ) ) ;
#33400 = CARTESIAN_POINT ( 'NONE',  ( 11.99999999999999822, -73.95703589263990807, 23.16143007188399139 ) ) ;
#33401 = CIRCLE ( 'NONE', #3436, 37.49900000000000944 ) ;
#33402 = DIRECTION ( 'NONE',  ( -1.000000000000000000, 0.000000000000000000, 0.000000000000000000 ) ) ;
#33404 = AXIS2_PLACEMENT_3D ( 'NONE', #9262, #19424, #14530 ) ;
#33403 = CARTESIAN_POINT ( 'NONE',  ( 93.84685191531248449, 91.99731107132950569, 87.63197916753379957 ) ) ;
#33405 = CARTESIAN_POINT ( 'NONE',  ( -92.35000000000005116, -211.0554082285339916, 75.04099707143593889 ) ) ;
#33406 = CARTESIAN_POINT ( 'NONE',  ( 0.000000000000000000, -10.45096189432314837, -21.10159698893440350 ) ) ;
#33407 = DIRECTION ( 'NONE',  ( 1.000000000000000000, 0.000000000000000000, 0.000000000000000000 ) ) ;
#33408 = AXIS2_PLACEMENT_3D ( 'NONE', #42995, #24949, #71167 ) ;
#33409 = DIRECTION ( 'NONE',  ( 0.000000000000000000, 0.000000000000000000, 1.000000000000000000 ) ) ;
#33411 = EDGE_CURVE ( 'NONE', #73705, #16368, #28696, .T. ) ;
#33410 = AXIS2_PLACEMENT_3D ( 'NONE', #5712, #63225, #28989 ) ;
#33412 = CARTESIAN_POINT ( 'NONE',  ( 10.00000000000000178, 1.530808498934191521E-15, -12.50000000000000000 ) ) ;
#33413 = CARTESIAN_POINT ( 'NONE',  ( 12.00000000000000000, 23.49999999999999645, 1.499999999999995337 ) ) ;
#33414 = DIRECTION ( 'NONE',  ( 0.000000000000000000, 0.000000000000000000, 1.000000000000000000 ) ) ;
#33415 = EDGE_CURVE ( 'NONE', #25489, #24434, #48806, .T. ) ;
#33416 =( BOUNDED_CURVE ( )  B_SPLINE_CURVE ( 2, ( #64406, #68937, #57660, #64040, #6166, #29069, #23443 ),
 .UNSPECIFIED., .F., .F. ) 
 B_SPLINE_CURVE_WITH_KNOTS ( ( 3, 2, 2, 3 ),
 ( 0.06249999999999966693, 0.06944444444444407283, 0.07638888888888849260, 0.08333333333333288462 ),
 .UNSPECIFIED. ) 
 CURVE ( )  GEOMETRIC_REPRESENTATION_ITEM ( )  RATIONAL_B_SPLINE_CURVE ( ( 1.000000000000006439, 0.8660254037844322683, 1.000000000000000000, 0.8660254037844387076, 1.000000000000000000, 0.8660254037844472563, 0.9999999999999914513 ) ) 
 REPRESENTATION_ITEM ( '' )  );
#33417 = CARTESIAN_POINT ( 'NONE',  ( -97.65000000000009095, 91.52997821335249284, 75.97708333333333997 ) ) ;
#33418 = DIRECTION ( 'NONE',  ( 0.000000000000000000, 0.000000000000000000, 1.000000000000000000 ) ) ;
#33419 = PRODUCT_DEFINITION ( 'UNKNOWN', '', #73629, #25845 ) ;
#33420 = EDGE_CURVE ( 'NONE', #40627, #1606, #59731, .T. ) ;
#33421 = DIRECTION ( 'NONE',  ( -1.000000000000000000, -0.000000000000000000, -0.000000000000000000 ) ) ;
#33422 = CARTESIAN_POINT ( 'NONE',  ( -92.35000000000003695, 90.00000000000004263, 90.00000000000000000 ) ) ;
#33423 = CARTESIAN_POINT ( 'NONE',  ( 5.204170427930421283E-15, 1.567547902908612184E-15, 12.79999999999999893 ) ) ;
#33424 = EDGE_CURVE ( 'NONE', #57988, #40784, #55155, .T. ) ;
#33425 = CARTESIAN_POINT ( 'NONE',  ( -97.64999999999994884, -208.4700217866474645, 83.59708333333334451 ) ) ;
#33426 = DIRECTION ( 'NONE',  ( -1.000000000000000000, 0.000000000000000000, 0.000000000000000000 ) ) ;
#33427 = EDGE_CURVE ( 'NONE', #66194, #16558, #52979, .T. ) ;
#33428 = CIRCLE ( 'NONE', #62282, 31.99999999999997868 ) ;
#33429 = DIRECTION ( 'NONE',  ( -1.000000000000000000, 0.000000000000000000, -0.000000000000000000 ) ) ;
#33430 = FACE_OUTER_BOUND ( 'NONE', #41617, .T. ) ;
#33431 = CARTESIAN_POINT ( 'NONE',  ( 10.00000000000000000, 0.000000000000000000, 0.000000000000000000 ) ) ;
#33432 = AXIS2_PLACEMENT_3D ( 'NONE', #1669, #52764, #34727 ) ;
#33433 = CIRCLE ( 'NONE', #46655, 26.50000000000552092 ) ;
#33434 = DIRECTION ( 'NONE',  ( 0.000000000000000000, 0.8660254037844363761, 0.5000000000000039968 ) ) ;
#33435 = CARTESIAN_POINT ( 'NONE',  ( 97.30629616937498838, -209.9999999999999716, 87.57906250086715261 ) ) ;
#33436 = VECTOR ( 'NONE', #32687, 1000.000000000000000 ) ;
#33437 = ORIENTED_EDGE ( 'NONE', *, *, #32125, .F. ) ;
#33438 = ORIENTED_EDGE ( 'NONE', *, *, #45196, .T. ) ;
#33439 = EDGE_CURVE ( 'NONE', #40791, #53797, #24770, .T. ) ;
#33440 = EDGE_CURVE ( 'NONE', #9966, #30983, #24402, .T. ) ;
#33441 = LINE ( 'NONE', #39478, #59624 ) ;
#33442 = VERTEX_POINT ( 'NONE', #13489 ) ;
#33443 = DIRECTION ( 'NONE',  ( 1.000000000000000000, 0.000000000000000000, 0.000000000000000000 ) ) ;
#33444 = CARTESIAN_POINT ( 'NONE',  ( 93.84685191531249870, -208.0026889286704943, 76.83697916753381207 ) ) ;
#33445 = ORIENTED_EDGE ( 'NONE', *, *, #11598, .T. ) ;
#33446 = CARTESIAN_POINT ( 'NONE',  ( 95.00000000000000000, -207.3369185715606307, 81.38781250086715602 ) ) ;
#33447 = CIRCLE ( 'NONE', #65898, 31.99999999999998579 ) ;
#33448 = ORIENTED_EDGE ( 'NONE', *, *, #58795, .F. ) ;
#33449 = DIRECTION ( 'NONE',  ( -1.427937372958396981E-15, 1.000000000000000000, -1.053567635648657358E-14 ) ) ;
#33450 = ORIENTED_EDGE ( 'NONE', *, *, #20949, .T. ) ;
#33451 = CARTESIAN_POINT ( 'NONE',  ( -96.15314808468751551, 88.00268892867056536, 75.30239583420048177 ) ) ;
#33452 = CIRCLE ( 'NONE', #49079, 82.00000000000000000 ) ;
#33453 = CARTESIAN_POINT ( 'NONE',  ( -92.35000000000395914, -210.0000045800647115, 76.42687486209126746 ) ) ;
#33454 = CIRCLE ( 'NONE', #53870, 42.00000000000000000 ) ;
#33455 = ORIENTED_EDGE ( 'NONE', *, *, #64686, .T. ) ;
#33456 = PLANE ( 'NONE',  #28128 ) ;
#33457 = DIRECTION ( 'NONE',  ( -1.000000000000000000, 0.000000000000000000, 0.000000000000000000 ) ) ;
#33458 = CIRCLE ( 'NONE', #39497, 12.49999999999999645 ) ;
#33459 = ORIENTED_EDGE ( 'NONE', *, *, #38002, .F. ) ;
#33460 = CARTESIAN_POINT ( 'NONE',  ( -10.00000000000000000, 0.000000000000000000, 0.000000000000000000 ) ) ;
#33461 = APPLICATION_CONTEXT ( 'automotive_design' ) ;
#33462 = EDGE_LOOP ( 'NONE', ( #7110, #6129, #39435, #1620 ) ) ;
#33463 = FACE_OUTER_BOUND ( 'NONE', #65980, .T. ) ;
#33464 = VERTEX_POINT ( 'NONE', #48077 ) ;
#33465 = VERTEX_POINT ( 'NONE', #36412 ) ;
#33466 = EDGE_LOOP ( 'NONE', ( #29368, #49493 ) ) ;
#33467 = CARTESIAN_POINT ( 'NONE',  ( -2.500000000000003997, -4.330127018922192761, -6.000000000000000000 ) ) ;
#33468 = ITEM_DEFINED_TRANSFORMATION ( 'NONE', 'NONE', #59209,  #43395 ) ;
#33469 = DIRECTION ( 'NONE',  ( 0.000000000000000000, 0.8660254037844432595, -0.4999999999999920064 ) ) ;
#33470 = ORIENTED_EDGE ( 'NONE', *, *, #1905, .T. ) ;
#33471 = ORIENTED_EDGE ( 'NONE', *, *, #875, .T. ) ;
#33472 = VERTEX_POINT ( 'NONE', #48439 ) ;
#33473 = CARTESIAN_POINT ( 'NONE',  ( 0.000000000000000000, 73.95703589264006439, -23.16143007188350822 ) ) ;
#33474 = DIRECTION ( 'NONE',  ( 0.000000000000000000, -0.7071067811865389130, -0.7071067811865561215 ) ) ;
#33476 = CARTESIAN_POINT ( 'NONE',  ( -97.65000000000001990, 88.47002178664754979, 89.41791666666667027 ) ) ;
#33475 = AXIS2_PLACEMENT_3D ( 'NONE', #50867, #23057, #45248 ) ;
#33477 = ADVANCED_FACE ( 'NONE', ( #19858 ), #7848, .T. ) ;
#33478 = VERTEX_POINT ( 'NONE', #15717 ) ;
#33479 = CARTESIAN_POINT ( 'NONE',  ( 10.00000000000000000, -35.92658777277517856, 10.74501242461269257 ) ) ;
#33480 = ORIENTED_EDGE ( 'NONE', *, *, #30110, .F. ) ;
#33481 = CARTESIAN_POINT ( 'NONE',  ( -96.15314808468745866, -211.9973110713294489, 85.30364583420046642 ) ) ;
#33482 = EDGE_LOOP ( 'NONE', ( #38936, #34522, #11666, #52927 ) ) ;
#33483 = CIRCLE ( 'NONE', #65926, 31.99999999999999289 ) ;
#33484 = DIRECTION ( 'NONE',  ( 0.000000000000000000, 0.000000000000000000, -1.000000000000000000 ) ) ;
#33485 = CARTESIAN_POINT ( 'NONE',  ( -10.00000000000000000, 0.000000000000000000, 0.000000000000000000 ) ) ;
#33486 = CARTESIAN_POINT ( 'NONE',  ( -92.69370383062498320, -208.6684592857803295, 80.48822916753380241 ) ) ;
#33487 = CIRCLE ( 'NONE', #41935, 31.99999999999999645 ) ;
#33488 = CIRCLE ( 'NONE', #9455, 31.99999999999999645 ) ;
#33489 = DIRECTION ( 'NONE',  ( 1.000000000000000000, -0.000000000000000000, -0.000000000000000000 ) ) ;
#33490 = CYLINDRICAL_SURFACE ( 'NONE', #31950, 31.99999999999997868 ) ;
#33491 = CARTESIAN_POINT ( 'NONE',  ( -97.64999999999990621, -211.5299782133524786, 79.25791666666667368 ) ) ;
#33492 = AXIS2_PLACEMENT_3D ( 'NONE', #39827, #39453, #22910 ) ;
#33493 = ORIENTED_EDGE ( 'NONE', *, *, #31324, .F. ) ;
#33494 = DIRECTION ( 'NONE',  ( 1.000000000000000000, -3.035766082959412415E-16, 0.000000000000000000 ) ) ;
#33495 = ADVANCED_FACE ( 'NONE', ( #72104 ), #26613, .F. ) ;
#33496 = DIRECTION ( 'NONE',  ( 0.000000000000000000, 0.9945218953682729568, 0.1045284632676578424 ) ) ;
#33497 = ADVANCED_FACE ( 'NONE', ( #66846 ), #64776, .T. ) ;
#33498 = CARTESIAN_POINT ( 'NONE',  ( 92.34999999999999432, 90.00000000000002842, 90.00000000000000000 ) ) ;
#33499 = CARTESIAN_POINT ( 'NONE',  ( -97.30629616937501680, 91.33154071421968467, 81.33489583420048064 ) ) ;
#33500 = CARTESIAN_POINT ( 'NONE',  ( -20.30386590532152979, -102.9045904027214959, 5.500000000000000000 ) ) ;
#33501 = CARTESIAN_POINT ( 'NONE',  ( 0.000000000000000000, 3.894527615419050903, -81.90746397400384637 ) ) ;
#33502 = EDGE_LOOP ( 'NONE', ( #59244, #11093, #11759, #51815 ) ) ;
#33503 = FACE_OUTER_BOUND ( 'NONE', #7881, .T. ) ;
#33504 = AXIS2_PLACEMENT_3D ( 'NONE', #46466, #29524, #12248 ) ;
#33505 = EDGE_CURVE ( 'NONE', #32793, #41146, #9479, .T. ) ;
#33506 = AXIS2_PLACEMENT_3D ( 'NONE', #56439, #83, #50777 ) ;
#33507 = DIRECTION ( 'NONE',  ( -1.000000000000000000, 0.000000000000000000, 0.000000000000000000 ) ) ;
#33509 = CYLINDRICAL_SURFACE ( 'NONE', #58644, 20.20000000000036522 ) ;
#33508 = VECTOR ( 'NONE', #32329, 1000.000000000000114 ) ;
#33510 = CIRCLE ( 'NONE', #15542, 31.99999999999999289 ) ;
#33511 = DIRECTION ( 'NONE',  ( 0.000000000000000000, 0.07845909572783797692, 0.9969173337331285190 ) ) ;
#33512 = DIRECTION ( 'NONE',  ( 1.000000000000000000, -0.000000000000000000, -0.000000000000000000 ) ) ;
#33513 = DIRECTION ( 'NONE',  ( 0.000000000000000000, 0.000000000000000000, 1.000000000000000000 ) ) ;
#33514 = CARTESIAN_POINT ( 'NONE',  ( -92.69370383062498320, -208.6684592857803011, 80.01197916753380923 ) ) ;
#33515 = CIRCLE ( 'NONE', #27511, 15.99999999999999822 ) ;
#33516 = CARTESIAN_POINT ( 'NONE',  ( 10.00000000000000000, -26.79245525562738095, 32.34446384429961796 ) ) ;
#33517 = VERTEX_POINT ( 'NONE', #61215 ) ;
#33518 = ADVANCED_FACE ( 'NONE', ( #32244 ), #55564, .T. ) ;
#33519 = LINE ( 'NONE', #27887, #20261 ) ;
#33520 = CARTESIAN_POINT ( 'NONE',  ( -96.32500000000001705, 92.29496732002878900, 88.62416666666665321 ) ) ;
#33521 = DIRECTION ( 'NONE',  ( 0.000000000000000000, -0.4539904997395350916, -0.8910065241883738940 ) ) ;
#33522 = EDGE_LOOP ( 'NONE', ( #20910, #59300, #60202, #54208 ) ) ;
#33523 = LINE ( 'NONE', #45202, #34157 ) ;
#33524 = DIRECTION ( 'NONE',  ( -1.000000000000000000, 0.000000000000000000, 0.000000000000000000 ) ) ;
#33525 = SHAPE_REPRESENTATION ( 'socket button head screw_iso_ISO 7380 - M5 x 20 - 20N', ( #43395 ), #56756 ) ;
#33526 = LINE ( 'NONE', #27523, #14389 ) ;
#33527 = ORIENTED_EDGE ( 'NONE', *, *, #57321, .F. ) ;
#33528 = EDGE_CURVE ( 'NONE', #6686, #1439, #33515, .T. ) ;
#33529 = CARTESIAN_POINT ( 'NONE',  ( -11.70000000000000107, 0.000000000000000000, 0.000000000000000000 ) ) ;
#33530 = EDGE_CURVE ( 'NONE', #43637, #66703, #61116, .T. ) ;
#33531 = CARTESIAN_POINT ( 'NONE',  ( -99.99999999999997158, -204.9999999999999716, -79.99999999999998579 ) ) ;
#33532 = ORIENTED_EDGE ( 'NONE', *, *, #12645, .T. ) ;
#33533 = VECTOR ( 'NONE', #74176, 1000.000000000000000 ) ;
#33534 = CARTESIAN_POINT ( 'NONE',  ( 95.00000000000000000, -212.6630814284392557, 88.53156250086716739 ) ) ;
#33535 = DIRECTION ( 'NONE',  ( 0.000000000000000000, 1.000000000000000000, 0.000000000000000000 ) ) ;
#33536 = EDGE_CURVE ( 'NONE', #11375, #47114, #70691, .T. ) ;
#33537 = VERTEX_POINT ( 'NONE', #39020 ) ;
#33538 = AXIS2_PLACEMENT_3D ( 'NONE', #10622, #67397, #33550 ) ;
#33539 = VECTOR ( 'NONE', #31488, 1000.000000000000000 ) ;
#33540 = DIRECTION ( 'NONE',  ( 0.000000000000000000, -0.9510565162951565288, 0.3090169943749382919 ) ) ;
#33541 = CIRCLE ( 'NONE', #23955, 37.49900000000001654 ) ;
#33542 = ORIENTED_EDGE ( 'NONE', *, *, #20041, .T. ) ;
#33543 = CARTESIAN_POINT ( 'NONE',  ( 10.00000000000000000, 27.74655509720778568, -77.16300072079631889 ) ) ;
#33544 = ORIENTED_EDGE ( 'NONE', *, *, #31825, .F. ) ;
#33545 = DIRECTION ( 'NONE',  ( 0.4279312458752976833, 0.9038112904824853189, -0.000000000000000000 ) ) ;
#33546 = VERTEX_POINT ( 'NONE', #55935 ) ;
#33547 = ORIENTED_EDGE ( 'NONE', *, *, #33959, .F. ) ;
#33548 = AXIS2_PLACEMENT_3D ( 'NONE', #12058, #44528, #5059 ) ;
#33549 = ORIENTED_EDGE ( 'NONE', *, *, #31120, .T. ) ;
#33550 = DIRECTION ( 'NONE',  ( 0.000000000000000000, 0.000000000000000000, 1.000000000000000000 ) ) ;
#33551 = ORIENTED_EDGE ( 'NONE', *, *, #64686, .F. ) ;
#33552 = ORIENTED_EDGE ( 'NONE', *, *, #43079, .T. ) ;
#33553 = CARTESIAN_POINT ( 'NONE',  ( 96.15314808468748708, 88.00268892867053694, 76.04322916753382344 ) ) ;
#33554 = CYLINDRICAL_SURFACE ( 'NONE', #66013, 32.00000000000000000 ) ;
#33555 = CARTESIAN_POINT ( 'NONE',  ( -114.1267819554185365, -82.91796067500661138, 5.500000000000000000 ) ) ;
#33556 = ORIENTED_EDGE ( 'NONE', *, *, #50505, .F. ) ;
#33558 = ORIENTED_EDGE ( 'NONE', *, *, #63614, .T. ) ;
#33557 = CIRCLE ( 'NONE', #32322, 1.000000000000000000 ) ;
#33559 = ORIENTED_EDGE ( 'NONE', *, *, #52728, .T. ) ;
#33560 = CARTESIAN_POINT ( 'NONE',  ( 92.69370383062498320, 88.66845928578037217, 88.42572916753380241 ) ) ;
#33561 = ORIENTED_EDGE ( 'NONE', *, *, #30371, .F. ) ;
#33562 = CARTESIAN_POINT ( 'NONE',  ( 92.69370383062501162, -209.9999999999999716, 85.19781250086714408 ) ) ;
#33563 = VECTOR ( 'NONE', #40802, 1000.000000000000000 ) ;
#33564 = AXIS2_PLACEMENT_3D ( 'NONE', #23163, #271, #16024 ) ;
#33565 = CARTESIAN_POINT ( 'NONE',  ( 8.499999999999992895, -72.99999999999998579, -205.0000000000000284 ) ) ;
#33566 = CARTESIAN_POINT ( 'NONE',  ( -23.49999999999740297, -119.9999999999996021, -65.00000000000061107 ) ) ;
#33567 = CARTESIAN_POINT ( 'NONE',  ( -97.64999999953592180, 89.99996903277666149, 77.38038495128051864 ) ) ;
#33568 = CYLINDRICAL_SURFACE ( 'NONE', #22097, 12.49999999999999645 ) ;
#33569 = DIRECTION ( 'NONE',  ( -1.000000000000000000, 0.000000000000000000, 0.000000000000000000 ) ) ;
#33570 = CARTESIAN_POINT ( 'NONE',  ( 10.00000000000000000, -16.65560815589439159, 38.55633173627004595 ) ) ;
#33571 = AXIS2_PLACEMENT_3D ( 'NONE', #39957, #62912, #27921 ) ;
#33572 = DIRECTION ( 'NONE',  ( 0.000000000000000000, 0.000000000000000000, -1.000000000000000000 ) ) ;
#33573 = VECTOR ( 'NONE', #55916, 1000.000000000000000 ) ;
#33574 = CARTESIAN_POINT ( 'NONE',  ( -96.15314808468745866, -211.9973110713294489, 88.47864583420047779 ) ) ;
#33575 = CARTESIAN_POINT ( 'NONE',  ( -97.30629616937501680, 90.00000000000004263, 84.72156250086715090 ) ) ;
#33576 = ORIENTED_EDGE ( 'NONE', *, *, #69522, .T. ) ;
#33578 = CARTESIAN_POINT ( 'NONE',  ( -92.69370383062502583, 91.33154071421968467, 85.56822916753380071 ) ) ;
#33577 = CARTESIAN_POINT ( 'NONE',  ( 97.30629616937498838, 90.00000000000002842, 88.05531250086713158 ) ) ;
#33579 = ORIENTED_EDGE ( 'NONE', *, *, #19170, .T. ) ;
#33580 = CARTESIAN_POINT ( 'NONE',  ( 10.00000000000000000, 12.42422080174639021, 35.38097989696516521 ) ) ;
#33581 = DIRECTION ( 'NONE',  ( 0.000000000000000000, 0.000000000000000000, 1.000000000000000000 ) ) ;
#33582 = CARTESIAN_POINT ( 'NONE',  ( 92.35000000000000853, -209.9999999999999716, 87.45999999999999375 ) ) ;
#33583 = FACE_OUTER_BOUND ( 'NONE', #18742, .T. ) ;
#33584 = DIRECTION ( 'NONE',  ( -1.000000000000000000, -0.000000000000000000, -0.000000000000000000 ) ) ;
#33585 = CARTESIAN_POINT ( 'NONE',  ( 92.35000000000000853, -209.9999999999999716, 82.37999999999999545 ) ) ;
#33586 = EDGE_CURVE ( 'NONE', #2804, #28446, #57524, .T. ) ;
#33587 = DIRECTION ( 'NONE',  ( 0.000000000000000000, 0.000000000000000000, 1.000000000000000000 ) ) ;
#33588 = CARTESIAN_POINT ( 'NONE',  ( 10.00000000000000000, 0.000000000000000000, 0.000000000000000000 ) ) ;
#33589 = LINE ( 'NONE', #184, #39485 ) ;
#33590 = EDGE_LOOP ( 'NONE', ( #20641, #1224, #66440, #72442 ) ) ;
#33591 = VERTEX_POINT ( 'NONE', #50284 ) ;
#33592 = ADVANCED_FACE ( 'NONE', ( #73214 ), #66484, .F. ) ;
#33593 = CARTESIAN_POINT ( 'NONE',  ( -93.67500000000003979, 92.29496732002878900, 81.53333333333333144 ) ) ;
#33594 = EDGE_CURVE ( 'NONE', #19615, #55850, #49446, .T. ) ;
#33595 = DIRECTION ( 'NONE',  ( -1.000000000000000000, 0.000000000000000000, 0.000000000000000000 ) ) ;
#33596 = DIRECTION ( 'NONE',  ( 1.000000000000000000, 1.427937372958405461E-15, 7.962523111839130290E-16 ) ) ;
#33597 = CARTESIAN_POINT ( 'NONE',  ( 12.00000000000000000, 20.85821328998741109, -10.92862929874522671 ) ) ;
#33598 = CARTESIAN_POINT ( 'NONE',  ( -97.64997259622870729, 91.52999403492728447, 79.86645724064027263 ) ) ;
#33599 = CARTESIAN_POINT ( 'NONE',  ( 0.000000000000000000, 0.000000000000000000, 42.00000000000001421 ) ) ;
#33600 = FACE_OUTER_BOUND ( 'NONE', #65943, .T. ) ;
#33601 = DIRECTION ( 'NONE',  ( -1.000000000000000000, -0.000000000000000000, 0.000000000000000000 ) ) ;
#33602 = AXIS2_PLACEMENT_3D ( 'NONE', #73906, #26650, #50983 ) ;
#33603 = EDGE_LOOP ( 'NONE', ( #72856, #16655, #66265, #12310, #20336, #42553 ) ) ;
#33604 = CARTESIAN_POINT ( 'NONE',  ( -92.69370383062502583, 88.66845928578038638, 79.74739583420047495 ) ) ;
#33605 = CIRCLE ( 'NONE', #57608, 31.99999999999999289 ) ;
#33606 = EDGE_CURVE ( 'NONE', #5670, #59848, #38274, .T. ) ;
#33608 = CARTESIAN_POINT ( 'NONE',  ( 2.117611129180199558, -93.54218975225703048, 5.500000000000000000 ) ) ;
#33607 = CIRCLE ( 'NONE', #26413, 42.00000000000000000 ) ;
#33609 = CARTESIAN_POINT ( 'NONE',  ( 95.00000000000000000, -209.9999999999999716, 90.00000000000000000 ) ) ;
#33610 = CARTESIAN_POINT ( 'NONE',  ( 11.99999999999999822, 50.95692526931414790, -58.39081064771693974 ) ) ;
#33611 = CARTESIAN_POINT ( 'NONE',  ( 0.000000000000000000, 0.000000000000000000, 0.000000000000000000 ) ) ;
#33612 = VECTOR ( 'NONE', #37567, 1000.000000000000000 ) ;
#33613 = CARTESIAN_POINT ( 'NONE',  ( -92.35000000000005116, 91.52997821335254969, 82.11541666666664696 ) ) ;
#33614 = DIRECTION ( 'NONE',  ( 0.000000000000000000, 0.2079116908177555123, -0.9781476007338064660 ) ) ;
#33615 =( LENGTH_UNIT ( ) NAMED_UNIT ( * ) SI_UNIT ( .MILLI., .METRE. ) );
#33616 = EDGE_CURVE ( 'NONE', #3606, #16264, #34711, .T. ) ;
#33617 = EDGE_CURVE ( 'NONE', #68833, #68809, #23930, .T. ) ;
#33618 = AXIS2_PLACEMENT_3D ( 'NONE', #40110, #16060, #28075 ) ;
#33619 = CARTESIAN_POINT ( 'NONE',  ( 97.30629616937498838, 91.33154071421968467, 80.01197916753382344 ) ) ;
#33620 = CARTESIAN_POINT ( 'NONE',  ( -93.84685191531247028, -211.9973110713294489, 79.21822916753382060 ) ) ;
#33621 = FACE_OUTER_BOUND ( 'NONE', #60494, .T. ) ;
#33622 = VERTEX_POINT ( 'NONE', #22099 ) ;
#33623 = CARTESIAN_POINT ( 'NONE',  ( -96.32500000000001705, 87.70503267997129626, 87.01020833506763097 ) ) ;
#33624 = CARTESIAN_POINT ( 'NONE',  ( 11.99999999999999822, 0.000000000000000000, 0.000000000000000000 ) ) ;
#33625 = CARTESIAN_POINT ( 'NONE',  ( 23.41451323550360186, -132.5004227906269989, 2.500000000000000000 ) ) ;
#33626 = VECTOR ( 'NONE', #28524, 1000.000000000000000 ) ;
#33627 = AXIS2_PLACEMENT_3D ( 'NONE', #17035, #17764, #11024 ) ;
#33628 = AXIS2_PLACEMENT_3D ( 'NONE', #12511, #41461, #12873 ) ;
#33629 = AXIS2_PLACEMENT_3D ( 'NONE', #37280, #26351, #37646 ) ;
#33630 = TOROIDAL_SURFACE ( 'NONE', #37244, 57.50000000000000000, 5.000000000000000000 ) ;
#33631 = CARTESIAN_POINT ( 'NONE',  ( -95.00000000000002842, 87.33691857156074434, 78.53031250086715431 ) ) ;
#33632 = CARTESIAN_POINT ( 'NONE',  ( 93.84685191531249870, -208.0026889286704943, 79.37697916753380412 ) ) ;
#33633 = ORIENTED_EDGE ( 'NONE', *, *, #32642, .F. ) ;
#33634 = EDGE_CURVE ( 'NONE', #808, #10842, #53930, .T. ) ;
#33635 = EDGE_CURVE ( 'NONE', #24993, #62465, #67217, .T. ) ;
#33636 = CARTESIAN_POINT ( 'NONE',  ( 12.69589495141918611, -96.69089767102708777, 5.500000000000000000 ) ) ;
#33637 = VERTEX_POINT ( 'NONE', #29476 ) ;
#33638 =( BOUNDED_CURVE ( )  B_SPLINE_CURVE ( 2, ( #31298, #21781, #54252, #48600, #71513, #8750, #37331 ),
 .UNSPECIFIED., .F., .F. ) 
 B_SPLINE_CURVE_WITH_KNOTS ( ( 3, 2, 2, 3 ),
 ( 0.3333333333333333703, 0.3402777777777777901, 0.3472222222222221544, 0.3541666666666665741 ),
 .UNSPECIFIED. ) 
 CURVE ( )  GEOMETRIC_REPRESENTATION_ITEM ( )  RATIONAL_B_SPLINE_CURVE ( ( 0.9999999999999988898, 0.8660254037844398178, 1.000000000000000000, 0.8660254037844387076, 1.000000000000000000, 0.8660254037844408170, 0.9999999999999978906 ) ) 
 REPRESENTATION_ITEM ( '' )  );
#33639 = CARTESIAN_POINT ( 'NONE',  ( -97.64999999998384794, -210.0000060634594661, 88.17456390440159453 ) ) ;
#33640 = ORIENTED_EDGE ( 'NONE', *, *, #33768, .F. ) ;
#33641 = LINE ( 'NONE', #38918, #2227 ) ;
#33642 = ORIENTED_EDGE ( 'NONE', *, *, #47066, .T. ) ;
#33643 = ORIENTED_EDGE ( 'NONE', *, *, #41769, .T. ) ;
#33644 = ORIENTED_EDGE ( 'NONE', *, *, #10890, .F. ) ;
#33645 = CARTESIAN_POINT ( 'NONE',  ( 92.69370383062501162, -209.9999999999999716, 75.19656250086714522 ) ) ;
#33646 = VERTEX_POINT ( 'NONE', #58814 ) ;
#33647 = CARTESIAN_POINT ( 'NONE',  ( 0.000000000000000000, 0.000000000000000000, 0.000000000000000000 ) ) ;
#33648 = DIRECTION ( 'NONE',  ( -1.000000000000000000, 0.000000000000000000, 0.000000000000000000 ) ) ;
#33649 = CARTESIAN_POINT ( 'NONE',  ( 93.84685191531248449, 91.99731107132950569, 85.25072916753381946 ) ) ;
#33650 = CARTESIAN_POINT ( 'NONE',  ( 10.00000000000000000, 27.75498641678786527, -31.52238457039571173 ) ) ;
#33651 = CARTESIAN_POINT ( 'NONE',  ( 97.64999999999997726, -208.4700217866474645, 76.40041666666667197 ) ) ;
#33652 = ORIENTED_EDGE ( 'NONE', *, *, #9173, .T. ) ;
#33653 = ORIENTED_EDGE ( 'NONE', *, *, #66562, .T. ) ;
#33654 = CIRCLE ( 'NONE', #63725, 31.99999999999998224 ) ;
#33655 = VERTEX_POINT ( 'NONE', #7310 ) ;
#33656 = ORIENTED_EDGE ( 'NONE', *, *, #5009, .T. ) ;
#33657 = DIRECTION ( 'NONE',  ( -1.427937372958396784E-15, 1.000000000000000000, -1.078060571631604545E-14 ) ) ;
#33658 = AXIS2_PLACEMENT_3D ( 'NONE', #36290, #19369, #18991 ) ;
#33659 =( LENGTH_UNIT ( ) NAMED_UNIT ( * ) SI_UNIT ( .MILLI., .METRE. ) );
#33660 = DIRECTION ( 'NONE',  ( -1.000000000000000000, 0.000000000000000000, -0.000000000000000000 ) ) ;
#33661 = DIRECTION ( 'NONE',  ( 1.000000000000000000, 0.000000000000000000, 0.000000000000000000 ) ) ;
#33662 = AXIS2_PLACEMENT_3D ( 'NONE', #27373, #50308, #44698 ) ;
#33663 = DIRECTION ( 'NONE',  ( -1.000000000000000000, 0.000000000000000000, 0.000000000000000000 ) ) ;
#33664 = CARTESIAN_POINT ( 'NONE',  ( 92.35004149907317128, 88.46999782714644311, 83.78229332575389776 ) ) ;
#33665 = ORIENTED_EDGE ( 'NONE', *, *, #66280, .T. ) ;
#33666 = CARTESIAN_POINT ( 'NONE',  ( -97.64999999999994884, -211.5299782133524502, 83.14729166840096752 ) ) ;
#33667 = EDGE_LOOP ( 'NONE', ( #52698, #7030, #47339, #70148 ) ) ;
#33668 = CARTESIAN_POINT ( 'NONE',  ( 0.000000000000000000, -2.663952781845850826, -41.91543099594819921 ) ) ;
#33669 = EDGE_LOOP ( 'NONE', ( #69747, #44109, #39951, #70991 ) ) ;
#33671 = CARTESIAN_POINT ( 'NONE',  ( -92.35000000000005116, 88.47002178664754979, 80.18395833506764347 ) ) ;
#33670 = CARTESIAN_POINT ( 'NONE',  ( 92.34999999999999432, 90.00000000000002842, 83.72937500173429726 ) ) ;
#33672 = EDGE_LOOP ( 'NONE', ( #67761, #11713, #51694, #67863 ) ) ;
#33673 = CARTESIAN_POINT ( 'NONE',  ( 92.69370383062498320, 88.66845928578037217, 82.86947916753382515 ) ) ;
#33674 = CARTESIAN_POINT ( 'NONE',  ( 94.99999999999998579, 93.05995642670504253, 83.49125000000000796 ) ) ;
#33675 = CARTESIAN_POINT ( 'NONE',  ( 10.00000000000000000, -0.8828120875903202602, 37.48860685352291000 ) ) ;
#33676 = EDGE_CURVE ( 'NONE', #42185, #7680, #18939, .T. ) ;
#33677 = CARTESIAN_POINT ( 'NONE',  ( 11.99999999999999822, 0.000000000000000000, 0.000000000000000000 ) ) ;
#33678 = VECTOR ( 'NONE', #72969, 1000.000000000000000 ) ;
#33679 = CYLINDRICAL_SURFACE ( 'NONE', #18602, 31.99999999999998579 ) ;
#33680 = CARTESIAN_POINT ( 'NONE',  ( 11.99999999999999822, 59.03961581697465277, -46.53671651293886669 ) ) ;
#33681 = ORIENTED_EDGE ( 'NONE', *, *, #22227, .T. ) ;
#33682 = CARTESIAN_POINT ( 'NONE',  ( 11.99999999999999822, -33.71516098798793593, 74.74816331893418919 ) ) ;
#33683 = DIRECTION ( 'NONE',  ( -1.000000000000000000, 0.000000000000000000, -0.000000000000000000 ) ) ;
#33684 = AXIS2_PLACEMENT_3D ( 'NONE', #49293, #50020, #43315 ) ;
#33685 = CARTESIAN_POINT ( 'NONE',  ( 0.000000000000000000, 16.45098606841173705, -33.79645857604496229 ) ) ;
#33686 = ORIENTED_EDGE ( 'NONE', *, *, #55487, .F. ) ;
#33687 = ADVANCED_FACE ( 'NONE', ( #51038 ), #6573, .F. ) ;
#33688 = ORIENTED_EDGE ( 'NONE', *, *, #47541, .T. ) ;
#33689 = EDGE_CURVE ( 'NONE', #44189, #13090, #47530, .T. ) ;
#33690 = AXIS2_PLACEMENT_3D ( 'NONE', #60647, #68024, #19645 ) ;
#33691 = ADVANCED_FACE ( 'NONE', ( #53171 ), #16457, .T. ) ;
#33692 = FACE_OUTER_BOUND ( 'NONE', #20903, .T. ) ;
#33693 = DIRECTION ( 'NONE',  ( 0.000000000000000000, 0.000000000000000000, 1.000000000000000000 ) ) ;
#33694 = CARTESIAN_POINT ( 'NONE',  ( -2.500000000000012879, -65.00000000000000000, -290.0000000000000568 ) ) ;
#33695 = CARTESIAN_POINT ( 'NONE',  ( -94.99999999999997158, -207.3369185715606307, 80.75281250086715090 ) ) ;
#33696 = ORIENTED_EDGE ( 'NONE', *, *, #64843, .T. ) ;
#33697 = CARTESIAN_POINT ( 'NONE',  ( -97.30629616937501680, 91.33154071421968467, 88.95489583420048518 ) ) ;
#33698 = VERTEX_POINT ( 'NONE', #1706 ) ;
#33699 = EDGE_CURVE ( 'NONE', #5557, #67207, #12568, .T. ) ;
#33700 = CARTESIAN_POINT ( 'NONE',  ( -97.64995975555112295, -211.5300014484957956, 77.43229327564779396 ) ) ;
#33701 = CARTESIAN_POINT ( 'NONE',  ( 96.32499999999998863, 87.70503267997126784, 82.03604166840096923 ) ) ;
#33702 = DIRECTION ( 'NONE',  ( 0.000000000000000000, 0.000000000000000000, 1.000000000000000000 ) ) ;
#33703 = FACE_OUTER_BOUND ( 'NONE', #3981, .T. ) ;
#33704 = DIRECTION ( 'NONE',  ( 0.6575728627325957421, -0.7533909544171993877, -1.230411769795008318E-16 ) ) ;
#33705 = DIRECTION ( 'NONE',  ( -1.000000000000000000, 0.000000000000000000, 0.000000000000000000 ) ) ;
#33706 = DIRECTION ( 'NONE',  ( 0.000000000000000000, 0.000000000000000000, 1.000000000000000000 ) ) ;
#33707 = DIRECTION ( 'NONE',  ( 0.000000000000000000, -0.5877852522924625900, -0.8090169943749551118 ) ) ;
#33708 = CYLINDRICAL_SURFACE ( 'NONE', #7625, 82.00000000000000000 ) ;
#33709 = DIRECTION ( 'NONE',  ( -1.000000000000000000, 0.000000000000000000, 0.000000000000000000 ) ) ;
#33710 = EDGE_CURVE ( 'NONE', #17023, #55763, #19134, .T. ) ;
#33711 = CARTESIAN_POINT ( 'NONE',  ( 10.00000000000000000, -75.54627589209955829, 17.28742895386058009 ) ) ;
#33712 = EDGE_CURVE ( 'NONE', #41677, #24219, #18702, .T. ) ;
#33713 = DIRECTION ( 'NONE',  ( -1.000000000000000000, -0.000000000000000000, 0.000000000000000000 ) ) ;
#33714 = EDGE_CURVE ( 'NONE', #30425, #20114, #39602, .T. ) ;
#33715 = DIRECTION ( 'NONE',  ( -0.000000000000000000, -0.000000000000000000, -1.000000000000000000 ) ) ;
#33716 = CARTESIAN_POINT ( 'NONE',  ( 10.00000000000000000, 0.000000000000000000, 0.000000000000000000 ) ) ;
#33717 = ORIENTED_EDGE ( 'NONE', *, *, #41968, .F. ) ;
#33718 = AXIS2_PLACEMENT_3D ( 'NONE', #53588, #13726, #6266 ) ;
#33719 = CARTESIAN_POINT ( 'NONE',  ( 6.250000000000005329, 0.000000000000000000, 0.000000000000000000 ) ) ;
#33720 = CARTESIAN_POINT ( 'NONE',  ( -95.00000000000002842, 92.66308142843932671, 80.59406250086715318 ) ) ;
#33721 = AXIS2_PLACEMENT_3D ( 'NONE', #32113, #59595, #48307 ) ;
#33722 = ADVANCED_FACE ( 'NONE', ( #36240 ), #41153, .T. ) ;
#33723 = EDGE_CURVE ( 'NONE', #63727, #50408, #35505, .T. ) ;
#33724 = CARTESIAN_POINT ( 'NONE',  ( 93.84685191531249870, -208.0026889286704943, 88.90197916753380980 ) ) ;
#33725 = EDGE_CURVE ( 'NONE', #5745, #21153, #29847, .T. ) ;
#33726 = VERTEX_POINT ( 'NONE', #47164 ) ;
#33727 = CARTESIAN_POINT ( 'NONE',  ( 12.00000000000000000, -13.04903810567646971, 19.60159698893442126 ) ) ;
#33728 = CARTESIAN_POINT ( 'NONE',  ( -94.99999999999997158, -209.9999999999999716, 90.00000000000000000 ) ) ;
#33729 = DIRECTION ( 'NONE',  ( 0.000000000000000000, 0.000000000000000000, 1.000000000000000000 ) ) ;
#33730 = VECTOR ( 'NONE', #30083, 1000.000000000000000 ) ;
#33731 = EDGE_CURVE ( 'NONE', #39126, #14221, #70072, .T. ) ;
#33732 = AXIS2_PLACEMENT_3D ( 'NONE', #36274, #20470, #25372 ) ;
#33733 = CARTESIAN_POINT ( 'NONE',  ( 3.429551818649054340, -146.3199197248623875, 5.500000000000000000 ) ) ;
#33734 = CARTESIAN_POINT ( 'NONE',  ( 95.00000000000000000, -207.3369185715606307, 76.30781250086715772 ) ) ;
#33735 = AXIS2_PLACEMENT_3D ( 'NONE', #41718, #22973, #51896 ) ;
#33736 = ORIENTED_EDGE ( 'NONE', *, *, #50560, .T. ) ;
#33737 = CIRCLE ( 'NONE', #31314, 31.99999999999999645 ) ;
#33738 = ORIENTED_EDGE ( 'NONE', *, *, #9367, .F. ) ;
#33739 = CARTESIAN_POINT ( 'NONE',  ( 97.06449789201064959, -208.9360650323630182, 74.79348190356853365 ) ) ;
#33740 = LINE ( 'NONE', #61947, #14717 ) ;
#33741 = CARTESIAN_POINT ( 'NONE',  ( 10.00000000000000000, 58.39081064771823293, -50.95692526931266286 ) ) ;
#33742 = DIRECTION ( 'NONE',  ( 1.000000000000000000, 0.000000000000000000, 0.000000000000000000 ) ) ;
#33743 = DIRECTION ( 'NONE',  ( 0.000000000000000000, 0.6691306063588661202, 0.7431448254773871387 ) ) ;
#33744 = CARTESIAN_POINT ( 'NONE',  ( 92.35000000000000853, -209.9999999999999716, 87.45999999999999375 ) ) ;
#33745 = EDGE_LOOP ( 'NONE', ( #27680, #597, #38171, #72552 ) ) ;
#33746 = DIRECTION ( 'NONE',  ( -0.000000000000000000, -0.000000000000000000, -1.000000000000000000 ) ) ;
#33747 = ORIENTED_EDGE ( 'NONE', *, *, #38622, .T. ) ;
#33748 = ORIENTED_EDGE ( 'NONE', *, *, #20394, .T. ) ;
#33749 = DIRECTION ( 'NONE',  ( -1.000000000000000000, 0.000000000000000000, -0.000000000000000000 ) ) ;
#33750 = DIRECTION ( 'NONE',  ( -1.000000000000000000, -0.000000000000000000, -0.000000000000000000 ) ) ;
#33751 = ORIENTED_EDGE ( 'NONE', *, *, #32514, .F. ) ;
#33752 = DIRECTION ( 'NONE',  ( 0.000000000000000000, 0.000000000000000000, 1.000000000000000000 ) ) ;
#33753 = CARTESIAN_POINT ( 'NONE',  ( 97.64999999999999147, -209.9999999999999716, 75.15687500173430635 ) ) ;
#33754 = CARTESIAN_POINT ( 'NONE',  ( 97.64999999999997726, 88.47002178664753558, 80.73958333333332860 ) ) ;
#33755 = EDGE_LOOP ( 'NONE', ( #68509, #18931 ) ) ;
#33756 = CARTESIAN_POINT ( 'NONE',  ( 10.00000000000000000, -72.35160999960801576, -20.41045688087902121 ) ) ;
#33757 = ORIENTED_EDGE ( 'NONE', *, *, #35070, .T. ) ;
#33758 = PLANE ( 'NONE',  #43470 ) ;
#33759 = ORIENTED_EDGE ( 'NONE', *, *, #37035, .T. ) ;
#33760 = FACE_OUTER_BOUND ( 'NONE', #30940, .T. ) ;
#33761 = CARTESIAN_POINT ( 'NONE',  ( -92.69370383062504004, 90.00000000000004263, 83.13406250086715943 ) ) ;
#33762 = CARTESIAN_POINT ( 'NONE',  ( 92.69370383062498320, 88.66845928578037217, 77.63072916753380071 ) ) ;
#33763 = ORIENTED_EDGE ( 'NONE', *, *, #54812, .F. ) ;
#33764 = DIRECTION ( 'NONE',  ( 0.000000000000000000, 0.9238795325112851842, 0.3826834323650937786 ) ) ;
#33765 = DIRECTION ( 'NONE',  ( -1.000000000000000000, 0.000000000000000000, -0.000000000000000000 ) ) ;
#33766 = CARTESIAN_POINT ( 'NONE',  ( 11.99999999999999822, -24.73286445877655382, -73.44644590900085745 ) ) ;
#33767 = VECTOR ( 'NONE', #50212, 1000.000000000000000 ) ;
#33768 = EDGE_CURVE ( 'NONE', #62654, #57250, #64455, .T. ) ;
#33769 = CARTESIAN_POINT ( 'NONE',  ( -23.30023580412278505, -123.4057321492263384, 5.500000000000000000 ) ) ;
#33770 = VERTEX_POINT ( 'NONE', #70433 ) ;
#33771 = DIRECTION ( 'NONE',  ( -1.000000000000000000, -0.000000000000000000, -0.000000000000000000 ) ) ;
#33772 = AXIS2_PLACEMENT_3D ( 'NONE', #52561, #2591, #65338 ) ;
#33773 = CARTESIAN_POINT ( 'NONE',  ( -94.99999999999997158, -212.6630814284392557, 79.00656250086713328 ) ) ;
#33774 = VERTEX_POINT ( 'NONE', #7673 ) ;
#33775 = EDGE_CURVE ( 'NONE', #67569, #44773, #5773, .T. ) ;
#33776 = AXIS2_PLACEMENT_3D ( 'NONE', #63680, #35455, #30179 ) ;
#33777 = ORIENTED_EDGE ( 'NONE', *, *, #81, .T. ) ;
#33778 = CARTESIAN_POINT ( 'NONE',  ( 100.0010000000000190, -123.9999999999999858, -40.00000000000002132 ) ) ;
#33779 = ADVANCED_FACE ( 'NONE', ( #55008 ), #36608, .F. ) ;
#33780 = ADVANCED_FACE ( 'NONE', ( #54287, #9148, #53910, #71177, #36981, #25341 ), #59556, .T. ) ;
#33781 = VECTOR ( 'NONE', #35250, 1000.000000000000227 ) ;
#33782 = ORIENTED_EDGE ( 'NONE', *, *, #69130, .T. ) ;
#33783 = CARTESIAN_POINT ( 'NONE',  ( 11.99999999999999822, -28.89263327155796190, 71.91182617369179297 ) ) ;
#33784 = ORIENTED_EDGE ( 'NONE', *, *, #48583, .T. ) ;
#33785 = CARTESIAN_POINT ( 'NONE',  ( -93.84685191531247028, -211.9973110713294489, 75.88447916753381151 ) ) ;
#33786 = ORIENTED_EDGE ( 'NONE', *, *, #30198, .T. ) ;
#33787 = CARTESIAN_POINT ( 'NONE',  ( -97.64999999996709334, -209.9999916080759306, 86.90410584369134028 ) ) ;
#33788 = DIRECTION ( 'NONE',  ( 0.000000000000000000, 0.2334453638558989796, 0.9723699203976782224 ) ) ;
#33789 = FACE_BOUND ( 'NONE', #39218, .T. ) ;
#33790 = CARTESIAN_POINT ( 'NONE',  ( 0.000000000000000000, -120.0000000000000000, 125.0000000000000000 ) ) ;
#33791 = LINE ( 'NONE', #16881, #63064 ) ;
#33792 = CIRCLE ( 'NONE', #20590, 2.375000000000000444 ) ;
#33793 = CIRCLE ( 'NONE', #66213, 42.00000000000000000 ) ;
#33794 = DIRECTION ( 'NONE',  ( 0.000000000000000000, 0.000000000000000000, 1.000000000000000000 ) ) ;
#33795 = CARTESIAN_POINT ( 'NONE',  ( 92.69370383062498320, 91.33154071421968467, 86.41489583420047893 ) ) ;
#33796 = FACE_OUTER_BOUND ( 'NONE', #19222, .T. ) ;
#33797 = AXIS2_PLACEMENT_3D ( 'NONE', #2519, #59243, #30288 ) ;
#33798 = DIRECTION ( 'NONE',  ( 0.9918136447140104561, -0.1276937514489679681, 0.000000000000000000 ) ) ;
#33799 = DIRECTION ( 'NONE',  ( 0.000000000000000000, 0.000000000000000000, 1.000000000000000000 ) ) ;
#33800 = DIRECTION ( 'NONE',  ( 0.000000000000000000, 0.000000000000000000, 1.000000000000000000 ) ) ;
#33801 = EDGE_CURVE ( 'NONE', #36080, #47197, #64822, .T. ) ;
#33802 = LINE ( 'NONE', #72521, #12797 ) ;
#33803 = CYLINDRICAL_SURFACE ( 'NONE', #33492, 14.09999999999999964 ) ;
#33804 = LINE ( 'NONE', #44726, #63891 ) ;
#33805 = CARTESIAN_POINT ( 'NONE',  ( -8.826826895187510402, -94.96827758698185562, 5.500000000000000000 ) ) ;
#33806 = DIRECTION ( 'NONE',  ( -1.000000000000000000, 0.000000000000000000, 0.000000000000000000 ) ) ;
#33807 = CARTESIAN_POINT ( 'NONE',  ( 0.000000000000000000, -27.74655509720617985, -77.16300072079690153 ) ) ;
#33808 = DIRECTION ( 'NONE',  ( -1.000000000000000000, -0.000000000000000000, -0.000000000000000000 ) ) ;
#33809 = EDGE_CURVE ( 'NONE', #37625, #34470, #20053, .T. ) ;
#33810 = ADVANCED_FACE ( 'NONE', ( #20799 ), #72301, .T. ) ;
#33811 = CARTESIAN_POINT ( 'NONE',  ( 10.00000000000000000, 0.000000000000000000, 0.000000000000000000 ) ) ;
#33812 = CARTESIAN_POINT ( 'NONE',  ( -97.64999999999996305, -209.9999999999999716, 86.18999999999999773 ) ) ;
#33813 = CARTESIAN_POINT ( 'NONE',  ( -92.35000000000003695, 90.00000000000004263, 80.15749999999999886 ) ) ;
#33814 = PRODUCT_DEFINITION_SHAPE ( 'NONE', 'NONE',  #66939 ) ;
#33815 = DIRECTION ( 'NONE',  ( -1.000000000000000000, -0.000000000000000000, -0.000000000000000000 ) ) ;
#33816 = LINE ( 'NONE', #51106, #51480 ) ;
#33817 = CARTESIAN_POINT ( 'NONE',  ( 11.99999999999999822, -23.16143007188376757, -73.95703589263997912 ) ) ;
#33818 = PRESENTATION_LAYER_ASSIGNMENT (  '', '', ( #66249 ) ) ;
#33819 = AXIS2_PLACEMENT_3D ( 'NONE', #39981, #58370, #24171 ) ;
#33820 = CARTESIAN_POINT ( 'NONE',  ( 97.30629616937498838, -208.6684592857803011, 85.72697916753381264 ) ) ;
#33821 = VECTOR ( 'NONE', #2308, 1000.000000000000000 ) ;
#33822 = ORIENTED_EDGE ( 'NONE', *, *, #61102, .F. ) ;
#33823 = ORIENTED_EDGE ( 'NONE', *, *, #37301, .T. ) ;
#33824 = CIRCLE ( 'NONE', #42221, 13.90444123027096879 ) ;
#33825 = DIRECTION ( 'NONE',  ( -0.000000000000000000, -0.000000000000000000, 1.000000000000000000 ) ) ;
#33826 = ORIENTED_EDGE ( 'NONE', *, *, #20644, .T. ) ;
#33827 = CARTESIAN_POINT ( 'NONE',  ( 11.99999999999999822, 64.81221759200343513, 50.23322058963371006 ) ) ;
#33828 = AXIS2_PLACEMENT_3D ( 'NONE', #71651, #61133, #14134 ) ;
#33829 = CARTESIAN_POINT ( 'NONE',  ( 92.69370383062501162, -209.9999999999999716, 76.94281250086713442 ) ) ;
#33830 = ORIENTED_EDGE ( 'NONE', *, *, #33420, .T. ) ;
#33831 = CARTESIAN_POINT ( 'NONE',  ( 95.00000000000000000, -212.6630814284392557, 82.97531250086716170 ) ) ;
#33832 = VERTEX_POINT ( 'NONE', #48267 ) ;
#33833 = CARTESIAN_POINT ( 'NONE',  ( 10.00000000000000000, 0.000000000000000000, 0.000000000000000000 ) ) ;
#33834 = ORIENTED_EDGE ( 'NONE', *, *, #11797, .F. ) ;
#33835 = CIRCLE ( 'NONE', #44648, 31.99999999999998224 ) ;
#33836 = ORIENTED_EDGE ( 'NONE', *, *, #6771, .F. ) ;
#33837 = DIRECTION ( 'NONE',  ( 0.000000000000000000, 0.6691306063588569053, -0.7431448254773954654 ) ) ;
#33838 = CIRCLE ( 'NONE', #50634, 31.99999999999998934 ) ;
#33839 = CARTESIAN_POINT ( 'NONE',  ( 15.00000000000000000, -23.29833615347104470, 3.418703333116808629 ) ) ;
#33840 = CIRCLE ( 'NONE', #67443, 82.00000000000000000 ) ;
#33841 = ORIENTED_EDGE ( 'NONE', *, *, #40556, .F. ) ;
#33842 = CARTESIAN_POINT ( 'NONE',  ( 92.35000000000000853, -209.9999999999999716, 76.74437500173429783 ) ) ;
#33843 = CARTESIAN_POINT ( 'NONE',  ( 95.00000000000000000, -213.0599564267049857, 88.33312500173428816 ) ) ;
#33844 = VERTEX_POINT ( 'NONE', #32445 ) ;
#33845 = DIRECTION ( 'NONE',  ( -1.000000000000000000, 0.000000000000000000, 0.000000000000000000 ) ) ;
#33846 = ORIENTED_EDGE ( 'NONE', *, *, #59736, .F. ) ;
#33847 =( BOUNDED_CURVE ( )  B_SPLINE_CURVE ( 2, ( #8193, #36391, #60097, #12720, #42786, #1497, #31122 ),
 .UNSPECIFIED., .F., .F. ) 
 B_SPLINE_CURVE_WITH_KNOTS ( ( 3, 2, 2, 3 ),
 ( 0.4166666666666662966, 0.4236111111111106609, 0.4305555555555550806, 0.4374999999999994449 ),
 .UNSPECIFIED. ) 
 CURVE ( )  GEOMETRIC_REPRESENTATION_ITEM ( )  RATIONAL_B_SPLINE_CURVE ( ( 1.000000000000007550, 0.8660254037844311581, 1.000000000000000000, 0.8660254037844387076, 1.000000000000000000, 0.8660254037844493658, 0.9999999999999893419 ) ) 
 REPRESENTATION_ITEM ( '' )  );
#33848 = DIRECTION ( 'NONE',  ( 0.000000000000000000, 0.000000000000000000, 1.000000000000000000 ) ) ;
#33849 = ORIENTED_EDGE ( 'NONE', *, *, #67572, .F. ) ;
#33850 = ADVANCED_FACE ( 'NONE', ( #14422 ), #70761, .T. ) ;
#33851 = VERTEX_POINT ( 'NONE', #26442 ) ;
#33852 = ORIENTED_EDGE ( 'NONE', *, *, #47517, .T. ) ;
#33853 = CARTESIAN_POINT ( 'NONE',  ( 96.15314808468750130, -211.9973110713294489, 75.24947916753380639 ) ) ;
#33854 = LINE ( 'NONE', #6411, #17412 ) ;
#33855 = VERTEX_POINT ( 'NONE', #3539 ) ;
#33856 = EDGE_LOOP ( 'NONE', ( #51227, #54829, #59877, #1881 ) ) ;
#33857 = EDGE_CURVE ( 'NONE', #16927, #50966, #28743, .T. ) ;
#33858 = ORIENTED_EDGE ( 'NONE', *, *, #14842, .T. ) ;
#33859 = CARTESIAN_POINT ( 'NONE',  ( 96.32499999999997442, 92.29496732002878900, 79.70770833506762187 ) ) ;
#33860 = LINE ( 'NONE', #15834, #46699 ) ;
#33861 = EDGE_CURVE ( 'NONE', #45442, #11526, #42631, .T. ) ;
#33862 = CARTESIAN_POINT ( 'NONE',  ( -97.30629616937501680, 90.00000000000004263, 76.46656250086715545 ) ) ;
#33863 = ORIENTED_EDGE ( 'NONE', *, *, #22866, .T. ) ;
#33864 = CARTESIAN_POINT ( 'NONE',  ( 93.84685191531248449, 91.99731107132950569, 74.93197916753379673 ) ) ;
#33865 = VECTOR ( 'NONE', #11166, 999.9999999999998863 ) ;
#33866 = ORIENTED_EDGE ( 'NONE', *, *, #21202, .T. ) ;
#33867 =( BOUNDED_SURFACE ( )  B_SPLINE_SURFACE ( 1, 2, ( 
 ( #34497, #344, #51052, #57440, #16856, #29579, #28865, #46907, #18318, #46526, #11204, #5216, #63832, #69095, #40896, #17583, #45432, #12305, #40515, #63459, #11934, #1077, #69452, #68361, #703, #23973, #23596, #71662, #43121, #48738, #54385, #36715, #66052, #58539, #70541, #20160, #7420, #35605, #29961, #7034, #54025, #1451, #2563, #19052, #14149, #30333, #52912, #24337, #25443, #47273, #2184, #42736, #59663, #18679, #53277, #42371, #47634, #8145, #65672, #1814, #53645, #70176, #24700, #31070, #36347, #42004, #48371, #13037, #13779, #64941, #41621, #71284, #37098, #48009, #13416, #64559, #19422, #19789, #60049, #25069, #2917, #8532, #31444, #35976, #25808, #59289, #58928, #7782, #30698, #70922, #65310, #44221, #27664, #21261, #26547, #54753, #31808, #4012, #55498, #15648, #38581, #14900, #32551, #60410, #66419, #49107, #38953, #66774, #4758, #50589, #4380, #72034, #73516, #21648, #55119, #73142, #72404, #22023, #44602, #20909, #67144, #43859, #67519, #27278, #37479, #61513, #56243, #16007, #44968, #14526, #8891, #33289, #9996, #3282, #26171, #49479, #20546, #60774, #43500, #37843, #9256, #32916, #32176, #55868, #15269, #61889, #3646, #38201, #61144, #50208, #9633, #26914, #10369, #49844, #72760, #62642, #261, #5498, #17496, #618, #11118, #11481, #23884, #39703, #40425, #68647, #34042, #11839, #45345, #46075, #28394, #73889, #10747, #51330, #28773, #33671, #34409, #39326, #35158, #6237, #63373, #46440, #52436, #17129, #34790, #69010, #16765, #74266, #57731, #23152, #29137, #22398, #52073, #23509, #56626, #68269, #5125, #56993, #22783, #58094, #29500, #69368, #28026, #990, #17864, #45725, #40810, #40061, #6596, #63745, #63022, #12221, #57352, #67894, #16384, #62262, #50968, #5864, #51713, #8444, #54307, #59959, #65589, #47916, #2832, #69735, #7334, #31355, #18597, #46820, #41176, #18235, #65221, #12593, #13692, #30250, #25362, #41537, #64112, #35524, #36629, #58451, #13329, #53937, #70835, #29873, #64474, #53557, #58834, #19336, #2475, #12949, #64850, #6949, #35886, #42292, #47550, #53189, #59574, #24258, #24981, #1725, #52825, #1367, #24613, #7692, #47182, #36263, #70094, #14056, #8060, #30981, #48289, #70454, #18961, #71197, #19703, #41910, #59201, #42651, #2094, #37006, #30609, #55406, #26825 ),
 ( #61430, #67429, #32830, #49751, #73048, #9909, #43415, #66337, #43027, #14810, #25721, #21176, #8806, #38858, #3196, #37757, #26086, #71575, #20072, #60691, #10282, #60328, #37394, #9170, #38491, #61801, #50113, #65968, #61051, #33204, #56148, #48660, #3562, #14440, #49016, #54668, #55779, #31723, #32093, #3929, #72674, #26460, #71947, #20461, #67051, #38112, #55033, #9548, #44127, #15558, #49396, #4297, #72322, #27185, #20821, #43773, #66692, #15178, #32464, #21554, #44512, #15925, #56535, #5772, #63287, #51620, #17042, #68920, #28679, #27943, #50873, #73430, #73796, #4667, #34325, #39236, #34693, #33578, #45254, #5038, #50502, #21937, #22310, #29053, #62166, #16296, #68171, #172, #57647, #17406, #44880, #74174, #27574, #67802, #10652, #23063, #62551, #45992, #45637, #16671, #39609, #51242, #11032, #33956, #68555, #40341, #56905, #6147, #5411, #28306, #22689, #39978, #62933, #11746, #11391, #57267, #39262, #55433, #44534, #50529, #32856, #62191, #54693, #66717, #16322, #3586, #67828, #26108, #31749, #50141, #71970, #73076, #15203, #10310, #26487, #3219, #49043, #21581, #20484, #72696, #38887, #55806, #14832, #49419, #38513, #43799, #4322, #61825, #72346, #49778, #43440, #20845, #27208, #32488, #38139, #67454, #9196, #9935, #61075, #37784, #66357, #21200, #15946, #33226, #32116, #44154, #60716, #55056, #9568, #56173, #3951, #21959, #26853, #4694, #67080, #15580, #27600, #61453, #73454, #44907, #23812, #69305, #17070, #17435, #40002, #63685, #555, #33604, #11770, #52377, #33981, #18172, #34348, #23450, #29432, #34724, #41115, #56563, #45658, #69674, #56930, #46754, #5066, #10678, #29075, #50899, #52003, #68581, #12152, #5434, #27964, #73823, #46379, #22337, #51647, #17792, #57668, #68201, #28329, #40364, #22719, #6173, #40742, #51267, #28708, #45280, #74202, #35098, #11415, #62961, #58025, #62578, #63310, #57288, #16698, #39633, #5802, #46016, #11060, #194, #23088, #925, #6531, #68947, #42586, #48596, #13268, #59512, #65161, #12887, #24552, #7998, #70772, #13632, #70029, #19274, #36562, #29806, #64414, #6889, #53127, #1667, #30916, #71137, #2032, #41840, #52761, #47847, #48227, #42230, #7629, #31291, #25298, #19639, #71507, #53860, #70391, #65524, #35818, #64788, #53496, #54245, #2408, #2773, #13995 ) ),
 .UNSPECIFIED., .F., .F., .F. ) 
 B_SPLINE_SURFACE_WITH_KNOTS ( ( 2, 2 ),
 ( 3, 2, 2, 2, 2, 2, 2, 2, 2, 2, 2, 2, 2, 2, 2, 2, 2, 2, 2, 2, 2, 2, 2, 2, 2, 2, 2, 2, 2, 2, 2, 2, 2, 2, 2, 2, 2, 2, 2, 2, 2, 2, 2, 2, 2, 2, 2, 2, 2, 2, 2, 2, 2, 2, 2, 2, 2, 2, 2, 2, 2, 2, 2, 2, 2, 2, 2, 2, 2, 2, 2, 2, 2, 2, 2, 2, 2, 2, 2, 2, 2, 2, 2, 2, 2, 2, 2, 2, 2, 2, 2, 2, 2, 2, 2, 2, 2, 2, 2, 2, 2, 2, 2, 2, 2, 2, 2, 2, 2, 2, 2, 2, 2, 2, 2, 2, 2, 2, 2, 2, 2, 2, 2, 2, 2, 2, 2, 2, 2, 2, 2, 2, 2, 2, 2, 2, 2, 2, 2, 2, 2, 2, 3 ),
 ( 0.000000000000000000, 1.000000000000000000 ),
 ( 0.000000000000000000, 0.006944444444444444059, 0.01388888888888888812, 0.02083333333333333218, 0.02777777777777777624, 0.03472222222222222376, 0.04166666666666666435, 0.04861111111111111188, 0.05555555555555555247, 0.06250000000000000000, 0.06944444444444444753, 0.07638888888888889506, 0.08333333333333332871, 0.09027777777777777624, 0.09722222222222222376, 0.1041666666666666713, 0.1111111111111111049, 0.1180555555555555525, 0.1250000000000000000, 0.1319444444444444475, 0.1388888888888888951, 0.1458333333333333426, 0.1527777777777777901, 0.1597222222222222099, 0.1666666666666666574, 0.1736111111111111049, 0.1805555555555555525, 0.1875000000000000000, 0.1944444444444444475, 0.2013888888888888951, 0.2083333333333333426, 0.2152777777777777901, 0.2222222222222222099, 0.2291666666666666574, 0.2361111111111111049, 0.2430555555555555525, 0.2500000000000000000, 0.2569444444444444198, 0.2638888888888888951, 0.2708333333333333148, 0.2777777777777777901, 0.2847222222222222099, 0.2916666666666666852, 0.2986111111111111049, 0.3055555555555555802, 0.3125000000000000000, 0.3194444444444444198, 0.3263888888888888951, 0.3333333333333333148, 0.3402777777777777901, 0.3472222222222222099, 0.3541666666666666852, 0.3611111111111111049, 0.3680555555555555802, 0.3750000000000000000, 0.3819444444444444198, 0.3888888888888888951, 0.3958333333333333148, 0.4027777777777777901, 0.4097222222222222099, 0.4166666666666666852, 0.4236111111111111049, 0.4305555555555555802, 0.4375000000000000000, 0.4444444444444444198, 0.4513888888888888951, 0.4583333333333333148, 0.4652777777777777901, 0.4722222222222222099, 0.4791666666666666852, 0.4861111111111111049, 0.4930555555555555802, 0.5000000000000000000, 0.5069444444444444198, 0.5138888888888888395, 0.5208333333333333703, 0.5277777777777777901, 0.5347222222222222099, 0.5416666666666666297, 0.5486111111111111605, 0.5555555555555555802, 0.5625000000000000000, 0.5694444444444444198, 0.5763888888888888395, 0.5833333333333333703, 0.5902777777777777901, 0.5972222222222222099, 0.6041666666666666297, 0.6111111111111111605, 0.6180555555555555802, 0.6250000000000000000, 0.6319444444444444198, 0.6388888888888888395, 0.6458333333333333703, 0.6527777777777777901, 0.6597222222222222099, 0.6666666666666666297, 0.6736111111111111605, 0.6805555555555555802, 0.6875000000000000000, 0.6944444444444444198, 0.7013888888888888395, 0.7083333333333333703, 0.7152777777777777901, 0.7222222222222222099, 0.7291666666666666297, 0.7361111111111111605, 0.7430555555555555802, 0.7500000000000000000, 0.7569444444444444198, 0.7638888888888888395, 0.7708333333333333703, 0.7777777777777777901, 0.7847222222222222099, 0.7916666666666666297, 0.7986111111111111605, 0.8055555555555555802, 0.8125000000000000000, 0.8194444444444444198, 0.8263888888888888395, 0.8333333333333333703, 0.8402777777777777901, 0.8472222222222222099, 0.8541666666666666297, 0.8611111111111111605, 0.8680555555555555802, 0.8750000000000000000, 0.8819444444444444198, 0.8888888888888888395, 0.8958333333333333703, 0.9027777777777777901, 0.9097222222222222099, 0.9166666666666666297, 0.9236111111111111605, 0.9305555555555555802, 0.9375000000000000000, 0.9444444444444444198, 0.9513888888888888395, 0.9583333333333333703, 0.9652777777777777901, 0.9722222222222222099, 0.9791666666666666297, 0.9842226981114289286 ),
 .UNSPECIFIED. ) 
 GEOMETRIC_REPRESENTATION_ITEM ( )  RATIONAL_B_SPLINE_SURFACE ( (
 ( 1.000000000000000000, 0.8660254037844387076, 1.000000000000000000, 0.8660254037844387076, 1.000000000000000000, 0.8660254037844387076, 1.000000000000000000, 0.8660254037844387076, 1.000000000000000000, 0.8660254037844387076, 1.000000000000000000, 0.8660254037844387076, 1.000000000000000000, 0.8660254037844387076, 1.000000000000000000, 0.8660254037844387076, 1.000000000000000000, 0.8660254037844387076, 1.000000000000000000, 0.8660254037844387076, 1.000000000000000000, 0.8660254037844387076, 1.000000000000000000, 0.8660254037844387076, 1.000000000000000000, 0.8660254037844387076, 1.000000000000000000, 0.8660254037844387076, 1.000000000000000000, 0.8660254037844387076, 1.000000000000000000, 0.8660254037844387076, 1.000000000000000000, 0.8660254037844387076, 1.000000000000000000, 0.8660254037844387076, 1.000000000000000000, 0.8660254037844387076, 1.000000000000000000, 0.8660254037844387076, 1.000000000000000000, 0.8660254037844387076, 1.000000000000000000, 0.8660254037844387076, 1.000000000000000000, 0.8660254037844387076, 1.000000000000000000, 0.8660254037844387076, 1.000000000000000000, 0.8660254037844387076, 1.000000000000000000, 0.8660254037844387076, 1.000000000000000000, 0.8660254037844387076, 1.000000000000000000, 0.8660254037844387076, 1.000000000000000000, 0.8660254037844387076, 1.000000000000000000, 0.8660254037844387076, 1.000000000000000000, 0.8660254037844387076, 1.000000000000000000, 0.8660254037844387076, 1.000000000000000000, 0.8660254037844387076, 1.000000000000000000, 0.8660254037844387076, 1.000000000000000000, 0.8660254037844387076, 1.000000000000000000, 0.8660254037844387076, 1.000000000000000000, 0.8660254037844387076, 1.000000000000000000, 0.8660254037844387076, 1.000000000000000000, 0.8660254037844387076, 1.000000000000000000, 0.8660254037844387076, 1.000000000000000000, 0.8660254037844387076, 1.000000000000000000, 0.8660254037844387076, 1.000000000000000000, 0.8660254037844387076, 1.000000000000000000, 0.8660254037844387076, 1.000000000000000000, 0.8660254037844387076, 1.000000000000000000, 0.8660254037844387076, 1.000000000000000000, 0.8660254037844387076, 1.000000000000000000, 0.8660254037844387076, 1.000000000000000000, 0.8660254037844387076, 1.000000000000000000, 0.8660254037844387076, 1.000000000000000000, 0.8660254037844387076, 1.000000000000000000, 0.8660254037844387076, 1.000000000000000000, 0.8660254037844387076, 1.000000000000000000, 0.8660254037844387076, 1.000000000000000000, 0.8660254037844387076, 1.000000000000000000, 0.8660254037844387076, 1.000000000000000000, 0.8660254037844387076, 1.000000000000000000, 0.8660254037844387076, 1.000000000000000000, 0.8660254037844387076, 1.000000000000000000, 0.8660254037844387076, 1.000000000000000000, 0.8660254037844387076, 1.000000000000000000, 0.8660254037844387076, 1.000000000000000000, 0.8660254037844387076, 1.000000000000000000, 0.8660254037844387076, 1.000000000000000000, 0.8660254037844387076, 1.000000000000000000, 0.8660254037844387076, 1.000000000000000000, 0.8660254037844387076, 1.000000000000000000, 0.8660254037844387076, 1.000000000000000000, 0.8660254037844387076, 1.000000000000000000, 0.8660254037844387076, 1.000000000000000000, 0.8660254037844387076, 1.000000000000000000, 0.8660254037844387076, 1.000000000000000000, 0.8660254037844387076, 1.000000000000000000, 0.8660254037844387076, 1.000000000000000000, 0.8660254037844387076, 1.000000000000000000, 0.8660254037844387076, 1.000000000000000000, 0.8660254037844387076, 1.000000000000000000, 0.8660254037844387076, 1.000000000000000000, 0.8660254037844387076, 1.000000000000000000, 0.8660254037844387076, 1.000000000000000000, 0.8660254037844387076, 1.000000000000000000, 0.8660254037844387076, 1.000000000000000000, 0.8660254037844387076, 1.000000000000000000, 0.8660254037844387076, 1.000000000000000000, 0.8660254037844387076, 1.000000000000000000, 0.8660254037844387076, 1.000000000000000000, 0.8660254037844387076, 1.000000000000000000, 0.8660254037844387076, 1.000000000000000000, 0.8660254037844387076, 1.000000000000000000, 0.8660254037844387076, 1.000000000000000000, 0.8660254037844387076, 1.000000000000000000, 0.8660254037844387076, 1.000000000000000000, 0.8660254037844387076, 1.000000000000000000, 0.8660254037844387076, 1.000000000000000000, 0.8660254037844387076, 1.000000000000000000, 0.8660254037844387076, 1.000000000000000000, 0.8660254037844387076, 1.000000000000000000, 0.8660254037844387076, 1.000000000000000000, 0.8660254037844387076, 1.000000000000000000, 0.8660254037844387076, 1.000000000000000000, 0.8660254037844387076, 1.000000000000000000, 0.8660254037844387076, 1.000000000000000000, 0.8660254037844387076, 1.000000000000000000, 0.8660254037844387076, 1.000000000000000000, 0.8660254037844387076, 1.000000000000000000, 0.8660254037844387076, 1.000000000000000000, 0.8660254037844387076, 1.000000000000000000, 0.8660254037844387076, 1.000000000000000000, 0.8660254037844387076, 1.000000000000000000, 0.8660254037844387076, 1.000000000000000000, 0.8660254037844387076, 1.000000000000000000, 0.8660254037844387076, 1.000000000000000000, 0.8660254037844387076, 1.000000000000000000, 0.8660254037844387076, 1.000000000000000000, 0.8660254037844387076, 1.000000000000000000, 0.8660254037844387076, 1.000000000000000000, 0.8660254037844387076, 1.000000000000000000, 0.8660254037844387076, 1.000000000000000000, 0.8660254037844387076, 1.000000000000000000, 0.8660254037844387076, 1.000000000000000000, 0.8660254037844387076, 1.000000000000000000, 0.8660254037844387076, 1.000000000000000000, 0.8660254037844387076, 1.000000000000000000, 0.8660254037844387076, 1.000000000000000000, 0.8660254037844387076, 1.000000000000000000, 0.8660254037844387076, 1.000000000000000000, 0.8660254037844387076, 1.000000000000000000, 0.8660254037844387076, 1.000000000000000000, 0.8660254037844387076, 1.000000000000000000, 0.8660254037844387076, 1.000000000000000000, 0.8660254037844387076, 1.000000000000000000, 0.8660254037844387076, 1.000000000000000000, 0.8660254037844387076, 1.000000000000000000, 0.8660254037844387076, 1.000000000000000000, 0.8660254037844387076, 1.000000000000000000, 0.8660254037844387076, 1.000000000000000000, 0.8660254037844387076, 1.000000000000000000, 0.8660254037844387076, 1.000000000000000000, 0.8660254037844387076, 1.000000000000000000, 0.8660254037844387076, 1.000000000000000000, 0.8660254037844387076, 1.000000000000000000, 0.9024573129378109515, 0.9469501470576147106),
 ( 1.000000000000000000, 0.8660254037844387076, 1.000000000000000000, 0.8660254037844387076, 1.000000000000000000, 0.8660254037844387076, 1.000000000000000000, 0.8660254037844387076, 1.000000000000000000, 0.8660254037844387076, 1.000000000000000000, 0.8660254037844387076, 1.000000000000000000, 0.8660254037844387076, 1.000000000000000000, 0.8660254037844387076, 1.000000000000000000, 0.8660254037844387076, 1.000000000000000000, 0.8660254037844387076, 1.000000000000000000, 0.8660254037844387076, 1.000000000000000000, 0.8660254037844387076, 1.000000000000000000, 0.8660254037844387076, 1.000000000000000000, 0.8660254037844387076, 1.000000000000000000, 0.8660254037844387076, 1.000000000000000000, 0.8660254037844387076, 1.000000000000000000, 0.8660254037844387076, 1.000000000000000000, 0.8660254037844387076, 1.000000000000000000, 0.8660254037844387076, 1.000000000000000000, 0.8660254037844387076, 1.000000000000000000, 0.8660254037844387076, 1.000000000000000000, 0.8660254037844387076, 1.000000000000000000, 0.8660254037844387076, 1.000000000000000000, 0.8660254037844387076, 1.000000000000000000, 0.8660254037844387076, 1.000000000000000000, 0.8660254037844387076, 1.000000000000000000, 0.8660254037844387076, 1.000000000000000000, 0.8660254037844387076, 1.000000000000000000, 0.8660254037844387076, 1.000000000000000000, 0.8660254037844387076, 1.000000000000000000, 0.8660254037844387076, 1.000000000000000000, 0.8660254037844387076, 1.000000000000000000, 0.8660254037844387076, 1.000000000000000000, 0.8660254037844387076, 1.000000000000000000, 0.8660254037844387076, 1.000000000000000000, 0.8660254037844387076, 1.000000000000000000, 0.8660254037844387076, 1.000000000000000000, 0.8660254037844387076, 1.000000000000000000, 0.8660254037844387076, 1.000000000000000000, 0.8660254037844387076, 1.000000000000000000, 0.8660254037844387076, 1.000000000000000000, 0.8660254037844387076, 1.000000000000000000, 0.8660254037844387076, 1.000000000000000000, 0.8660254037844387076, 1.000000000000000000, 0.8660254037844387076, 1.000000000000000000, 0.8660254037844387076, 1.000000000000000000, 0.8660254037844387076, 1.000000000000000000, 0.8660254037844387076, 1.000000000000000000, 0.8660254037844387076, 1.000000000000000000, 0.8660254037844387076, 1.000000000000000000, 0.8660254037844387076, 1.000000000000000000, 0.8660254037844387076, 1.000000000000000000, 0.8660254037844387076, 1.000000000000000000, 0.8660254037844387076, 1.000000000000000000, 0.8660254037844387076, 1.000000000000000000, 0.8660254037844387076, 1.000000000000000000, 0.8660254037844387076, 1.000000000000000000, 0.8660254037844387076, 1.000000000000000000, 0.8660254037844387076, 1.000000000000000000, 0.8660254037844387076, 1.000000000000000000, 0.8660254037844387076, 1.000000000000000000, 0.8660254037844387076, 1.000000000000000000, 0.8660254037844387076, 1.000000000000000000, 0.8660254037844387076, 1.000000000000000000, 0.8660254037844387076, 1.000000000000000000, 0.8660254037844387076, 1.000000000000000000, 0.8660254037844387076, 1.000000000000000000, 0.8660254037844387076, 1.000000000000000000, 0.8660254037844387076, 1.000000000000000000, 0.8660254037844387076, 1.000000000000000000, 0.8660254037844387076, 1.000000000000000000, 0.8660254037844387076, 1.000000000000000000, 0.8660254037844387076, 1.000000000000000000, 0.8660254037844387076, 1.000000000000000000, 0.8660254037844387076, 1.000000000000000000, 0.8660254037844387076, 1.000000000000000000, 0.8660254037844387076, 1.000000000000000000, 0.8660254037844387076, 1.000000000000000000, 0.8660254037844387076, 1.000000000000000000, 0.8660254037844387076, 1.000000000000000000, 0.8660254037844387076, 1.000000000000000000, 0.8660254037844387076, 1.000000000000000000, 0.8660254037844387076, 1.000000000000000000, 0.8660254037844387076, 1.000000000000000000, 0.8660254037844387076, 1.000000000000000000, 0.8660254037844387076, 1.000000000000000000, 0.8660254037844387076, 1.000000000000000000, 0.8660254037844387076, 1.000000000000000000, 0.8660254037844387076, 1.000000000000000000, 0.8660254037844387076, 1.000000000000000000, 0.8660254037844387076, 1.000000000000000000, 0.8660254037844387076, 1.000000000000000000, 0.8660254037844387076, 1.000000000000000000, 0.8660254037844387076, 1.000000000000000000, 0.8660254037844387076, 1.000000000000000000, 0.8660254037844387076, 1.000000000000000000, 0.8660254037844387076, 1.000000000000000000, 0.8660254037844387076, 1.000000000000000000, 0.8660254037844387076, 1.000000000000000000, 0.8660254037844387076, 1.000000000000000000, 0.8660254037844387076, 1.000000000000000000, 0.8660254037844387076, 1.000000000000000000, 0.8660254037844387076, 1.000000000000000000, 0.8660254037844387076, 1.000000000000000000, 0.8660254037844387076, 1.000000000000000000, 0.8660254037844387076, 1.000000000000000000, 0.8660254037844387076, 1.000000000000000000, 0.8660254037844387076, 1.000000000000000000, 0.8660254037844387076, 1.000000000000000000, 0.8660254037844387076, 1.000000000000000000, 0.8660254037844387076, 1.000000000000000000, 0.8660254037844387076, 1.000000000000000000, 0.8660254037844387076, 1.000000000000000000, 0.8660254037844387076, 1.000000000000000000, 0.8660254037844387076, 1.000000000000000000, 0.8660254037844387076, 1.000000000000000000, 0.8660254037844387076, 1.000000000000000000, 0.8660254037844387076, 1.000000000000000000, 0.8660254037844387076, 1.000000000000000000, 0.8660254037844387076, 1.000000000000000000, 0.8660254037844387076, 1.000000000000000000, 0.8660254037844387076, 1.000000000000000000, 0.8660254037844387076, 1.000000000000000000, 0.8660254037844387076, 1.000000000000000000, 0.8660254037844387076, 1.000000000000000000, 0.8660254037844387076, 1.000000000000000000, 0.8660254037844387076, 1.000000000000000000, 0.8660254037844387076, 1.000000000000000000, 0.8660254037844387076, 1.000000000000000000, 0.8660254037844387076, 1.000000000000000000, 0.8660254037844387076, 1.000000000000000000, 0.8660254037844387076, 1.000000000000000000, 0.8660254037844387076, 1.000000000000000000, 0.8660254037844387076, 1.000000000000000000, 0.8660254037844387076, 1.000000000000000000, 0.8660254037844387076, 1.000000000000000000, 0.8660254037844387076, 1.000000000000000000, 0.8660254037844387076, 1.000000000000000000, 0.8660254037844387076, 1.000000000000000000, 0.8660254037844387076, 1.000000000000000000, 0.8660254037844387076, 1.000000000000000000, 0.9024573129378109515, 0.9469501470576147106) ) ) 
 REPRESENTATION_ITEM ( '' )  SURFACE ( )  );
#33868 = CARTESIAN_POINT ( 'NONE',  ( 11.99999999999999822, 0.000000000000000000, 0.000000000000000000 ) ) ;
#33869 = CARTESIAN_POINT ( 'NONE',  ( -92.69370383062498320, -209.9999999999999716, 87.42031250086714067 ) ) ;
#33871 = ORIENTED_EDGE ( 'NONE', *, *, #44346, .T. ) ;
#33870 = EDGE_CURVE ( 'NONE', #3810, #13922, #13185, .T. ) ;
#33872 = CARTESIAN_POINT ( 'NONE',  ( 2.018853055115724882, -4.607917337070903230, -0.5666985376598668855 ) ) ;
#33873 = CARTESIAN_POINT ( 'NONE',  ( -10.00000000000000000, 0.000000000000000000, 0.000000000000000000 ) ) ;
#33874 = CARTESIAN_POINT ( 'NONE',  ( 10.00000000000000000, -23.16143007188481207, 73.95703589263968070 ) ) ;
#33875 = CARTESIAN_POINT ( 'NONE',  ( -92.69370383062498320, -209.9999999999999716, 75.35531250086714294 ) ) ;
#33876 = MECHANICAL_DESIGN_GEOMETRIC_PRESENTATION_REPRESENTATION (  '', ( #47083 ), #68715 ) ;
#33877 = DIRECTION ( 'NONE',  ( 0.000000000000000000, 0.9510565162951504226, -0.3090169943749573322 ) ) ;
#33878 = DIRECTION ( 'NONE',  ( -1.000000000000000000, 0.000000000000000000, 0.000000000000000000 ) ) ;
#33879 = AXIS2_PLACEMENT_3D ( 'NONE', #48044, #52945, #64978 ) ;
#33880 = CYLINDRICAL_SURFACE ( 'NONE', #28845, 31.99999999999998579 ) ;
#33881 = DIRECTION ( 'NONE',  ( -1.000000000000000000, 0.000000000000000000, -0.000000000000000000 ) ) ;
#33882 = EDGE_CURVE ( 'NONE', #61698, #56516, #48993, .T. ) ;
#33883 = LINE ( 'NONE', #74099, #12734 ) ;
#33884 = CIRCLE ( 'NONE', #31460, 82.00000000000000000 ) ;
#33885 = EDGE_CURVE ( 'NONE', #9195, #40982, #65941, .T. ) ;
#33886 = CARTESIAN_POINT ( 'NONE',  ( -97.30629616937501680, 88.66845928578038638, 83.34572916753380412 ) ) ;
#33887 = CARTESIAN_POINT ( 'NONE',  ( 10.00000000000000000, 0.000000000000000000, 0.000000000000000000 ) ) ;
#33888 = DIRECTION ( 'NONE',  ( 0.000000000000000000, 0.000000000000000000, 1.000000000000000000 ) ) ;
#33889 = AXIS2_PLACEMENT_3D ( 'NONE', #5226, #63114, #28490 ) ;
#33890 = ORIENTED_EDGE ( 'NONE', *, *, #15169, .T. ) ;
#33891 = CARTESIAN_POINT ( 'NONE',  ( -92.34999999999999432, -210.0000000983656605, 80.23687499810813506 ) ) ;
#33892 = DIRECTION ( 'NONE',  ( 0.000000000000000000, 0.000000000000000000, 1.000000000000000000 ) ) ;
#33893 = DIRECTION ( 'NONE',  ( -1.000000000000000000, 0.000000000000000000, 0.000000000000000000 ) ) ;
#33894 = EDGE_CURVE ( 'NONE', #25438, #60516, #37370, .T. ) ;
#33896 = EDGE_CURVE ( 'NONE', #37374, #57268, #40783, .T. ) ;
#33895 = VECTOR ( 'NONE', #35521, 1000.000000000000000 ) ;
#33897 = DIRECTION ( 'NONE',  ( 0.000000000000000000, -0.3826834323650969427, 0.9238795325112837409 ) ) ;
#33898 = DIRECTION ( 'NONE',  ( -1.000000000000000000, -0.000000000000000000, -0.000000000000000000 ) ) ;
#33899 = DIRECTION ( 'NONE',  ( -1.000000000000000000, 0.000000000000000000, -0.000000000000000000 ) ) ;
#33900 = CARTESIAN_POINT ( 'NONE',  ( -97.30629616937497417, -211.3315407142195852, 79.69447916753381378 ) ) ;
#33901 = CARTESIAN_POINT ( 'NONE',  ( 26.47460221209471953, -121.8961639463267090, -2.500000000000000000 ) ) ;
#33902 = ORIENTED_EDGE ( 'NONE', *, *, #5707, .T. ) ;
#33903 = DIRECTION ( 'NONE',  ( 0.9580045777625458836, 0.2867529058022011412, 0.000000000000000000 ) ) ;
#33904 = CARTESIAN_POINT ( 'NONE',  ( 97.64999999999996305, -209.9999996502043018, 77.69687501385438111 ) ) ;
#33905 = CARTESIAN_POINT ( 'NONE',  ( 15.00000000000000000, 20.85821328998756385, 10.92862929874494249 ) ) ;
#33906 = CARTESIAN_POINT ( 'NONE',  ( 0.000000000000000000, -27.05870788708213226, -26.08949754953053102 ) ) ;
#33907 = DIRECTION ( 'NONE',  ( -0.000000000000000000, -0.000000000000000000, 1.000000000000000000 ) ) ;
#33908 = CARTESIAN_POINT ( 'NONE',  ( 11.99999999999999822, -59.03342792756231461, -46.54456581323868392 ) ) ;
#33909 = ORIENTED_EDGE ( 'NONE', *, *, #6534, .F. ) ;
#33910 = CARTESIAN_POINT ( 'NONE',  ( -10.00000000000000000, 0.000000000000000000, 0.000000000000000000 ) ) ;
#33911 = DIRECTION ( 'NONE',  ( 0.000000000000000000, -0.9876883405951358830, -0.1564344650402420822 ) ) ;
#33912 = ORIENTED_EDGE ( 'NONE', *, *, #38272, .F. ) ;
#33913 = CARTESIAN_POINT ( 'NONE',  ( -3.000000000000000000, 20.85821328998756385, -10.92862929874494959 ) ) ;
#33914 = DIRECTION ( 'NONE',  ( -1.000000000000000000, -0.000000000000000000, -0.000000000000000000 ) ) ;
#33915 = ORIENTED_EDGE ( 'NONE', *, *, #43804, .F. ) ;
#33916 = EDGE_CURVE ( 'NONE', #50573, #32331, #66670, .T. ) ;
#33917 = DIRECTION ( 'NONE',  ( 0.000000000000000000, 0.8910065241883657894, 0.4539904997395510788 ) ) ;
#33918 = COLOUR_RGB ( '', 0.31764706, 0.68627451, 0.89019608) ;
#33919 = ORIENTED_EDGE ( 'NONE', *, *, #43804, .T. ) ;
#33920 = FACE_BOUND ( 'NONE', #44055, .T. ) ;
#33921 = ORIENTED_EDGE ( 'NONE', *, *, #3324, .F. ) ;
#33922 = DIRECTION ( 'NONE',  ( -0.9038112904824853189, 0.4279312458752976833, 0.000000000000000000 ) ) ;
#33923 = VECTOR ( 'NONE', #73851, 1000.000000000000000 ) ;
#33924 = ORIENTED_EDGE ( 'NONE', *, *, #17344, .F. ) ;
#33925 = VERTEX_POINT ( 'NONE', #65200 ) ;
#33926 = EDGE_CURVE ( 'NONE', #61974, #51872, #8366, .T. ) ;
#33927 = EDGE_LOOP ( 'NONE', ( #50929, #4478, #43741, #18412 ) ) ;
#33928 = DIRECTION ( 'NONE',  ( 0.000000000000000000, 0.000000000000000000, 1.000000000000000000 ) ) ;
#33929 = EDGE_CURVE ( 'NONE', #69505, #57102, #50366, .T. ) ;
#33930 = AXIS2_PLACEMENT_3D ( 'NONE', #3213, #2494, #49414 ) ;
#33931 = ORIENTED_EDGE ( 'NONE', *, *, #2596, .T. ) ;
#33932 = AXIS2_PLACEMENT_3D ( 'NONE', #22091, #45030, #27343 ) ;
#33933 = ORIENTED_EDGE ( 'NONE', *, *, #37785, .F. ) ;
#33934 = CARTESIAN_POINT ( 'NONE',  ( 96.32499999999998863, 87.70503267997126784, 87.67166666666666686 ) ) ;
#33935 = FACE_OUTER_BOUND ( 'NONE', #26566, .T. ) ;
#33936 = CYLINDRICAL_SURFACE ( 'NONE', #74147, 37.49900000000000233 ) ;
#33937 = ORIENTED_EDGE ( 'NONE', *, *, #12912, .T. ) ;
#33938 = EDGE_CURVE ( 'NONE', #15883, #50966, #32806, .T. ) ;
#33939 = ORIENTED_EDGE ( 'NONE', *, *, #67968, .F. ) ;
#33940 = ORIENTED_EDGE ( 'NONE', *, *, #25861, .T. ) ;
#33941 = CARTESIAN_POINT ( 'NONE',  ( 97.30629616937498838, 90.00000000000002842, 84.88031250086713442 ) ) ;
#33942 = CIRCLE ( 'NONE', #48381, 15.80000000000028315 ) ;
#33943 = VERTEX_POINT ( 'NONE', #4272 ) ;
#33944 = CARTESIAN_POINT ( 'NONE',  ( 92.69370383062501162, -211.3315407142195852, 85.88572916753382458 ) ) ;
#33945 = APPLICATION_PROTOCOL_DEFINITION ( 'draft international standard', 'automotive_design', 1998, #34457 ) ;
#33946 = CARTESIAN_POINT ( 'NONE',  ( 50.00005079999999680, 12.24744871391589207, -2.499999999999994671 ) ) ;
#33947 = CARTESIAN_POINT ( 'NONE',  ( 10.00000000000000000, -76.41127070299280888, 12.93880638057289012 ) ) ;
#33948 = CARTESIAN_POINT ( 'NONE',  ( 10.00000000000000000, -8.830959090341869100, -74.65491531819127147 ) ) ;
#33949 = DIRECTION ( 'NONE',  ( -1.000000000000000000, 0.000000000000000000, 0.000000000000000000 ) ) ;
#33950 = CARTESIAN_POINT ( 'NONE',  ( -96.32500000000001705, 87.70503267997129626, 79.31083333333333485 ) ) ;
#33951 = CARTESIAN_POINT ( 'NONE',  ( 0.000000000000000000, -36.88895765772637247, 6.736453364083436313 ) ) ;
#33952 = CARTESIAN_POINT ( 'NONE',  ( -93.84685191531248449, -208.0026889286704943, 86.25614583420048120 ) ) ;
#33953 = CARTESIAN_POINT ( 'NONE',  ( -97.30629616937501680, 90.00000000000004263, 85.99156250086716113 ) ) ;
#33954 = EDGE_LOOP ( 'NONE', ( #63918, #44488, #17215, #2729 ) ) ;
#33956 = CARTESIAN_POINT ( 'NONE',  ( -92.69370383062502583, 88.66845928578038638, 84.19239583420046813 ) ) ;
#33955 = CARTESIAN_POINT ( 'NONE',  ( 97.30629616937498838, 88.66845928578037217, 82.92239583420045790 ) ) ;
#33957 = ORIENTED_EDGE ( 'NONE', *, *, #55444, .F. ) ;
#33958 = FACE_OUTER_BOUND ( 'NONE', #46625, .T. ) ;
#33959 = EDGE_CURVE ( 'NONE', #11821, #47514, #67404, .T. ) ;
#33960 = CARTESIAN_POINT ( 'NONE',  ( -94.99999999999997158, -213.0599564267049857, 80.71312500173429783 ) ) ;
#33961 = CARTESIAN_POINT ( 'NONE',  ( 11.99999999999999822, 76.66974797899852945, -11.30684508768257679 ) ) ;
#33962 = CARTESIAN_POINT ( 'NONE',  ( 0.000000000000000000, -10.41901085202050581, -40.68715046381939970 ) ) ;
#33963 = CARTESIAN_POINT ( 'NONE',  ( -92.69370383062498320, -208.6684592857803295, 88.10822916753380696 ) ) ;
#33964 = CARTESIAN_POINT ( 'NONE',  ( -92.34999999999996589, -211.5299782133524502, 82.00958333333333883 ) ) ;
#33965 = DIRECTION ( 'NONE',  ( 0.000000000000000000, -0.5000000000000039968, -0.8660254037844363761 ) ) ;
#33966 = LINE ( 'NONE', #34335, #21767 ) ;
#33967 = FACE_OUTER_BOUND ( 'NONE', #67517, .T. ) ;
#33968 = EDGE_LOOP ( 'NONE', ( #29603, #58014, #4404, #17564 ) ) ;
#33969 = VERTEX_POINT ( 'NONE', #74151 ) ;
#33970 = CARTESIAN_POINT ( 'NONE',  ( -96.32500000000001705, 92.29496732002878900, 78.46416666666667084 ) ) ;
#33971 = EDGE_CURVE ( 'NONE', #29677, #14426, #61406, .T. ) ;
#33972 = DIRECTION ( 'NONE',  ( 0.000000000000000000, 0.000000000000000000, 1.000000000000000000 ) ) ;
#33973 = ADVANCED_FACE ( 'NONE', ( #33935 ), #28283, .F. ) ;
#33974 = CARTESIAN_POINT ( 'NONE',  ( -7.499999999999969802, 76.29999999999999716, -255.0000000000000000 ) ) ;
#33975 = CARTESIAN_POINT ( 'NONE',  ( -92.35000000000306386, -210.0000040461925437, 77.06187486178056645 ) ) ;
#33976 = DIRECTION ( 'NONE',  ( 0.000000000000000000, 0.3826834323650904479, -0.9238795325112865164 ) ) ;
#33977 = CARTESIAN_POINT ( 'NONE',  ( 0.000000000000000000, -22.67460108101774807, -6.353146135318215038 ) ) ;
#33978 = CARTESIAN_POINT ( 'NONE',  ( -3.000000000000000000, 14.60985201121704513, 18.46759930825707841 ) ) ;
#33979 = EDGE_CURVE ( 'NONE', #67669, #31441, #55200, .T. ) ;
#33980 = ORIENTED_EDGE ( 'NONE', *, *, #41370, .T. ) ;
#33981 = CARTESIAN_POINT ( 'NONE',  ( -96.15314808468751551, 88.00268892867056536, 79.58864583420047722 ) ) ;
#33982 = AXIS2_PLACEMENT_3D ( 'NONE', #20060, #19324, #14046 ) ;
#33983 = DIRECTION ( 'NONE',  ( 0.000000000000000000, 1.000000000000000000, 0.000000000000000000 ) ) ;
#33984 = DIRECTION ( 'NONE',  ( -0.000000000000000000, -1.000000000000000000, -0.000000000000000000 ) ) ;
#33985 = AXIS2_PLACEMENT_3D ( 'NONE', #71720, #49540, #13837 ) ;
#33986 = CARTESIAN_POINT ( 'NONE',  ( 10.00000000000000000, 0.000000000000000000, 0.000000000000000000 ) ) ;
#33987 = DIRECTION ( 'NONE',  ( -1.000000000000000000, 0.000000000000000000, -0.000000000000000000 ) ) ;
#33988 = DIRECTION ( 'NONE',  ( 0.000000000000000000, 0.000000000000000000, 1.000000000000000000 ) ) ;
#33989 = LINE ( 'NONE', #50537, #74243 ) ;
#33990 =( BOUNDED_CURVE ( )  B_SPLINE_CURVE ( 2, ( #26317, #66188, #54890, #9391, #53778, #2701, #65813 ),
 .UNSPECIFIED., .F., .F. ) 
 B_SPLINE_CURVE_WITH_KNOTS ( ( 3, 2, 2, 3 ),
 ( 0.7408554641864679713, 0.7479111473335298133, 0.7549669128744131985, 0.7620226289464459013 ),
 .UNSPECIFIED. ) 
 CURVE ( )  GEOMETRIC_REPRESENTATION_ITEM ( )  RATIONAL_B_SPLINE_CURVE ( ( 0.9999968710553057694, 0.8660269682750552089, 1.000000000000000000, 0.8660254037844387076, 1.000000000000000000, 0.8660263430970122078, 0.9999981213880242414 ) ) 
 REPRESENTATION_ITEM ( '' )  );
#33991 = AXIS2_PLACEMENT_3D ( 'NONE', #17927, #18656, #69794 ) ;
#33992 = AXIS2_PLACEMENT_3D ( 'NONE', #12895, #35824, #63692 ) ;
#33993 = CARTESIAN_POINT ( 'NONE',  ( 93.84685191531248449, 88.00268892867053694, 78.47739583420049314 ) ) ;
#33994 = CARTESIAN_POINT ( 'NONE',  ( -92.69370383062498320, -211.3315407142195852, 80.54114583420049200 ) ) ;
#33995 = CARTESIAN_POINT ( 'NONE',  ( 10.00000000000000000, 81.96053171279901051, -2.543863470248666658 ) ) ;
#33996 = EDGE_LOOP ( 'NONE', ( #14665, #17291, #40321, #13108, #56651, #29111 ) ) ;
#33997 = CARTESIAN_POINT ( 'NONE',  ( -12.49999999999999822, -120.0000000000000000, -125.0000000000000000 ) ) ;
#33998 = DIRECTION ( 'NONE',  ( 0.000000000000000000, 0.1564344650402311743, -0.9876883405951377704 ) ) ;
#33999 = CARTESIAN_POINT ( 'NONE',  ( -12.49999999999999822, -120.0000000000000000, 125.0000000000000000 ) ) ;
#34000 = AXIS2_PLACEMENT_3D ( 'NONE', #37955, #37226, #73269 ) ;
#34001 = CARTESIAN_POINT ( 'NONE',  ( -97.30629616937501680, 91.33154071421968467, 77.04864583420048518 ) ) ;
#34002 = CARTESIAN_POINT ( 'NONE',  ( 95.00000000000000000, -212.6630814284392557, 79.64156250086713840 ) ) ;
#34003 = EDGE_LOOP ( 'NONE', ( #23028, #3939 ) ) ;
#34004 = FACE_OUTER_BOUND ( 'NONE', #22975, .T. ) ;
#34005 = ORIENTED_EDGE ( 'NONE', *, *, #45680, .T. ) ;
#34006 = FACE_OUTER_BOUND ( 'NONE', #61942, .T. ) ;
#34007 = ORIENTED_EDGE ( 'NONE', *, *, #68354, .F. ) ;
#34008 = CARTESIAN_POINT ( 'NONE',  ( 92.34999999999999432, 90.00000000000002842, 90.00000000000000000 ) ) ;
#34009 = EDGE_LOOP ( 'NONE', ( #60704, #67577, #20443, #12843, #67504 ) ) ;
#34010 = ORIENTED_EDGE ( 'NONE', *, *, #28622, .T. ) ;
#34011 = EDGE_CURVE ( 'NONE', #53012, #35341, #22663, .T. ) ;
#34012 = VERTEX_POINT ( 'NONE', #61777 ) ;
#34013 = CARTESIAN_POINT ( 'NONE',  ( 97.30629616937498838, -208.6684592857803295, 76.20197916753382117 ) ) ;
#34014 = EDGE_CURVE ( 'NONE', #16321, #21495, #5754, .T. ) ;
#34015 = EDGE_LOOP ( 'NONE', ( #33287, #62264, #63997, #57039 ) ) ;
#34016 =( REPRESENTATION_RELATIONSHIP ('NONE','NONE', #31117, #72820 ) REPRESENTATION_RELATIONSHIP_WITH_TRANSFORMATION ( #8704 )SHAPE_REPRESENTATION_RELATIONSHIP( ) );
#34017 = CARTESIAN_POINT ( 'NONE',  ( 10.00000000000000000, -25.88420570971419821, 27.13269053701087330 ) ) ;
#34018 = AXIS2_PLACEMENT_3D ( 'NONE', #71608, #12982, #65256 ) ;
#34019 = DIRECTION ( 'NONE',  ( 0.000000000000000000, 0.000000000000000000, 1.000000000000000000 ) ) ;
#34020 = CARTESIAN_POINT ( 'NONE',  ( 93.84685191531248449, 88.00268892867053694, 84.19239583420049655 ) ) ;
#34021 = CARTESIAN_POINT ( 'NONE',  ( 97.64999999999999147, -209.9999999999999716, 78.88750000000000284 ) ) ;
#34022 = ORIENTED_EDGE ( 'NONE', *, *, #12545, .F. ) ;
#34023 = EDGE_CURVE ( 'NONE', #48419, #30862, #16269, .T. ) ;
#34024 = LINE ( 'NONE', #45439, #24463 ) ;
#34025 = ORIENTED_EDGE ( 'NONE', *, *, #29091, .T. ) ;
#34026 = EDGE_CURVE ( 'NONE', #44464, #73369, #27566, .T. ) ;
#34027 = ORIENTED_EDGE ( 'NONE', *, *, #15424, .F. ) ;
#34028 = ORIENTED_EDGE ( 'NONE', *, *, #6039, .F. ) ;
#34029 = DIRECTION ( 'NONE',  ( -1.000000000000000000, 0.000000000000000000, 0.000000000000000000 ) ) ;
#34030 = AXIS2_PLACEMENT_3D ( 'NONE', #46883, #29194, #13018 ) ;
#34031 = CARTESIAN_POINT ( 'NONE',  ( 92.34999999999999432, 90.00000000000002842, 83.65000000000000568 ) ) ;
#34032 = DIRECTION ( 'NONE',  ( -1.000000000000000000, 0.000000000000000000, 0.000000000000000000 ) ) ;
#34033 = CYLINDRICAL_SURFACE ( 'NONE', #46220, 20.99999999999999645 ) ;
#34034 = CARTESIAN_POINT ( 'NONE',  ( 0.000000000000000000, 0.000000000000000000, -270.0000000000000000 ) ) ;
#34035 = CYLINDRICAL_SURFACE ( 'NONE', #60829, 2.649999999999999467 ) ;
#34036 = ORIENTED_EDGE ( 'NONE', *, *, #8139, .F. ) ;
#34037 = CARTESIAN_POINT ( 'NONE',  ( -97.64999999999996305, -209.9999999999999716, 83.72937500173429726 ) ) ;
#34038 = ORIENTED_EDGE ( 'NONE', *, *, #56224, .F. ) ;
#34039 = DIRECTION ( 'NONE',  ( 0.000000000000000000, 0.000000000000000000, 1.000000000000000000 ) ) ;
#34040 = ORIENTED_EDGE ( 'NONE', *, *, #22748, .F. ) ;
#34042 = CARTESIAN_POINT ( 'NONE',  ( -96.32500000000001705, 87.70503267997129626, 80.66020833506763665 ) ) ;
#34041 = CARTESIAN_POINT ( 'NONE',  ( 97.64999999999997726, 91.52997821335252127, 78.38479166840096468 ) ) ;
#34043 = AXIS2_PLACEMENT_3D ( 'NONE', #73305, #8691, #21426 ) ;
#34044 = VERTEX_POINT ( 'NONE', #51223 ) ;
#34045 = CARTESIAN_POINT ( 'NONE',  ( 93.84685191531248449, 88.00268892867053694, 83.55739583420049144 ) ) ;
#34046 = AXIS2_PLACEMENT_3D ( 'NONE', #59059, #54161, #2692 ) ;
#34047 = EDGE_CURVE ( 'NONE', #43336, #52788, #5017, .T. ) ;
#34048 = DIRECTION ( 'NONE',  ( 0.000000000000000000, -0.9510565162951499785, -0.3090169943749582204 ) ) ;
#34049 = CARTESIAN_POINT ( 'NONE',  ( 97.64999999999999147, 90.00000000000002842, 90.00000000000000000 ) ) ;
#34050 = DIRECTION ( 'NONE',  ( -1.000000000000000000, 0.000000000000000000, 0.000000000000000000 ) ) ;
#34051 = CARTESIAN_POINT ( 'NONE',  ( 11.99999999999999822, 0.000000000000000000, 0.000000000000000000 ) ) ;
#34052 = CYLINDRICAL_SURFACE ( 'NONE', #17938, 16.00000000000000000 ) ;
#34053 = VERTEX_POINT ( 'NONE', #67782 ) ;
#34054 = CARTESIAN_POINT ( 'NONE',  ( -95.00000000000002842, 90.00000000000004263, 90.00000000000000000 ) ) ;
#34056 = CARTESIAN_POINT ( 'NONE',  ( -3.000000000000002665, 0.000000000000000000, 0.000000000000000000 ) ) ;
#34055 = VECTOR ( 'NONE', #37135, 1000.000000000000000 ) ;
#34057 = CARTESIAN_POINT ( 'NONE',  ( -3.249999999999999556, -13.95926121303099343, -1.199999999999999956 ) ) ;
#34058 = VERTEX_POINT ( 'NONE', #45610 ) ;
#34059 = ORIENTED_EDGE ( 'NONE', *, *, #26044, .T. ) ;
#34060 = DIRECTION ( 'NONE',  ( -0.000000000000000000, -0.000000000000000000, -1.000000000000000000 ) ) ;
#34061 = ADVANCED_FACE ( 'NONE', ( #17021 ), #33554, .T. ) ;
#34062 = EDGE_CURVE ( 'NONE', #39425, #28922, #23989, .T. ) ;
#34063 = CYLINDRICAL_SURFACE ( 'NONE', #10819, 82.00000000000000000 ) ;
#34064 = EDGE_CURVE ( 'NONE', #39002, #70270, #71997, .T. ) ;
#34065 = FACE_OUTER_BOUND ( 'NONE', #20922, .T. ) ;
#34066 = PLANE ( 'NONE',  #1765 ) ;
#34067 = CARTESIAN_POINT ( 'NONE',  ( -93.84685191531247028, -211.9973110713294489, 81.75822916753382685 ) ) ;
#34068 = ORIENTED_EDGE ( 'NONE', *, *, #58978, .T. ) ;
#34069 = ORIENTED_EDGE ( 'NONE', *, *, #64499, .T. ) ;
#34070 = VECTOR ( 'NONE', #30512, 1000.000000000000000 ) ;
#34071 = FACE_OUTER_BOUND ( 'NONE', #51266, .T. ) ;
#34072 = CARTESIAN_POINT ( 'NONE',  ( -95.29566955672730444, -212.6272429001226953, 74.99300273738367650 ) ) ;
#34073 = CARTESIAN_POINT ( 'NONE',  ( 15.00000000000000000, 24.81905959214275370, 9.408202855044498492 ) ) ;
#34074 = CARTESIAN_POINT ( 'NONE',  ( 93.84685191531248449, 88.00268892867053694, 75.14364583420046984 ) ) ;
#34075 = DIRECTION ( 'NONE',  ( -1.000000000000000000, 0.000000000000000000, 0.000000000000000000 ) ) ;
#34076 = CARTESIAN_POINT ( 'NONE',  ( 10.00000000000000000, 33.17418723428307459, 17.67226234102837878 ) ) ;
#34077 = LINE ( 'NONE', #23183, #5264 ) ;
#34078 = DIRECTION ( 'NONE',  ( 0.000000000000000000, 0.7071067811865437980, 0.7071067811865512365 ) ) ;
#34079 = CYLINDRICAL_SURFACE ( 'NONE', #24963, 31.99999999999998579 ) ;
#34080 = CIRCLE ( 'NONE', #62931, 31.99999999999998579 ) ;
#34081 =( BOUNDED_CURVE ( )  B_SPLINE_CURVE ( 2, ( #21715, #45412, #5567, #28842, #22095, #45034, #67958, #28096, #16453 ),
 .UNSPECIFIED., .F., .F. ) 
 B_SPLINE_CURVE_WITH_KNOTS ( ( 3, 2, 2, 2, 3 ),
 ( 0.4868478063929145838, 0.4939035878617654696, 0.5009593534026473005, 0.5080151189435291315, 0.5080151867253829279 ),
 .UNSPECIFIED. ) 
 CURVE ( )  GEOMETRIC_REPRESENTATION_ITEM ( )  RATIONAL_B_SPLINE_CURVE ( ( 1.000000000000000000, 0.8660254037844387076, 1.000000000000000000, 0.8660254037844387076, 1.000000000000000000, 0.8660254037844387076, 1.000000000000000000, 0.9999987129608483016, 0.9999974259464248227 ) ) 
 REPRESENTATION_ITEM ( '' )  );
#34082 = CARTESIAN_POINT ( 'NONE',  ( 96.15314808468748708, 88.00268892867053694, 86.83822916753382515 ) ) ;
#34083 = CIRCLE ( 'NONE', #480, 77.49899999999998101 ) ;
#34084 = CARTESIAN_POINT ( 'NONE',  ( -96.15314808468745866, -211.9973110713294489, 89.27239583420049485 ) ) ;
#34085 = CARTESIAN_POINT ( 'NONE',  ( 7.999999999999994671, 1.778014505780935420E-13, 15.80000000000000426 ) ) ;
#34086 = VERTEX_POINT ( 'NONE', #21159 ) ;
#34087 = DIRECTION ( 'NONE',  ( 1.000000000000000000, 0.000000000000000000, 0.000000000000000000 ) ) ;
#34088 = CARTESIAN_POINT ( 'NONE',  ( -97.30629616937501680, 91.33154071421968467, 78.79489583420047438 ) ) ;
#34089 = CIRCLE ( 'NONE', #54529, 3.299999999999997158 ) ;
#34090 = CARTESIAN_POINT ( 'NONE',  ( 0.000000000000000000, 0.000000000000000000, 0.000000000000000000 ) ) ;
#34091 = AXIS2_PLACEMENT_3D ( 'NONE', #5915, #50636, #51755 ) ;
#34092 = EDGE_CURVE ( 'NONE', #57897, #9142, #43203, .T. ) ;
#34093 = ORIENTED_EDGE ( 'NONE', *, *, #69046, .F. ) ;
#34094 = VECTOR ( 'NONE', #20233, 1000.000000000000000 ) ;
#34095 = PLANE ( 'NONE',  #48646 ) ;
#34097 = PLANE ( 'NONE',  #27568 ) ;
#34096 = AXIS2_PLACEMENT_3D ( 'NONE', #1682, #46034, #29822 ) ;
#34098 = LINE ( 'NONE', #45024, #10763 ) ;
#34099 = ADVANCED_FACE ( 'NONE', ( #16643 ), #73776, .F. ) ;
#34100 = AXIS2_PLACEMENT_3D ( 'NONE', #49050, #30639, #26495 ) ;
#34101 = DIRECTION ( 'NONE',  ( -1.000000000000000000, 0.000000000000000000, 0.000000000000000000 ) ) ;
#34102 = CARTESIAN_POINT ( 'NONE',  ( 10.00000000000000000, 10.96151621346487914, 35.95386929396260456 ) ) ;
#34103 = EDGE_CURVE ( 'NONE', #34053, #28563, #20382, .T. ) ;
#34104 = EDGE_LOOP ( 'NONE', ( #63260, #63473, #29925, #54838 ) ) ;
#34105 = EDGE_CURVE ( 'NONE', #26720, #65774, #25218, .T. ) ;
#34106 = ORIENTED_EDGE ( 'NONE', *, *, #15438, .T. ) ;
#34107 = DIRECTION ( 'NONE',  ( 1.000000000000000000, -0.000000000000000000, 0.000000000000000000 ) ) ;
#34108 = DIRECTION ( 'NONE',  ( -1.000000000000000000, -0.000000000000000000, -0.000000000000000000 ) ) ;
#34109 = CARTESIAN_POINT ( 'NONE',  ( 10.00000000000000000, -12.26510123303234501, -35.53030884539098366 ) ) ;
#34110 = CARTESIAN_POINT ( 'NONE',  ( -7.499999999999970690, 69.70000000000001705, -204.9999999999999716 ) ) ;
#34111 = DIRECTION ( 'NONE',  ( 1.000000000000000000, -0.000000000000000000, -0.000000000000000000 ) ) ;
#34112 = CARTESIAN_POINT ( 'NONE',  ( 92.35000000000002274, -211.5299782133524502, 88.78291666666667936 ) ) ;
#34113 = AXIS2_PLACEMENT_3D ( 'NONE', #64380, #30150, #41082 ) ;
#34114 = EDGE_LOOP ( 'NONE', ( #22686, #615, #12193, #66227 ) ) ;
#34115 = EDGE_CURVE ( 'NONE', #60600, #48290, #40695, .T. ) ;
#34116 = ORIENTED_EDGE ( 'NONE', *, *, #2237, .T. ) ;
#34117 = DIRECTION ( 'NONE',  ( 0.000000000000000000, 1.224646799147353207E-16, 1.000000000000000000 ) ) ;
#34118 = VERTEX_POINT ( 'NONE', #51963 ) ;
#34119 = ORIENTED_EDGE ( 'NONE', *, *, #61867, .F. ) ;
#34120 = DIRECTION ( 'NONE',  ( 0.9135454576426059736, -0.4067366430757887730, 0.000000000000000000 ) ) ;
#34121 = CARTESIAN_POINT ( 'NONE',  ( 10.00000000000000000, -6.736453364083292428, -36.88895765772640800 ) ) ;
#34122 = CARTESIAN_POINT ( 'NONE',  ( 0.000000000000000000, -70.52718814184240159, -26.02418014898383802 ) ) ;
#34123 = CARTESIAN_POINT ( 'NONE',  ( 97.64999999999997726, -208.4700217866474645, 77.74979166840097378 ) ) ;
#34124 = CARTESIAN_POINT ( 'NONE',  ( 94.99999999999998579, 93.05995642670504253, 82.22124999999999773 ) ) ;
#34125 = ORIENTED_EDGE ( 'NONE', *, *, #56753, .T. ) ;
#34126 = DIRECTION ( 'NONE',  ( 1.000000000000000000, 0.000000000000000000, 0.000000000000000000 ) ) ;
#34127 = ORIENTED_EDGE ( 'NONE', *, *, #12900, .T. ) ;
#34128 = DIRECTION ( 'NONE',  ( -0.000000000000000000, -0.000000000000000000, 1.000000000000000000 ) ) ;
#34129 = AXIS2_PLACEMENT_3D ( 'NONE', #5148, #56260, #45367 ) ;
#34130 = ADVANCED_FACE ( 'NONE', ( #53083, #58347 ), #57982, .F. ) ;
#34131 = ORIENTED_EDGE ( 'NONE', *, *, #38897, .F. ) ;
#34132 = CARTESIAN_POINT ( 'NONE',  ( 92.35002600533567829, 88.47000677245996769, 84.41729270697884147 ) ) ;
#34133 = CARTESIAN_POINT ( 'NONE',  ( -92.69370383062505425, 91.33154071421968467, 80.64697916753382856 ) ) ;
#34134 = CARTESIAN_POINT ( 'NONE',  ( 93.84685191531248449, 91.99731107132950569, 76.83697916753381207 ) ) ;
#34135 = EDGE_CURVE ( 'NONE', #18610, #28278, #64321, .T. ) ;
#34136 = VERTEX_POINT ( 'NONE', #511 ) ;
#34137 = CARTESIAN_POINT ( 'NONE',  ( 0.000000000000000000, 0.000000000000000000, 0.000000000000000000 ) ) ;
#34138 = DIRECTION ( 'NONE',  ( -0.000000000000000000, -1.000000000000000000, -0.000000000000000000 ) ) ;
#34139 = CARTESIAN_POINT ( 'NONE',  ( 0.000000000000000000, 21.60688246758696707, -79.10210256391346206 ) ) ;
#34140 = CARTESIAN_POINT ( 'NONE',  ( -94.99999999999997158, -206.9400435732949575, 77.77624999999999034 ) ) ;
#34141 = ORIENTED_EDGE ( 'NONE', *, *, #1674, .F. ) ;
#34142 = DIRECTION ( 'NONE',  ( 0.000000000000000000, 0.5877852522924689183, -0.8090169943749504489 ) ) ;
#34143 = EDGE_CURVE ( 'NONE', #51953, #47366, #59554, .T. ) ;
#34144 = CARTESIAN_POINT ( 'NONE',  ( -97.30629616937497417, -208.6684592857803011, 78.79489583420047438 ) ) ;
#34145 = VECTOR ( 'NONE', #62348, 1000.000000000000000 ) ;
#34146 = ORIENTED_EDGE ( 'NONE', *, *, #68358, .F. ) ;
#34147 = ORIENTED_EDGE ( 'NONE', *, *, #29887, .T. ) ;
#34148 = FACE_BOUND ( 'NONE', #62057, .T. ) ;
#34149 = ORIENTED_EDGE ( 'NONE', *, *, #29627, .T. ) ;
#34150 = EDGE_CURVE ( 'NONE', #54409, #24772, #23043, .T. ) ;
#34151 = DIRECTION ( 'NONE',  ( 0.000000000000000000, 0.000000000000000000, 1.000000000000000000 ) ) ;
#34152 = AXIS2_PLACEMENT_3D ( 'NONE', #13117, #36055, #59000 ) ;
#34153 = CARTESIAN_POINT ( 'NONE',  ( 10.00000000000000000, -37.58145647212455032, 0.6853352020789044152 ) ) ;
#34154 = ORIENTED_EDGE ( 'NONE', *, *, #38786, .T. ) ;
#34155 = CARTESIAN_POINT ( 'NONE',  ( -97.30629616937495996, -209.9999999999999716, 76.94281250086713442 ) ) ;
#34156 = ORIENTED_EDGE ( 'NONE', *, *, #12984, .F. ) ;
#34157 = VECTOR ( 'NONE', #74124, 1000.000000000000114 ) ;
#34158 = DIRECTION ( 'NONE',  ( 0.000000000000000000, 0.000000000000000000, 1.000000000000000000 ) ) ;
#34159 = CARTESIAN_POINT ( 'NONE',  ( 11.99999999999999822, -46.21855187248673502, 62.20884554314003623 ) ) ;
#34160 = CARTESIAN_POINT ( 'NONE',  ( 92.35000000003358878, -210.0000076551254153, 78.01464417100928017 ) ) ;
#34161 = CARTESIAN_POINT ( 'NONE',  ( 100.0010000000000190, -115.9999999999999716, -40.00000000000002132 ) ) ;
#34162 = EDGE_CURVE ( 'NONE', #60745, #60196, #18131, .T. ) ;
#34163 = CYLINDRICAL_SURFACE ( 'NONE', #22252, 82.00000000000000000 ) ;
#34164 = CIRCLE ( 'NONE', #1782, 5.000000000000000000 ) ;
#34165 = CIRCLE ( 'NONE', #53367, 15.99999999999999467 ) ;
#34166 = FACE_OUTER_BOUND ( 'NONE', #61, .T. ) ;
#34167 = CARTESIAN_POINT ( 'NONE',  ( 97.30629616937498838, 88.66845928578035796, 85.46239583420044994 ) ) ;
#34168 = CARTESIAN_POINT ( 'NONE',  ( 5.000000000000002665, 81.34940948281337114, 10.30890764327411979 ) ) ;
#34169 = PLANE ( 'NONE',  #61414 ) ;
#34170 = AXIS2_PLACEMENT_3D ( 'NONE', #64688, #41745, #1942 ) ;
#34171 = DIRECTION ( 'NONE',  ( 0.000000000000000000, -0.5877852522924624790, -0.8090169943749551118 ) ) ;
#34172 = DIRECTION ( 'NONE',  ( -1.000000000000000000, -0.000000000000000000, -0.000000000000000000 ) ) ;
#34173 = DIRECTION ( 'NONE',  ( 0.000000000000000000, 1.000000000000000000, -1.625241993126352398E-15 ) ) ;
#34174 = CARTESIAN_POINT ( 'NONE',  ( -97.64999999980591383, 89.99998015682162134, 84.36502760998403971 ) ) ;
#34175 = LINE ( 'NONE', #69494, #19477 ) ;
#34176 = VECTOR ( 'NONE', #46, 1000.000000000000000 ) ;
#34177 = CARTESIAN_POINT ( 'NONE',  ( -5.000000000000000000, 2.886751345948137981, -5.553418012614792509 ) ) ;
#34178 = CARTESIAN_POINT ( 'NONE',  ( 0.000000000000000000, 14.66109333815564852, -73.73191006444555740 ) ) ;
#34179 = AXIS2_PLACEMENT_3D ( 'NONE', #73240, #21742, #42928 ) ;
#34180 = LINE ( 'NONE', #16897, #14515 ) ;
#34181 = DIRECTION ( 'NONE',  ( 0.000000000000000000, 0.8090169943749438985, -0.5877852522924780221 ) ) ;
#34182 = LINE ( 'NONE', #753, #1199 ) ;
#34183 = CARTESIAN_POINT ( 'NONE',  ( -93.67499999999998295, -212.2949673200287179, 83.22666666666665947 ) ) ;
#34184 = CARTESIAN_POINT ( 'NONE',  ( -22.53294031248082163, -134.0273518838794757, 5.500000000000000000 ) ) ;
#34185 = ORIENTED_EDGE ( 'NONE', *, *, #47515, .T. ) ;
#34186 = DIRECTION ( 'NONE',  ( -1.000000000000000000, -0.000000000000000000, 0.000000000000000000 ) ) ;
#34187 = DIRECTION ( 'NONE',  ( -1.000000000000000000, 0.000000000000000000, 0.000000000000000000 ) ) ;
#34188 = DIRECTION ( 'NONE',  ( 0.000000000000000000, 0.9945218953682740670, 0.1045284632676459352 ) ) ;
#34189 = EDGE_CURVE ( 'NONE', #9567, #15614, #45679, .T. ) ;
#34190 = AXIS2_PLACEMENT_3D ( 'NONE', #31799, #55110, #26537 ) ;
#34191 = CARTESIAN_POINT ( 'NONE',  ( 97.30629616937498838, -211.3315407142195852, 84.35114583420049428 ) ) ;
#34192 = ADVANCED_FACE ( 'NONE', ( #46332 ), #150, .T. ) ;
#34193 = ORIENTED_EDGE ( 'NONE', *, *, #68089, .F. ) ;
#34194 = EDGE_CURVE ( 'NONE', #68106, #45130, #16845, .T. ) ;
#34195 = ORIENTED_EDGE ( 'NONE', *, *, #9136, .F. ) ;
#34196 = EDGE_CURVE ( 'NONE', #69865, #23551, #30139, .T. ) ;
#34197 = DIRECTION ( 'NONE',  ( -0.000000000000000000, -0.000000000000000000, -1.000000000000000000 ) ) ;
#34198 = ORIENTED_EDGE ( 'NONE', *, *, #55949, .F. ) ;
#34199 = CARTESIAN_POINT ( 'NONE',  ( 0.000000000000000000, 35.95386929396256903, -10.96151621346501237 ) ) ;
#34200 = CARTESIAN_POINT ( 'NONE',  ( 95.00000000000000000, -212.6630814284392557, 77.73656250086713726 ) ) ;
#34201 = VECTOR ( 'NONE', #43636, 1000.000000000000000 ) ;
#34202 = VERTEX_POINT ( 'NONE', #2725 ) ;
#34203 = CARTESIAN_POINT ( 'NONE',  ( 97.30629616937498838, -209.9999999999999716, 83.76906250086716454 ) ) ;
#34204 = VERTEX_POINT ( 'NONE', #54557 ) ;
#34205 = DIRECTION ( 'NONE',  ( -0.6516173805718067369, 0.7585478161175716050, 0.000000000000000000 ) ) ;
#34206 = ORIENTED_EDGE ( 'NONE', *, *, #27240, .F. ) ;
#34207 = AXIS2_PLACEMENT_3D ( 'NONE', #70791, #41860, #36583 ) ;
#34208 = ORIENTED_EDGE ( 'NONE', *, *, #25229, .T. ) ;
#34209 = EDGE_CURVE ( 'NONE', #36728, #18118, #31213, .T. ) ;
#34210 = DIRECTION ( 'NONE',  ( -1.000000000000000000, -0.000000000000000000, -0.000000000000000000 ) ) ;
#34211 = ORIENTED_EDGE ( 'NONE', *, *, #29282, .F. ) ;
#34212 = CARTESIAN_POINT ( 'NONE',  ( 97.65000000000009095, 91.52997821335247863, 85.92541666666664923 ) ) ;
#34213 = CARTESIAN_POINT ( 'NONE',  ( 97.64999999999997726, -211.5299782133524502, 85.26395833506762756 ) ) ;
#34214 = ADVANCED_FACE ( 'NONE', ( #3450 ), #3086, .F. ) ;
#34215 = VERTEX_POINT ( 'NONE', #49280 ) ;
#34216 = LINE ( 'NONE', #56791, #21376 ) ;
#34217 = VERTEX_POINT ( 'NONE', #42541 ) ;
#34218 = DIRECTION ( 'NONE',  ( -1.000000000000000000, -0.000000000000000000, 0.000000000000000000 ) ) ;
#34219 = EDGE_LOOP ( 'NONE', ( #20125, #21720, #71820, #527 ) ) ;
#34220 = VECTOR ( 'NONE', #73523, 1000.000000000000000 ) ;
#34221 = ORIENTED_EDGE ( 'NONE', *, *, #13300, .F. ) ;
#34222 = ORIENTED_EDGE ( 'NONE', *, *, #63245, .F. ) ;
#34223 = DIRECTION ( 'NONE',  ( 0.7273375899149812085, -0.6862798483830533369, 0.000000000000000000 ) ) ;
#34224 = EDGE_CURVE ( 'NONE', #73310, #46312, #26435, .T. ) ;
#34225 = EDGE_CURVE ( 'NONE', #69166, #29201, #37243, .T. ) ;
#34226 = CARTESIAN_POINT ( 'NONE',  ( 10.00000000000000000, -17.80606268964563554, 33.00180498840040855 ) ) ;
#34227 = ORIENTED_EDGE ( 'NONE', *, *, #43068, .T. ) ;
#34228 = VERTEX_POINT ( 'NONE', #1983 ) ;
#34229 = AXIS2_PLACEMENT_3D ( 'NONE', #30273, #70478, #64878 ) ;
#34230 = ORIENTED_EDGE ( 'NONE', *, *, #879, .F. ) ;
#34231 = DIRECTION ( 'NONE',  ( 0.000000000000000000, -0.8090169943749403458, -0.5877852522924830181 ) ) ;
#34232 = CARTESIAN_POINT ( 'NONE',  ( 10.00000000000000000, -37.58145647212455032, 0.6853352020789044152 ) ) ;
#34233 = CARTESIAN_POINT ( 'NONE',  ( -96.32500000000001705, 87.70503267997129626, 88.20083333333332121 ) ) ;
#34234 = ORIENTED_EDGE ( 'NONE', *, *, #17879, .T. ) ;
#34235 = EDGE_CURVE ( 'NONE', #44854, #29642, #529, .T. ) ;
#34236 = CARTESIAN_POINT ( 'NONE',  ( 97.30629616937498838, 90.00000000000002842, 74.72031250086713783 ) ) ;
#34237 = ORIENTED_EDGE ( 'NONE', *, *, #72299, .T. ) ;
#34238 = CARTESIAN_POINT ( 'NONE',  ( 10.00000000000000000, 0.000000000000000000, 0.000000000000000000 ) ) ;
#34239 = CARTESIAN_POINT ( 'NONE',  ( -97.30629616937497417, -211.3315407142195852, 84.61572916753380014 ) ) ;
#34240 = EDGE_LOOP ( 'NONE', ( #3977, #70500, #35436, #16001 ) ) ;
#34241 = DIRECTION ( 'NONE',  ( 0.000000000000000000, 0.1564344650402311743, -0.9876883405951376593 ) ) ;
#34242 = FACE_OUTER_BOUND ( 'NONE', #20046, .T. ) ;
#34243 = CARTESIAN_POINT ( 'NONE',  ( 10.00000000000000000, 39.04073710021344112, 15.48615015657596317 ) ) ;
#34244 = CARTESIAN_POINT ( 'NONE',  ( -92.69370383062498320, -209.9999999999999716, 77.26031250086714408 ) ) ;
#34245 = CARTESIAN_POINT ( 'NONE',  ( -92.35000000000003695, 89.99999989488615881, 86.58687499784845443 ) ) ;
#34246 = DIRECTION ( 'NONE',  ( -0.000000000000000000, -0.000000000000000000, 1.000000000000000000 ) ) ;
#34247 = AXIS2_PLACEMENT_3D ( 'NONE', #36622, #71190, #8797 ) ;
#34248 = CARTESIAN_POINT ( 'NONE',  ( 10.00000000000000000, 0.000000000000000000, 0.000000000000000000 ) ) ;
#34249 = CARTESIAN_POINT ( 'NONE',  ( 0.000000000000000000, -17.67226234102849958, 33.17418723428301774 ) ) ;
#34250 = LINE ( 'NONE', #24100, #17579 ) ;
#34251 = CARTESIAN_POINT ( 'NONE',  ( -97.30629616937501680, 91.33154071421968467, 78.79489583420047438 ) ) ;
#34252 = DIRECTION ( 'NONE',  ( -1.000000000000000000, 0.000000000000000000, -0.000000000000000000 ) ) ;
#34253 = DIRECTION ( 'NONE',  ( 1.000000000000000000, 0.000000000000000000, 0.000000000000000000 ) ) ;
#34254 = AXIS2_PLACEMENT_3D ( 'NONE', #47980, #32427, #55742 ) ;
#34255 = EDGE_LOOP ( 'NONE', ( #10334, #34492, #37546, #4944 ) ) ;
#34256 = AXIS2_PLACEMENT_3D ( 'NONE', #51517, #28955, #24075 ) ;
#34258 = CARTESIAN_POINT ( 'NONE',  ( 0.000000000000000000, 69.42325613327489009, -34.44570377933524696 ) ) ;
#34257 = AXIS2_PLACEMENT_3D ( 'NONE', #61503, #33660, #56229 ) ;
#34259 = FACE_OUTER_BOUND ( 'NONE', #41497, .T. ) ;
#34260 = DIRECTION ( 'NONE',  ( 0.000000000000000000, -0.1564344650402380854, 0.9876883405951365491 ) ) ;
#34261 = DIRECTION ( 'NONE',  ( -1.000000000000000000, -0.000000000000000000, -0.000000000000000000 ) ) ;
#34262 = FACE_OUTER_BOUND ( 'NONE', #1180, .T. ) ;
#34263 = CARTESIAN_POINT ( 'NONE',  ( -94.99999999999997158, -212.6630814284392557, 80.43531250086715545 ) ) ;
#34264 = AXIS2_PLACEMENT_3D ( 'NONE', #68669, #11501, #1388 ) ;
#34265 = CARTESIAN_POINT ( 'NONE',  ( 10.00000000000000000, 75.16055320797059380, -18.89407956138177269 ) ) ;
#34266 = EDGE_LOOP ( 'NONE', ( #41255, #38110, #34496, #39715 ) ) ;
#34267 = CARTESIAN_POINT ( 'NONE',  ( 70.53423027509757048, -217.0820393249931044, -5.500000000000000000 ) ) ;
#34268 = AXIS2_PLACEMENT_3D ( 'NONE', #25370, #9555, #65976 ) ;
#34269 = CARTESIAN_POINT ( 'NONE',  ( 93.67499999999998295, 92.29496732002878900, 76.63854166840096127 ) ) ;
#34270 = LINE ( 'NONE', #62500, #63395 ) ;
#34271 = DIRECTION ( 'NONE',  ( 0.000000000000000000, 0.000000000000000000, 1.000000000000000000 ) ) ;
#34272 = EDGE_CURVE ( 'NONE', #70197, #24794, #66223, .T. ) ;
#34273 = EDGE_CURVE ( 'NONE', #8568, #37924, #46853, .T. ) ;
#34274 = AXIS2_PLACEMENT_3D ( 'NONE', #12914, #30576, #58796 ) ;
#34275 = FACE_OUTER_BOUND ( 'NONE', #218, .T. ) ;
#34276 = VERTEX_POINT ( 'NONE', #31981 ) ;
#34277 = EDGE_CURVE ( 'NONE', #47282, #56810, #15605, .T. ) ;
#34278 = DIRECTION ( 'NONE',  ( -0.9435911131814395114, 0.3311129884571304971, 0.000000000000000000 ) ) ;
#34279 = CARTESIAN_POINT ( 'NONE',  ( 9.984461079971730157, -95.40710393340120277, 2.500000000000000000 ) ) ;
#34280 = ORIENTED_EDGE ( 'NONE', *, *, #29009, .T. ) ;
#34281 =( BOUNDED_SURFACE ( )  B_SPLINE_SURFACE ( 1, 2, ( 
 ( #41413, #35404, #47065, #48163, #64720, #6825, #29737, #7933, #36134, #52693, #59083, #24134, #64354, #12827, #19212, #69967, #42162, #65466, #35753, #30849, #7202, #25237, #70329, #65096, #71073, #13930, #47785, #19575, #58704, #42523, #7571, #36871, #59820, #49263, #65827, #21418, #20695, #61666, #61300, #66921, #4167, #9409, #66570, #48888, #54906, #42900, #72188, #43647, #32336, #27437, #71444, #54539, #10153, #19943, #9044, #60201, #3068, #25963, #9788, #15050, #15415, #26694, #15803, #27064, #14314, #37261, #4539, #8684, #31964, #31595, #71812, #44377, #44007, #43283, #14682, #60919, #32701, #20325, #37988, #66206, #33076, #55279, #55647, #3428, #26336, #56019, #67304, #37630, #60566, #49995, #38363, #3799, #49621, #21057, #72551, #38738, #72914, #68434, #34566, #10908, #51122, #51867, #63169, #6387, #56778, #49, #16537, #22941, #22186, #45881, #410, #45127, #68802, #57885, #34203, #62807, #4916, #50374, #74046, #46231, #73295, #50745, #68046, #17283, #63532, #62431, #40217, #21808, #45503, #33831, #5287, #44756, #56409, #57514, #28188, #11626, #62044, #6027, #39484, #69165, #67679, #12009, #22557, #28929, #16922, #11269, #23303, #57150, #17655, #40587, #39860, #5656, #16168, #73670, #34945, #39107, #10521, #28549, #51488, #33446, #27816, #30397, #59729, #65004, #48075, #70985, #24046, #47698, #59357, #775, #35667, #1147, #69524, #13486, #7484, #53708, #1517, #12372, #36046, #46969, #12739, #58606, #7107, #13841, #41686, #36410, #24767, #70608, #13109, #1880, #7846, #30761, #2249, #19125, #19487, #25144, #58992, #52230, #53341, #18025, #24400, #42073, #42438, #40965, #65375, #52592, #30031, #36783, #29289, #23660, #35317, #46596, #18749, #63901, #58245, #6744, #52975, #29650, #69882, #18378, #41325, #64266, #64624, #47335, #70240, #72469, #32240, #60478, #43924, #43192, #54449, #4081, #66844, #2625, #32617, #55562, #38269, #61212, #72102, #49175, #26609, #8593, #26236, #72828, #71723, #20224, #20610, #60836, #48436, #44284, #21330, #19856, #49543, #8958, #43565, #55190, #31508, #31140, #37170, #9701, #31876, #15715, #8209, #20972, #54820, #67213, #3346, #38650, #2979, #25872, #9318, #54094, #3715, #26978, #48804, #15327, #66118, #49908, #14591, #25505, #71351, #42806, #14967, #66481, #37543, #65736, #37906 ),
 ( #14216, #60115, #67959, #51779, #34479, #50280, #73210, #22850, #5568, #73583, #68338, #11182, #39769, #11543, #68713, #5195, #45791, #22096, #62334, #63085, #74337, #17561, #16454, #34112, #27731, #57059, #33355, #28464, #57422, #56313, #51397, #69074, #45413, #73956, #16082, #61581, #10818, #5934, #10065, #61953, #4830, #17199, #324, #45035, #40129, #32986, #56689, #39394, #33744, #55933, #67588, #28843, #28097, #23218, #21716, #46145, #50655, #4450, #27348, #44671, #51035, #39018, #22470, #16831, #10436, #62716, #19034, #7401, #69798, #47250, #70903, #63813, #30314, #53258, #63444, #1058, #24319, #46887, #29940, #18296, #34856, #64916, #64181, #30677, #1795, #35955, #47612, #52890, #35585, #17933, #23950, #11913, #41237, #12653, #1435, #40495, #57796, #23572, #53620, #6299, #52501, #29198, #46505, #69434, #24680, #58520, #58906, #70157, #59271, #70520, #52141, #685, #47991, #40877, #7015, #12284, #35222, #13398, #13021, #58156, #6655, #36327, #29562, #64541, #18661, #41600, #25051, #41985, #7765, #2164, #32533, #8873, #15247, #3627, #25429, #2896, #49459, #42719, #2545, #72383, #3989, #31787, #8123, #60391, #9233, #43482, #71642, #55101, #54368, #65652, #38180, #26526, #13763, #43841, #66758, #20887, #61126, #54734, #3260, #37825, #19770, #37461, #9616, #8508, #31428, #26151, #72013, #59640, #55478, #26893, #31052, #60755, #20138, #49089, #66399, #14125, #42352, #48351, #49821, #43102, #19404, #65291, #32155, #66030, #36699, #14503, #54005, #37076, #60026, #20523, #71265, #14881, #25790, #48720, #68248, #61865, #16745, #10350, #73869, #11099, #68626, #5108, #56604, #73123, #39681, #44580, #33265, #15988, #22378, #28751, #34021, #17110, #40040, #67501, #62622, #28377, #44198, #4741, #38931, #38561, #56971, #50946, #22764, #44950, #55848, #28006, #56222, #27643, #50568, #73497, #57331, #10729, #5479, #51308, #74241, #45323, #45700, #62999, #11458, #34390, #5842, #72743, #21243, #67124, #15629, #61497, #9975, #67872, #32895, #4359, #27257, #50187, #21627, #22004, #16363, #39306, #62238, #33651, #40403, #1347, #596, #58069, #36242, #30231, #18941, #34771, #64831, #41154, #47531, #35862, #57707, #35136, #7312, #23487, #6215, #53172, #59185, #64094, #63352, #18213, #41517, #24239, #29477, #12928, #12195, #46419, #70435 ) ),
 .UNSPECIFIED., .F., .F., .F. ) 
 B_SPLINE_SURFACE_WITH_KNOTS ( ( 2, 2 ),
 ( 3, 2, 2, 2, 2, 2, 2, 2, 2, 2, 2, 2, 2, 2, 2, 2, 2, 2, 2, 2, 2, 2, 2, 2, 2, 2, 2, 2, 2, 2, 2, 2, 2, 2, 2, 2, 2, 2, 2, 2, 2, 2, 2, 2, 2, 2, 2, 2, 2, 2, 2, 2, 2, 2, 2, 2, 2, 2, 2, 2, 2, 2, 2, 2, 2, 2, 2, 2, 2, 2, 2, 2, 2, 2, 2, 2, 2, 2, 2, 2, 2, 2, 2, 2, 2, 2, 2, 2, 2, 2, 2, 2, 2, 2, 2, 2, 2, 2, 2, 2, 2, 2, 2, 2, 2, 2, 2, 2, 2, 2, 2, 2, 2, 2, 2, 2, 2, 2, 2, 2, 2, 2, 2, 2, 2, 2, 2, 2, 2, 2, 2, 2, 2, 2, 2, 2, 2, 2, 2, 2, 2, 2, 2, 3 ),
 ( 0.000000000000000000, 1.000000000000000000 ),
 ( 0.000000000000000000, 0.006944444444444444059, 0.01388888888888888812, 0.02083333333333333218, 0.02777777777777777624, 0.03472222222222222376, 0.04166666666666666435, 0.04861111111111111188, 0.05555555555555555247, 0.06250000000000000000, 0.06944444444444444753, 0.07638888888888889506, 0.08333333333333332871, 0.09027777777777777624, 0.09722222222222222376, 0.1041666666666666713, 0.1111111111111111049, 0.1180555555555555525, 0.1250000000000000000, 0.1319444444444444475, 0.1388888888888888951, 0.1458333333333333426, 0.1527777777777777901, 0.1597222222222222099, 0.1666666666666666574, 0.1736111111111111049, 0.1805555555555555525, 0.1875000000000000000, 0.1944444444444444475, 0.2013888888888888951, 0.2083333333333333426, 0.2152777777777777901, 0.2222222222222222099, 0.2291666666666666574, 0.2361111111111111049, 0.2430555555555555525, 0.2500000000000000000, 0.2569444444444444198, 0.2638888888888888951, 0.2708333333333333148, 0.2777777777777777901, 0.2847222222222222099, 0.2916666666666666852, 0.2986111111111111049, 0.3055555555555555802, 0.3125000000000000000, 0.3194444444444444198, 0.3263888888888888951, 0.3333333333333333148, 0.3402777777777777901, 0.3472222222222222099, 0.3541666666666666852, 0.3611111111111111049, 0.3680555555555555802, 0.3750000000000000000, 0.3819444444444444198, 0.3888888888888888951, 0.3958333333333333148, 0.4027777777777777901, 0.4097222222222222099, 0.4166666666666666852, 0.4236111111111111049, 0.4305555555555555802, 0.4375000000000000000, 0.4444444444444444198, 0.4513888888888888951, 0.4583333333333333148, 0.4652777777777777901, 0.4722222222222222099, 0.4791666666666666852, 0.4861111111111111049, 0.4930555555555555802, 0.5000000000000000000, 0.5069444444444444198, 0.5138888888888888395, 0.5208333333333333703, 0.5277777777777777901, 0.5347222222222222099, 0.5416666666666666297, 0.5486111111111111605, 0.5555555555555555802, 0.5625000000000000000, 0.5694444444444444198, 0.5763888888888888395, 0.5833333333333333703, 0.5902777777777777901, 0.5972222222222222099, 0.6041666666666666297, 0.6111111111111111605, 0.6180555555555555802, 0.6250000000000000000, 0.6319444444444444198, 0.6388888888888888395, 0.6458333333333333703, 0.6527777777777777901, 0.6597222222222222099, 0.6666666666666666297, 0.6736111111111111605, 0.6805555555555555802, 0.6875000000000000000, 0.6944444444444444198, 0.7013888888888888395, 0.7083333333333333703, 0.7152777777777777901, 0.7222222222222222099, 0.7291666666666666297, 0.7361111111111111605, 0.7430555555555555802, 0.7500000000000000000, 0.7569444444444444198, 0.7638888888888888395, 0.7708333333333333703, 0.7777777777777777901, 0.7847222222222222099, 0.7916666666666666297, 0.7986111111111111605, 0.8055555555555555802, 0.8125000000000000000, 0.8194444444444444198, 0.8263888888888888395, 0.8333333333333333703, 0.8402777777777777901, 0.8472222222222222099, 0.8541666666666666297, 0.8611111111111111605, 0.8680555555555555802, 0.8750000000000000000, 0.8819444444444444198, 0.8888888888888888395, 0.8958333333333333703, 0.9027777777777777901, 0.9097222222222222099, 0.9166666666666666297, 0.9236111111111111605, 0.9305555555555555802, 0.9375000000000000000, 0.9444444444444444198, 0.9513888888888888395, 0.9583333333333333703, 0.9652777777777777901, 0.9722222222222222099, 0.9791666666666666297, 0.9842226772312638872, 0.9940649040035764994 ),
 .UNSPECIFIED. ) 
 GEOMETRIC_REPRESENTATION_ITEM ( )  RATIONAL_B_SPLINE_SURFACE ( (
 ( 1.000000000000000000, 0.8660254037844387076, 1.000000000000000000, 0.8660254037844387076, 1.000000000000000000, 0.8660254037844387076, 1.000000000000000000, 0.8660254037844387076, 1.000000000000000000, 0.8660254037844387076, 1.000000000000000000, 0.8660254037844387076, 1.000000000000000000, 0.8660254037844387076, 1.000000000000000000, 0.8660254037844387076, 1.000000000000000000, 0.8660254037844387076, 1.000000000000000000, 0.8660254037844387076, 1.000000000000000000, 0.8660254037844387076, 1.000000000000000000, 0.8660254037844387076, 1.000000000000000000, 0.8660254037844387076, 1.000000000000000000, 0.8660254037844387076, 1.000000000000000000, 0.8660254037844387076, 1.000000000000000000, 0.8660254037844387076, 1.000000000000000000, 0.8660254037844387076, 1.000000000000000000, 0.8660254037844387076, 1.000000000000000000, 0.8660254037844387076, 1.000000000000000000, 0.8660254037844387076, 1.000000000000000000, 0.8660254037844387076, 1.000000000000000000, 0.8660254037844387076, 1.000000000000000000, 0.8660254037844387076, 1.000000000000000000, 0.8660254037844387076, 1.000000000000000000, 0.8660254037844387076, 1.000000000000000000, 0.8660254037844387076, 1.000000000000000000, 0.8660254037844387076, 1.000000000000000000, 0.8660254037844387076, 1.000000000000000000, 0.8660254037844387076, 1.000000000000000000, 0.8660254037844387076, 1.000000000000000000, 0.8660254037844387076, 1.000000000000000000, 0.8660254037844387076, 1.000000000000000000, 0.8660254037844387076, 1.000000000000000000, 0.8660254037844387076, 1.000000000000000000, 0.8660254037844387076, 1.000000000000000000, 0.8660254037844387076, 1.000000000000000000, 0.8660254037844387076, 1.000000000000000000, 0.8660254037844387076, 1.000000000000000000, 0.8660254037844387076, 1.000000000000000000, 0.8660254037844387076, 1.000000000000000000, 0.8660254037844387076, 1.000000000000000000, 0.8660254037844387076, 1.000000000000000000, 0.8660254037844387076, 1.000000000000000000, 0.8660254037844387076, 1.000000000000000000, 0.8660254037844387076, 1.000000000000000000, 0.8660254037844387076, 1.000000000000000000, 0.8660254037844387076, 1.000000000000000000, 0.8660254037844387076, 1.000000000000000000, 0.8660254037844387076, 1.000000000000000000, 0.8660254037844387076, 1.000000000000000000, 0.8660254037844387076, 1.000000000000000000, 0.8660254037844387076, 1.000000000000000000, 0.8660254037844387076, 1.000000000000000000, 0.8660254037844387076, 1.000000000000000000, 0.8660254037844387076, 1.000000000000000000, 0.8660254037844387076, 1.000000000000000000, 0.8660254037844387076, 1.000000000000000000, 0.8660254037844387076, 1.000000000000000000, 0.8660254037844387076, 1.000000000000000000, 0.8660254037844387076, 1.000000000000000000, 0.8660254037844387076, 1.000000000000000000, 0.8660254037844387076, 1.000000000000000000, 0.8660254037844387076, 1.000000000000000000, 0.8660254037844387076, 1.000000000000000000, 0.8660254037844387076, 1.000000000000000000, 0.8660254037844387076, 1.000000000000000000, 0.8660254037844387076, 1.000000000000000000, 0.8660254037844387076, 1.000000000000000000, 0.8660254037844387076, 1.000000000000000000, 0.8660254037844387076, 1.000000000000000000, 0.8660254037844387076, 1.000000000000000000, 0.8660254037844387076, 1.000000000000000000, 0.8660254037844387076, 1.000000000000000000, 0.8660254037844387076, 1.000000000000000000, 0.8660254037844387076, 1.000000000000000000, 0.8660254037844387076, 1.000000000000000000, 0.8660254037844387076, 1.000000000000000000, 0.8660254037844387076, 1.000000000000000000, 0.8660254037844387076, 1.000000000000000000, 0.8660254037844387076, 1.000000000000000000, 0.8660254037844387076, 1.000000000000000000, 0.8660254037844387076, 1.000000000000000000, 0.8660254037844387076, 1.000000000000000000, 0.8660254037844387076, 1.000000000000000000, 0.8660254037844387076, 1.000000000000000000, 0.8660254037844387076, 1.000000000000000000, 0.8660254037844387076, 1.000000000000000000, 0.8660254037844387076, 1.000000000000000000, 0.8660254037844387076, 1.000000000000000000, 0.8660254037844387076, 1.000000000000000000, 0.8660254037844387076, 1.000000000000000000, 0.8660254037844387076, 1.000000000000000000, 0.8660254037844387076, 1.000000000000000000, 0.8660254037844387076, 1.000000000000000000, 0.8660254037844387076, 1.000000000000000000, 0.8660254037844387076, 1.000000000000000000, 0.8660254037844387076, 1.000000000000000000, 0.8660254037844387076, 1.000000000000000000, 0.8660254037844387076, 1.000000000000000000, 0.8660254037844387076, 1.000000000000000000, 0.8660254037844387076, 1.000000000000000000, 0.8660254037844387076, 1.000000000000000000, 0.8660254037844387076, 1.000000000000000000, 0.8660254037844387076, 1.000000000000000000, 0.8660254037844387076, 1.000000000000000000, 0.8660254037844387076, 1.000000000000000000, 0.8660254037844387076, 1.000000000000000000, 0.8660254037844387076, 1.000000000000000000, 0.8660254037844387076, 1.000000000000000000, 0.8660254037844387076, 1.000000000000000000, 0.8660254037844387076, 1.000000000000000000, 0.8660254037844387076, 1.000000000000000000, 0.8660254037844387076, 1.000000000000000000, 0.8660254037844387076, 1.000000000000000000, 0.8660254037844387076, 1.000000000000000000, 0.8660254037844387076, 1.000000000000000000, 0.8660254037844387076, 1.000000000000000000, 0.8660254037844387076, 1.000000000000000000, 0.8660254037844387076, 1.000000000000000000, 0.8660254037844387076, 1.000000000000000000, 0.8660254037844387076, 1.000000000000000000, 0.8660254037844387076, 1.000000000000000000, 0.8660254037844387076, 1.000000000000000000, 0.8660254037844387076, 1.000000000000000000, 0.8660254037844387076, 1.000000000000000000, 0.8660254037844387076, 1.000000000000000000, 0.8660254037844387076, 1.000000000000000000, 0.8660254037844387076, 1.000000000000000000, 0.8660254037844387076, 1.000000000000000000, 0.8660254037844387076, 1.000000000000000000, 0.8660254037844387076, 1.000000000000000000, 0.8660254037844387076, 1.000000000000000000, 0.8660254037844387076, 1.000000000000000000, 0.8660254037844387076, 1.000000000000000000, 0.8660254037844387076, 1.000000000000000000, 0.8660254037844387076, 1.000000000000000000, 0.8660254037844387076, 1.000000000000000000, 0.8660254037844387076, 1.000000000000000000, 0.8660254037844387076, 1.000000000000000000, 0.8660254037844387076, 1.000000000000000000, 0.8660254037844387076, 1.000000000000000000, 0.9024577157650929271, 0.9469497795711361299, 0.9469497795711361299, 0.9469497795711361299),
 ( 1.000000000000000000, 0.8660254037844387076, 1.000000000000000000, 0.8660254037844387076, 1.000000000000000000, 0.8660254037844387076, 1.000000000000000000, 0.8660254037844387076, 1.000000000000000000, 0.8660254037844387076, 1.000000000000000000, 0.8660254037844387076, 1.000000000000000000, 0.8660254037844387076, 1.000000000000000000, 0.8660254037844387076, 1.000000000000000000, 0.8660254037844387076, 1.000000000000000000, 0.8660254037844387076, 1.000000000000000000, 0.8660254037844387076, 1.000000000000000000, 0.8660254037844387076, 1.000000000000000000, 0.8660254037844387076, 1.000000000000000000, 0.8660254037844387076, 1.000000000000000000, 0.8660254037844387076, 1.000000000000000000, 0.8660254037844387076, 1.000000000000000000, 0.8660254037844387076, 1.000000000000000000, 0.8660254037844387076, 1.000000000000000000, 0.8660254037844387076, 1.000000000000000000, 0.8660254037844387076, 1.000000000000000000, 0.8660254037844387076, 1.000000000000000000, 0.8660254037844387076, 1.000000000000000000, 0.8660254037844387076, 1.000000000000000000, 0.8660254037844387076, 1.000000000000000000, 0.8660254037844387076, 1.000000000000000000, 0.8660254037844387076, 1.000000000000000000, 0.8660254037844387076, 1.000000000000000000, 0.8660254037844387076, 1.000000000000000000, 0.8660254037844387076, 1.000000000000000000, 0.8660254037844387076, 1.000000000000000000, 0.8660254037844387076, 1.000000000000000000, 0.8660254037844387076, 1.000000000000000000, 0.8660254037844387076, 1.000000000000000000, 0.8660254037844387076, 1.000000000000000000, 0.8660254037844387076, 1.000000000000000000, 0.8660254037844387076, 1.000000000000000000, 0.8660254037844387076, 1.000000000000000000, 0.8660254037844387076, 1.000000000000000000, 0.8660254037844387076, 1.000000000000000000, 0.8660254037844387076, 1.000000000000000000, 0.8660254037844387076, 1.000000000000000000, 0.8660254037844387076, 1.000000000000000000, 0.8660254037844387076, 1.000000000000000000, 0.8660254037844387076, 1.000000000000000000, 0.8660254037844387076, 1.000000000000000000, 0.8660254037844387076, 1.000000000000000000, 0.8660254037844387076, 1.000000000000000000, 0.8660254037844387076, 1.000000000000000000, 0.8660254037844387076, 1.000000000000000000, 0.8660254037844387076, 1.000000000000000000, 0.8660254037844387076, 1.000000000000000000, 0.8660254037844387076, 1.000000000000000000, 0.8660254037844387076, 1.000000000000000000, 0.8660254037844387076, 1.000000000000000000, 0.8660254037844387076, 1.000000000000000000, 0.8660254037844387076, 1.000000000000000000, 0.8660254037844387076, 1.000000000000000000, 0.8660254037844387076, 1.000000000000000000, 0.8660254037844387076, 1.000000000000000000, 0.8660254037844387076, 1.000000000000000000, 0.8660254037844387076, 1.000000000000000000, 0.8660254037844387076, 1.000000000000000000, 0.8660254037844387076, 1.000000000000000000, 0.8660254037844387076, 1.000000000000000000, 0.8660254037844387076, 1.000000000000000000, 0.8660254037844387076, 1.000000000000000000, 0.8660254037844387076, 1.000000000000000000, 0.8660254037844387076, 1.000000000000000000, 0.8660254037844387076, 1.000000000000000000, 0.8660254037844387076, 1.000000000000000000, 0.8660254037844387076, 1.000000000000000000, 0.8660254037844387076, 1.000000000000000000, 0.8660254037844387076, 1.000000000000000000, 0.8660254037844387076, 1.000000000000000000, 0.8660254037844387076, 1.000000000000000000, 0.8660254037844387076, 1.000000000000000000, 0.8660254037844387076, 1.000000000000000000, 0.8660254037844387076, 1.000000000000000000, 0.8660254037844387076, 1.000000000000000000, 0.8660254037844387076, 1.000000000000000000, 0.8660254037844387076, 1.000000000000000000, 0.8660254037844387076, 1.000000000000000000, 0.8660254037844387076, 1.000000000000000000, 0.8660254037844387076, 1.000000000000000000, 0.8660254037844387076, 1.000000000000000000, 0.8660254037844387076, 1.000000000000000000, 0.8660254037844387076, 1.000000000000000000, 0.8660254037844387076, 1.000000000000000000, 0.8660254037844387076, 1.000000000000000000, 0.8660254037844387076, 1.000000000000000000, 0.8660254037844387076, 1.000000000000000000, 0.8660254037844387076, 1.000000000000000000, 0.8660254037844387076, 1.000000000000000000, 0.8660254037844387076, 1.000000000000000000, 0.8660254037844387076, 1.000000000000000000, 0.8660254037844387076, 1.000000000000000000, 0.8660254037844387076, 1.000000000000000000, 0.8660254037844387076, 1.000000000000000000, 0.8660254037844387076, 1.000000000000000000, 0.8660254037844387076, 1.000000000000000000, 0.8660254037844387076, 1.000000000000000000, 0.8660254037844387076, 1.000000000000000000, 0.8660254037844387076, 1.000000000000000000, 0.8660254037844387076, 1.000000000000000000, 0.8660254037844387076, 1.000000000000000000, 0.8660254037844387076, 1.000000000000000000, 0.8660254037844387076, 1.000000000000000000, 0.8660254037844387076, 1.000000000000000000, 0.8660254037844387076, 1.000000000000000000, 0.8660254037844387076, 1.000000000000000000, 0.8660254037844387076, 1.000000000000000000, 0.8660254037844387076, 1.000000000000000000, 0.8660254037844387076, 1.000000000000000000, 0.8660254037844387076, 1.000000000000000000, 0.8660254037844387076, 1.000000000000000000, 0.8660254037844387076, 1.000000000000000000, 0.8660254037844387076, 1.000000000000000000, 0.8660254037844387076, 1.000000000000000000, 0.8660254037844387076, 1.000000000000000000, 0.8660254037844387076, 1.000000000000000000, 0.8660254037844387076, 1.000000000000000000, 0.8660254037844387076, 1.000000000000000000, 0.8660254037844387076, 1.000000000000000000, 0.8660254037844387076, 1.000000000000000000, 0.8660254037844387076, 1.000000000000000000, 0.8660254037844387076, 1.000000000000000000, 0.8660254037844387076, 1.000000000000000000, 0.8660254037844387076, 1.000000000000000000, 0.8660254037844387076, 1.000000000000000000, 0.8660254037844387076, 1.000000000000000000, 0.8660254037844387076, 1.000000000000000000, 0.8660254037844387076, 1.000000000000000000, 0.8660254037844387076, 1.000000000000000000, 0.8660254037844387076, 1.000000000000000000, 0.8660254037844387076, 1.000000000000000000, 0.8660254037844387076, 1.000000000000000000, 0.8660254037844387076, 1.000000000000000000, 0.8660254037844387076, 1.000000000000000000, 0.8660254037844387076, 1.000000000000000000, 0.8660254037844387076, 1.000000000000000000, 0.8660254037844387076, 1.000000000000000000, 0.9024577157650929271, 0.9469497795711361299, 0.9469497795711361299, 0.9469497795711361299) ) ) 
 REPRESENTATION_ITEM ( '' )  SURFACE ( )  );
#34282 = ADVANCED_FACE ( 'NONE', ( #25609 ), #42182, .T. ) ;
#34283 = CARTESIAN_POINT ( 'NONE',  ( 92.69370383062501162, -209.9999999999999716, 89.00781250086714635 ) ) ;
#34284 = CARTESIAN_POINT ( 'NONE',  ( -94.99999999999997158, -206.9400435732949575, 83.57062500173429953 ) ) ;
#34285 = ORIENTED_EDGE ( 'NONE', *, *, #14170, .T. ) ;
#34286 = LINE ( 'NONE', #22275, #897 ) ;
#34287 = ORIENTED_EDGE ( 'NONE', *, *, #12635, .F. ) ;
#34288 = CARTESIAN_POINT ( 'NONE',  ( 10.00000000000000000, -36.13751322684404244, -21.40280677340410165 ) ) ;
#34289 = EDGE_LOOP ( 'NONE', ( #37900, #20628, #48182, #51646 ) ) ;
#34290 = DIRECTION ( 'NONE',  ( -0.000000000000000000, 0.5877852522924696954, 0.8090169943749498938 ) ) ;
#34291 = ORIENTED_EDGE ( 'NONE', *, *, #17918, .T. ) ;
#34292 = DIRECTION ( 'NONE',  ( -1.000000000000000000, 0.000000000000000000, -0.000000000000000000 ) ) ;
#34293 = EDGE_LOOP ( 'NONE', ( #5005, #50393, #57705, #51413 ) ) ;
#34294 = ORIENTED_EDGE ( 'NONE', *, *, #38991, .F. ) ;
#34295 = DIRECTION ( 'NONE',  ( -1.000000000000000000, -0.000000000000000000, 0.000000000000000000 ) ) ;
#34296 = EDGE_CURVE ( 'NONE', #7474, #1262, #59465, .T. ) ;
#34297 = EDGE_CURVE ( 'NONE', #49630, #57628, #55259, .T. ) ;
#34298 = EDGE_LOOP ( 'NONE', ( #27259, #14159, #2573, #14921 ) ) ;
#34299 = VERTEX_POINT ( 'NONE', #60221 ) ;
#34300 = DIRECTION ( 'NONE',  ( 1.000000000000000000, 0.000000000000000000, 0.000000000000000000 ) ) ;
#34302 = CARTESIAN_POINT ( 'NONE',  ( -92.35000000000003695, 89.99999999755290503, 75.15687493081163950 ) ) ;
#34301 = VECTOR ( 'NONE', #74272, 1000.000000000000000 ) ;
#34303 = ORIENTED_EDGE ( 'NONE', *, *, #58654, .F. ) ;
#34304 = ORIENTED_EDGE ( 'NONE', *, *, #61916, .T. ) ;
#34305 = CARTESIAN_POINT ( 'NONE',  ( 94.99999999999998579, 92.66308142843935514, 86.30906250086715659 ) ) ;
#34306 = EDGE_LOOP ( 'NONE', ( #2526, #60106, #61969, #19519 ) ) ;
#34307 = AXIS2_PLACEMENT_3D ( 'NONE', #32903, #56613, #62248 ) ;
#34308 = CARTESIAN_POINT ( 'NONE',  ( 92.69370383062501162, -209.9999999999999716, 82.65781250086713783 ) ) ;
#34309 = EDGE_CURVE ( 'NONE', #34480, #30579, #68480, .T. ) ;
#34310 = EDGE_CURVE ( 'NONE', #35350, #42474, #104, .T. ) ;
#34311 = SHAPE_DEFINITION_REPRESENTATION ( #44618, #23897 ) ;
#34312 = CARTESIAN_POINT ( 'NONE',  ( -96.32499999999996021, -212.2949673200287179, 81.29520833506762756 ) ) ;
#34313 = CARTESIAN_POINT ( 'NONE',  ( -92.35000000000000853, 88.47002178664756400, 84.54958333333334508 ) ) ;
#34314 = AXIS2_PLACEMENT_3D ( 'NONE', #31865, #72456, #47776 ) ;
#34315 = DIRECTION ( 'NONE',  ( -1.000000000000000000, 0.000000000000000000, 0.000000000000000000 ) ) ;
#34316 = PLANE ( 'NONE',  #47574 ) ;
#34317 = VECTOR ( 'NONE', #70477, 1000.000000000000000 ) ;
#34318 = DIRECTION ( 'NONE',  ( -1.000000000000000000, 0.000000000000000000, 0.000000000000000000 ) ) ;
#34319 = CARTESIAN_POINT ( 'NONE',  ( 10.00000000000000000, 0.000000000000000000, 0.000000000000000000 ) ) ;
#34320 = CARTESIAN_POINT ( 'NONE',  ( -92.69370383062498320, -211.3315407142195852, 88.00239583420047040 ) ) ;
#34321 = CARTESIAN_POINT ( 'NONE',  ( -93.84685191531252713, 88.00268892867056536, 85.56822916753381492 ) ) ;
#34322 = VERTEX_POINT ( 'NONE', #42917 ) ;
#34323 = AXIS2_PLACEMENT_3D ( 'NONE', #5794, #49770, #55797 ) ;
#34325 = CARTESIAN_POINT ( 'NONE',  ( -96.15314808468752972, 91.99731107132950569, 85.72697916753379843 ) ) ;
#34324 = CARTESIAN_POINT ( 'NONE',  ( 92.69370383062498320, 90.00000000000002842, 85.83281250086714920 ) ) ;
#34326 = AXIS2_PLACEMENT_3D ( 'NONE', #35081, #36545, #35446 ) ;
#34327 = VERTEX_POINT ( 'NONE', #38751 ) ;
#34328 = LINE ( 'NONE', #5413, #25126 ) ;
#34329 = CARTESIAN_POINT ( 'NONE',  ( 12.00000000000000000, 14.60985201121729737, 18.46759930825687590 ) ) ;
#34330 = CARTESIAN_POINT ( 'NONE',  ( -8.826826895187510402, -94.96827758698185562, -5.500000000000000000 ) ) ;
#34331 = CARTESIAN_POINT ( 'NONE',  ( 92.35000000000000853, 91.52997821335253548, 87.40708333333333258 ) ) ;
#34332 = CARTESIAN_POINT ( 'NONE',  ( -94.99999999999997158, -207.3369185715606307, 87.57906250086713840 ) ) ;
#34333 = CARTESIAN_POINT ( 'NONE',  ( 10.00000000000000000, -71.91182617369167929, -28.89263327155822481 ) ) ;
#34334 = DIRECTION ( 'NONE',  ( 0.000000000000000000, 0.000000000000000000, -1.000000000000000000 ) ) ;
#34335 = CARTESIAN_POINT ( 'NONE',  ( -34.02017708624681092, -109.8571428571428470, 102.9091629284897493 ) ) ;
#34336 = DIRECTION ( 'NONE',  ( 0.000000000000000000, 0.9969173337331276308, 0.07845909572784864894 ) ) ;
#34337 = EDGE_LOOP ( 'NONE', ( #59186, #56480, #33167, #57593 ) ) ;
#34338 = CIRCLE ( 'NONE', #11522, 37.49900000000000233 ) ;
#34339 = ORIENTED_EDGE ( 'NONE', *, *, #12373, .F. ) ;
#34340 = CARTESIAN_POINT ( 'NONE',  ( -95.00000000000002842, 93.05995642670501411, 76.50624999999999432 ) ) ;
#34341 = DIRECTION ( 'NONE',  ( -0.000000000000000000, -0.000000000000000000, 1.000000000000000000 ) ) ;
#34342 = CARTESIAN_POINT ( 'NONE',  ( 93.67500000000001137, -207.7050326799711968, 81.00416666666666288 ) ) ;
#34343 = FACE_BOUND ( 'NONE', #30495, .T. ) ;
#34344 = CARTESIAN_POINT ( 'NONE',  ( 0.000000000000000000, -75.54627589209955829, 17.28742895386058009 ) ) ;
#34345 = DIRECTION ( 'NONE',  ( 0.000000000000000000, 0.9969173337331281859, -0.07845909572784168229 ) ) ;
#34346 = CARTESIAN_POINT ( 'NONE',  ( 11.99999999999999822, -8.840884882374576037, -74.65374052328658649 ) ) ;
#34347 = ORIENTED_EDGE ( 'NONE', *, *, #31834, .T. ) ;
#34348 = CARTESIAN_POINT ( 'NONE',  ( -97.30629616937501680, 90.00000000000004263, 79.48281250086714067 ) ) ;
#34349 = FACE_OUTER_BOUND ( 'NONE', #30718, .T. ) ;
#34350 = DIRECTION ( 'NONE',  ( -1.000000000000000000, 0.000000000000000000, -0.000000000000000000 ) ) ;
#34351 = PLANE ( 'NONE',  #62224 ) ;
#34352 = FACE_OUTER_BOUND ( 'NONE', #20559, .T. ) ;
#34353 = DIRECTION ( 'NONE',  ( 0.000000000000000000, 0.000000000000000000, 1.000000000000000000 ) ) ;
#34354 = CARTESIAN_POINT ( 'NONE',  ( -94.99999999999997158, -209.9999999999999716, 90.00000000000000000 ) ) ;
#34355 = ADVANCED_FACE ( 'NONE', ( #33463 ), #50386, .T. ) ;
#34356 = EDGE_CURVE ( 'NONE', #47902, #1611, #36037, .T. ) ;
#34357 = EDGE_CURVE ( 'NONE', #57544, #33176, #21435, .T. ) ;
#34358 = CIRCLE ( 'NONE', #63206, 15.99999999999999822 ) ;
#34359 = CARTESIAN_POINT ( 'NONE',  ( 94.99999999999998579, 87.33691857156068750, 77.89531250086714920 ) ) ;
#34360 = EDGE_CURVE ( 'NONE', #54220, #19667, #72570, .T. ) ;
#34361 = CARTESIAN_POINT ( 'NONE',  ( -93.84685191531247028, -211.9973110713294489, 80.48822916753381662 ) ) ;
#34362 = CARTESIAN_POINT ( 'NONE',  ( 11.99999999999999822, 0.000000000000000000, 0.000000000000000000 ) ) ;
#34363 = ORIENTED_EDGE ( 'NONE', *, *, #51705, .F. ) ;
#34364 = DIRECTION ( 'NONE',  ( 0.000000000000000000, -0.5877852522924624790, -0.8090169943749550008 ) ) ;
#34365 = DIRECTION ( 'NONE',  ( 0.000000000000000000, -0.8090169943749531134, 0.5877852522924653655 ) ) ;
#34366 = DIRECTION ( 'NONE',  ( 1.000000000000000000, 0.000000000000000000, 0.000000000000000000 ) ) ;
#34367 = VECTOR ( 'NONE', #70737, 1000.000000000000000 ) ;
#34368 = EDGE_CURVE ( 'NONE', #58109, #44775, #50427, .T. ) ;
#34369 = AXIS2_PLACEMENT_3D ( 'NONE', #67277, #4893, #10880 ) ;
#34370 = CARTESIAN_POINT ( 'NONE',  ( -92.69370383062505425, 91.33154071421968467, 74.93197916753381094 ) ) ;
#34371 = CARTESIAN_POINT ( 'NONE',  ( 92.69370383062501162, -211.3315407142195852, 78.90072916753381094 ) ) ;
#34372 = ORIENTED_EDGE ( 'NONE', *, *, #5280, .F. ) ;
#34373 = AXIS2_PLACEMENT_3D ( 'NONE', #24455, #6078, #28980 ) ;
#34374 = DIRECTION ( 'NONE',  ( 0.9827303690289279636, 0.1850432970638681840, 0.000000000000000000 ) ) ;
#34375 = ORIENTED_EDGE ( 'NONE', *, *, #56208, .T. ) ;
#34376 = EDGE_CURVE ( 'NONE', #32419, #22189, #42065, .T. ) ;
#34377 = LINE ( 'NONE', #62984, #20719 ) ;
#34378 = VERTEX_POINT ( 'NONE', #39504 ) ;
#34379 = CARTESIAN_POINT ( 'NONE',  ( -93.67499999999998295, -207.7050326799711968, 83.43833333333333258 ) ) ;
#34380 = AXIS2_PLACEMENT_3D ( 'NONE', #25865, #31133, #60473 ) ;
#34381 = VERTEX_POINT ( 'NONE', #60938 ) ;
#34382 = ORIENTED_EDGE ( 'NONE', *, *, #20442, .F. ) ;
#34383 = VERTEX_POINT ( 'NONE', #3816 ) ;
#34384 = DIRECTION ( 'NONE',  ( -8.119982227976398872E-16, -1.065814103640131188E-14, -1.000000000000000000 ) ) ;
#34385 = ADVANCED_FACE ( 'NONE', ( #28205 ), #68447, .T. ) ;
#34386 = EDGE_CURVE ( 'NONE', #22507, #73223, #21604, .T. ) ;
#34387 = ORIENTED_EDGE ( 'NONE', *, *, #67293, .F. ) ;
#34388 = VERTEX_POINT ( 'NONE', #9430 ) ;
#34389 = CARTESIAN_POINT ( 'NONE',  ( 96.15314808468748708, 91.99731107132950569, 81.96989583420048575 ) ) ;
#34390 = CARTESIAN_POINT ( 'NONE',  ( 92.35000000000002274, -211.5299782133524502, 77.35291666666665833 ) ) ;
#34391 = ORIENTED_EDGE ( 'NONE', *, *, #29797, .T. ) ;
#34392 = ORIENTED_EDGE ( 'NONE', *, *, #70497, .F. ) ;
#34393 = EDGE_LOOP ( 'NONE', ( #26979, #58089, #30136, #64360, #20429 ) ) ;
#34394 = VERTEX_POINT ( 'NONE', #16184 ) ;
#34395 = CARTESIAN_POINT ( 'NONE',  ( 11.99999999999999822, -56.15606465354916566, -59.75363087400133111 ) ) ;
#34396 = DIRECTION ( 'NONE',  ( -0.7533909544171990547, -0.6575728627325962972, -1.172970231617250413E-15 ) ) ;
#34397 = DIRECTION ( 'NONE',  ( -1.000000000000000000, -0.000000000000000000, 0.000000000000000000 ) ) ;
#34398 = DIRECTION ( 'NONE',  ( -1.000000000000000000, 0.000000000000000000, 0.000000000000000000 ) ) ;
#34399 = DIRECTION ( 'NONE',  ( 1.000000000000000000, -0.000000000000000000, -0.000000000000000000 ) ) ;
#34400 = FACE_OUTER_BOUND ( 'NONE', #10798, .T. ) ;
#34401 = LINE ( 'NONE', #29864, #58801 ) ;
#34402 = DIRECTION ( 'NONE',  ( 0.000000000000000000, 0.000000000000000000, 1.000000000000000000 ) ) ;
#34403 = EDGE_LOOP ( 'NONE', ( #30052, #61869, #73692, #7089 ) ) ;
#34404 = CARTESIAN_POINT ( 'NONE',  ( -97.64999999999994884, -208.4700217866474645, 83.04145833506763097 ) ) ;
#34405 = ORIENTED_EDGE ( 'NONE', *, *, #62045, .F. ) ;
#34406 = DIRECTION ( 'NONE',  ( -1.000000000000000000, -0.000000000000000000, 0.000000000000000000 ) ) ;
#34407 = ORIENTED_EDGE ( 'NONE', *, *, #46101, .T. ) ;
#34409 = CARTESIAN_POINT ( 'NONE',  ( -93.67500000000003979, 87.70503267997129626, 80.13104166840095388 ) ) ;
#34408 = CARTESIAN_POINT ( 'NONE',  ( 96.32499999999997442, 92.29496732002878900, 77.80270833506763495 ) ) ;
#34410 = ORIENTED_EDGE ( 'NONE', *, *, #20442, .T. ) ;
#34411 = CARTESIAN_POINT ( 'NONE',  ( 92.69370383062498320, 88.66845928578037217, 79.05947916753382287 ) ) ;
#34412 = VECTOR ( 'NONE', #13155, 1000.000000000000000 ) ;
#34413 = CARTESIAN_POINT ( 'NONE',  ( 10.00000000000000000, -27.05870788708250885, 26.08949754953014022 ) ) ;
#34414 = LINE ( 'NONE', #35893, #38620 ) ;
#34415 = AXIS2_PLACEMENT_3D ( 'NONE', #23760, #51957, #34668 ) ;
#34416 = FACE_OUTER_BOUND ( 'NONE', #3534, .T. ) ;
#34417 = EDGE_LOOP ( 'NONE', ( #20358, #13667, #26642, #64815 ) ) ;
#34418 = CARTESIAN_POINT ( 'NONE',  ( 0.000000000000000000, 15.33399622253483408, 80.55351364060595643 ) ) ;
#34419 = DIRECTION ( 'NONE',  ( -0.000000000000000000, 0.2079116908177543743, 0.9781476007338066880 ) ) ;
#34420 = CARTESIAN_POINT ( 'NONE',  ( -7.400000000000003908, -1.056673655988042765E-14, -5.892267102755452808E-15 ) ) ;
#34421 = EDGE_LOOP ( 'NONE', ( #55671, #56869, #42653 ) ) ;
#34422 = CIRCLE ( 'NONE', #54867, 82.00000000000000000 ) ;
#34423 = ORIENTED_EDGE ( 'NONE', *, *, #33616, .T. ) ;
#34424 = AXIS2_PLACEMENT_3D ( 'NONE', #45098, #5257, #68402 ) ;
#34425 = ADVANCED_FACE ( 'NONE', ( #68062 ), #45141, .T. ) ;
#34426 = PRODUCT_DEFINITION_SHAPE ( 'NONE', 'NONE',  #74364 ) ;
#34427 = DIRECTION ( 'NONE',  ( 1.000000000000000000, 0.000000000000000000, 0.000000000000000000 ) ) ;
#34428 = CIRCLE ( 'NONE', #28417, 42.00000000000000000 ) ;
#34429 = CARTESIAN_POINT ( 'NONE',  ( 5.999999999999999112, 67.80270845531956070, -46.11716303203111522 ) ) ;
#34430 = LINE ( 'NONE', #33694, #13730 ) ;
#34431 = CARTESIAN_POINT ( 'NONE',  ( -92.69370383062498320, -209.9999999999999716, 81.22906250086715829 ) ) ;
#34432 = ORIENTED_EDGE ( 'NONE', *, *, #5370, .T. ) ;
#34433 = ORIENTED_EDGE ( 'NONE', *, *, #45185, .T. ) ;
#34434 = CARTESIAN_POINT ( 'NONE',  ( 97.64999999964365429, -210.0000434577794408, 89.12687334326047051 ) ) ;
#34435 = CARTESIAN_POINT ( 'NONE',  ( -97.51895106303136629, -210.1706338775387621, 74.92125785461011844 ) ) ;
#34436 = AXIS2_PLACEMENT_3D ( 'NONE', #70151, #58900, #63438 ) ;
#34437 = DIRECTION ( 'NONE',  ( -1.000000000000000000, 0.000000000000000000, 0.000000000000000000 ) ) ;
#34438 = CARTESIAN_POINT ( 'NONE',  ( -6.880223345695647197, -142.5202692415819854, -2.500000000000000000 ) ) ;
#34439 = DIRECTION ( 'NONE',  ( -1.000000000000000000, 0.000000000000000000, 0.000000000000000000 ) ) ;
#34440 = DIRECTION ( 'NONE',  ( -0.8225049752423776450, -0.5687579148473765889, 0.000000000000000000 ) ) ;
#34441 = EDGE_CURVE ( 'NONE', #73312, #20472, #33092, .T. ) ;
#34442 = CARTESIAN_POINT ( 'NONE',  ( 92.34999999999999432, 90.00000000000002842, 76.66499999999999204 ) ) ;
#34443 = CARTESIAN_POINT ( 'NONE',  ( -94.99999999999997158, -206.9400435732949575, 76.58562500173430010 ) ) ;
#34444 = CARTESIAN_POINT ( 'NONE',  ( 99.99999999999998579, 95.00000000000002842, 90.00000000000000000 ) ) ;
#34446 = EDGE_CURVE ( 'NONE', #7952, #52503, #73222, .T. ) ;
#34445 = AXIS2_PLACEMENT_3D ( 'NONE', #19394, #36688, #59630 ) ;
#34447 = DIRECTION ( 'NONE',  ( -1.000000000000000000, -0.000000000000000000, 0.000000000000000000 ) ) ;
#34448 = CARTESIAN_POINT ( 'NONE',  ( 93.84685191531248449, 91.99731107132950569, 87.79072916753381151 ) ) ;
#34449 = EDGE_CURVE ( 'NONE', #16195, #54579, #43266, .T. ) ;
#34450 = CARTESIAN_POINT ( 'NONE',  ( -93.84685191531248449, -208.0026889286704943, 88.31989583420048007 ) ) ;
#34451 = CARTESIAN_POINT ( 'NONE',  ( -92.35000000000003695, 90.00000000000004263, 80.79249999999998977 ) ) ;
#34452 = ORIENTED_EDGE ( 'NONE', *, *, #17675, .F. ) ;
#34453 = EDGE_CURVE ( 'NONE', #4731, #34500, #7237, .T. ) ;
#34454 = CARTESIAN_POINT ( 'NONE',  ( 5.000000000000002665, 76.69515212746057387, -29.01471420065480089 ) ) ;
#34455 = CARTESIAN_POINT ( 'NONE',  ( -95.00000000000002842, 87.33691857156074434, 79.64156250086713840 ) ) ;
#34456 = DIRECTION ( 'NONE',  ( 0.000000000000000000, -0.9876883405951394357, 0.1564344650402205716 ) ) ;
#34457 = APPLICATION_CONTEXT ( 'automotive_design' ) ;
#34458 = EDGE_LOOP ( 'NONE', ( #1152, #63797, #57783, #54990 ) ) ;
#34459 = LINE ( 'NONE', #52123, #24660 ) ;
#34460 = CARTESIAN_POINT ( 'NONE',  ( 10.00000000000000000, 0.000000000000000000, 0.000000000000000000 ) ) ;
#34461 = EDGE_CURVE ( 'NONE', #24497, #19214, #55297, .T. ) ;
#34462 = VECTOR ( 'NONE', #9741, 1000.000000000000114 ) ;
#34463 = CARTESIAN_POINT ( 'NONE',  ( 10.00000000000000000, 24.73286445877703699, 73.44644590900070114 ) ) ;
#34464 = AXIS2_PLACEMENT_3D ( 'NONE', #10466, #72496, #72854 ) ;
#34465 = DIRECTION ( 'NONE',  ( 1.000000000000000000, 0.000000000000000000, 0.000000000000000000 ) ) ;
#34466 = CARTESIAN_POINT ( 'NONE',  ( 96.15314808468750130, -211.9973110713294489, 76.67822916753381435 ) ) ;
#34467 = AXIS2_PLACEMENT_3D ( 'NONE', #53754, #13886, #2669 ) ;
#34468 = ORIENTED_EDGE ( 'NONE', *, *, #25527, .F. ) ;
#34469 = AXIS2_PLACEMENT_3D ( 'NONE', #47176, #47911, #46433 ) ;
#34470 = VERTEX_POINT ( 'NONE', #38379 ) ;
#34471 = CARTESIAN_POINT ( 'NONE',  ( 92.69370383062501162, -208.6684592857803295, 84.66864583420047552 ) ) ;
#34472 = EDGE_CURVE ( 'NONE', #50309, #21580, #27454, .T. ) ;
#34473 = LINE ( 'NONE', #23943, #10442 ) ;
#34474 = CYLINDRICAL_SURFACE ( 'NONE', #26730, 82.00000000000000000 ) ;
#34475 = CARTESIAN_POINT ( 'NONE',  ( -93.67499999999998295, -207.7050326799711968, 77.16770833506762983 ) ) ;
#34476 = FACE_OUTER_BOUND ( 'NONE', #70264, .T. ) ;
#34477 = ADVANCED_FACE ( 'NONE', ( #4185 ), #72930, .T. ) ;
#34478 = CARTESIAN_POINT ( 'NONE',  ( -12.49999999999999645, 0.000000000000000000, 125.0000000000000000 ) ) ;
#34479 = CARTESIAN_POINT ( 'NONE',  ( 96.32499999999998863, -207.7050326799711968, 89.78833333333332689 ) ) ;
#34480 = VERTEX_POINT ( 'NONE', #10537 ) ;
#34481 = EDGE_LOOP ( 'NONE', ( #61559, #46176, #60495, #12637 ) ) ;
#34482 = ORIENTED_EDGE ( 'NONE', *, *, #54013, .F. ) ;
#34483 = ORIENTED_EDGE ( 'NONE', *, *, #67553, .T. ) ;
#34484 =( NAMED_UNIT ( * ) PLANE_ANGLE_UNIT ( ) SI_UNIT ( $, .RADIAN. ) );
#34485 =( GEOMETRIC_REPRESENTATION_CONTEXT ( 3 ) GLOBAL_UNCERTAINTY_ASSIGNED_CONTEXT ( ( #30824 ) ) GLOBAL_UNIT_ASSIGNED_CONTEXT ( ( #31507, #4080, #71350 ) ) REPRESENTATION_CONTEXT ( 'NONE', 'WORKASPACE' ) );
#34486 = CARTESIAN_POINT ( 'NONE',  ( -93.84685191531254134, 91.99731107132950569, 88.95489583420049939 ) ) ;
#34487 = CARTESIAN_POINT ( 'NONE',  ( 10.00000000000000000, 6.555932627142418312, 37.01155633439060466 ) ) ;
#34488 = DIRECTION ( 'NONE',  ( 0.000000000000000000, 0.000000000000000000, -1.000000000000000000 ) ) ;
#34489 = CARTESIAN_POINT ( 'NONE',  ( 95.00000000000000000, -213.0599564267049857, 76.26812500173430465 ) ) ;
#34490 = CARTESIAN_POINT ( 'NONE',  ( 97.64999999999997726, 88.47002178664753558, 78.83458333333334167 ) ) ;
#34491 = VECTOR ( 'NONE', #13856, 1000.000000000000000 ) ;
#34492 = ORIENTED_EDGE ( 'NONE', *, *, #69941, .T. ) ;
#34493 = CARTESIAN_POINT ( 'NONE',  ( 97.65000000000000568, -208.4700217866474645, 75.20979166840096752 ) ) ;
#34494 = ORIENTED_EDGE ( 'NONE', *, *, #14750, .T. ) ;
#34495 = CARTESIAN_POINT ( 'NONE',  ( 0.000000000000000000, -72.35160999960801576, -20.41045688087902121 ) ) ;
#34496 = ORIENTED_EDGE ( 'NONE', *, *, #66791, .T. ) ;
#34497 = CARTESIAN_POINT ( 'NONE',  ( -97.65000000000001990, 90.00000000000004263, 89.44437500173430067 ) ) ;
#34498 = CARTESIAN_POINT ( 'NONE',  ( -97.30629616937501680, 90.00000000000004263, 80.91156250086716284 ) ) ;
#34499 = CARTESIAN_POINT ( 'NONE',  ( 96.15314808468748708, 88.00268892867053694, 88.74322916753382628 ) ) ;
#34500 = VERTEX_POINT ( 'NONE', #17668 ) ;
#34501 = DIRECTION ( 'NONE',  ( -1.000000000000000000, 0.000000000000000000, 0.000000000000000000 ) ) ;
#34502 = CARTESIAN_POINT ( 'NONE',  ( 0.000000000000000000, 0.000000000000000000, 0.000000000000000000 ) ) ;
#34503 = DIRECTION ( 'NONE',  ( -1.000000000000000000, -0.000000000000000000, 0.000000000000000000 ) ) ;
#34504 = CYLINDRICAL_SURFACE ( 'NONE', #55239, 12.75000000000265388 ) ;
#34505 = ORIENTED_EDGE ( 'NONE', *, *, #47643, .F. ) ;
#34506 = CYLINDRICAL_SURFACE ( 'NONE', #2750, 31.99999999999998579 ) ;
#34507 = CARTESIAN_POINT ( 'NONE',  ( -97.30629616937497417, -208.6684592857803011, 77.52489583420046415 ) ) ;
#34508 = ORIENTED_EDGE ( 'NONE', *, *, #59873, .T. ) ;
#34509 = VERTEX_POINT ( 'NONE', #57534 ) ;
#34510 = FACE_BOUND ( 'NONE', #35773, .T. ) ;
#34511 = EDGE_LOOP ( 'NONE', ( #62037, #70733, #42996, #29513 ) ) ;
#34512 = CYLINDRICAL_SURFACE ( 'NONE', #47961, 82.00000000000000000 ) ;
#34513 = DIRECTION ( 'NONE',  ( -1.000000000000000000, -0.000000000000000000, 0.000000000000000000 ) ) ;
#34514 = VERTEX_POINT ( 'NONE', #64 ) ;
#34515 =( BOUNDED_CURVE ( )  B_SPLINE_CURVE ( 2, ( #54016, #43850, #55486, #49833, #2554, #72751, #25435 ),
 .UNSPECIFIED., .F., .F. ) 
 B_SPLINE_CURVE_WITH_KNOTS ( ( 3, 2, 2, 3 ),
 ( 0.8333333333333334814, 0.8402777777777779011, 0.8472222222222222099, 0.8541666666666666297 ),
 .UNSPECIFIED. ) 
 CURVE ( )  GEOMETRIC_REPRESENTATION_ITEM ( )  RATIONAL_B_SPLINE_CURVE ( ( 0.9999999999999978906, 0.8660254037844408170, 1.000000000000000000, 0.8660254037844387076, 1.000000000000000000, 0.8660254037844387076, 1.000000000000000000 ) ) 
 REPRESENTATION_ITEM ( '' )  );
#34516 = CARTESIAN_POINT ( 'NONE',  ( -97.30629616937497417, -211.3315407142195852, 76.99572916753380980 ) ) ;
#34517 = ORIENTED_EDGE ( 'NONE', *, *, #70284, .F. ) ;
#34518 = DIRECTION ( 'NONE',  ( -1.000000000000000000, 0.000000000000000000, 0.000000000000000000 ) ) ;
#34519 = CIRCLE ( 'NONE', #50116, 31.99999999999999289 ) ;
#34520 = CARTESIAN_POINT ( 'NONE',  ( 22.75000000000000000, 0.000000000000000000, 0.000000000000000000 ) ) ;
#34521 = CARTESIAN_POINT ( 'NONE',  ( -26.50044424985086522, 0.001194404165032690894, -65.00000000000069633 ) ) ;
#34522 = ORIENTED_EDGE ( 'NONE', *, *, #15216, .F. ) ;
#34523 = PRESENTATION_LAYER_ASSIGNMENT (  '', '', ( #10522 ) ) ;
#34524 = CARTESIAN_POINT ( 'NONE',  ( 12.00000000000000000, 22.07842321921492612, 8.187992925817123790 ) ) ;
#34525 = CIRCLE ( 'NONE', #14114, 57.50000000000000000 ) ;
#34526 = CARTESIAN_POINT ( 'NONE',  ( 92.34999999999999432, -210.0000225208804068, 86.26937578065383150 ) ) ;
#34527 = CARTESIAN_POINT ( 'NONE',  ( 92.69370383062498320, 90.00000000000002842, 83.92781250086714806 ) ) ;
#34528 = AXIS2_PLACEMENT_3D ( 'NONE', #60720, #14471, #9200 ) ;
#34529 = CARTESIAN_POINT ( 'NONE',  ( -92.34999999999990905, -211.5299782133524218, 83.91458333333333997 ) ) ;
#34530 = CARTESIAN_POINT ( 'NONE',  ( -95.00000000000002842, 86.94004357329504273, 88.25374999999999659 ) ) ;
#34531 = EDGE_CURVE ( 'NONE', #62864, #69166, #39657, .T. ) ;
#34532 = CARTESIAN_POINT ( 'NONE',  ( 0.000000000000000000, 28.89263327155746097, 71.91182617369197771 ) ) ;
#34533 = FACE_OUTER_BOUND ( 'NONE', #66851, .T. ) ;
#34534 = FACE_OUTER_BOUND ( 'NONE', #411, .T. ) ;
#34535 = EDGE_CURVE ( 'NONE', #57460, #25525, #40886, .T. ) ;
#34536 = LINE ( 'NONE', #6356, #17888 ) ;
#34537 = DIRECTION ( 'NONE',  ( 0.000000000000000000, 0.000000000000000000, 1.000000000000000000 ) ) ;
#34538 = DIRECTION ( 'NONE',  ( 0.000000000000000000, 0.000000000000000000, 1.000000000000000000 ) ) ;
#34539 = EDGE_CURVE ( 'NONE', #61251, #41269, #26498, .T. ) ;
#34540 = CARTESIAN_POINT ( 'NONE',  ( 7.001685179585692254, -14.98378029539707512, -1.199999999999999956 ) ) ;
#34541 = B_SPLINE_CURVE_WITH_KNOTS ( 'NONE', 3,
 ( #45177, #32755, #44440, #67353, #38788, #66975, #15476, #68100, #45559, #61721, #55705, #32391, #73352, #5335, #50046, #38419, #72971, #50795, #4592, #60972, #27113, #73721, #15855, #10205 ),
 .UNSPECIFIED., .F., .F.,
 ( 4, 2, 2, 2, 2, 2, 2, 2, 2, 2, 2, 4 ),
 ( -0.009991285186810519234, -0.009254074022779607347, -0.008516862858748697196, -0.007779651694717785310, -0.007411046112702331101, -0.007042440530686875158, -0.006673834948671420950, -0.006305229366655965006, -0.005568018202625055722, -0.004830807038594145571, -0.004462201456578723455, -0.004093595874563301339 ),
 .UNSPECIFIED. ) ;
#34542 = LINE ( 'NONE', #39834, #67757 ) ;
#34543 = CARTESIAN_POINT ( 'NONE',  ( -3.000000000000000000, -20.55727247249748046, 16.78983467731285018 ) ) ;
#34544 = VECTOR ( 'NONE', #39949, 1000.000000000000000 ) ;
#34545 = VECTOR ( 'NONE', #60629, 1000.000000000000000 ) ;
#34546 = CARTESIAN_POINT ( 'NONE',  ( -97.65000000000001990, 90.00000000000004263, 79.83999999999998920 ) ) ;
#34547 = ADVANCED_FACE ( 'NONE', ( #46612 ), #6759, .T. ) ;
#34548 = VECTOR ( 'NONE', #45946, 1000.000000000000000 ) ;
#34549 = CARTESIAN_POINT ( 'NONE',  ( 0.000000000000000000, -50.23322058963393744, 64.81221759200325039 ) ) ;
#34550 = EDGE_CURVE ( 'NONE', #15874, #3632, #68528, .T. ) ;
#34551 = CARTESIAN_POINT ( 'NONE',  ( -11.59517495878806947, -96.12423995607481686, 2.500000000000000000 ) ) ;
#34552 = SURFACE_SIDE_STYLE ('',( #40571 ) ) ;
#34553 = CARTESIAN_POINT ( 'NONE',  ( 0.000000000000000000, 0.000000000000000000, 0.000000000000000000 ) ) ;
#34554 = DIRECTION ( 'NONE',  ( 1.000000000000000000, 1.390371824233641368E-16, 0.000000000000000000 ) ) ;
#34555 = EDGE_CURVE ( 'NONE', #15732, #19667, #31265, .T. ) ;
#34556 = CARTESIAN_POINT ( 'NONE',  ( 97.30629616937498838, -208.6684592857803011, 86.36197916753383197 ) ) ;
#34557 = ORIENTED_EDGE ( 'NONE', *, *, #58215, .T. ) ;
#34558 = VERTEX_POINT ( 'NONE', #35684 ) ;
#34559 = EDGE_CURVE ( 'NONE', #26707, #1365, #63184, .T. ) ;
#34560 = DIRECTION ( 'NONE',  ( -0.000000000000000000, -0.000000000000000000, 1.000000000000000000 ) ) ;
#34561 = ORIENTED_EDGE ( 'NONE', *, *, #72967, .T. ) ;
#34562 = CARTESIAN_POINT ( 'NONE',  ( -96.32499999999996021, -207.7050326799711968, 79.81354166840095843 ) ) ;
#34563 = LINE ( 'NONE', #18376, #35208 ) ;
#34564 = AXIS2_PLACEMENT_3D ( 'NONE', #70247, #29655, #41331 ) ;
#34565 = ORIENTED_EDGE ( 'NONE', *, *, #16027, .F. ) ;
#34566 = CARTESIAN_POINT ( 'NONE',  ( 93.84685191531249870, -208.0026889286704943, 84.61572916753381435 ) ) ;
#34567 = AXIS2_PLACEMENT_3D ( 'NONE', #8837, #66361, #14089 ) ;
#34568 = CIRCLE ( 'NONE', #34749, 37.49900000000000944 ) ;
#34569 = EDGE_LOOP ( 'NONE', ( #52713, #30869 ) ) ;
#34570 = CARTESIAN_POINT ( 'NONE',  ( 10.00000000000000000, 0.000000000000000000, 0.000000000000000000 ) ) ;
#34571 = ORIENTED_EDGE ( 'NONE', *, *, #73671, .F. ) ;
#34572 = ORIENTED_EDGE ( 'NONE', *, *, #64282, .F. ) ;
#34573 = CARTESIAN_POINT ( 'NONE',  ( 12.00000000000000000, 5.835314593368777558, 22.81335362449846471 ) ) ;
#34574 = UNCERTAINTY_MEASURE_WITH_UNIT (LENGTH_MEASURE( 1.000000000000000082E-05 ), #70864, 'distance_accuracy_value', 'NONE');
#34575 = VECTOR ( 'NONE', #5795, 1000.000000000000000 ) ;
#34576 = DIRECTION ( 'NONE',  ( 1.000000000000000000, 0.000000000000000000, 0.000000000000000000 ) ) ;
#34577 = AXIS2_PLACEMENT_3D ( 'NONE', #68492, #44448, #5714 ) ;
#34578 = EDGE_LOOP ( 'NONE', ( #30494, #40033, #19309, #19576 ) ) ;
#34579 = DIRECTION ( 'NONE',  ( 0.9435911131814398445, -0.3311129884571295534, 0.000000000000000000 ) ) ;
#34580 = CARTESIAN_POINT ( 'NONE',  ( 95.00000000000000000, -213.0599564267049857, 87.69812500173429726 ) ) ;
#34581 = ORIENTED_EDGE ( 'NONE', *, *, #28113, .T. ) ;
#34582 = LINE ( 'NONE', #46244, #16685 ) ;
#34583 = VERTEX_POINT ( 'NONE', #29303 ) ;
#34584 = DIRECTION ( 'NONE',  ( -1.000000000000000000, 0.000000000000000000, 0.000000000000000000 ) ) ;
#34585 = EDGE_LOOP ( 'NONE', ( #64864, #543, #72305, #31525 ) ) ;
#34586 = ADVANCED_BREP_SHAPE_REPRESENTATION ( '', ( #62016, #43395 ), #59053 ) ;
#34587 = EDGE_LOOP ( 'NONE', ( #14731, #54008, #46245, #16563 ) ) ;
#34588 = ORIENTED_EDGE ( 'NONE', *, *, #41414, .F. ) ;
#34589 = CARTESIAN_POINT ( 'NONE',  ( 5.000000000000002665, 76.69515212746016175, 29.01471420065591289 ) ) ;
#34590 = CARTESIAN_POINT ( 'NONE',  ( -4.999999999999999112, -2.691295138309024448, -1.881393335304213821 ) ) ;
#34591 = EDGE_LOOP ( 'NONE', ( #54944, #26559, #22501, #24079 ) ) ;
#34592 = AXIS2_PLACEMENT_3D ( 'NONE', #38179, #8507, #42718 ) ;
#34593 = ORIENTED_EDGE ( 'NONE', *, *, #54636, .F. ) ;
#34594 = AXIS2_PLACEMENT_3D ( 'NONE', #11209, #44695, #45438 ) ;
#34595 = ORIENTED_EDGE ( 'NONE', *, *, #565, .T. ) ;
#34596 = CARTESIAN_POINT ( 'NONE',  ( 93.67500000000001137, -212.2949673200287179, 76.13583333333333769 ) ) ;
#34597 = CARTESIAN_POINT ( 'NONE',  ( -11.59999999999999787, 0.000000000000000000, 42.00000000000001421 ) ) ;
#34598 = AXIS2_PLACEMENT_3D ( 'NONE', #17462, #52038, #23477 ) ;
#34599 = VECTOR ( 'NONE', #29818, 1000.000000000000000 ) ;
#34600 = CARTESIAN_POINT ( 'NONE',  ( -92.35000000000005116, 88.47002178664754979, 86.45458333333333201 ) ) ;
#34601 = ORIENTED_EDGE ( 'NONE', *, *, #22594, .F. ) ;
#34602 = CARTESIAN_POINT ( 'NONE',  ( 97.30629616937498838, 91.33154071421968467, 74.77322916753379900 ) ) ;
#34603 = ORIENTED_EDGE ( 'NONE', *, *, #24270, .T. ) ;
#34604 = DIRECTION ( 'NONE',  ( 0.000000000000000000, 0.000000000000000000, -1.000000000000000000 ) ) ;
#34605 = CARTESIAN_POINT ( 'NONE',  ( -93.84685191531248449, -208.0026889286704943, 86.25614583420048120 ) ) ;
#34606 = VERTEX_POINT ( 'NONE', #51511 ) ;
#34607 = CARTESIAN_POINT ( 'NONE',  ( 0.000000000000000000, -35.38097989696503021, -12.42422080174676147 ) ) ;
#34608 = FACE_OUTER_BOUND ( 'NONE', #59257, .T. ) ;
#34609 = DIRECTION ( 'NONE',  ( 0.000000000000000000, -0.000000000000000000, 1.000000000000000000 ) ) ;
#34610 = CARTESIAN_POINT ( 'NONE',  ( -97.30629616937497417, -208.6684592857803295, 76.88989583420047325 ) ) ;
#34611 = ADVANCED_FACE ( 'NONE', ( #63550 ), #41344, .T. ) ;
#34612 = DIRECTION ( 'NONE',  ( 1.000000000000000000, -7.571537405616606460E-15, -2.598394312951952234E-14 ) ) ;
#34613 = DIRECTION ( 'NONE',  ( 0.3420201433256714330, 0.000000000000000000, 0.9396926207859073177 ) ) ;
#34614 = EDGE_CURVE ( 'NONE', #24962, #49804, #42127, .T. ) ;
#34615 = CARTESIAN_POINT ( 'NONE',  ( -92.35000000000012221, 90.00000071509187194, 85.31687502647973531 ) ) ;
#34616 = EDGE_CURVE ( 'NONE', #29034, #38013, #12023, .T. ) ;
#34617 = ADVANCED_FACE ( 'NONE', ( #47355 ), #18042, .T. ) ;
#34618 = DIRECTION ( 'NONE',  ( 0.000000000000000000, -6.938893903907228378E-15, 1.000000000000000000 ) ) ;
#34619 = DIRECTION ( 'NONE',  ( 0.000000000000000000, 0.000000000000000000, 1.000000000000000000 ) ) ;
#34620 = CARTESIAN_POINT ( 'NONE',  ( -95.00000000000002842, 87.33691857156074434, 79.00656250086713328 ) ) ;
#34621 = DIRECTION ( 'NONE',  ( -2.628368902995175337E-16, -1.000000000000000000, 0.000000000000000000 ) ) ;
#34622 = DIRECTION ( 'NONE',  ( -1.000000000000000000, 0.000000000000000000, 0.000000000000000000 ) ) ;
#34623 = EDGE_CURVE ( 'NONE', #54553, #47528, #25771, .T. ) ;
#34624 = AXIS2_PLACEMENT_3D ( 'NONE', #64187, #23958, #17941 ) ;
#34625 = ORIENTED_EDGE ( 'NONE', *, *, #8395, .T. ) ;
#34626 = CARTESIAN_POINT ( 'NONE',  ( 11.99999999999999822, 62.20884554314020676, 46.21855187248652896 ) ) ;
#34627 = VECTOR ( 'NONE', #66721, 1000.000000000000000 ) ;
#34628 = VECTOR ( 'NONE', #27881, 1000.000000000000000 ) ;
#34629 = EDGE_CURVE ( 'NONE', #14315, #17407, #23116, .T. ) ;
#34630 = CARTESIAN_POINT ( 'NONE',  ( -10.00000000000000000, 0.000000000000000000, 0.000000000000000000 ) ) ;
#34631 = DIRECTION ( 'NONE',  ( 0.000000000000000000, 0.8910065241883688980, -0.4539904997395446951 ) ) ;
#34632 = DIRECTION ( 'NONE',  ( -1.000000000000000000, -0.000000000000000000, 0.000000000000000000 ) ) ;
#34633 = FACE_OUTER_BOUND ( 'NONE', #65049, .T. ) ;
#34634 = DIRECTION ( 'NONE',  ( 1.000000000000000000, 0.000000000000000000, 0.000000000000000000 ) ) ;
#34635 = CARTESIAN_POINT ( 'NONE',  ( -94.99999999999997158, -212.6630814284392557, 75.35531250086715715 ) ) ;
#34636 = VECTOR ( 'NONE', #54976, 1000.000000000000000 ) ;
#34637 = FACE_OUTER_BOUND ( 'NONE', #49186, .T. ) ;
#34638 = ORIENTED_EDGE ( 'NONE', *, *, #45498, .T. ) ;
#34639 = DIRECTION ( 'NONE',  ( -1.000000000000000000, 0.000000000000000000, -0.000000000000000000 ) ) ;
#34640 = EDGE_CURVE ( 'NONE', #63672, #1816, #58050, .T. ) ;
#34641 = CYLINDRICAL_SURFACE ( 'NONE', #41880, 42.00000000000000000 ) ;
#34642 = LINE ( 'NONE', #15877, #72953 ) ;
#34643 = DIRECTION ( 'NONE',  ( 0.000000000000000000, 0.4539904997395477482, -0.8910065241883673437 ) ) ;
#34644 = AXIS2_PLACEMENT_3D ( 'NONE', #40762, #58788, #12174 ) ;
#34645 = EDGE_CURVE ( 'NONE', #9362, #32052, #9690, .T. ) ;
#34646 = ADVANCED_FACE ( 'NONE', ( #22740 ), #11793, .T. ) ;
#34648 = CARTESIAN_POINT ( 'NONE',  ( 10.00000000000000000, -73.95703589263958122, -23.16143007188506431 ) ) ;
#34647 = AXIS2_PLACEMENT_3D ( 'NONE', #29017, #52320, #57233 ) ;
#34649 = ORIENTED_EDGE ( 'NONE', *, *, #22560, .T. ) ;
#34650 = AXIS2_PLACEMENT_3D ( 'NONE', #11335, #34639, #28252 ) ;
#34651 = CARTESIAN_POINT ( 'NONE',  ( 0.000000000000000000, 17.67226234102826510, 33.17418723428314564 ) ) ;
#34652 = EDGE_CURVE ( 'NONE', #37997, #35415, #50476, .T. ) ;
#34653 = FACE_OUTER_BOUND ( 'NONE', #22363, .T. ) ;
#34654 = ORIENTED_EDGE ( 'NONE', *, *, #22929, .F. ) ;
#34655 = CIRCLE ( 'NONE', #57533, 77.49900000000000944 ) ;
#34656 = CARTESIAN_POINT ( 'NONE',  ( 97.30629616937498838, -211.3315407142195852, 89.27239583420048064 ) ) ;
#34657 = DIRECTION ( 'NONE',  ( -2.628368902995175337E-16, -1.000000000000000000, 0.000000000000000000 ) ) ;
#34658 = ORIENTED_EDGE ( 'NONE', *, *, #56527, .T. ) ;
#34659 = DIRECTION ( 'NONE',  ( 0.000000000000000000, 0.000000000000000000, 1.000000000000000000 ) ) ;
#34660 = ORIENTED_EDGE ( 'NONE', *, *, #59788, .T. ) ;
#34661 = CARTESIAN_POINT ( 'NONE',  ( 10.00000000000000000, -70.53064760720336324, 26.01480285779810231 ) ) ;
#34662 = ORIENTED_EDGE ( 'NONE', *, *, #63763, .T. ) ;
#34663 = DIRECTION ( 'NONE',  ( -1.000000000000000000, -0.000000000000000000, 0.000000000000000000 ) ) ;
#34664 = ORIENTED_EDGE ( 'NONE', *, *, #66110, .T. ) ;
#34665 = FACE_OUTER_BOUND ( 'NONE', #10608, .T. ) ;
#34666 = ORIENTED_EDGE ( 'NONE', *, *, #4147, .T. ) ;
#34667 = ORIENTED_EDGE ( 'NONE', *, *, #17232, .F. ) ;
#34668 = DIRECTION ( 'NONE',  ( 0.000000000000000000, 0.000000000000000000, 1.000000000000000000 ) ) ;
#34669 = AXIS2_PLACEMENT_3D ( 'NONE', #10998, #44852, #66687 ) ;
#34670 = ORIENTED_EDGE ( 'NONE', *, *, #19612, .F. ) ;
#34671 = ORIENTED_EDGE ( 'NONE', *, *, #32603, .F. ) ;
#34672 = CARTESIAN_POINT ( 'NONE',  ( 92.49271422325853109, 89.65937732759924472, 74.92458348457969919 ) ) ;
#34673 = AXIS2_PLACEMENT_3D ( 'NONE', #15951, #51653, #38892 ) ;
#34674 = ORIENTED_EDGE ( 'NONE', *, *, #7083, .T. ) ;
#34675 = AXIS2_PLACEMENT_3D ( 'NONE', #44733, #67657, #3406 ) ;
#34676 = ORIENTED_EDGE ( 'NONE', *, *, #4965, .F. ) ;
#34677 = CARTESIAN_POINT ( 'NONE',  ( 93.84685191531248449, 88.00268892867053694, 84.03364583420047040 ) ) ;
#34678 = ORIENTED_EDGE ( 'NONE', *, *, #10154, .F. ) ;
#34679 = CARTESIAN_POINT ( 'NONE',  ( 93.84685191531249870, -208.0026889286704943, 80.64697916753381435 ) ) ;
#34680 = PRODUCT_CONTEXT ( 'NONE', #15240, 'mechanical' ) ;
#34681 = DIRECTION ( 'NONE',  ( -1.000000000000000000, 0.000000000000000000, 0.000000000000000000 ) ) ;
#34682 = AXIS2_PLACEMENT_3D ( 'NONE', #41382, #64319, #64684 ) ;
#34683 = DIRECTION ( 'NONE',  ( -1.000000000000000000, -0.000000000000000000, -0.000000000000000000 ) ) ;
#34684 = CARTESIAN_POINT ( 'NONE',  ( 10.00000000000000000, 0.000000000000000000, 0.000000000000000000 ) ) ;
#34685 = AXIS2_PLACEMENT_3D ( 'NONE', #24120, #59432, #28998 ) ;
#34686 = DIRECTION ( 'NONE',  ( -1.000000000000000000, -0.000000000000000000, 0.000000000000000000 ) ) ;
#34687 = CARTESIAN_POINT ( 'NONE',  ( 5.999999999999999112, 27.74655509720779989, -77.16300072079631889 ) ) ;
#34688 = CARTESIAN_POINT ( 'NONE',  ( 0.000000000000000000, 71.87247863392471459, -39.47590169984771080 ) ) ;
#34689 = CARTESIAN_POINT ( 'NONE',  ( -96.15314808468747287, -208.0026889286704943, 85.09197916753380753 ) ) ;
#34690 = CARTESIAN_POINT ( 'NONE',  ( -92.69370383062504004, 90.00000000000004263, 82.49906250086715431 ) ) ;
#34691 = VERTEX_POINT ( 'NONE', #57310 ) ;
#34693 = CARTESIAN_POINT ( 'NONE',  ( -93.84685191531254134, 91.99731107132950569, 85.62114583420046188 ) ) ;
#34692 = CARTESIAN_POINT ( 'NONE',  ( 97.30629616937498838, 90.00000000000002842, 83.61031250086713840 ) ) ;
#34694 = ORIENTED_EDGE ( 'NONE', *, *, #73298, .T. ) ;
#34695 = DIRECTION ( 'NONE',  ( -1.000000000000000000, -0.000000000000000000, 0.000000000000000000 ) ) ;
#34696 = DIRECTION ( 'NONE',  ( 0.000000000000000000, 0.000000000000000000, -1.000000000000000000 ) ) ;
#34697 = CYLINDRICAL_SURFACE ( 'NONE', #45164, 2.649999999999985700 ) ;
#34698 = DIRECTION ( 'NONE',  ( -0.000000000000000000, -0.000000000000000000, -1.000000000000000000 ) ) ;
#34699 = CIRCLE ( 'NONE', #58753, 31.99999999999998579 ) ;
#34700 = CARTESIAN_POINT ( 'NONE',  ( -96.15314808468747287, -208.0026889286704943, 86.99697916753380866 ) ) ;
#34701 = DIRECTION ( 'NONE',  ( 0.000000000000000000, 0.000000000000000000, 1.000000000000000000 ) ) ;
#34702 = AXIS2_PLACEMENT_3D ( 'NONE', #52638, #13523, #64303 ) ;
#34703 = CARTESIAN_POINT ( 'NONE',  ( 10.00000000000000000, 0.000000000000000000, 0.000000000000000000 ) ) ;
#34704 = DIRECTION ( 'NONE',  ( 0.000000000000000000, 0.000000000000000000, 1.000000000000000000 ) ) ;
#34705 = DIRECTION ( 'NONE',  ( 0.000000000000000000, 0.000000000000000000, 1.000000000000000000 ) ) ;
#34706 = ORIENTED_EDGE ( 'NONE', *, *, #61002, .F. ) ;
#34707 = VECTOR ( 'NONE', #19045, 1000.000000000000000 ) ;
#34708 = AXIS2_PLACEMENT_3D ( 'NONE', #33460, #56419, #36796 ) ;
#34709 = EDGE_CURVE ( 'NONE', #1535, #4351, #52397, .T. ) ;
#34710 = VERTEX_POINT ( 'NONE', #23468 ) ;
#34711 = CIRCLE ( 'NONE', #44321, 82.00000000000000000 ) ;
#34712 = EDGE_CURVE ( 'NONE', #51075, #73312, #28856, .T. ) ;
#34713 = AXIS2_PLACEMENT_3D ( 'NONE', #4149, #15399, #38342 ) ;
#34714 = ADVANCED_FACE ( 'NONE', ( #40766, #63707, #6551 ), #944, .F. ) ;
#34715 = CARTESIAN_POINT ( 'NONE',  ( -93.67500000000003979, 92.29496732002878900, 77.72333333333332916 ) ) ;
#34716 = DIRECTION ( 'NONE',  ( -0.000000000000000000, -0.000000000000000000, 1.000000000000000000 ) ) ;
#34717 = CARTESIAN_POINT ( 'NONE',  ( 10.00000000000000000, 0.000000000000000000, 0.000000000000000000 ) ) ;
#34718 = CARTESIAN_POINT ( 'NONE',  ( 10.00000000000000000, 21.40280677340372151, 36.13751322684426981 ) ) ;
#34719 = DIRECTION ( 'NONE',  ( 1.000000000000000000, -1.047380211910311281E-14, -2.618450529775778123E-14 ) ) ;
#34720 = CYLINDRICAL_SURFACE ( 'NONE', #46931, 31.99999999999998579 ) ;
#34721 = CARTESIAN_POINT ( 'NONE',  ( 1.192633404626820770, -120.9097392825245407, -2.500000000000000000 ) ) ;
#34722 = VECTOR ( 'NONE', #58508, 1000.000000000000000 ) ;
#34723 = VERTEX_POINT ( 'NONE', #37350 ) ;
#34724 = CARTESIAN_POINT ( 'NONE',  ( -95.00000000000002842, 92.66308142843932671, 79.32406250086714294 ) ) ;
#34725 = CARTESIAN_POINT ( 'NONE',  ( 4.250000000000000000, -13.95926121303099343, -1.199999999999999956 ) ) ;
#34726 = CARTESIAN_POINT ( 'NONE',  ( 10.00000000000000000, -33.79645857604525361, 16.45098606841114730 ) ) ;
#34727 = DIRECTION ( 'NONE',  ( 0.000000000000000000, 0.000000000000000000, 1.000000000000000000 ) ) ;
#34728 = CARTESIAN_POINT ( 'NONE',  ( 92.34999999999999432, 90.00000000000002842, 86.82500000000000284 ) ) ;
#34729 = LINE ( 'NONE', #58031, #30381 ) ;
#34730 = CARTESIAN_POINT ( 'NONE',  ( -93.84685191531247028, -211.9973110713294489, 88.10822916753382117 ) ) ;
#34731 =( NAMED_UNIT ( * ) SI_UNIT ( $, .STERADIAN. ) SOLID_ANGLE_UNIT ( ) );
#34732 = EDGE_CURVE ( 'NONE', #51812, #38728, #14476, .T. ) ;
#34733 = AXIS2_PLACEMENT_3D ( 'NONE', #3829, #54939, #60597 ) ;
#34734 = EDGE_CURVE ( 'NONE', #36787, #68327, #14398, .T. ) ;
#34735 =( BOUNDED_CURVE ( )  B_SPLINE_CURVE ( 2, ( #18835, #41776, #30487, #48526, #18114, #1240, #8308 ),
 .UNSPECIFIED., .F., .F. ) 
 B_SPLINE_CURVE_WITH_KNOTS ( ( 3, 2, 2, 3 ),
 ( 0.6666666666666667407, 0.6736111111111112715, 0.6805555555555555802, 0.6875000000000000000 ),
 .UNSPECIFIED. ) 
 CURVE ( )  GEOMETRIC_REPRESENTATION_ITEM ( )  RATIONAL_B_SPLINE_CURVE ( ( 0.9999999999999978906, 0.8660254037844408170, 1.000000000000000000, 0.8660254037844387076, 1.000000000000000000, 0.8660254037844387076, 1.000000000000000000 ) ) 
 REPRESENTATION_ITEM ( '' )  );
#34736 = AXIS2_PLACEMENT_3D ( 'NONE', #60603, #9448, #49662 ) ;
#34737 = CARTESIAN_POINT ( 'NONE',  ( 93.84685191531248449, 91.99731107132950569, 77.63072916753381492 ) ) ;
#34738 = VECTOR ( 'NONE', #13302, 1000.000000000000000 ) ;
#34739 = CIRCLE ( 'NONE', #38335, 42.00000000000000000 ) ;
#34740 = CARTESIAN_POINT ( 'NONE',  ( -93.84685191531247028, -211.9973110713294489, 81.12322916753382174 ) ) ;
#34741 = CARTESIAN_POINT ( 'NONE',  ( 5.000000000000002665, -21.60688246758530440, -79.10210256391390260 ) ) ;
#34742 = ORIENTED_EDGE ( 'NONE', *, *, #65258, .F. ) ;
#34743 = DIRECTION ( 'NONE',  ( 0.000000000000000000, -0.4999999999999998335, 0.8660254037844387076 ) ) ;
#34744 = CARTESIAN_POINT ( 'NONE',  ( -94.99999999999997158, -213.0599564267049857, 76.18874999999999886 ) ) ;
#34745 = AXIS2_PLACEMENT_3D ( 'NONE', #62270, #56635, #26921 ) ;
#34746 = CARTESIAN_POINT ( 'NONE',  ( 11.99999999999999822, 0.000000000000000000, 0.000000000000000000 ) ) ;
#34747 = ADVANCED_FACE ( 'NONE', ( #25680 ), #32046, .F. ) ;
#34748 = ADVANCED_FACE ( 'NONE', ( #71155 ), #70793, .T. ) ;
#34749 = AXIS2_PLACEMENT_3D ( 'NONE', #5535, #69398, #29168 ) ;
#34750 = CIRCLE ( 'NONE', #2375, 15.80000000000028315 ) ;
#34751 = CARTESIAN_POINT ( 'NONE',  ( -92.69370383062505425, 91.33154071421968467, 75.56697916753383026 ) ) ;
#34752 = CARTESIAN_POINT ( 'NONE',  ( 92.69370383062501162, -209.9999999999999716, 76.94281250086713442 ) ) ;
#34753 = EDGE_LOOP ( 'NONE', ( #35853, #37725, #54818, #34119 ) ) ;
#34754 = CYLINDRICAL_SURFACE ( 'NONE', #25111, 32.00000000000000000 ) ;
#34755 = ORIENTED_EDGE ( 'NONE', *, *, #19374, .T. ) ;
#34756 = DIRECTION ( 'NONE',  ( 0.000000000000000000, -0.8660254037844363761, -0.5000000000000039968 ) ) ;
#34757 = EDGE_LOOP ( 'NONE', ( #35050, #42924, #67312, #52090 ) ) ;
#34758 = AXIS2_PLACEMENT_3D ( 'NONE', #22890, #57461, #28884 ) ;
#34759 = CARTESIAN_POINT ( 'NONE',  ( -95.00000000000002842, 93.05995642670504253, 79.12562500173429214 ) ) ;
#34760 = CIRCLE ( 'NONE', #20830, 15.99999999999999645 ) ;
#34761 = AXIS2_PLACEMENT_3D ( 'NONE', #36340, #47269, #13411 ) ;
#34762 = ORIENTED_EDGE ( 'NONE', *, *, #68791, .T. ) ;
#34763 = ORIENTED_EDGE ( 'NONE', *, *, #47024, .F. ) ;
#34764 = VECTOR ( 'NONE', #48637, 1000.000000000000000 ) ;
#34765 = ORIENTED_EDGE ( 'NONE', *, *, #11231, .T. ) ;
#34766 = AXIS2_PLACEMENT_3D ( 'NONE', #43548, #60098, #54437 ) ;
#34767 = CARTESIAN_POINT ( 'NONE',  ( 97.64999999999999147, -209.9999999999999716, 75.07749999999998636 ) ) ;
#34768 = ORIENTED_EDGE ( 'NONE', *, *, #74167, .T. ) ;
#34769 = ORIENTED_EDGE ( 'NONE', *, *, #1935, .T. ) ;
#34770 = CARTESIAN_POINT ( 'NONE',  ( 92.69370383062498320, 90.00000000000002842, 82.81656250086714977 ) ) ;
#34771 = CARTESIAN_POINT ( 'NONE',  ( 92.35000000000002274, -208.4700217866474645, 75.97708333333333997 ) ) ;
#34772 = EDGE_LOOP ( 'NONE', ( #37769, #41184, #3060, #50073 ) ) ;
#34773 = ORIENTED_EDGE ( 'NONE', *, *, #67032, .F. ) ;
#34774 = ORIENTED_EDGE ( 'NONE', *, *, #71626, .T. ) ;
#34775 = EDGE_LOOP ( 'NONE', ( #65244, #44390, #46137, #62735 ) ) ;
#34776 = CARTESIAN_POINT ( 'NONE',  ( 10.00000000000000000, 27.13269053701096922, 25.88420570971410228 ) ) ;
#34777 = CARTESIAN_POINT ( 'NONE',  ( 4.574237413256307008E-15, 3.992474787516313146E-15, 42.00000000000001421 ) ) ;
#34778 = FACE_OUTER_BOUND ( 'NONE', #12414, .T. ) ;
#34779 = CARTESIAN_POINT ( 'NONE',  ( 10.00000000000000000, 0.8261519478441983200, -77.49459641780885022 ) ) ;
#34780 = CARTESIAN_POINT ( 'NONE',  ( -32.50000000000000000, -120.0000000000000000, 102.9091629284897493 ) ) ;
#34781 = LINE ( 'NONE', #41529, #42675 ) ;
#34782 = CARTESIAN_POINT ( 'NONE',  ( 10.00000000000000000, -10.41901085202050403, -40.68715046381940681 ) ) ;
#34783 = CARTESIAN_POINT ( 'NONE',  ( -97.64999999999996305, -209.9999999999999716, 89.90078125043358170 ) ) ;
#34784 = ORIENTED_EDGE ( 'NONE', *, *, #1330, .T. ) ;
#34785 = CARTESIAN_POINT ( 'NONE',  ( -92.34999999999999432, -211.5299782133524502, 78.91395833506763324 ) ) ;
#34786 = ORIENTED_EDGE ( 'NONE', *, *, #59149, .F. ) ;
#34787 = CARTESIAN_POINT ( 'NONE',  ( 10.00000000000000000, 0.000000000000000000, 0.000000000000000000 ) ) ;
#34788 = ORIENTED_EDGE ( 'NONE', *, *, #66787, .F. ) ;
#34790 = CARTESIAN_POINT ( 'NONE',  ( -93.67500000000003979, 92.29496732002878900, 79.70770833506762187 ) ) ;
#34789 = CARTESIAN_POINT ( 'NONE',  ( 97.64999999999997726, 91.52997821335252127, 79.01979166840095559 ) ) ;
#34791 = VECTOR ( 'NONE', #71631, 1000.000000000000000 ) ;
#34792 = ORIENTED_EDGE ( 'NONE', *, *, #26540, .F. ) ;
#34793 = CARTESIAN_POINT ( 'NONE',  ( 96.15314808468748708, 88.00268892867053694, 79.85322916753381151 ) ) ;
#34794 = DIRECTION ( 'NONE',  ( -1.000000000000000000, 0.000000000000000000, 0.000000000000000000 ) ) ;
#34795 = CARTESIAN_POINT ( 'NONE',  ( 11.99999999999999822, 75.11725578898472122, -2.956366410619845730 ) ) ;
#34796 = CIRCLE ( 'NONE', #62447, 42.00000000000000000 ) ;
#34797 = EDGE_CURVE ( 'NONE', #45506, #44699, #20028, .T. ) ;
#34798 = DIRECTION ( 'NONE',  ( 1.000000000000000000, 0.000000000000000000, 0.000000000000000000 ) ) ;
#34799 = CARTESIAN_POINT ( 'NONE',  ( 5.000000000000000000, 41.91543099594818500, -2.663952781846291362 ) ) ;
#34800 = CIRCLE ( 'NONE', #32414, 2.499999999999999556 ) ;
#34801 = EDGE_LOOP ( 'NONE', ( #71658, #74191, #22104, #33172 ) ) ;
#34802 = CARTESIAN_POINT ( 'NONE',  ( 0.000000000000000000, 34.94270380257639630, 74.18225833017899618 ) ) ;
#34803 = CARTESIAN_POINT ( 'NONE',  ( 10.00000000000000000, 12.26510123303259725, 35.53030884539089840 ) ) ;
#34804 = CARTESIAN_POINT ( 'NONE',  ( -97.64999999999996305, -209.9999999999999716, 90.00000000000000000 ) ) ;
#34805 = ORIENTED_EDGE ( 'NONE', *, *, #20042, .F. ) ;
#34806 = EDGE_CURVE ( 'NONE', #63739, #53879, #30086, .T. ) ;
#34807 = ORIENTED_EDGE ( 'NONE', *, *, #15694, .T. ) ;
#34808 = AXIS2_PLACEMENT_3D ( 'NONE', #16317, #4687, #29701 ) ;
#34809 = EDGE_CURVE ( 'NONE', #65173, #9528, #13287, .T. ) ;
#34810 = CYLINDRICAL_SURFACE ( 'NONE', #38454, 31.99999999999999289 ) ;
#34811 = CARTESIAN_POINT ( 'NONE',  ( 11.99999999999999822, -51.29473840253269401, 63.97538442413408433 ) ) ;
#34812 = DIRECTION ( 'NONE',  ( 0.000000000000000000, 0.000000000000000000, -1.000000000000000000 ) ) ;
#34813 = CARTESIAN_POINT ( 'NONE',  ( -94.99999999999997158, -212.6630814284392557, 76.62531250086715318 ) ) ;
#34814 = EDGE_CURVE ( 'NONE', #30208, #11931, #54083, .T. ) ;
#34815 = ORIENTED_EDGE ( 'NONE', *, *, #57470, .T. ) ;
#34816 = AXIS2_PLACEMENT_3D ( 'NONE', #18334, #36734, #36362 ) ;
#34817 = CARTESIAN_POINT ( 'NONE',  ( 11.99999999999999822, 73.72996012237460661, -14.67089635893632504 ) ) ;
#34818 = VECTOR ( 'NONE', #56528, 1000.000000000000114 ) ;
#34819 = AXIS2_PLACEMENT_3D ( 'NONE', #22039, #44981, #10760 ) ;
#34820 = CARTESIAN_POINT ( 'NONE',  ( -96.10855813657714464, -212.3693961633073855, 74.97612907457856579 ) ) ;
#34821 = CARTESIAN_POINT ( 'NONE',  ( 0.000000000000000000, 0.000000000000000000, 0.000000000000000000 ) ) ;
#34822 = CARTESIAN_POINT ( 'NONE',  ( 94.99999999999998579, 92.66308142843932671, 76.14906250086716000 ) ) ;
#34823 = DIRECTION ( 'NONE',  ( -1.000000000000000000, 0.000000000000000000, -0.000000000000000000 ) ) ;
#34824 = CARTESIAN_POINT ( 'NONE',  ( -10.00000000000000000, 0.000000000000000000, 0.000000000000000000 ) ) ;
#34825 = LINE ( 'NONE', #62295, #27708 ) ;
#34826 = AXIS2_PLACEMENT_3D ( 'NONE', #44022, #50008, #49640 ) ;
#34827 = FACE_OUTER_BOUND ( 'NONE', #55224, .T. ) ;
#34828 = AXIS2_PLACEMENT_3D ( 'NONE', #7466, #24748, #7832 ) ;
#34829 = CARTESIAN_POINT ( 'NONE',  ( 0.000000000000000000, 27.75498641678786527, -31.52238457039571173 ) ) ;
#34830 = EDGE_CURVE ( 'NONE', #913, #66848, #2792, .T. ) ;
#34831 = DIRECTION ( 'NONE',  ( -1.000000000000000000, -0.000000000000000000, 0.000000000000000000 ) ) ;
#34832 = ADVANCED_FACE ( 'NONE', ( #65919 ), #8020, .T. ) ;
#34833 = CARTESIAN_POINT ( 'NONE',  ( 92.69370383062498320, 90.00000000000002842, 87.26156250086715715 ) ) ;
#34834 = LINE ( 'NONE', #29170, #21408 ) ;
#34835 = CARTESIAN_POINT ( 'NONE',  ( 0.000000000000000000, 76.66974797899852945, -11.30684508768257679 ) ) ;
#34836 = VERTEX_POINT ( 'NONE', #64810 ) ;
#34837 = CARTESIAN_POINT ( 'NONE',  ( 92.35004028547589883, -211.5300014721827608, 83.14729327728633734 ) ) ;
#34838 = CARTESIAN_POINT ( 'NONE',  ( -96.15314808468751551, 88.00268892867056536, 80.22364583420046813 ) ) ;
#34839 = CARTESIAN_POINT ( 'NONE',  ( 10.00000000000000000, 71.27951684758026829, 30.41916302227139113 ) ) ;
#34840 = ORIENTED_EDGE ( 'NONE', *, *, #54143, .T. ) ;
#34841 = CARTESIAN_POINT ( 'NONE',  ( 0.000000000000000000, 23.16143007188426850, 73.95703589263983702 ) ) ;
#34842 = CARTESIAN_POINT ( 'NONE',  ( 93.67500000000001137, -207.7050326799711968, 87.35416666666665719 ) ) ;
#34843 = FACE_OUTER_BOUND ( 'NONE', #3722, .T. ) ;
#34844 = AXIS2_PLACEMENT_3D ( 'NONE', #59694, #30364, #25104 ) ;
#34845 = DIRECTION ( 'NONE',  ( -1.000000000000000000, 0.000000000000000000, 0.000000000000000000 ) ) ;
#34846 = CARTESIAN_POINT ( 'NONE',  ( 0.000000000000000000, -37.48860685352291711, 0.8828120875899322373 ) ) ;
#34847 = AXIS2_PLACEMENT_3D ( 'NONE', #31166, #4107, #14244 ) ;
#34848 = ORIENTED_EDGE ( 'NONE', *, *, #57057, .F. ) ;
#34849 = ORIENTED_EDGE ( 'NONE', *, *, #70875, .F. ) ;
#34850 = CARTESIAN_POINT ( 'NONE',  ( 95.00000000000000000, -212.6630814284392557, 80.43531250086715545 ) ) ;
#34851 = CARTESIAN_POINT ( 'NONE',  ( -94.99999999999997158, -209.9999999999999716, 90.00000000000000000 ) ) ;
#34852 = CARTESIAN_POINT ( 'NONE',  ( 94.99999999999998579, 90.00000000000002842, 90.00000000000000000 ) ) ;
#34853 = CARTESIAN_POINT ( 'NONE',  ( -97.64999999999996305, -210.0000348529796668, 77.37937620717859488 ) ) ;
#34854 = CARTESIAN_POINT ( 'NONE',  ( 93.67499999999998295, 92.29496732002878900, 83.62354166840097491 ) ) ;
#34855 = DIRECTION ( 'NONE',  ( 0.000000000000000000, 0.000000000000000000, 1.000000000000000000 ) ) ;
#34856 = CARTESIAN_POINT ( 'NONE',  ( 96.32499999999998863, -212.2949673200287179, 85.76666666666665151 ) ) ;
#34857 = EDGE_CURVE ( 'NONE', #38997, #67308, #8476, .T. ) ;
#34858 = VECTOR ( 'NONE', #32387, 1000.000000000000000 ) ;
#34859 = EDGE_LOOP ( 'NONE', ( #6763, #329 ) ) ;
#34860 = ORIENTED_EDGE ( 'NONE', *, *, #60813, .T. ) ;
#34861 = ORIENTED_EDGE ( 'NONE', *, *, #16413, .F. ) ;
#34862 = CONICAL_SURFACE ( 'NONE', #54079, 4.749999999999999112, 0.4572823821333981131 ) ;
#34863 = ORIENTED_EDGE ( 'NONE', *, *, #26415, .T. ) ;
#34864 = CARTESIAN_POINT ( 'NONE',  ( 0.000000000000000000, -71.27951684758005513, -30.41916302227188851 ) ) ;
#34865 = CIRCLE ( 'NONE', #33684, 3.299999999999997158 ) ;
#34866 =( NAMED_UNIT ( * ) PLANE_ANGLE_UNIT ( ) SI_UNIT ( $, .RADIAN. ) );
#34867 = CARTESIAN_POINT ( 'NONE',  ( -96.15314808468752972, 91.99731107132950569, 85.88572916753381037 ) ) ;
#34868 = LINE ( 'NONE', #51042, #25722 ) ;
#34869 = ADVANCED_FACE ( 'NONE', ( #47506 ), #8764, .F. ) ;
#34870 = AXIS2_PLACEMENT_3D ( 'NONE', #14763, #9123, #59910 ) ;
#34871 = DIRECTION ( 'NONE',  ( -0.000000000000000000, -0.000000000000000000, 1.000000000000000000 ) ) ;
#34872 = CARTESIAN_POINT ( 'NONE',  ( 97.64999999999997726, -208.4700217866474645, 76.47979166840096354 ) ) ;
#34874 = CIRCLE ( 'NONE', #49244, 82.00000000000000000 ) ;
#34873 = CARTESIAN_POINT ( 'NONE',  ( 92.34999999999999432, 90.00000000000002842, 77.93499999999998806 ) ) ;
#34875 = EDGE_CURVE ( 'NONE', #23361, #14859, #60107, .T. ) ;
#34876 = ORIENTED_EDGE ( 'NONE', *, *, #51461, .F. ) ;
#34877 = CARTESIAN_POINT ( 'NONE',  ( 92.35000000005783249, -210.0000112241611703, 75.47473230081648410 ) ) ;
#34878 = ORIENTED_EDGE ( 'NONE', *, *, #13717, .T. ) ;
#34879 = DIRECTION ( 'NONE',  ( 0.000000000000000000, 0.000000000000000000, 1.000000000000000000 ) ) ;
#34880 = VERTEX_POINT ( 'NONE', #53885 ) ;
#34881 = DIRECTION ( 'NONE',  ( -1.000000000000000000, 0.000000000000000000, 0.000000000000000000 ) ) ;
#34882 = CARTESIAN_POINT ( 'NONE',  ( -96.15314808468752972, 91.99731107132950569, 80.17072916753382117 ) ) ;
#34883 = CARTESIAN_POINT ( 'NONE',  ( 92.69370383062498320, 88.66845928578037217, 88.58447916753382856 ) ) ;
#34884 = VERTEX_POINT ( 'NONE', #13288 ) ;
#34885 = CARTESIAN_POINT ( 'NONE',  ( 10.00000000000000000, 37.58145647212453611, 16.68533520207917675 ) ) ;
#34886 = EDGE_CURVE ( 'NONE', #72362, #18854, #24098, .T. ) ;
#34887 = DIRECTION ( 'NONE',  ( 0.000000000000000000, 0.000000000000000000, 1.000000000000000000 ) ) ;
#34888 = DIRECTION ( 'NONE',  ( -1.000000000000000000, -0.000000000000000000, -0.000000000000000000 ) ) ;
#34889 = CARTESIAN_POINT ( 'NONE',  ( -93.26027265873601380, 91.51405112163766375, 74.79348190356853365 ) ) ;
#34890 = ORIENTED_EDGE ( 'NONE', *, *, #11525, .F. ) ;
#34891 = CARTESIAN_POINT ( 'NONE',  ( -3.000000000000000000, -3.948201729842348850, 23.21447184625293048 ) ) ;
#34892 = CARTESIAN_POINT ( 'NONE',  ( -93.84685191531247028, -211.9973110713294489, 78.42447916753381776 ) ) ;
#34893 = ORIENTED_EDGE ( 'NONE', *, *, #63875, .T. ) ;
#34894 = ORIENTED_EDGE ( 'NONE', *, *, #7414, .T. ) ;
#34895 = CARTESIAN_POINT ( 'NONE',  ( 10.00000000000000000, -41.76937507738745836, -62.50329211542482710 ) ) ;
#34896 = ORIENTED_EDGE ( 'NONE', *, *, #71282, .T. ) ;
#34897 = CARTESIAN_POINT ( 'NONE',  ( 15.00000000000000000, 5.835314593368777558, 22.81335362449846471 ) ) ;
#34898 = FACE_OUTER_BOUND ( 'NONE', #25339, .T. ) ;
#34899 = ORIENTED_EDGE ( 'NONE', *, *, #60762, .F. ) ;
#34900 = CARTESIAN_POINT ( 'NONE',  ( -96.15314808468747287, -208.0026889286704943, 87.79072916753381151 ) ) ;
#34901 = ORIENTED_EDGE ( 'NONE', *, *, #34225, .F. ) ;
#34903 = ADVANCED_FACE ( 'NONE', ( #19298 ), #8398, .T. ) ;
#34902 = CARTESIAN_POINT ( 'NONE',  ( 11.99999999999999822, 0.000000000000000000, 0.000000000000000000 ) ) ;
#34904 = DIRECTION ( 'NONE',  ( -1.000000000000000000, 0.000000000000000000, 0.000000000000000000 ) ) ;
#34905 = ORIENTED_EDGE ( 'NONE', *, *, #2758, .F. ) ;
#34906 = ORIENTED_EDGE ( 'NONE', *, *, #52186, .F. ) ;
#34907 = VECTOR ( 'NONE', #13452, 999.9999999999998863 ) ;
#34908 = B_SPLINE_CURVE_WITH_KNOTS ( 'NONE', 3,
 ( #71140, #65530, #36945, #26025, #59893, #38054, #54251, #20399, #49330, #37699, #25664, #3494, #26401, #9476, #4231, #56474, #5347, #39545, #73364, #22249 ),
 .UNSPECIFIED., .F., .F.,
 ( 4, 2, 2, 2, 2, 2, 2, 2, 2, 4 ),
 ( 2.781148944365360171E-07, 0.0008372784139787578517, 0.001674278713063079033, 0.002511279012147400649, 0.003348279311231721830, 0.003766779460773882204, 0.004185279610316042578, 0.005022279909400362459, 0.005859280208484684074, 0.006696280507569004822 ),
 .UNSPECIFIED. ) ;
#34909 = DIRECTION ( 'NONE',  ( -1.000000000000000000, 0.000000000000000000, 0.000000000000000000 ) ) ;
#34910 = AXIS2_PLACEMENT_3D ( 'NONE', #49038, #71965, #25385 ) ;
#34911 = DIRECTION ( 'NONE',  ( -1.000000000000000000, 0.000000000000000000, 0.000000000000000000 ) ) ;
#34912 = CARTESIAN_POINT ( 'NONE',  ( 94.99999999999998579, 87.33691857156068750, 85.35656250086714181 ) ) ;
#34913 = DIRECTION ( 'NONE',  ( 0.000000000000000000, -0.2334453638559126909, 0.9723699203976748917 ) ) ;
#34914 = CARTESIAN_POINT ( 'NONE',  ( -92.35000000000003695, 90.00000000000004263, 75.71250000000000568 ) ) ;
#34915 = DIRECTION ( 'NONE',  ( -1.000000000000000000, 0.000000000000000000, 0.000000000000000000 ) ) ;
#34916 = CARTESIAN_POINT ( 'NONE',  ( -11.69999999999999929, 2.571758278209441267E-15, 20.99999999999999645 ) ) ;
#34917 = CARTESIAN_POINT ( 'NONE',  ( 10.00000000000000000, -12.42422080174663712, 35.38097989696507994 ) ) ;
#34918 = ADVANCED_FACE ( 'NONE', ( #2432 ), #25321, .T. ) ;
#34919 = DIRECTION ( 'NONE',  ( -1.000000000000000000, 7.331661483372147883E-15, 2.592266024478009537E-14 ) ) ;
#34920 = CARTESIAN_POINT ( 'NONE',  ( 0.000000000000000000, 35.95386929396241271, 10.96151621346552751 ) ) ;
#34921 = EDGE_CURVE ( 'NONE', #44983, #70418, #45101, .T. ) ;
#34922 = EDGE_CURVE ( 'NONE', #18301, #61409, #16904, .T. ) ;
#34923 = FACE_OUTER_BOUND ( 'NONE', #62903, .T. ) ;
#34924 = AXIS2_PLACEMENT_3D ( 'NONE', #34248, #5699, #45556 ) ;
#34925 = FACE_OUTER_BOUND ( 'NONE', #57913, .T. ) ;
#34926 = CARTESIAN_POINT ( 'NONE',  ( 10.00000000000000000, -22.74946021919153694, 29.81001611431000597 ) ) ;
#34927 = AXIS2_PLACEMENT_3D ( 'NONE', #37405, #60702, #59211 ) ;
#34928 = CARTESIAN_POINT ( 'NONE',  ( 92.35000000000000853, -209.9999999999999716, 90.00000000000000000 ) ) ;
#34929 = AXIS2_PLACEMENT_3D ( 'NONE', #52204, #56757, #51839 ) ;
#34930 = DIRECTION ( 'NONE',  ( -1.000000000000000000, 0.000000000000000000, -0.000000000000000000 ) ) ;
#34931 = ORIENTED_EDGE ( 'NONE', *, *, #7164, .T. ) ;
#34932 = DIRECTION ( 'NONE',  ( -1.000000000000000000, -0.000000000000000000, 0.000000000000000000 ) ) ;
#34933 = DIRECTION ( 'NONE',  ( -1.000000000000000000, 0.000000000000000000, 0.000000000000000000 ) ) ;
#34934 = DIRECTION ( 'NONE',  ( 0.000000000000000000, 0.000000000000000000, 1.000000000000000000 ) ) ;
#34935 = DIRECTION ( 'NONE',  ( -1.000000000000000000, -0.000000000000000000, -0.000000000000000000 ) ) ;
#34936 = CARTESIAN_POINT ( 'NONE',  ( 10.00000000000000000, 0.000000000000000000, 37.49900000000000233 ) ) ;
#34937 = CARTESIAN_POINT ( 'NONE',  ( 93.84685191531251292, -211.9973110713294489, 86.73239583420048859 ) ) ;
#34938 = ORIENTED_EDGE ( 'NONE', *, *, #32246, .F. ) ;
#34939 = VERTEX_POINT ( 'NONE', #61642 ) ;
#34940 = DIRECTION ( 'NONE',  ( -2.603472992746261562E-14, -2.546204323184492723E-14, 1.000000000000000000 ) ) ;
#34941 = ORIENTED_EDGE ( 'NONE', *, *, #7917, .F. ) ;
#34942 = CARTESIAN_POINT ( 'NONE',  ( 93.67500000000001137, -207.7050326799711968, 88.62416666666665321 ) ) ;
#34943 = DIRECTION ( 'NONE',  ( 0.000000000000000000, 0.000000000000000000, 1.000000000000000000 ) ) ;
#34944 = VERTEX_POINT ( 'NONE', #59518 ) ;
#34945 = CARTESIAN_POINT ( 'NONE',  ( 93.84685191531251292, -211.9973110713294489, 81.65239583420049030 ) ) ;
#34946 = ADVANCED_FACE ( 'NONE', ( #8004 ), #55992, .T. ) ;
#34947 = CIRCLE ( 'NONE', #12085, 35.50000000000000711 ) ;
#34948 = AXIS2_PLACEMENT_3D ( 'NONE', #13697, #49019, #14443 ) ;
#34949 = ORIENTED_EDGE ( 'NONE', *, *, #15644, .T. ) ;
#34950 = LINE ( 'NONE', #57889, #50318 ) ;
#34951 = VERTEX_POINT ( 'NONE', #53866 ) ;
#34952 = CIRCLE ( 'NONE', #12140, 16.00000000000000000 ) ;
#34953 = ORIENTED_EDGE ( 'NONE', *, *, #65043, .F. ) ;
#34954 = DIRECTION ( 'NONE',  ( -1.000000000000000000, 0.000000000000000000, 0.000000000000000000 ) ) ;
#34955 =( LENGTH_UNIT ( ) NAMED_UNIT ( * ) SI_UNIT ( .MILLI., .METRE. ) );
#34956 = CARTESIAN_POINT ( 'NONE',  ( 10.00000000000000000, 0.000000000000000000, 0.000000000000000000 ) ) ;
#34957 = EDGE_CURVE ( 'NONE', #9632, #60502, #52901, .T. ) ;
#34958 = EDGE_LOOP ( 'NONE', ( #33919, #73103, #34227, #60378 ) ) ;
#34959 = CARTESIAN_POINT ( 'NONE',  ( 0.000000000000000000, -33.80338159004296017, 16.23288003029484727 ) ) ;
#34960 = CARTESIAN_POINT ( 'NONE',  ( 97.64999999999997726, -211.5299782133524502, 88.43895833506762472 ) ) ;
#34961 = EDGE_CURVE ( 'NONE', #61399, #21904, #33049, .T. ) ;
#34962 = EDGE_LOOP ( 'NONE', ( #55957, #7823, #5300, #45431 ) ) ;
#34963 = CARTESIAN_POINT ( 'NONE',  ( 11.99999999999999822, -62.50329211542465657, 41.76937507738766442 ) ) ;
#34964 = ORIENTED_EDGE ( 'NONE', *, *, #35070, .F. ) ;
#34965 =( BOUNDED_CURVE ( )  B_SPLINE_CURVE ( 2, ( #22519, #23258, #45835, #68757, #62766, #53573, #63131 ),
 .UNSPECIFIED., .F., .F. ) 
 B_SPLINE_CURVE_WITH_KNOTS ( ( 3, 2, 2, 3 ),
 ( 0.5416666666666665186, 0.5486111111111110494, 0.5555555555555553582, 0.5624999999999997780 ),
 .UNSPECIFIED. ) 
 CURVE ( )  GEOMETRIC_REPRESENTATION_ITEM ( )  RATIONAL_B_SPLINE_CURVE ( ( 1.000000000000002220, 0.8660254037844365982, 1.000000000000000000, 0.8660254037844387076, 1.000000000000000000, 0.8660254037844430375, 0.9999999999999956701 ) ) 
 REPRESENTATION_ITEM ( '' )  );
#34966 = CARTESIAN_POINT ( 'NONE',  ( 5.000000000000000888, -2.488288133785820033, -1.689848211693934621 ) ) ;
#34967 = ORIENTED_EDGE ( 'NONE', *, *, #27582, .F. ) ;
#34968 = ADVANCED_FACE ( 'NONE', ( #4514 ), #50719, .F. ) ;
#34969 = ORIENTED_EDGE ( 'NONE', *, *, #45269, .T. ) ;
#34970 = ORIENTED_EDGE ( 'NONE', *, *, #26808, .T. ) ;
#34971 = DIRECTION ( 'NONE',  ( -1.000000000000000000, 0.000000000000000000, 0.000000000000000000 ) ) ;
#34972 = VECTOR ( 'NONE', #65881, 1000.000000000000000 ) ;
#34973 = CARTESIAN_POINT ( 'NONE',  ( -10.00000000000000000, 0.000000000000000000, 0.000000000000000000 ) ) ;
#34974 = ORIENTED_EDGE ( 'NONE', *, *, #66489, .T. ) ;
#34975 = CIRCLE ( 'NONE', #69787, 23.50000000000000355 ) ;
#34976 = ORIENTED_EDGE ( 'NONE', *, *, #60380, .T. ) ;
#34977 = ORIENTED_EDGE ( 'NONE', *, *, #6625, .F. ) ;
#34978 = CARTESIAN_POINT ( 'NONE',  ( 11.99999999999999822, 72.35432306680455383, 20.40083707023012494 ) ) ;
#34979 = CIRCLE ( 'NONE', #45842, 37.49900000000000233 ) ;
#34980 = DIRECTION ( 'NONE',  ( -0.9997280174009349762, 0.02332147558787674504, 0.000000000000000000 ) ) ;
#34981 = CARTESIAN_POINT ( 'NONE',  ( -92.35000000000005116, 88.47002178664754979, 87.72458333333332803 ) ) ;
#34982 = VERTEX_POINT ( 'NONE', #65531 ) ;
#34983 = CARTESIAN_POINT ( 'NONE',  ( 93.67500000000001137, -207.7050326799711968, 89.89416666666666345 ) ) ;
#34984 = CIRCLE ( 'NONE', #38582, 11.59999999999999964 ) ;
#34985 = VERTEX_POINT ( 'NONE', #20011 ) ;
#34986 = DIRECTION ( 'NONE',  ( -1.000000000000000000, -0.000000000000000000, -0.000000000000000000 ) ) ;
#34987 = CARTESIAN_POINT ( 'NONE',  ( -96.15314808468745866, -211.9973110713294489, 85.93864583420048575 ) ) ;
#34988 = ORIENTED_EDGE ( 'NONE', *, *, #59612, .F. ) ;
#34990 = EDGE_CURVE ( 'NONE', #32052, #70437, #71882, .T. ) ;
#34989 = LINE ( 'NONE', #51532, #54228 ) ;
#34991 = FACE_OUTER_BOUND ( 'NONE', #3004, .T. ) ;
#34992 = CARTESIAN_POINT ( 'NONE',  ( 5.000000000000000000, -39.04073710021332744, -15.48615015657624205 ) ) ;
#34993 = CARTESIAN_POINT ( 'NONE',  ( -93.84685191531247028, -211.9973110713294489, 77.15447916753380753 ) ) ;
#34994 = DIRECTION ( 'NONE',  ( 0.000000000000000000, 0.000000000000000000, 1.000000000000000000 ) ) ;
#34995 = DIRECTION ( 'NONE',  ( 1.000000000000000000, 0.000000000000000000, 0.000000000000000000 ) ) ;
#34996 = DIRECTION ( 'NONE',  ( -1.000000000000000000, 0.000000000000000000, 0.000000000000000000 ) ) ;
#34997 = DIRECTION ( 'NONE',  ( 0.000000000000000000, 0.000000000000000000, 1.000000000000000000 ) ) ;
#34998 = CARTESIAN_POINT ( 'NONE',  ( 12.00000000000000000, -18.13022148937242761, 15.02647892043569122 ) ) ;
#34999 = CARTESIAN_POINT ( 'NONE',  ( 93.67499999999999716, 87.70503267997126784, 80.02520833506763154 ) ) ;
#35000 = EDGE_CURVE ( 'NONE', #67617, #16833, #62019, .T. ) ;
#35001 = CARTESIAN_POINT ( 'NONE',  ( -96.15314808468752972, 91.99731107132950569, 80.01197916753380923 ) ) ;
#35002 = DIRECTION ( 'NONE',  ( 0.000000000000000000, 1.000000000000000000, 3.491481338843133355E-15 ) ) ;
#35003 = CARTESIAN_POINT ( 'NONE',  ( 10.00000000000000000, 22.74946021919175720, -29.81001611430984255 ) ) ;
#35004 = EDGE_CURVE ( 'NONE', #56502, #65113, #8522, .T. ) ;
#35005 = ORIENTED_EDGE ( 'NONE', *, *, #5448, .T. ) ;
#35006 = CARTESIAN_POINT ( 'NONE',  ( 10.00000000000000000, 22.74946021919133088, 29.81001611431016229 ) ) ;
#35007 = MECHANICAL_DESIGN_GEOMETRIC_PRESENTATION_REPRESENTATION (  '', ( #54171 ), #57822 ) ;
#35008 = CIRCLE ( 'NONE', #6198, 23.50000000000041922 ) ;
#35009 = AXIS2_PLACEMENT_3D ( 'NONE', #42226, #61265, #38700 ) ;
#35010 = CARTESIAN_POINT ( 'NONE',  ( -23.97194136764370853, -131.3950000906648938, 2.500000000000000000 ) ) ;
#35011 = PLANE ( 'NONE',  #65791 ) ;
#35012 = DIRECTION ( 'NONE',  ( 1.000000000000000000, -0.000000000000000000, 0.000000000000000000 ) ) ;
#35013 = CARTESIAN_POINT ( 'NONE',  ( 4.999999999999999112, 9.188173127307294408, 40.98264845739752360 ) ) ;
#35014 = AXIS2_PLACEMENT_3D ( 'NONE', #72248, #59138, #9102 ) ;
#35015 = CARTESIAN_POINT ( 'NONE',  ( 92.35000000000000853, -209.9999999999999716, 78.57000000000000739 ) ) ;
#35016 = CARTESIAN_POINT ( 'NONE',  ( -96.15314808468747287, -208.0026889286704943, 75.72572916753382799 ) ) ;
#35017 = AXIS2_PLACEMENT_3D ( 'NONE', #69103, #40520, #46532 ) ;
#35018 = CARTESIAN_POINT ( 'NONE',  ( 0.000000000000000000, -39.04073710021356192, 15.48615015657568073 ) ) ;
#35019 = EDGE_LOOP ( 'NONE', ( #29855, #23656, #29689, #25499 ) ) ;
#35020 = DIRECTION ( 'NONE',  ( -0.8225049752423776450, -0.5687579148473765889, 0.000000000000000000 ) ) ;
#35021 = DIRECTION ( 'NONE',  ( 1.000000000000000000, 1.427937372958405461E-15, 7.962523111839130290E-16 ) ) ;
#35022 = DIRECTION ( 'NONE',  ( -1.000000000000000000, -0.000000000000000000, -0.000000000000000000 ) ) ;
#35023 = CARTESIAN_POINT ( 'NONE',  ( 10.00000000000000000, -41.81611651403864727, 3.925862922256025289 ) ) ;
#35024 = CIRCLE ( 'NONE', #51827, 82.00000000000000000 ) ;
#35025 = DIRECTION ( 'NONE',  ( 1.000000000000000000, 0.000000000000000000, 0.000000000000000000 ) ) ;
#35026 = EDGE_LOOP ( 'NONE', ( #74139, #34347, #42470, #51900 ) ) ;
#35027 = DIRECTION ( 'NONE',  ( 1.000000000000000000, -0.000000000000000000, 0.000000000000000000 ) ) ;
#35028 =( NAMED_UNIT ( * ) PLANE_ANGLE_UNIT ( ) SI_UNIT ( $, .RADIAN. ) );
#35029 = VERTEX_POINT ( 'NONE', #50348 ) ;
#35030 = EDGE_CURVE ( 'NONE', #56011, #54022, #8379, .T. ) ;
#35031 = CARTESIAN_POINT ( 'NONE',  ( 97.30629616937498838, -208.6684592857803295, 86.20322916753380582 ) ) ;
#35032 = DIRECTION ( 'NONE',  ( 0.000000000000000000, 0.000000000000000000, 1.000000000000000000 ) ) ;
#35033 = EDGE_LOOP ( 'NONE', ( #29576, #71959, #70611, #5451 ) ) ;
#35034 = EDGE_CURVE ( 'NONE', #26649, #72759, #73277, .T. ) ;
#35035 = DIRECTION ( 'NONE',  ( 1.000000000000000000, 0.000000000000000000, 0.000000000000000000 ) ) ;
#35036 = VERTEX_POINT ( 'NONE', #14000 ) ;
#35037 = DIRECTION ( 'NONE',  ( -1.000000000000000000, -0.000000000000000000, 0.000000000000000000 ) ) ;
#35038 = VERTEX_POINT ( 'NONE', #36946 ) ;
#35039 = CARTESIAN_POINT ( 'NONE',  ( -95.00000000000002842, 92.66308142843932671, 79.48281250086715488 ) ) ;
#35040 = EDGE_CURVE ( 'NONE', #21350, #19673, #36146, .T. ) ;
#35041 = ORIENTED_EDGE ( 'NONE', *, *, #18076, .F. ) ;
#35042 = EDGE_LOOP ( 'NONE', ( #28484, #43570, #50695, #34025 ) ) ;
#35043 = EDGE_CURVE ( 'NONE', #8298, #29646, #13345, .T. ) ;
#35044 = ORIENTED_EDGE ( 'NONE', *, *, #14190, .T. ) ;
#35045 = DIRECTION ( 'NONE',  ( 1.000000000000000000, 0.000000000000000000, 0.000000000000000000 ) ) ;
#35046 = EDGE_LOOP ( 'NONE', ( #24504, #22574, #1003, #36978 ) ) ;
#35047 = DIRECTION ( 'NONE',  ( 0.9997280174009349762, -0.02332147558787674158, 0.000000000000000000 ) ) ;
#35048 = ORIENTED_EDGE ( 'NONE', *, *, #2162, .T. ) ;
#35049 = DIRECTION ( 'NONE',  ( 0.000000000000000000, -0.4539904997395350361, -0.8910065241883738940 ) ) ;
#35050 = ORIENTED_EDGE ( 'NONE', *, *, #68329, .F. ) ;
#35051 = EDGE_CURVE ( 'NONE', #58070, #41704, #33638, .T. ) ;
#35052 = STYLED_ITEM ( 'NONE', ( #24790 ), #65097 ) ;
#35053 = CIRCLE ( 'NONE', #17024, 37.49900000000000233 ) ;
#35054 = ORIENTED_EDGE ( 'NONE', *, *, #3770, .T. ) ;
#35055 = CARTESIAN_POINT ( 'NONE',  ( 92.69370383062498320, 91.33154071421968467, 85.77989583420048803 ) ) ;
#35056 = EDGE_LOOP ( 'NONE', ( #28218, #55013, #50638, #42527 ) ) ;
#35057 = CARTESIAN_POINT ( 'NONE',  ( 95.00000000000000000, -207.3369185715606307, 81.86406250086714920 ) ) ;
#35058 = PRODUCT_CONTEXT ( 'NONE', #16238, 'mechanical' ) ;
#35059 = DIRECTION ( 'NONE',  ( 1.000000000000000000, 0.000000000000000000, 0.000000000000000000 ) ) ;
#35061 = CYLINDRICAL_SURFACE ( 'NONE', #25785, 16.00000000000000000 ) ;
#35060 = AXIS2_PLACEMENT_3D ( 'NONE', #31936, #19910, #65795 ) ;
#35062 = CARTESIAN_POINT ( 'NONE',  ( 95.00000000000000000, -206.9400435732949575, 79.04624999999997215 ) ) ;
#35063 = FACE_OUTER_BOUND ( 'NONE', #51323, .T. ) ;
#35064 = CARTESIAN_POINT ( 'NONE',  ( -93.67500000000003979, 87.70503267997129626, 79.41666666666665719 ) ) ;
#35065 = DIRECTION ( 'NONE',  ( 0.000000000000000000, 0.000000000000000000, -1.000000000000000000 ) ) ;
#35066 = CARTESIAN_POINT ( 'NONE',  ( -92.69370383062498320, -211.3315407142195852, 85.46239583420047836 ) ) ;
#35067 = CARTESIAN_POINT ( 'NONE',  ( -93.84685191531254134, 91.99731107132950569, 81.33489583420049485 ) ) ;
#35068 = AXIS2_PLACEMENT_3D ( 'NONE', #22605, #45550, #69204 ) ;
#35069 = ORIENTED_EDGE ( 'NONE', *, *, #15215, .T. ) ;
#35070 = EDGE_CURVE ( 'NONE', #14784, #4987, #33737, .T. ) ;
#35071 = CARTESIAN_POINT ( 'NONE',  ( 93.84685191531248449, 88.00268892867053694, 85.30364583420046642 ) ) ;
#35072 = VERTEX_POINT ( 'NONE', #17261 ) ;
#35073 = DIRECTION ( 'NONE',  ( 0.000000000000000000, -0.9723699203976741146, -0.2334453638559159938 ) ) ;
#35075 = EDGE_CURVE ( 'NONE', #60043, #1351, #27724, .T. ) ;
#35074 = DIRECTION ( 'NONE',  ( -1.000000000000000000, 0.000000000000000000, 0.000000000000000000 ) ) ;
#35076 = DIRECTION ( 'NONE',  ( -1.000000000000000000, 0.000000000000000000, -0.000000000000000000 ) ) ;
#35077 = CARTESIAN_POINT ( 'NONE',  ( 96.32499999999998863, -207.7050326799711968, 85.34333333333333371 ) ) ;
#35078 = CARTESIAN_POINT ( 'NONE',  ( -93.84685191531248449, -208.0026889286704943, 85.62114583420046188 ) ) ;
#35079 = CYLINDRICAL_SURFACE ( 'NONE', #51080, 82.00000000000000000 ) ;
#35080 = CARTESIAN_POINT ( 'NONE',  ( -92.35000000035638834, 89.99995654222792041, 89.12687334326074051 ) ) ;
#35081 = CARTESIAN_POINT ( 'NONE',  ( -10.00000000000000000, 0.000000000000000000, 0.000000000000000000 ) ) ;
#35082 = VECTOR ( 'NONE', #42716, 1000.000000000000000 ) ;
#35083 = ADVANCED_FACE ( 'NONE', ( #34925 ), #63144, .T. ) ;
#35084 = EDGE_CURVE ( 'NONE', #34944, #37007, #74021, .T. ) ;
#35085 = PLANE ( 'NONE',  #3487 ) ;
#35086 = ORIENTED_EDGE ( 'NONE', *, *, #28573, .T. ) ;
#35087 = AXIS2_PLACEMENT_3D ( 'NONE', #54237, #13988, #24908 ) ;
#35088 = ORIENTED_EDGE ( 'NONE', *, *, #49964, .T. ) ;
#35089 = CARTESIAN_POINT ( 'NONE',  ( -96.32500000000001705, 92.29496732002878900, 76.55916666666666970 ) ) ;
#35090 = CARTESIAN_POINT ( 'NONE',  ( -95.00000000002611955, 90.00000000000007105, -75.00000000000000000 ) ) ;
#35091 = EDGE_CURVE ( 'NONE', #73994, #35854, #69751, .T. ) ;
#35092 = CARTESIAN_POINT ( 'NONE',  ( -93.84685191531254134, 91.99731107132950569, 88.16114583420046813 ) ) ;
#35093 = CARTESIAN_POINT ( 'NONE',  ( 0.000000000000000000, 6.555932627142418312, 37.01155633439060466 ) ) ;
#35094 = DIRECTION ( 'NONE',  ( -2.628368902995164490E-16, -1.000000000000000000, 0.000000000000000000 ) ) ;
#35095 = CARTESIAN_POINT ( 'NONE',  ( -3.000000000000000000, -1.278221433540145391, -26.51162292216073979 ) ) ;
#35096 = DIRECTION ( 'NONE',  ( -1.000000000000000000, 0.000000000000000000, 0.000000000000000000 ) ) ;
#35097 = EDGE_LOOP ( 'NONE', ( #22019, #44056, #51960, #42506 ) ) ;
#35098 = CARTESIAN_POINT ( 'NONE',  ( -97.30629616937501680, 88.66845928578038638, 77.63072916753380071 ) ) ;
#35099 = EDGE_CURVE ( 'NONE', #2787, #19205, #63507, .T. ) ;
#35100 = CARTESIAN_POINT ( 'NONE',  ( -22.53294031248082163, -134.0273518838794757, 5.500000000000000000 ) ) ;
#35101 = DIRECTION ( 'NONE',  ( 0.000000000000000000, -0.9723699203976789995, 0.2334453638558956490 ) ) ;
#35102 = LINE ( 'NONE', #29811, #39470 ) ;
#35103 = CARTESIAN_POINT ( 'NONE',  ( 97.64999999999999147, -210.0000000255706709, 84.04687500080852658 ) ) ;
#35104 = CARTESIAN_POINT ( 'NONE',  ( 10.00000000000000000, -63.18004540532994184, -44.88180994100446952 ) ) ;
#35105 = CARTESIAN_POINT ( 'NONE',  ( -97.30629616937495996, -209.9999999999999716, 85.35656250086715602 ) ) ;
#35106 = LINE ( 'NONE', #58400, #35 ) ;
#35107 = CARTESIAN_POINT ( 'NONE',  ( 92.69370383062498320, 88.66845928578035796, 77.15447916753382174 ) ) ;
#35108 = CARTESIAN_POINT ( 'NONE',  ( -94.99999999999997158, -207.3369185715606307, 75.67281250086715261 ) ) ;
#35109 = CYLINDRICAL_SURFACE ( 'NONE', #25420, 82.00000000000000000 ) ;
#35110 = ORIENTED_EDGE ( 'NONE', *, *, #33616, .F. ) ;
#35111 = CARTESIAN_POINT ( 'NONE',  ( -92.35000000002600018, 89.99998827382285072, 82.77687459617033028 ) ) ;
#35112 = CARTESIAN_POINT ( 'NONE',  ( -97.65000000000001990, 90.00000000000004263, 82.37999999999999545 ) ) ;
#35113 = CARTESIAN_POINT ( 'NONE',  ( 12.00000000000000000, 8.688484142254226938, 21.88630264137359305 ) ) ;
#35114 = CARTESIAN_POINT ( 'NONE',  ( -96.15314808468752972, 91.99731107132950569, 75.72572916753382799 ) ) ;
#35115 = CARTESIAN_POINT ( 'NONE',  ( 97.30629616937498838, -211.3315407142195852, 77.84239583420045960 ) ) ;
#35116 = ORIENTED_EDGE ( 'NONE', *, *, #71633, .T. ) ;
#35117 = CONICAL_SURFACE ( 'NONE', #2747, 2.449999999999998845, 0.9599310885968813656 ) ;
#35118 = CARTESIAN_POINT ( 'NONE',  ( 10.00000000000000000, 37.48860685352291000, -0.8828120875901940279 ) ) ;
#35119 = ORIENTED_EDGE ( 'NONE', *, *, #35867, .F. ) ;
#35120 = VECTOR ( 'NONE', #71671, 1000.000000000000000 ) ;
#35121 = CARTESIAN_POINT ( 'NONE',  ( 11.99999999999999822, 75.11725578898467859, 2.956366410620910656 ) ) ;
#35122 = EDGE_LOOP ( 'NONE', ( #69723, #38672, #24637, #71523 ) ) ;
#35123 = EDGE_CURVE ( 'NONE', #28591, #54942, #22537, .T. ) ;
#35124 = AXIS2_PLACEMENT_3D ( 'NONE', #47389, #36103, #19177 ) ;
#35125 = DIRECTION ( 'NONE',  ( 0.000000000000000000, 0.000000000000000000, 1.000000000000000000 ) ) ;
#35126 = AXIS2_PLACEMENT_3D ( 'NONE', #69933, #2302, #47390 ) ;
#35127 = EDGE_CURVE ( 'NONE', #14793, #48891, #29263, .T. ) ;
#35128 = ORIENTED_EDGE ( 'NONE', *, *, #72115, .F. ) ;
#35129 = ORIENTED_EDGE ( 'NONE', *, *, #2529, .T. ) ;
#35131 = VERTEX_POINT ( 'NONE', #16514 ) ;
#35130 = EDGE_CURVE ( 'NONE', #18028, #36077, #24016, .T. ) ;
#35132 = EDGE_CURVE ( 'NONE', #32115, #63620, #57487, .T. ) ;
#35133 = ORIENTED_EDGE ( 'NONE', *, *, #31971, .F. ) ;
#35134 = EDGE_LOOP ( 'NONE', ( #41047, #63380, #10239, #69335 ) ) ;
#35135 = CARTESIAN_POINT ( 'NONE',  ( 92.69370383062498320, 91.33154071421968467, 82.12864583420048348 ) ) ;
#35136 = CARTESIAN_POINT ( 'NONE',  ( 97.64999999999997726, -211.5299782133524502, 75.65958333333333030 ) ) ;
#35137 = ORIENTED_EDGE ( 'NONE', *, *, #15148, .F. ) ;
#35138 = VERTEX_POINT ( 'NONE', #33807 ) ;
#35139 = ORIENTED_EDGE ( 'NONE', *, *, #68502, .T. ) ;
#35140 = EDGE_LOOP ( 'NONE', ( #37939, #29978, #72735, #69983 ) ) ;
#35141 = CYLINDRICAL_SURFACE ( 'NONE', #14282, 31.99999999999998579 ) ;
#35142 = ORIENTED_EDGE ( 'NONE', *, *, #28272, .T. ) ;
#35143 = DIRECTION ( 'NONE',  ( 1.000000000000000000, 0.000000000000000000, 0.000000000000000000 ) ) ;
#35144 = CARTESIAN_POINT ( 'NONE',  ( 0.000000000000000000, 46.54456581323888997, -59.03342792756214408 ) ) ;
#35145 = CARTESIAN_POINT ( 'NONE',  ( 11.99999999999999822, 6.903761155837791819, 77.19088730480525840 ) ) ;
#35146 = EDGE_CURVE ( 'NONE', #30862, #21153, #51466, .T. ) ;
#35147 = DIRECTION ( 'NONE',  ( 1.000000000000000000, -0.000000000000000000, -0.000000000000000000 ) ) ;
#35148 = DIRECTION ( 'NONE',  ( 0.000000000000000000, 0.000000000000000000, 1.000000000000000000 ) ) ;
#35149 = DIRECTION ( 'NONE',  ( -1.000000000000000000, 0.000000000000000000, 0.000000000000000000 ) ) ;
#35150 = ADVANCED_FACE ( 'NONE', ( #22 ), #17995, .T. ) ;
#35151 = CARTESIAN_POINT ( 'NONE',  ( 19.29194287201271862, -133.5026271600380880, 5.500000000000000000 ) ) ;
#35152 = EDGE_LOOP ( 'NONE', ( #34658, #70919, #8022, #5674 ) ) ;
#35153 = CARTESIAN_POINT ( 'NONE',  ( -97.64999999999994884, -208.4700217866474645, 78.59645833506763779 ) ) ;
#35154 = ORIENTED_EDGE ( 'NONE', *, *, #48525, .F. ) ;
#35155 = CARTESIAN_POINT ( 'NONE',  ( 97.65000000002596892, -210.0000000000000853, -64.99999999999342037 ) ) ;
#35156 = ORIENTED_EDGE ( 'NONE', *, *, #72199, .T. ) ;
#35158 = CARTESIAN_POINT ( 'NONE',  ( -96.32500000000001705, 87.70503267997129626, 80.02520833506763154 ) ) ;
#35157 = CARTESIAN_POINT ( 'NONE',  ( 93.67499999999999716, 87.70503267997126784, 80.02520833506763154 ) ) ;
#35159 = ORIENTED_EDGE ( 'NONE', *, *, #71085, .F. ) ;
#35160 = CARTESIAN_POINT ( 'NONE',  ( 97.30629616937498838, 90.00000000000002842, 78.68906250086715204 ) ) ;
#35161 = CARTESIAN_POINT ( 'NONE',  ( 94.99999999999998579, 86.94004357329502852, 75.55375000000000796 ) ) ;
#35162 = FACE_OUTER_BOUND ( 'NONE', #8307, .T. ) ;
#35163 = LINE ( 'NONE', #28781, #14662 ) ;
#35164 = DIRECTION ( 'NONE',  ( 0.000000000000000000, -0.8660254037844384856, 0.5000000000000004441 ) ) ;
#35165 =( GEOMETRIC_REPRESENTATION_CONTEXT ( 3 ) GLOBAL_UNCERTAINTY_ASSIGNED_CONTEXT ( ( #14474 ) ) GLOBAL_UNIT_ASSIGNED_CONTEXT ( ( #49830, #10356, #74249 ) ) REPRESENTATION_CONTEXT ( 'NONE', 'WORKASPACE' ) );
#35166 = ORIENTED_EDGE ( 'NONE', *, *, #14309, .T. ) ;
#35167 = CARTESIAN_POINT ( 'NONE',  ( 93.67500000000001137, -207.7050326799711968, 77.19416666666666060 ) ) ;
#35168 = EDGE_CURVE ( 'NONE', #2800, #65294, #40557, .T. ) ;
#35169 = EDGE_CURVE ( 'NONE', #16367, #1257, #4946, .T. ) ;
#35170 = CARTESIAN_POINT ( 'NONE',  ( -10.00000000000000000, 0.000000000000000000, 0.000000000000000000 ) ) ;
#35171 = ORIENTED_EDGE ( 'NONE', *, *, #25041, .T. ) ;
#35172 = VECTOR ( 'NONE', #71567, 1000.000000000000000 ) ;
#35173 = VERTEX_POINT ( 'NONE', #51097 ) ;
#35174 = CARTESIAN_POINT ( 'NONE',  ( -0.8815729230226008184, -93.47222532549339746, 5.500000000000000000 ) ) ;
#35175 = CARTESIAN_POINT ( 'NONE',  ( -1.324703144935793775, -5.008684974571242066, -0.8655517945778401501 ) ) ;
#35176 = CARTESIAN_POINT ( 'NONE',  ( 5.000000000000000000, 67.80270845531887858, 46.11716303203210998 ) ) ;
#35177 = AXIS2_PLACEMENT_3D ( 'NONE', #39388, #62712, #40125 ) ;
#35178 =( BOUNDED_CURVE ( )  B_SPLINE_CURVE ( 2, ( #39174, #50057, #73734, #49331, #68112, #72985, #10586 ),
 .UNSPECIFIED., .F., .F. ) 
 B_SPLINE_CURVE_WITH_KNOTS ( ( 3, 2, 2, 3 ),
 ( 0.1666666666666666852, 0.1736111111111111049, 0.1805555555555554970, 0.1874999999999999167 ),
 .UNSPECIFIED. ) 
 CURVE ( )  GEOMETRIC_REPRESENTATION_ITEM ( )  RATIONAL_B_SPLINE_CURVE ( ( 0.9999999999999994449, 0.8660254037844392627, 1.000000000000000000, 0.8660254037844387076, 1.000000000000000000, 0.8660254037844402619, 0.9999999999999984457 ) ) 
 REPRESENTATION_ITEM ( '' )  );
#35179 = CARTESIAN_POINT ( 'NONE',  ( -94.99999999999997158, -212.6630814284392557, 79.16531250086715943 ) ) ;
#35180 = ORIENTED_EDGE ( 'NONE', *, *, #43330, .T. ) ;
#35181 = CARTESIAN_POINT ( 'NONE',  ( 0.000000000000000000, 21.40280677340421889, -36.13751322684397138 ) ) ;
#35182 = CIRCLE ( 'NONE', #5200, 2.500000000000000000 ) ;
#35183 = AXIS2_PLACEMENT_3D ( 'NONE', #31845, #54788, #26205 ) ;
#35184 = DIRECTION ( 'NONE',  ( -0.000000000000000000, -2.312964634635746211E-15, 1.000000000000000000 ) ) ;
#35185 = CARTESIAN_POINT ( 'NONE',  ( 0.000000000000000000, 73.73191006444551476, 14.66109333815590254 ) ) ;
#35186 = CYLINDRICAL_SURFACE ( 'NONE', #65661, 2.649999999999985700 ) ;
#35187 = DIRECTION ( 'NONE',  ( 0.000000000000000000, 0.000000000000000000, -1.000000000000000000 ) ) ;
#35188 = DIRECTION ( 'NONE',  ( 0.000000000000000000, 0.000000000000000000, 1.000000000000000000 ) ) ;
#35189 = DIRECTION ( 'NONE',  ( 1.000000000000000000, 0.000000000000000000, 0.000000000000000000 ) ) ;
#35190 = DIRECTION ( 'NONE',  ( -1.000000000000000000, 0.000000000000000000, 0.000000000000000000 ) ) ;
#35191 = FACE_OUTER_BOUND ( 'NONE', #27057, .T. ) ;
#35192 = DIRECTION ( 'NONE',  ( 1.000000000000000000, 1.387778780781445478E-15, 0.000000000000000000 ) ) ;
#35193 = CARTESIAN_POINT ( 'NONE',  ( 92.69370383062498320, 91.33154071421968467, 87.20864583420048177 ) ) ;
#35194 = CARTESIAN_POINT ( 'NONE',  ( -96.15314808468747287, -208.0026889286704943, 89.69572916753382685 ) ) ;
#35195 = DIRECTION ( 'NONE',  ( -0.2079116908177587875, 0.000000000000000000, 0.9781476007338056888 ) ) ;
#35196 = ORIENTED_EDGE ( 'NONE', *, *, #16028, .F. ) ;
#35197 = CARTESIAN_POINT ( 'NONE',  ( 0.000000000000000000, -26.79245525562738095, 32.34446384429961796 ) ) ;
#35198 = CARTESIAN_POINT ( 'NONE',  ( -93.84685191531252713, 88.00268892867056536, 77.15447916753380753 ) ) ;
#35199 = CARTESIAN_POINT ( 'NONE',  ( 95.00000000000000000, -207.3369185715606307, 86.94406250086714749 ) ) ;
#35200 = CIRCLE ( 'NONE', #41219, 42.00000000000000000 ) ;
#35201 = ORIENTED_EDGE ( 'NONE', *, *, #63390, .T. ) ;
#35202 = CARTESIAN_POINT ( 'NONE',  ( 96.32499999999998863, -207.7050326799711968, 87.24833333333333485 ) ) ;
#35203 = VERTEX_POINT ( 'NONE', #69143 ) ;
#35204 = AXIS2_PLACEMENT_3D ( 'NONE', #47537, #46062, #52060 ) ;
#35205 = EDGE_CURVE ( 'NONE', #40611, #21247, #17627, .T. ) ;
#35206 = CARTESIAN_POINT ( 'NONE',  ( 2.500000000000003109, -4.330127018922192761, -6.000000000000000000 ) ) ;
#35207 = DIRECTION ( 'NONE',  ( 0.000000000000000000, 0.9945218953682742891, -0.1045284632676436315 ) ) ;
#35208 = VECTOR ( 'NONE', #6384, 1000.000000000000000 ) ;
#35209 = EDGE_CURVE ( 'NONE', #3737, #14250, #34180, .T. ) ;
#35210 = ORIENTED_EDGE ( 'NONE', *, *, #12481, .T. ) ;
#35211 = ORIENTED_EDGE ( 'NONE', *, *, #157, .T. ) ;
#35212 = ADVANCED_FACE ( 'NONE', ( #62782 ), #23639, .F. ) ;
#35213 = CARTESIAN_POINT ( 'NONE',  ( 95.00000000000000000, -212.6630814284392557, 82.34031250086714238 ) ) ;
#35214 = CARTESIAN_POINT ( 'NONE',  ( 11.99999999999999822, 51.02545421589402252, -55.20638768913705263 ) ) ;
#35215 = CYLINDRICAL_SURFACE ( 'NONE', #14769, 30.50000000000000000 ) ;
#35216 = VECTOR ( 'NONE', #19585, 1000.000000000000000 ) ;
#35217 = DIRECTION ( 'NONE',  ( -1.000000000000000000, 0.000000000000000000, -0.000000000000000000 ) ) ;
#35218 = DIRECTION ( 'NONE',  ( 1.000000000000000000, -0.000000000000000000, -0.000000000000000000 ) ) ;
#35219 = ADVANCED_FACE ( 'NONE', ( #58216 ), #57121, .T. ) ;
#35220 = VECTOR ( 'NONE', #12805, 1000.000000000000000 ) ;
#35221 = DIRECTION ( 'NONE',  ( 1.000000000000000000, 0.000000000000000000, 0.000000000000000000 ) ) ;
#35222 = CARTESIAN_POINT ( 'NONE',  ( 96.32499999999998863, -212.2949673200287179, 83.86166666666666458 ) ) ;
#35223 = ORIENTED_EDGE ( 'NONE', *, *, #16720, .F. ) ;
#35224 = VERTEX_POINT ( 'NONE', #58581 ) ;
#35225 = ORIENTED_EDGE ( 'NONE', *, *, #25057, .F. ) ;
#35226 = AXIS2_PLACEMENT_3D ( 'NONE', #46561, #52192, #36372 ) ;
#35227 = EDGE_LOOP ( 'NONE', ( #30743, #56332 ) ) ;
#35229 = VECTOR ( 'NONE', #18443, 1000.000000000000227 ) ;
#35228 = CARTESIAN_POINT ( 'NONE',  ( 96.90829729882862864, -211.8387227684681591, 74.99954709728268654 ) ) ;
#35230 = VECTOR ( 'NONE', #60628, 1000.000000000000000 ) ;
#35231 =( NAMED_UNIT ( * ) SI_UNIT ( $, .STERADIAN. ) SOLID_ANGLE_UNIT ( ) );
#35232 = CARTESIAN_POINT ( 'NONE',  ( -92.69370383062504004, 90.00000000000004263, 87.57906250086715261 ) ) ;
#35233 = DIRECTION ( 'NONE',  ( 0.000000000000000000, 0.000000000000000000, 1.000000000000000000 ) ) ;
#35234 = DIRECTION ( 'NONE',  ( 0.000000000000000000, 0.000000000000000000, 1.000000000000000000 ) ) ;
#35235 = CARTESIAN_POINT ( 'NONE',  ( 95.00000000000000000, -206.9400435732949575, 75.31562500173430408 ) ) ;
#35236 = CARTESIAN_POINT ( 'NONE',  ( 97.64999999999997726, 88.47002178664753558, 76.92958333333332632 ) ) ;
#35237 = EDGE_CURVE ( 'NONE', #20511, #63342, #24377, .T. ) ;
#35238 = EDGE_LOOP ( 'NONE', ( #12600, #10946, #3995, #68498 ) ) ;
#35239 = CARTESIAN_POINT ( 'NONE',  ( 97.65000000000000568, 91.52997821335252127, 79.57541666666666913 ) ) ;
#35240 = ORIENTED_EDGE ( 'NONE', *, *, #40605, .F. ) ;
#35241 = ADVANCED_FACE ( 'NONE', ( #70216 ), #25847, .T. ) ;
#35242 = CARTESIAN_POINT ( 'NONE',  ( 10.00000000000000000, -51.03279382321125723, 55.19960302592048862 ) ) ;
#35243 = EDGE_LOOP ( 'NONE', ( #33759, #22954 ) ) ;
#35244 = DIRECTION ( 'NONE',  ( 0.000000000000000000, 0.000000000000000000, 1.000000000000000000 ) ) ;
#35245 = CARTESIAN_POINT ( 'NONE',  ( -97.30629616937501680, 88.66845928578038638, 81.59947916753382913 ) ) ;
#35246 = CARTESIAN_POINT ( 'NONE',  ( 92.69370383062498320, 88.66845928578037217, 76.36072916753381890 ) ) ;
#35247 = ORIENTED_EDGE ( 'NONE', *, *, #31320, .F. ) ;
#35248 = DIRECTION ( 'NONE',  ( -1.000000000000000000, -0.000000000000000000, -0.000000000000000000 ) ) ;
#35249 = CIRCLE ( 'NONE', #6492, 82.00000000000000000 ) ;
#35250 = DIRECTION ( 'NONE',  ( -0.000000000000000000, 0.8090169943749503378, 0.5877852522924690293 ) ) ;
#35251 = LINE ( 'NONE', #1087, #48607 ) ;
#35252 = CARTESIAN_POINT ( 'NONE',  ( 11.99999999999999822, -11.30684508768284680, -76.66974797899850103 ) ) ;
#35253 = ORIENTED_EDGE ( 'NONE', *, *, #69323, .T. ) ;
#35254 = DIRECTION ( 'NONE',  ( 0.000000000000000000, 0.000000000000000000, 1.000000000000000000 ) ) ;
#35255 = EDGE_CURVE ( 'NONE', #22660, #62740, #54424, .T. ) ;
#35256 = EDGE_CURVE ( 'NONE', #1142, #27456, #44544, .T. ) ;
#35257 = CARTESIAN_POINT ( 'NONE',  ( -92.69370383062498320, -209.9999999999999716, 74.72031250086713783 ) ) ;
#35258 = VERTEX_POINT ( 'NONE', #70962 ) ;
#35259 = ORIENTED_EDGE ( 'NONE', *, *, #45361, .F. ) ;
#35260 = CYLINDRICAL_SURFACE ( 'NONE', #25377, 37.49900000000000233 ) ;
#35261 = VERTEX_POINT ( 'NONE', #47671 ) ;
#35262 = DIRECTION ( 'NONE',  ( -1.000000000000000000, 0.000000000000000000, 0.000000000000000000 ) ) ;
#35263 = CIRCLE ( 'NONE', #2877, 82.00000000000000000 ) ;
#35264 = FACE_OUTER_BOUND ( 'NONE', #55883, .T. ) ;
#35265 = ORIENTED_EDGE ( 'NONE', *, *, #20806, .T. ) ;
#35266 = CARTESIAN_POINT ( 'NONE',  ( -94.99999999999997158, -207.3369185715606307, 88.37281250086715545 ) ) ;
#35267 = ORIENTED_EDGE ( 'NONE', *, *, #1744, .T. ) ;
#35268 = FACE_OUTER_BOUND ( 'NONE', #26909, .T. ) ;
#35269 = DIRECTION ( 'NONE',  ( -1.000000000000000000, 0.000000000000000000, 0.000000000000000000 ) ) ;
#35270 = ORIENTED_EDGE ( 'NONE', *, *, #63274, .F. ) ;
#35271 = AXIS2_PLACEMENT_3D ( 'NONE', #59900, #18907, #8382 ) ;
#35272 = DIRECTION ( 'NONE',  ( 0.000000000000000000, 0.000000000000000000, 1.000000000000000000 ) ) ;
#35273 = ORIENTED_EDGE ( 'NONE', *, *, #51777, .F. ) ;
#35274 = FACE_OUTER_BOUND ( 'NONE', #53156, .T. ) ;
#35275 = VECTOR ( 'NONE', #39766, 1000.000000000000000 ) ;
#35276 = DIRECTION ( 'NONE',  ( -1.000000000000000000, -0.000000000000000000, -0.000000000000000000 ) ) ;
#35277 = CARTESIAN_POINT ( 'NONE',  ( 93.84685191531248449, 91.99731107132950569, 83.18697916753382060 ) ) ;
#35278 = CYLINDRICAL_SURFACE ( 'NONE', #25614, 31.99999999999998579 ) ;
#35279 = DIRECTION ( 'NONE',  ( -1.000000000000000000, -0.000000000000000000, -0.000000000000000000 ) ) ;
#35280 = CARTESIAN_POINT ( 'NONE',  ( -97.65000000000010516, 91.52997821335249284, 81.05708333333332405 ) ) ;
#35281 = CYLINDRICAL_SURFACE ( 'NONE', #31573, 77.49899999999999523 ) ;
#35282 = CARTESIAN_POINT ( 'NONE',  ( 10.00000000000000000, 0.000000000000000000, 0.000000000000000000 ) ) ;
#35283 = CARTESIAN_POINT ( 'NONE',  ( -95.00000000000002842, 93.05995642670504253, 84.20562500173429044 ) ) ;
#35284 = DIRECTION ( 'NONE',  ( 0.000000000000000000, -0.5877852522924624790, -0.8090169943749553338 ) ) ;
#35285 = AXIS2_PLACEMENT_3D ( 'NONE', #51129, #39868, #56785 ) ;
#35286 = AXIS2_PLACEMENT_3D ( 'NONE', #49435, #55075, #8102 ) ;
#35287 = CARTESIAN_POINT ( 'NONE',  ( 7.400000000000003908, 1.056673655987569448E-14, 5.892267102770835596E-15 ) ) ;
#35288 = CARTESIAN_POINT ( 'NONE',  ( -0.0004442498558709490585, 0.001194404164628348752, 127.4927882439603195 ) ) ;
#35289 = AXIS2_PLACEMENT_3D ( 'NONE', #22055, #63049, #50620 ) ;
#35290 = CARTESIAN_POINT ( 'NONE',  ( -95.00000000000002842, 92.66308142843932671, 88.84906250086713442 ) ) ;
#35291 = VECTOR ( 'NONE', #10215, 1000.000000000000000 ) ;
#35292 = CYLINDRICAL_SURFACE ( 'NONE', #63576, 37.49900000000000233 ) ;
#35293 = EDGE_CURVE ( 'NONE', #63719, #31053, #19098, .T. ) ;
#35294 = ADVANCED_FACE ( 'NONE', ( #64983 ), #53682, .T. ) ;
#35295 = DIRECTION ( 'NONE',  ( 1.000000000000000000, -0.000000000000000000, 0.000000000000000000 ) ) ;
#35296 = EDGE_CURVE ( 'NONE', #37933, #28395, #39762, .T. ) ;
#35297 = ORIENTED_EDGE ( 'NONE', *, *, #27249, .F. ) ;
#35298 = CARTESIAN_POINT ( 'NONE',  ( 11.99999999999999822, 20.40083707022987625, -72.35432306680462489 ) ) ;
#35299 = DIRECTION ( 'NONE',  ( -1.000000000000000000, 0.000000000000000000, -0.000000000000000000 ) ) ;
#35300 = CARTESIAN_POINT ( 'NONE',  ( 97.64999999999999147, 90.00000000000002842, 76.98250000000000171 ) ) ;
#35301 = FACE_OUTER_BOUND ( 'NONE', #2248, .T. ) ;
#35302 = VECTOR ( 'NONE', #61039, 1000.000000000000000 ) ;
#35303 = EDGE_CURVE ( 'NONE', #61251, #21350, #47316, .T. ) ;
#35304 = CARTESIAN_POINT ( 'NONE',  ( 2.746650072473138780E-12, -120.0000000000000000, -70.59999999999999432 ) ) ;
#35305 = CARTESIAN_POINT ( 'NONE',  ( 0.000000000000000000, -39.78640506895652607, 66.50666863321986000 ) ) ;
#35306 = CARTESIAN_POINT ( 'NONE',  ( 96.15314808468750130, -211.9973110713294489, 85.56822916753381492 ) ) ;
#35307 = ADVANCED_FACE ( 'NONE', ( #64599 ), #69859, .T. ) ;
#35308 = VERTEX_POINT ( 'NONE', #59331 ) ;
#35309 = ORIENTED_EDGE ( 'NONE', *, *, #65721, .F. ) ;
#35310 = CYLINDRICAL_SURFACE ( 'NONE', #842, 77.49899999999999523 ) ;
#35311 = ORIENTED_EDGE ( 'NONE', *, *, #3994, .F. ) ;
#35312 = CONICAL_SURFACE ( 'NONE', #67735, 62.50000000000000000, 0.7853981633974497223 ) ;
#35313 = CARTESIAN_POINT ( 'NONE',  ( -97.65000000000001990, 90.00000000000004263, 90.00000000000000000 ) ) ;
#35314 = DIRECTION ( 'NONE',  ( -1.000000000000000000, -0.000000000000000000, 0.000000000000000000 ) ) ;
#35315 = EDGE_CURVE ( 'NONE', #3278, #25333, #19828, .T. ) ;
#35316 = ORIENTED_EDGE ( 'NONE', *, *, #22939, .T. ) ;
#35317 = CARTESIAN_POINT ( 'NONE',  ( 97.30629616937498838, -209.9999999999999716, 78.68906250086715204 ) ) ;
#35318 = ORIENTED_EDGE ( 'NONE', *, *, #47344, .F. ) ;
#35319 = CARTESIAN_POINT ( 'NONE',  ( 21.85433023846372436, -135.0628101570779620, 2.500000000000000000 ) ) ;
#35320 = VERTEX_POINT ( 'NONE', #65348 ) ;
#35321 = VERTEX_POINT ( 'NONE', #24741 ) ;
#35322 = CARTESIAN_POINT ( 'NONE',  ( -2.499999999999974243, 62.44997998398397954, -189.9999999999999147 ) ) ;
#35323 = CIRCLE ( 'NONE', #41332, 37.49900000000001654 ) ;
#35324 = SURFACE_SIDE_STYLE ('',( #36417 ) ) ;
#35325 = DIRECTION ( 'NONE',  ( 0.000000000000000000, -0.3090169943749549453, 0.9510565162951511997 ) ) ;
#35326 = ORIENTED_EDGE ( 'NONE', *, *, #28923, .T. ) ;
#35327 = CARTESIAN_POINT ( 'NONE',  ( 12.74955575014744547, 0.001194404164628405998, -80.00000000000001421 ) ) ;
#35328 = CARTESIAN_POINT ( 'NONE',  ( 93.67500000000001137, -207.7050326799711968, 85.52854166840096184 ) ) ;
#35329 = CARTESIAN_POINT ( 'NONE',  ( 97.64999999999997726, 88.47002178664753558, 88.35958333333333314 ) ) ;
#35330 = EDGE_CURVE ( 'NONE', #54114, #16652, #56573, .T. ) ;
#35331 = EDGE_LOOP ( 'NONE', ( #30873, #25793 ) ) ;
#35332 = CYLINDRICAL_SURFACE ( 'NONE', #70690, 31.99999999999999289 ) ;
#35333 = EDGE_CURVE ( 'NONE', #9811, #48440, #42779, .T. ) ;
#35334 = AXIS2_PLACEMENT_3D ( 'NONE', #22103, #21723, #45799 ) ;
#35335 = ORIENTED_EDGE ( 'NONE', *, *, #4072, .T. ) ;
#35336 = ORIENTED_EDGE ( 'NONE', *, *, #1649, .T. ) ;
#35337 = DIRECTION ( 'NONE',  ( -1.000000000000000000, -0.000000000000000000, 0.000000000000000000 ) ) ;
#35338 = AXIS2_PLACEMENT_3D ( 'NONE', #58691, #5726, #35392 ) ;
#35339 = VERTEX_POINT ( 'NONE', #2222 ) ;
#35340 = CARTESIAN_POINT ( 'NONE',  ( 93.67499999999999716, 87.70503267997126784, 87.01020833506763097 ) ) ;
#35341 = VERTEX_POINT ( 'NONE', #8183 ) ;
#35342 = VECTOR ( 'NONE', #19732, 1000.000000000000000 ) ;
#35343 = ORIENTED_EDGE ( 'NONE', *, *, #18162, .T. ) ;
#35344 = CARTESIAN_POINT ( 'NONE',  ( 11.99999999999999822, -14.67089635893658794, -73.72996012237454977 ) ) ;
#35345 = CIRCLE ( 'NONE', #47364, 42.00000000000000000 ) ;
#35346 = ITEM_DEFINED_TRANSFORMATION ( 'NONE', 'NONE', #426,  #43395 ) ;
#35347 = DIRECTION ( 'NONE',  ( 0.000000000000000000, 0.000000000000000000, 1.000000000000000000 ) ) ;
#35348 = VERTEX_POINT ( 'NONE', #37145 ) ;
#35349 = ORIENTED_EDGE ( 'NONE', *, *, #50637, .F. ) ;
#35350 = VERTEX_POINT ( 'NONE', #53318 ) ;
#35351 = DIRECTION ( 'NONE',  ( 0.000000000000000000, 0.000000000000000000, 1.000000000000000000 ) ) ;
#35352 = CARTESIAN_POINT ( 'NONE',  ( 11.99999999999999822, 5.256550761633951296, -77.32052557432835727 ) ) ;
#35353 = CARTESIAN_POINT ( 'NONE',  ( -95.00000000000002842, 86.94004357329504273, 86.34874999999999545 ) ) ;
#35354 = ORIENTED_EDGE ( 'NONE', *, *, #48781, .T. ) ;
#35355 = CARTESIAN_POINT ( 'NONE',  ( 0.000000000000000000, -55.38113227695745167, -54.21277698773732823 ) ) ;
#35356 = CIRCLE ( 'NONE', #46207, 31.99999999999998934 ) ;
#35357 = DIRECTION ( 'NONE',  ( 1.000000000000000000, 0.000000000000000000, 0.000000000000000000 ) ) ;
#35358 = ORIENTED_EDGE ( 'NONE', *, *, #40609, .T. ) ;
#35359 = LINE ( 'NONE', #58283, #46822 ) ;
#35360 = CARTESIAN_POINT ( 'NONE',  ( -97.30629616937495996, -209.9999999999999716, 83.29281250086714294 ) ) ;
#35361 = ORIENTED_EDGE ( 'NONE', *, *, #1849, .F. ) ;
#35362 = CYLINDRICAL_SURFACE ( 'NONE', #49436, 77.49899999999999523 ) ;
#35363 = DIRECTION ( 'NONE',  ( -1.000000000000000000, -0.000000000000000000, -0.000000000000000000 ) ) ;
#35364 = DIRECTION ( 'NONE',  ( -1.000000000000000000, -0.000000000000000000, -0.000000000000000000 ) ) ;
#35365 = CARTESIAN_POINT ( 'NONE',  ( -96.15314808468747287, -208.0026889286704943, 77.47197916753380298 ) ) ;
#35366 = AXIS2_PLACEMENT_3D ( 'NONE', #39419, #34503, #30418 ) ;
#35367 = DIRECTION ( 'NONE',  ( 1.000000000000000000, -0.000000000000000000, 0.000000000000000000 ) ) ;
#35368 = CARTESIAN_POINT ( 'NONE',  ( -92.35000000000005116, 88.47002178664754979, 85.26395833506762756 ) ) ;
#35369 = CARTESIAN_POINT ( 'NONE',  ( 0.000000000000000000, 0.000000000000000000, -189.9999999999999147 ) ) ;
#35370 = DIRECTION ( 'NONE',  ( 0.000000000000000000, -0.7604059656000227152, -0.6494480483301933171 ) ) ;
#35371 = CARTESIAN_POINT ( 'NONE',  ( 97.64999999999999147, 90.00000000000002842, 88.41249999999999432 ) ) ;
#35372 = EDGE_CURVE ( 'NONE', #73771, #63204, #28911, .T. ) ;
#35373 = CARTESIAN_POINT ( 'NONE',  ( -92.69370383062502583, 91.33154071421968467, 78.58322916753381548 ) ) ;
#35374 = DIRECTION ( 'NONE',  ( -0.000000000000000000, 0.000000000000000000, 1.000000000000000000 ) ) ;
#35375 = ORIENTED_EDGE ( 'NONE', *, *, #16809, .T. ) ;
#35376 = DIRECTION ( 'NONE',  ( 1.000000000000000000, 1.427937372958388501E-15, -7.962523111839142123E-16 ) ) ;
#35377 = CARTESIAN_POINT ( 'NONE',  ( 0.000000000000000000, 0.000000000000000000, 0.000000000000000000 ) ) ;
#35378 = LINE ( 'NONE', #7547, #74258 ) ;
#35379 = AXIS2_PLACEMENT_3D ( 'NONE', #2635, #31151, #37917 ) ;
#35380 = DIRECTION ( 'NONE',  ( -1.000000000000000000, -0.000000000000000000, -0.000000000000000000 ) ) ;
#35381 = CYLINDRICAL_SURFACE ( 'NONE', #10529, 42.00000000000000000 ) ;
#35382 = PLANE ( 'NONE',  #13587 ) ;
#35383 = CARTESIAN_POINT ( 'NONE',  ( -92.69370383062498320, -208.6684592857803011, 77.47197916753381719 ) ) ;
#35384 = ADVANCED_FACE ( 'NONE', ( #58967 ), #13816, .F. ) ;
#35385 = EDGE_CURVE ( 'NONE', #31227, #62260, #21708, .T. ) ;
#35386 = DIRECTION ( 'NONE',  ( 1.000000000000000000, 0.000000000000000000, 0.000000000000000000 ) ) ;
#35387 = VERTEX_POINT ( 'NONE', #2600 ) ;
#35388 = LINE ( 'NONE', #53777, #28745 ) ;
#35389 = AXIS2_PLACEMENT_3D ( 'NONE', #73786, #50492, #39597 ) ;
#35390 = FACE_OUTER_BOUND ( 'NONE', #44523, .T. ) ;
#35391 = EDGE_CURVE ( 'NONE', #66421, #71848, #41322, .T. ) ;
#35392 = DIRECTION ( 'NONE',  ( -1.000000000000000000, 7.331661483372147883E-15, 2.592266024478009537E-14 ) ) ;
#35393 = EDGE_CURVE ( 'NONE', #34509, #69471, #30758, .T. ) ;
#35394 = VECTOR ( 'NONE', #60994, 1000.000000000000114 ) ;
#35395 = CARTESIAN_POINT ( 'NONE',  ( 0.000000000000000000, 0.000000000000000000, 5.500000000000000000 ) ) ;
#35396 = ORIENTED_EDGE ( 'NONE', *, *, #58677, .F. ) ;
#35397 = CARTESIAN_POINT ( 'NONE',  ( 10.00000000000000000, 18.89407956138256139, 75.16055320797038064 ) ) ;
#35398 = ORIENTED_EDGE ( 'NONE', *, *, #30537, .F. ) ;
#35399 =( BOUNDED_CURVE ( )  B_SPLINE_CURVE ( 2, ( #22514, #17977, #57842, #40919, #57103, #45458, #39809 ),
 .UNSPECIFIED., .F., .T. ) 
 B_SPLINE_CURVE_WITH_KNOTS ( ( 3, 2, 2, 3 ),
 ( 0.5416666666666665186, 0.5486111111111110494, 0.5555555555555553582, 0.5624999999999997780 ),
 .UNSPECIFIED. ) 
 CURVE ( )  GEOMETRIC_REPRESENTATION_ITEM ( )  RATIONAL_B_SPLINE_CURVE ( ( 1.000000000000002220, 0.8660254037844365982, 1.000000000000000000, 0.8660254037844387076, 1.000000000000000000, 0.8660254037844430375, 0.9999999999999956701 ) ) 
 REPRESENTATION_ITEM ( '' )  );
#35400 = CARTESIAN_POINT ( 'NONE',  ( 92.69370383062501162, -208.6684592857803295, 83.87489583420047268 ) ) ;
#35401 = CARTESIAN_POINT ( 'NONE',  ( 10.00000000000000000, 0.6853352020795618893, -37.58145647212453611 ) ) ;
#35402 = ADVANCED_FACE ( 'NONE', ( #26587 ), #44261, .T. ) ;
#35403 = ORIENTED_EDGE ( 'NONE', *, *, #4434, .F. ) ;
#35404 = CARTESIAN_POINT ( 'NONE',  ( 92.69370383062501162, -208.6684592857803011, 89.74864583420048803 ) ) ;
#35405 = VERTEX_POINT ( 'NONE', #33325 ) ;
#35406 = DIRECTION ( 'NONE',  ( 0.000000000000000000, 0.000000000000000000, 1.000000000000000000 ) ) ;
#35407 = ORIENTED_EDGE ( 'NONE', *, *, #51513, .T. ) ;
#35408 = CARTESIAN_POINT ( 'NONE',  ( -96.15314808468751551, 88.00268892867056536, 81.01739583420049939 ) ) ;
#35409 = VERTEX_POINT ( 'NONE', #32959 ) ;
#35410 = VERTEX_POINT ( 'NONE', #50252 ) ;
#35411 = CARTESIAN_POINT ( 'NONE',  ( 10.00000000000000000, -44.88180994100329713, -63.18004540533077318 ) ) ;
#35412 = ORIENTED_EDGE ( 'NONE', *, *, #3587, .T. ) ;
#35413 = CARTESIAN_POINT ( 'NONE',  ( 12.49999999999999645, 1.530808498934191127E-15, 125.0000000000000000 ) ) ;
#35414 = EDGE_CURVE ( 'NONE', #30764, #37620, #54285, .T. ) ;
#35415 = VERTEX_POINT ( 'NONE', #20199 ) ;
#35416 = CARTESIAN_POINT ( 'NONE',  ( 92.34999999999999432, 88.47002178664752137, 80.60729166840097548 ) ) ;
#35417 = ORIENTED_EDGE ( 'NONE', *, *, #51928, .F. ) ;
#35418 = CARTESIAN_POINT ( 'NONE',  ( 93.89144186338212705, 87.63060383671354714, 74.97612907457775577 ) ) ;
#35419 = EDGE_CURVE ( 'NONE', #41967, #20003, #20587, .T. ) ;
#35420 = ORIENTED_EDGE ( 'NONE', *, *, #49306, .T. ) ;
#35421 = VERTEX_POINT ( 'NONE', #38624 ) ;
#35422 = ORIENTED_EDGE ( 'NONE', *, *, #41917, .F. ) ;
#35423 = CARTESIAN_POINT ( 'NONE',  ( 95.00000000000000000, -207.3369185715606307, 83.13406250086714522 ) ) ;
#35424 = CIRCLE ( 'NONE', #72596, 12.49999999999999645 ) ;
#35425 = APPLICATION_PROTOCOL_DEFINITION ( 'draft international standard', 'automotive_design', 1998, #33461 ) ;
#35426 = DIRECTION ( 'NONE',  ( 0.000000000000000000, 0.000000000000000000, 1.000000000000000000 ) ) ;
#35427 = DIRECTION ( 'NONE',  ( 0.08130631524009970801, -0.9966891607226786576, 0.000000000000000000 ) ) ;
#35428 = CARTESIAN_POINT ( 'NONE',  ( 96.32499999999998863, 87.70503267997126784, 85.13166666666666060 ) ) ;
#35429 = CARTESIAN_POINT ( 'NONE',  ( 0.000000000000000000, 0.000000000000000000, 2.499999999999999556 ) ) ;
#35430 = DIRECTION ( 'NONE',  ( -0.000000000000000000, -0.000000000000000000, 1.000000000000000000 ) ) ;
#35431 = DIRECTION ( 'NONE',  ( -1.000000000000000000, -0.000000000000000000, 0.000000000000000000 ) ) ;
#35432 = CARTESIAN_POINT ( 'NONE',  ( -92.69370383062498320, -208.6684592857803011, 83.66322916753379957 ) ) ;
#35433 = CARTESIAN_POINT ( 'NONE',  ( -92.69370383062502583, 91.33154071421968467, 82.55197916753382970 ) ) ;
#35434 = ORIENTED_EDGE ( 'NONE', *, *, #61045, .T. ) ;
#35435 = CARTESIAN_POINT ( 'NONE',  ( 94.99999999999998579, 87.33691857156068750, 85.35656250086714181 ) ) ;
#35436 = ORIENTED_EDGE ( 'NONE', *, *, #13418, .T. ) ;
#35437 = CARTESIAN_POINT ( 'NONE',  ( 10.00000000000000000, -29.81001611431024756, 22.74946021919122785 ) ) ;
#35439 = CIRCLE ( 'NONE', #17458, 16.00000000000000355 ) ;
#35438 = DIRECTION ( 'NONE',  ( -1.000000000000000000, -0.000000000000000000, 0.000000000000000000 ) ) ;
#35440 = CARTESIAN_POINT ( 'NONE',  ( 9.984461079971730157, -95.40710393340120277, -5.500000000000000000 ) ) ;
#35441 = VECTOR ( 'NONE', #36075, 1000.000000000000000 ) ;
#35442 = DIRECTION ( 'NONE',  ( -1.000000000000000000, 3.061616997868383141E-16, -0.000000000000000000 ) ) ;
#35443 = DIRECTION ( 'NONE',  ( -1.000000000000000000, 0.000000000000000000, 0.000000000000000000 ) ) ;
#35444 = CARTESIAN_POINT ( 'NONE',  ( -92.69370383062498320, -211.3315407142195852, 87.36739583420047950 ) ) ;
#35445 = CARTESIAN_POINT ( 'NONE',  ( 0.000000000000000000, 27.05870788708231700, 26.08949754953034272 ) ) ;
#35446 = DIRECTION ( 'NONE',  ( 0.000000000000000000, 0.000000000000000000, 1.000000000000000000 ) ) ;
#35447 = PLANE ( 'NONE',  #41888 ) ;
#35448 = ORIENTED_EDGE ( 'NONE', *, *, #27835, .F. ) ;
#35449 = ORIENTED_EDGE ( 'NONE', *, *, #27846, .F. ) ;
#35450 = AXIS2_PLACEMENT_3D ( 'NONE', #48764, #25470, #36745 ) ;
#35451 = CARTESIAN_POINT ( 'NONE',  ( -92.35000000000005116, 91.52997821335253548, 77.67041666666665378 ) ) ;
#35452 = DIRECTION ( 'NONE',  ( -0.000000000000000000, -0.000000000000000000, -1.000000000000000000 ) ) ;
#35453 = CARTESIAN_POINT ( 'NONE',  ( -96.15314808468752972, 91.99731107132950569, 88.26697916753380468 ) ) ;
#35454 = CARTESIAN_POINT ( 'NONE',  ( 25.81725066941077529, -113.8380548628854854, -2.500000000000000444 ) ) ;
#35455 = DIRECTION ( 'NONE',  ( -1.000000000000000000, -0.000000000000000000, -0.000000000000000000 ) ) ;
#35456 =( REPRESENTATION_RELATIONSHIP ('NONE','NONE', #31117, #10045 ) REPRESENTATION_RELATIONSHIP_WITH_TRANSFORMATION ( #49286 )SHAPE_REPRESENTATION_RELATIONSHIP( ) );
#35457 = ADVANCED_FACE ( 'NONE', ( #9295 ), #55164, .T. ) ;
#35458 = DIRECTION ( 'NONE',  ( 1.000000000000000000, -0.000000000000000000, 0.000000000000000000 ) ) ;
#35459 = CARTESIAN_POINT ( 'NONE',  ( 10.00000000000000000, 0.000000000000000000, 0.000000000000000000 ) ) ;
#35460 = ORIENTED_EDGE ( 'NONE', *, *, #43715, .T. ) ;
#35461 = DIRECTION ( 'NONE',  ( 0.8774505977381978905, 0.4796670183876304283, 0.000000000000000000 ) ) ;
#35462 = AXIS2_PLACEMENT_3D ( 'NONE', #28402, #51337, #68653 ) ;
#35463 = DIRECTION ( 'NONE',  ( -0.000000000000000000, -0.000000000000000000, 1.000000000000000000 ) ) ;
#35464 = DIRECTION ( 'NONE',  ( -0.000000000000000000, -0.000000000000000000, 1.000000000000000000 ) ) ;
#35465 = EDGE_CURVE ( 'NONE', #7320, #56343, #16997, .T. ) ;
#35466 = CYLINDRICAL_SURFACE ( 'NONE', #13042, 31.99999999999998579 ) ;
#35467 = PLANE ( 'NONE',  #21361 ) ;
#35468 = CARTESIAN_POINT ( 'NONE',  ( -10.00000000000000000, 0.000000000000000000, 0.000000000000000000 ) ) ;
#35469 = CARTESIAN_POINT ( 'NONE',  ( -94.99999999999997158, -207.3369185715606307, 85.83281250086714920 ) ) ;
#35470 = PRESENTATION_STYLE_ASSIGNMENT (( #12533 ) ) ;
#35471 = EDGE_CURVE ( 'NONE', #20819, #29677, #43431, .T. ) ;
#35472 = CARTESIAN_POINT ( 'NONE',  ( 96.15314808468748708, 91.99731107132950569, 77.52489583420047836 ) ) ;
#35473 = CARTESIAN_POINT ( 'NONE',  ( -96.15314808468747287, -208.0026889286704943, 76.99572916753382401 ) ) ;
#35474 = CARTESIAN_POINT ( 'NONE',  ( 0.000000000000000000, 0.000000000000000000, 0.000000000000000000 ) ) ;
#35475 = ORIENTED_EDGE ( 'NONE', *, *, #17134, .T. ) ;
#35476 = EDGE_CURVE ( 'NONE', #4362, #22507, #10985, .T. ) ;
#35477 = LINE ( 'NONE', #5817, #40114 ) ;
#35478 = CARTESIAN_POINT ( 'NONE',  ( 23.50000000000000355, -120.0000000000000000, -64.00000000000000000 ) ) ;
#35479 = CARTESIAN_POINT ( 'NONE',  ( 92.35000000006144205, 90.00001182123735077, 81.82400613091868991 ) ) ;
#35480 = CIRCLE ( 'NONE', #31866, 31.99999999999998579 ) ;
#35481 = CARTESIAN_POINT ( 'NONE',  ( -92.69370383062504004, 90.00000000000004263, 76.14906250086716000 ) ) ;
#35482 = CARTESIAN_POINT ( 'NONE',  ( 95.00000000000000000, -207.3369185715606307, 76.14906250086716000 ) ) ;
#35483 = ORIENTED_EDGE ( 'NONE', *, *, #20955, .F. ) ;
#35484 = FACE_OUTER_BOUND ( 'NONE', #4465, .T. ) ;
#35485 = ADVANCED_FACE ( 'NONE', ( #55541 ), #38240, .F. ) ;
#35486 = VERTEX_POINT ( 'NONE', #4055 ) ;
#35487 = CARTESIAN_POINT ( 'NONE',  ( 94.99999999999998579, 90.00000000000002842, 90.00000000000000000 ) ) ;
#35488 = EDGE_CURVE ( 'NONE', #11208, #21866, #31217, .T. ) ;
#35489 = AXIS2_PLACEMENT_3D ( 'NONE', #36633, #2480, #72327 ) ;
#35490 = ORIENTED_EDGE ( 'NONE', *, *, #57797, .F. ) ;
#35491 = LINE ( 'NONE', #58422, #1049 ) ;
#35492 = EDGE_CURVE ( 'NONE', #69389, #73994, #57767, .T. ) ;
#35493 = AXIS2_PLACEMENT_3D ( 'NONE', #50577, #73877, #45330 ) ;
#35494 = ORIENTED_EDGE ( 'NONE', *, *, #33327, .T. ) ;
#35495 = ORIENTED_EDGE ( 'NONE', *, *, #20488, .F. ) ;
#35496 = AXIS2_PLACEMENT_3D ( 'NONE', #20185, #43527, #65699 ) ;
#35497 = ORIENTED_EDGE ( 'NONE', *, *, #69986, .T. ) ;
#35498 = CARTESIAN_POINT ( 'NONE',  ( 97.65000000000000568, -208.4700217866474645, 79.65479166840096070 ) ) ;
#35499 = EDGE_CURVE ( 'NONE', #41023, #30425, #25379, .T. ) ;
#35500 = ORIENTED_EDGE ( 'NONE', *, *, #32311, .F. ) ;
#35501 = CIRCLE ( 'NONE', #36735, 12.49999999999999822 ) ;
#35502 = CIRCLE ( 'NONE', #9104, 32.00000000000000000 ) ;
#35503 = EDGE_LOOP ( 'NONE', ( #63354, #27247, #29199, #33748 ) ) ;
#35504 = CARTESIAN_POINT ( 'NONE',  ( 94.99999999999998579, 92.66308142843935514, 82.02281250086714692 ) ) ;
#35505 = LINE ( 'NONE', #6925, #31149 ) ;
#35506 = DIRECTION ( 'NONE',  ( -0.8541291221503261033, 0.5200609990133016058, 0.000000000000000000 ) ) ;
#35507 = ORIENTED_EDGE ( 'NONE', *, *, #7962, .T. ) ;
#35508 = VERTEX_POINT ( 'NONE', #16428 ) ;
#35509 = ORIENTED_EDGE ( 'NONE', *, *, #39974, .F. ) ;
#35510 = DIRECTION ( 'NONE',  ( -1.000000000000000000, 0.000000000000000000, 0.000000000000000000 ) ) ;
#35511 = ORIENTED_EDGE ( 'NONE', *, *, #34011, .F. ) ;
#35512 = SURFACE_STYLE_USAGE ( .BOTH. , #12205 ) ;
#35513 = COLOUR_RGB ( '', 0.72549020, 0.75294118, 0.79215686) ;
#35514 = DIRECTION ( 'NONE',  ( -1.000000000000000000, -0.000000000000000000, -0.000000000000000000 ) ) ;
#35515 = DIRECTION ( 'NONE',  ( -0.08130631524010122069, 0.9966891607226784355, 0.000000000000000000 ) ) ;
#35516 = CARTESIAN_POINT ( 'NONE',  ( 0.000000000000000000, 0.000000000000000000, 0.000000000000000000 ) ) ;
#35517 = DIRECTION ( 'NONE',  ( 0.000000000000000000, 0.000000000000000000, -1.000000000000000000 ) ) ;
#35518 = CYLINDRICAL_SURFACE ( 'NONE', #38068, 1.000000000000000888 ) ;
#35519 = CARTESIAN_POINT ( 'NONE',  ( -96.32499999999996021, -207.7050326799711968, 79.81354166840095843 ) ) ;
#35520 = ORIENTED_EDGE ( 'NONE', *, *, #41402, .T. ) ;
#35521 = DIRECTION ( 'NONE',  ( -1.000000000000000000, -0.000000000000000000, -0.000000000000000000 ) ) ;
#35522 = EDGE_LOOP ( 'NONE', ( #21365, #25791 ) ) ;
#35524 = CARTESIAN_POINT ( 'NONE',  ( -97.65000000000001990, 88.47002178664754979, 76.79729166840095900 ) ) ;
#35523 = CARTESIAN_POINT ( 'NONE',  ( 96.32499999999997442, 92.29496732002878900, 80.97770833506763211 ) ) ;
#35525 = ORIENTED_EDGE ( 'NONE', *, *, #63417, .T. ) ;
#35526 = CARTESIAN_POINT ( 'NONE',  ( 96.15314808468748708, 88.00268892867053694, 81.12322916753382174 ) ) ;
#35527 = CARTESIAN_POINT ( 'NONE',  ( 93.67499999999999716, 87.70503267997126784, 75.50083333333331836 ) ) ;
#35528 = CARTESIAN_POINT ( 'NONE',  ( 4.999999999999999112, 40.98264845739763018, -9.188173127306860977 ) ) ;
#35529 = CYLINDRICAL_SURFACE ( 'NONE', #30224, 82.00000000000000000 ) ;
#35530 = CARTESIAN_POINT ( 'NONE',  ( 1.560000000000000053, 1.732050807568878747, 7.017607234860990640E-28 ) ) ;
#35531 = ORIENTED_EDGE ( 'NONE', *, *, #15334, .F. ) ;
#35532 = DIRECTION ( 'NONE',  ( 0.9038112904824853189, -0.4279312458752977388, 0.000000000000000000 ) ) ;
#35533 = DIRECTION ( 'NONE',  ( -1.000000000000000000, -0.000000000000000000, -0.000000000000000000 ) ) ;
#35534 = ORIENTED_EDGE ( 'NONE', *, *, #31116, .F. ) ;
#35535 = ORIENTED_EDGE ( 'NONE', *, *, #13725, .F. ) ;
#35536 = CARTESIAN_POINT ( 'NONE',  ( -93.09170270117142820, -211.8387227684682159, 74.99954709728268654 ) ) ;
#35537 = CARTESIAN_POINT ( 'NONE',  ( -0.3476802294499993229, -5.572769417831399785, -1.687189089856318880 ) ) ;
#35538 = CARTESIAN_POINT ( 'NONE',  ( 0.000000000000000000, -26.08949754953044220, 27.05870788708222818 ) ) ;
#35539 = CARTESIAN_POINT ( 'NONE',  ( -93.84685191531247028, -211.9973110713294489, 76.04322916753382344 ) ) ;
#35540 = AXIS2_PLACEMENT_3D ( 'NONE', #56153, #44132, #39241 ) ;
#35541 = ORIENTED_EDGE ( 'NONE', *, *, #29134, .F. ) ;
#35542 = EDGE_CURVE ( 'NONE', #31963, #36799, #45388, .T. ) ;
#35543 = EDGE_CURVE ( 'NONE', #1166, #52158, #34979, .T. ) ;
#35544 = CARTESIAN_POINT ( 'NONE',  ( 2.459674775249762302, 3.512261536898573354E-15, 1.958521724562357923E-15 ) ) ;
#35545 = DIRECTION ( 'NONE',  ( 0.9966891607226786576, 0.08130631524009862554, 0.000000000000000000 ) ) ;
#35546 = ADVANCED_FACE ( 'NONE', ( #46479 ), #16805, .T. ) ;
#35547 = CARTESIAN_POINT ( 'NONE',  ( 96.32499999999998863, 87.70503267997126784, 85.84604166840097150 ) ) ;
#35548 = AXIS2_PLACEMENT_3D ( 'NONE', #20600, #59074, #70692 ) ;
#35549 = CARTESIAN_POINT ( 'NONE',  ( -95.00000000000002842, 90.00000000000004263, 90.00000000000000000 ) ) ;
#35550 = CARTESIAN_POINT ( 'NONE',  ( 15.00000000000000000, 5.835314593368777558, 22.81335362449846471 ) ) ;
#35551 = DIRECTION ( 'NONE',  ( 1.000000000000000000, 0.000000000000000000, 0.000000000000000000 ) ) ;
#35552 = AXIS2_PLACEMENT_3D ( 'NONE', #30272, #47572, #2501 ) ;
#35553 = FACE_OUTER_BOUND ( 'NONE', #20328, .T. ) ;
#35554 = DIRECTION ( 'NONE',  ( -1.000000000000000000, 0.000000000000000000, 0.000000000000000000 ) ) ;
#35555 = EDGE_CURVE ( 'NONE', #70629, #44617, #59028, .T. ) ;
#35556 = LINE ( 'NONE', #52860, #6453 ) ;
#35557 = CARTESIAN_POINT ( 'NONE',  ( 92.34999999999999432, 90.00000000000002842, 90.00000000000000000 ) ) ;
#35558 = VECTOR ( 'NONE', #56463, 1000.000000000000000 ) ;
#35559 = VECTOR ( 'NONE', #64675, 1000.000000000000000 ) ;
#35560 = EDGE_CURVE ( 'NONE', #35348, #71136, #72490, .T. ) ;
#35561 = CARTESIAN_POINT ( 'NONE',  ( 92.69370383062498320, 91.33154071421968467, 88.47864583420047779 ) ) ;
#35562 = CARTESIAN_POINT ( 'NONE',  ( -96.15314808468745866, -211.9973110713294489, 88.00239583420048461 ) ) ;
#35563 = CARTESIAN_POINT ( 'NONE',  ( 11.99999999999999822, -31.46837873495025306, 68.27212725128265447 ) ) ;
#35564 = ORIENTED_EDGE ( 'NONE', *, *, #49964, .F. ) ;
#35565 = CARTESIAN_POINT ( 'NONE',  ( -15.70000000000052687, -119.9999999999998721, -70.59999999999959641 ) ) ;
#35566 = CARTESIAN_POINT ( 'NONE',  ( -97.64999999999994884, -208.4700217866474645, 82.96208333333333940 ) ) ;
#35567 = CARTESIAN_POINT ( 'NONE',  ( -97.30629616937501680, 88.66845928578038638, 77.63072916753380071 ) ) ;
#35568 = CARTESIAN_POINT ( 'NONE',  ( 97.30629616937498838, -211.3315407142195852, 88.00239583420047040 ) ) ;
#35569 = EDGE_LOOP ( 'NONE', ( #2630, #34953, #61017, #42838 ) ) ;
#35570 = EDGE_LOOP ( 'NONE', ( #57550, #25529, #51894, #40958, #25997 ) ) ;
#35571 = ORIENTED_EDGE ( 'NONE', *, *, #24955, .F. ) ;
#35572 = EDGE_CURVE ( 'NONE', #47715, #9195, #65041, .T. ) ;
#35573 = EDGE_CURVE ( 'NONE', #72747, #25082, #51011, .T. ) ;
#35575 = CLOSED_SHELL ( 'NONE', ( #71250, #43, #66547, #54071, #51880, #55571, #25812, #22234, #39392, #65363, #71775, #25606, #64496, #67163, #72788, #13745, #25867, #36210, #19329, #9769, #40230, #50913, #9519, #6839, #61098, #21967, #17601, #22842, #44229, #48801, #31657, #24614, #20771, #41276, #58134, #69899, #71710, #35219, #62131, #51506, #13931, #52876, #49294, #27078, #2683, #38736, #27301, #57496, #71040, #70617, #28115, #21027, #49735, #59310, #69085, #66941, #58892, #9236, #32904, #54853, #46585, #67315, #68702, #29340, #23783, #47018, #23499, #23626, #16825, #49883, #53072, #1592, #2673, #59675, #56995, #18927, #55092, #11027, #11138, #45107, #43382, #24800, #59622, #45496, #72962, #21737, #8600, #46006, #34282, #23674, #12784, #12973, #65994, #21363, #34903, #69619, #45414, #14209, #42428, #54506, #20304, #36921, #50230, #37468, #60843, #711, #40100, #17805, #1139, #70225, #62497, #5821, #48869, #23038, #49795, #24382, #34748, #48582, #11478, #44754, #28673, #15782, #30367, #44336, #37610, #59093, #56174, #16813, #62163, #35657, #45019, #31927, #24374, #70933, #6984, #56030, #17062, #52502, #55003, #16654, #27127, #59754, #16977, #6364, #34061, #54177, #48130, #64416, #11784, #46951, #12236, #34355, #23097, #26194, #13139, #32859, #63857, #32090, #4366, #11285, #71429, #10109, #2063, #52189, #38089, #4572, #51964, #53150, #34611, #38182, #8297, #60811, #29592, #54770, #11095, #72416, #14106, #38478, #65960, #60346, #60766, #58737, #62407, #37303, #55251, #48689, #8746, #51327, #70668, #43513, #61108, #13507, #56699, #12792, #27609, #41865, #24051, #63407, #15872, #4500, #148, #33348, #6622, #32675, #66464, #48271, #23370, #27392, #15016, #69830, #54432, #64341, #35830, #50680, #73330, #8656, #30306, #33166, #57038, #8160, #71792, #12308, #9309, #7638, #73472, #13894, #36765, #49044, #52946, #36659, #9671, #61006, #40422, #22262, #57924, #37956, #40314, #14865, #37888, #41483, #64210, #26074, #17835, #33023, #6490, #30908, #29031, #65782, #4943, #15610, #35925, #32567, #15007, #18004, #44737, #61205, #67386, #71092, #50645, #35150, #37892, #24526, #71958, #3772, #24426, #63784, #37958, #36020, #61047, #68896, #18813, #31928, #4858, #40373, #68701, #72060, #30019, #58498, #64676, #39580, #21558, #7028, #6130, #43659, #54728, #19092, #31628, #56617, #34946, #59858, #258, #28948, #56272, #1872, #12222, #5099, #37000, #26751, #54392, #14933, #49048, #38530, #20524, #40667, #43304, #36296, #59787, #51846, #1232, #40051, #52888, #27864, #73118, #48613, #12070, #9356, #74169, #30993, #45086, #62744, #37346, #18659, #26654, #10035, #21523, #47545, #71347, #20475, #30488, #38175, #72332, #2263, #24564 ) ) ;
#35574 = CYLINDRICAL_SURFACE ( 'NONE', #40272, 37.49900000000000233 ) ;
#35576 = ORIENTED_EDGE ( 'NONE', *, *, #34652, .F. ) ;
#35577 = ORIENTED_EDGE ( 'NONE', *, *, #44985, .F. ) ;
#35578 = CARTESIAN_POINT ( 'NONE',  ( 97.30629616937498838, -211.3315407142195852, 81.81114583420048803 ) ) ;
#35579 = DIRECTION ( 'NONE',  ( -1.000000000000000000, -0.000000000000000000, -0.000000000000000000 ) ) ;
#35580 = EDGE_CURVE ( 'NONE', #27851, #62613, #11518, .T. ) ;
#35581 = LINE ( 'NONE', #36322, #22024 ) ;
#35582 = DIRECTION ( 'NONE',  ( 0.000000000000000000, 0.000000000000000000, 1.000000000000000000 ) ) ;
#35583 = FACE_OUTER_BOUND ( 'NONE', #28747, .T. ) ;
#35584 = CARTESIAN_POINT ( 'NONE',  ( -4.653126046682595884, -146.1313684676804314, -5.500000000000000000 ) ) ;
#35585 = CARTESIAN_POINT ( 'NONE',  ( 96.32499999999998863, -207.7050326799711968, 85.34333333333333371 ) ) ;
#35586 = ORIENTED_EDGE ( 'NONE', *, *, #7336, .F. ) ;
#35587 = ORIENTED_EDGE ( 'NONE', *, *, #43238, .F. ) ;
#35588 = ORIENTED_EDGE ( 'NONE', *, *, #42902, .F. ) ;
#35589 = ORIENTED_EDGE ( 'NONE', *, *, #35000, .T. ) ;
#35590 = CARTESIAN_POINT ( 'NONE',  ( -18.24502636017238899, -100.7225776329765665, -5.500000000000000000 ) ) ;
#35591 = SHAPE_REPRESENTATION_RELATIONSHIP ( 'NONE' , 'NONE' ,  #67135, #13932 ) ;
#35592 = CARTESIAN_POINT ( 'NONE',  ( -93.84685191531254134, 91.99731107132950569, 87.68489583420048916 ) ) ;
#35593 = VECTOR ( 'NONE', #18010, 1000.000000000000000 ) ;
#35594 = CARTESIAN_POINT ( 'NONE',  ( 10.00000000000000000, -41.76106447765443619, -62.50884508063471401 ) ) ;
#35595 = AXIS2_PLACEMENT_3D ( 'NONE', #4511, #39456, #51463 ) ;
#35596 = DIRECTION ( 'NONE',  ( 0.000000000000000000, 0.000000000000000000, 1.000000000000000000 ) ) ;
#35597 = CARTESIAN_POINT ( 'NONE',  ( 96.32499999999998863, -212.2949673200287179, 75.05104166840095559 ) ) ;
#35598 = CARTESIAN_POINT ( 'NONE',  ( 92.34999999999999432, 91.52997821335252127, 77.88208333333332689 ) ) ;
#35599 = ORIENTED_EDGE ( 'NONE', *, *, #24124, .T. ) ;
#35600 = CARTESIAN_POINT ( 'NONE',  ( -92.34999999999999432, -208.4700217866474645, 87.90979166840095615 ) ) ;
#35601 = ORIENTED_EDGE ( 'NONE', *, *, #6785, .F. ) ;
#35602 = DIRECTION ( 'NONE',  ( 0.000000000000000000, 0.9135454576426063067, -0.4067366430757881068 ) ) ;
#35603 = AXIS2_PLACEMENT_3D ( 'NONE', #28519, #40191, #17989 ) ;
#35604 = VERTEX_POINT ( 'NONE', #34835 ) ;
#35605 = CARTESIAN_POINT ( 'NONE',  ( -97.65000000000001990, 91.52997821335253548, 87.48645833506763836 ) ) ;
#35606 =( BOUNDED_CURVE ( )  B_SPLINE_CURVE ( 2, ( #63229, #18449, #51182, #11689, #39924, #62872, #28992, #6090, #51926 ),
 .UNSPECIFIED., .F., .F. ) 
 B_SPLINE_CURVE_WITH_KNOTS ( ( 3, 2, 2, 2, 3 ),
 ( 0.2540073681283128160, 0.2540075594717651764, 0.2610633250126475624, 0.2681190905535300040, 0.2751748541904413536 ),
 .UNSPECIFIED. ) 
 CURVE ( )  GEOMETRIC_REPRESENTATION_ITEM ( )  RATIONAL_B_SPLINE_CURVE ( ( 0.9999927337532890093, 0.9999963667781160970, 1.000000000000000000, 0.8660254037844387076, 1.000000000000000000, 0.8660254037844387076, 1.000000000000000000, 0.8660254037844387076, 1.000000000000000000 ) ) 
 REPRESENTATION_ITEM ( '' )  );
#35607 = CARTESIAN_POINT ( 'NONE',  ( 96.15314808468748708, 88.00268892867053694, 75.24947916753380639 ) ) ;
#35608 = VERTEX_POINT ( 'NONE', #34451 ) ;
#35609 = CARTESIAN_POINT ( 'NONE',  ( 97.64999999999999147, -209.9999999999999716, 83.96750000000000114 ) ) ;
#35610 = FACE_OUTER_BOUND ( 'NONE', #3619, .T. ) ;
#35611 = DIRECTION ( 'NONE',  ( 0.000000000000000000, 0.000000000000000000, -1.000000000000000000 ) ) ;
#35612 = VERTEX_POINT ( 'NONE', #23550 ) ;
#35613 = DIRECTION ( 'NONE',  ( 1.000000000000000000, 0.000000000000000000, 0.000000000000000000 ) ) ;
#35614 = CARTESIAN_POINT ( 'NONE',  ( 10.00000000000000000, 6.736453364084091788, -36.88895765772625879 ) ) ;
#35615 = EDGE_LOOP ( 'NONE', ( #29844, #14773, #53747, #34010 ) ) ;
#35616 = AXIS2_PLACEMENT_3D ( 'NONE', #69517, #41318, #64259 ) ;
#35617 = EDGE_LOOP ( 'NONE', ( #27158, #50887, #17662, #20051 ) ) ;
#35618 = CARTESIAN_POINT ( 'NONE',  ( 0.000000000000000000, -81.50828551894220197, -8.966570791701583332 ) ) ;
#35619 = CARTESIAN_POINT ( 'NONE',  ( 5.000000000000000000, 2.886751345948137981, -5.553418012614792509 ) ) ;
#35620 = DIRECTION ( 'NONE',  ( 0.000000000000000000, 0.000000000000000000, 1.000000000000000000 ) ) ;
#35621 = VERTEX_POINT ( 'NONE', #5169 ) ;
#35622 = CARTESIAN_POINT ( 'NONE',  ( -94.99999999999997158, -207.3369185715606307, 87.73781250086715033 ) ) ;
#35623 = ORIENTED_EDGE ( 'NONE', *, *, #57576, .T. ) ;
#35624 = SURFACE_SIDE_STYLE ('',( #8550 ) ) ;
#35625 = ORIENTED_EDGE ( 'NONE', *, *, #315, .T. ) ;
#35626 = VERTEX_POINT ( 'NONE', #34085 ) ;
#35627 = EDGE_CURVE ( 'NONE', #45615, #31053, #57785, .T. ) ;
#35628 = DIRECTION ( 'NONE',  ( 1.000000000000000000, 0.000000000000000000, 0.000000000000000000 ) ) ;
#35629 = CARTESIAN_POINT ( 'NONE',  ( 97.30629616937498838, 91.33154071421968467, 83.02822916753379445 ) ) ;
#35630 = CARTESIAN_POINT ( 'NONE',  ( 10.00000000000000000, 0.000000000000000000, 0.000000000000000000 ) ) ;
#35631 = DIRECTION ( 'NONE',  ( 0.000000000000000000, 0.000000000000000000, 1.000000000000000000 ) ) ;
#35632 = DIRECTION ( 'NONE',  ( 0.2867529058022035837, -0.9580045777625452175, 0.000000000000000000 ) ) ;
#35633 = FACE_OUTER_BOUND ( 'NONE', #71656, .T. ) ;
#35635 = EDGE_CURVE ( 'NONE', #34880, #22108, #11162, .T. ) ;
#35634 = CARTESIAN_POINT ( 'NONE',  ( 3.000000000000000000, -1.467624384280027838, 2.542000000000001592 ) ) ;
#35636 = DIRECTION ( 'NONE',  ( -1.000000000000000000, 0.000000000000000000, 0.000000000000000000 ) ) ;
#35637 = LINE ( 'NONE', #28903, #49492 ) ;
#35638 = EDGE_CURVE ( 'NONE', #18312, #63042, #27706, .T. ) ;
#35639 = CIRCLE ( 'NONE', #22454, 31.99999999999997868 ) ;
#35640 = LINE ( 'NONE', #48046, #30015 ) ;
#35641 = CIRCLE ( 'NONE', #21201, 31.99999999999999289 ) ;
#35642 = DIRECTION ( 'NONE',  ( -0.1276937514489705217, -0.9918136447140101231, 0.000000000000000000 ) ) ;
#35643 = CARTESIAN_POINT ( 'NONE',  ( -97.30629616937501680, 91.33154071421968467, 85.14489583420045449 ) ) ;
#35644 = LINE ( 'NONE', #8186, #33539 ) ;
#35645 = CIRCLE ( 'NONE', #5678, 16.00000000000000000 ) ;
#35646 = EDGE_CURVE ( 'NONE', #43675, #45993, #63787, .T. ) ;
#35647 = CARTESIAN_POINT ( 'NONE',  ( 0.000000000000000000, -72.35432306680469594, -20.40083707022958848 ) ) ;
#35648 = EDGE_CURVE ( 'NONE', #31332, #65728, #57030, .T. ) ;
#35649 = AXIS2_PLACEMENT_3D ( 'NONE', #59322, #66091, #54418 ) ;
#35650 = ORIENTED_EDGE ( 'NONE', *, *, #42180, .F. ) ;
#35651 = DIRECTION ( 'NONE',  ( -0.4796670183876317051, 0.8774505977381972244, 0.000000000000000000 ) ) ;
#35652 = CARTESIAN_POINT ( 'NONE',  ( 97.64999999999999147, 90.00000000000002842, 90.00000000000000000 ) ) ;
#35653 = VECTOR ( 'NONE', #45484, 1000.000000000000000 ) ;
#35654 = CARTESIAN_POINT ( 'NONE',  ( 5.000000000000000000, 56.15606465354959198, 59.75363087400094741 ) ) ;
#35655 = LINE ( 'NONE', #41312, #68027 ) ;
#35656 = EDGE_CURVE ( 'NONE', #51075, #14449, #32600, .T. ) ;
#35657 = ADVANCED_FACE ( 'NONE', ( #58493 ), #41212, .T. ) ;
#35658 = CARTESIAN_POINT ( 'NONE',  ( 93.84685191531251292, -211.9973110713294489, 81.65239583420049030 ) ) ;
#35659 = VECTOR ( 'NONE', #54729, 1000.000000000000000 ) ;
#35660 = VERTEX_POINT ( 'NONE', #36671 ) ;
#35661 = ORIENTED_EDGE ( 'NONE', *, *, #59933, .T. ) ;
#35662 = VECTOR ( 'NONE', #30119, 1000.000000000000000 ) ;
#35663 = ORIENTED_EDGE ( 'NONE', *, *, #4294, .T. ) ;
#35664 = DIRECTION ( 'NONE',  ( 0.6516173805718078471, -0.7585478161175706058, 0.000000000000000000 ) ) ;
#35665 = CARTESIAN_POINT ( 'NONE',  ( 95.00000000000000000, -212.6630814284392557, 75.83156250086715033 ) ) ;
#35666 = VERTEX_POINT ( 'NONE', #19742 ) ;
#35667 = CARTESIAN_POINT ( 'NONE',  ( 93.84685191531249870, -208.0026889286704943, 80.80572916753382628 ) ) ;
#35668 = ORIENTED_EDGE ( 'NONE', *, *, #68576, .F. ) ;
#35669 = CARTESIAN_POINT ( 'NONE',  ( 3.000000000000000000, 2.935248768560057897, -3.252606517456513302E-15 ) ) ;
#35670 = ORIENTED_EDGE ( 'NONE', *, *, #47865, .T. ) ;
#35671 = ORIENTED_EDGE ( 'NONE', *, *, #45409, .F. ) ;
#35672 = LINE ( 'NONE', #23666, #4596 ) ;
#35673 =( LENGTH_UNIT ( ) NAMED_UNIT ( * ) SI_UNIT ( .MILLI., .METRE. ) );
#35674 = CARTESIAN_POINT ( 'NONE',  ( -15.70044424985254850, 0.001194404164626844313, -85.59999999999999432 ) ) ;
#35675 = ORIENTED_EDGE ( 'NONE', *, *, #50706, .F. ) ;
#35676 = CARTESIAN_POINT ( 'NONE',  ( 10.00000000000000000, 69.42325613327489009, -34.44570377933524696 ) ) ;
#35677 = CARTESIAN_POINT ( 'NONE',  ( 96.32499999999998863, -207.7050326799711968, 84.15270833506762926 ) ) ;
#35678 = CARTESIAN_POINT ( 'NONE',  ( 92.34999999999999432, 91.52997821335252127, 88.67708333333332860 ) ) ;
#35679 = VERTEX_POINT ( 'NONE', #58878 ) ;
#35680 = CARTESIAN_POINT ( 'NONE',  ( 97.65000000000000568, 91.52997821335252127, 84.73479166840094479 ) ) ;
#35681 = CARTESIAN_POINT ( 'NONE',  ( -94.26819495033768703, 87.36255141571193406, 75.02735117824596500 ) ) ;
#35682 = EDGE_LOOP ( 'NONE', ( #73373, #4920, #24589, #28492 ) ) ;
#35683 = EDGE_LOOP ( 'NONE', ( #72030, #22962, #28707, #62446 ) ) ;
#35684 = CARTESIAN_POINT ( 'NONE',  ( 0.000000000000000000, 12.24744871391589207, -2.499999999999994671 ) ) ;
#35685 = ORIENTED_EDGE ( 'NONE', *, *, #39550, .F. ) ;
#35687 = CARTESIAN_POINT ( 'NONE',  ( 92.34999999999999432, 91.52997821335252127, 86.21645833506764234 ) ) ;
#35686 = CIRCLE ( 'NONE', #11645, 31.99999999999998579 ) ;
#35688 = ORIENTED_EDGE ( 'NONE', *, *, #31308, .F. ) ;
#35689 = ORIENTED_EDGE ( 'NONE', *, *, #39044, .T. ) ;
#35690 = CARTESIAN_POINT ( 'NONE',  ( -94.99999999999997158, -213.0599564267049857, 78.17312500173430578 ) ) ;
#35691 = CARTESIAN_POINT ( 'NONE',  ( -92.34999999999990905, -208.4700217866474929, 75.13041666666666174 ) ) ;
#35692 = ORIENTED_EDGE ( 'NONE', *, *, #41952, .T. ) ;
#35693 = ORIENTED_EDGE ( 'NONE', *, *, #44412, .F. ) ;
#35694 = VECTOR ( 'NONE', #39148, 1000.000000000000000 ) ;
#35695 = EDGE_LOOP ( 'NONE', ( #52893, #35776, #59931, #19952, #12384 ) ) ;
#35696 = VECTOR ( 'NONE', #18902, 1000.000000000000114 ) ;
#35697 = CARTESIAN_POINT ( 'NONE',  ( 0.000000000000000000, 8.966570791701871102, -81.50828551894218776 ) ) ;
#35698 = CARTESIAN_POINT ( 'NONE',  ( 97.64999999999993463, 91.52997821335253548, 81.48041666666665606 ) ) ;
#35699 = CARTESIAN_POINT ( 'NONE',  ( -92.35000000000003695, 90.00000000000004263, 88.41249999999999432 ) ) ;
#35700 = EDGE_LOOP ( 'NONE', ( #70932, #7606, #66856, #17092 ) ) ;
#35701 = DIRECTION ( 'NONE',  ( -0.000000000000000000, -0.000000000000000000, 1.000000000000000000 ) ) ;
#35702 = EDGE_CURVE ( 'NONE', #65117, #14143, #29540, .T. ) ;
#35703 = CARTESIAN_POINT ( 'NONE',  ( 10.00000000000000000, -11.30684508768284680, -76.66974797899850103 ) ) ;
#35704 = VERTEX_POINT ( 'NONE', #70133 ) ;
#35705 = CARTESIAN_POINT ( 'NONE',  ( -3.000000000000000000, 8.688484142253939169, 21.88630264137371029 ) ) ;
#35706 = CARTESIAN_POINT ( 'NONE',  ( -97.30629616937497417, -211.3315407142195852, 83.34572916753380412 ) ) ;
#35707 = EDGE_LOOP ( 'NONE', ( #38818, #45027, #9210, #22505 ) ) ;
#35708 = CYLINDRICAL_SURFACE ( 'NONE', #42257, 37.49900000000000233 ) ;
#35709 = DIRECTION ( 'NONE',  ( -1.000000000000000000, 0.000000000000000000, 0.000000000000000000 ) ) ;
#35710 = CARTESIAN_POINT ( 'NONE',  ( 0.000000000000000000, 63.18004540533092239, -44.88180994100307686 ) ) ;
#35711 = DIRECTION ( 'NONE',  ( 0.000000000000000000, 0.000000000000000000, 1.000000000000000000 ) ) ;
#35712 = EDGE_CURVE ( 'NONE', #53902, #15045, #70490, .T. ) ;
#35713 = DIRECTION ( 'NONE',  ( 1.000000000000000000, 0.000000000000000000, 0.000000000000000000 ) ) ;
#35714 = AXIS2_PLACEMENT_3D ( 'NONE', #5194, #5933, #45790 ) ;
#35715 = EDGE_CURVE ( 'NONE', #35704, #16558, #15861, .T. ) ;
#35716 = DIRECTION ( 'NONE',  ( -1.000000000000000000, 0.000000000000000000, -0.000000000000000000 ) ) ;
#35717 = CARTESIAN_POINT ( 'NONE',  ( 10.00000000000000000, -74.65491531819111515, 23.16904090965678975 ) ) ;
#35718 = DIRECTION ( 'NONE',  ( 0.000000000000000000, 0.000000000000000000, 1.000000000000000000 ) ) ;
#35719 = AXIS2_PLACEMENT_3D ( 'NONE', #43211, #9716, #14611 ) ;
#35721 = EDGE_CURVE ( 'NONE', #69158, #50412, #19395, .T. ) ;
#35720 = DIRECTION ( 'NONE',  ( 0.000000000000000000, 0.000000000000000000, 1.000000000000000000 ) ) ;
#35722 = CARTESIAN_POINT ( 'NONE',  ( -95.00000000000002842, 92.66308142843932671, 79.95906250086713385 ) ) ;
#35723 = DIRECTION ( 'NONE',  ( 0.000000000000000000, 0.000000000000000000, 1.000000000000000000 ) ) ;
#35724 = DIRECTION ( 'NONE',  ( -1.000000000000000000, -0.000000000000000000, -0.000000000000000000 ) ) ;
#35725 = EDGE_CURVE ( 'NONE', #42459, #8427, #8100, .T. ) ;
#35726 = LINE ( 'NONE', #3773, #10011 ) ;
#35727 = DIRECTION ( 'NONE',  ( 4.476705744456277943E-17, -1.000000000000000000, 0.000000000000000000 ) ) ;
#35728 = CARTESIAN_POINT ( 'NONE',  ( 3.000000000000000000, 2.935248768560057897, -3.252606517456513302E-15 ) ) ;
#35729 = DIRECTION ( 'NONE',  ( -0.000000000000000000, -0.000000000000000000, 1.000000000000000000 ) ) ;
#35730 = CYLINDRICAL_SURFACE ( 'NONE', #17723, 42.00000000000000000 ) ;
#35731 = CARTESIAN_POINT ( 'NONE',  ( -3.000000000000000000, 16.61724383029390140, -20.69703378468903665 ) ) ;
#35732 = CARTESIAN_POINT ( 'NONE',  ( -97.30629616937497417, -211.3315407142195852, 75.88447916753382572 ) ) ;
#35733 = EDGE_CURVE ( 'NONE', #4438, #5103, #41573, .T. ) ;
#35734 = CARTESIAN_POINT ( 'NONE',  ( 94.99999999999998579, 90.00000000000002842, 90.00000000000000000 ) ) ;
#35735 = EDGE_CURVE ( 'NONE', #68616, #45600, #38631, .T. ) ;
#35736 = ORIENTED_EDGE ( 'NONE', *, *, #19629, .T. ) ;
#35737 = CIRCLE ( 'NONE', #74177, 16.00000000000000000 ) ;
#35738 = FACE_OUTER_BOUND ( 'NONE', #62314, .T. ) ;
#35739 = DIRECTION ( 'NONE',  ( 0.000000000000000000, 0.000000000000000000, 1.000000000000000000 ) ) ;
#35740 = DIRECTION ( 'NONE',  ( -1.000000000000000000, -0.000000000000000000, 0.000000000000000000 ) ) ;
#35741 = CIRCLE ( 'NONE', #4540, 77.49900000000000944 ) ;
#35742 = DIRECTION ( 'NONE',  ( 0.000000000000000000, 0.000000000000000000, 1.000000000000000000 ) ) ;
#35743 = VECTOR ( 'NONE', #51078, 1000.000000000000000 ) ;
#35744 = AXIS2_PLACEMENT_3D ( 'NONE', #44068, #31664, #54609 ) ;
#35745 = DIRECTION ( 'NONE',  ( -1.000000000000000000, -0.000000000000000000, 0.000000000000000000 ) ) ;
#35746 = ORIENTED_EDGE ( 'NONE', *, *, #20951, .F. ) ;
#35747 = CARTESIAN_POINT ( 'NONE',  ( -35.50000000000000711, -120.0000000000000000, -2.500000000000000000 ) ) ;
#35748 = DIRECTION ( 'NONE',  ( 0.000000000000000000, 0.000000000000000000, 1.000000000000000000 ) ) ;
#35749 = ORIENTED_EDGE ( 'NONE', *, *, #53135, .T. ) ;
#35750 = CARTESIAN_POINT ( 'NONE',  ( 97.30629616937498838, -208.6684592857803295, 84.29822916753380468 ) ) ;
#35751 = CARTESIAN_POINT ( 'NONE',  ( 95.00000000000000000, -207.3369185715606307, 89.00781250086716057 ) ) ;
#35752 = VERTEX_POINT ( 'NONE', #13734 ) ;
#35753 = CARTESIAN_POINT ( 'NONE',  ( 97.30629616937498838, -209.9999999999999716, 88.84906250086716284 ) ) ;
#35754 = VERTEX_POINT ( 'NONE', #31023 ) ;
#35755 = DIRECTION ( 'NONE',  ( -0.000000000000000000, -0.6691306063588671194, 0.7431448254773862505 ) ) ;
#35756 = ORIENTED_EDGE ( 'NONE', *, *, #31246, .T. ) ;
#35757 = CARTESIAN_POINT ( 'NONE',  ( -92.69370383062504004, 90.00000000000004263, 79.95906250086714806 ) ) ;
#35758 = VECTOR ( 'NONE', #62237, 1000.000000000000114 ) ;
#35759 = ORIENTED_EDGE ( 'NONE', *, *, #34150, .T. ) ;
#35760 = ORIENTED_EDGE ( 'NONE', *, *, #68143, .T. ) ;
#35761 = CIRCLE ( 'NONE', #38190, 32.00000000000000000 ) ;
#35762 = CYLINDRICAL_SURFACE ( 'NONE', #54485, 77.49899999999999523 ) ;
#35763 = AXIS2_PLACEMENT_3D ( 'NONE', #5921, #27332, #73202 ) ;
#35764 = EDGE_LOOP ( 'NONE', ( #10530, #65306, #40001, #61226 ) ) ;
#35765 = DIRECTION ( 'NONE',  ( -0.9730327541852497042, 0.2306669878475622604, 0.000000000000000000 ) ) ;
#35766 = CYLINDRICAL_SURFACE ( 'NONE', #60883, 15.70000000000000284 ) ;
#35767 = CIRCLE ( 'NONE', #20153, 2.650000000000540812 ) ;
#35768 = VERTEX_POINT ( 'NONE', #42691 ) ;
#35769 = FACE_OUTER_BOUND ( 'NONE', #29384, .T. ) ;
#35770 = ORIENTED_EDGE ( 'NONE', *, *, #29348, .F. ) ;
#35771 = AXIS2_PLACEMENT_3D ( 'NONE', #66282, #49337, #72266 ) ;
#35772 = CARTESIAN_POINT ( 'NONE',  ( 92.35000000000000853, -209.9999844236436672, 80.55437446300187787 ) ) ;
#35773 = EDGE_LOOP ( 'NONE', ( #56402, #19262, #25962, #7350 ) ) ;
#35774 = ADVANCED_FACE ( 'NONE', ( #6989 ), #29912, .F. ) ;
#35775 = ORIENTED_EDGE ( 'NONE', *, *, #1266, .T. ) ;
#35776 = ORIENTED_EDGE ( 'NONE', *, *, #7641, .T. ) ;
#35777 = CARTESIAN_POINT ( 'NONE',  ( 95.00000000000000000, -212.6630814284392557, 81.54656250086715374 ) ) ;
#35778 = CARTESIAN_POINT ( 'NONE',  ( 10.00000000000000000, 10.74501242461282757, 35.92658777277515014 ) ) ;
#35779 = SHAPE_DEFINITION_REPRESENTATION ( #15781, #30982 ) ;
#35780 = DIRECTION ( 'NONE',  ( 1.000000000000000000, 0.000000000000000000, 0.000000000000000000 ) ) ;
#35781 = DIRECTION ( 'NONE',  ( 0.000000000000000000, 0.000000000000000000, 1.000000000000000000 ) ) ;
#35782 = CARTESIAN_POINT ( 'NONE',  ( -96.32499999999996021, -207.7050326799711968, 89.25916666666667254 ) ) ;
#35783 = EDGE_CURVE ( 'NONE', #5732, #5518, #7391, .T. ) ;
#35784 = CARTESIAN_POINT ( 'NONE',  ( 0.000000000000000000, -65.59268652807237743, 36.72794159290217664 ) ) ;
#35785 = FACE_OUTER_BOUND ( 'NONE', #31978, .T. ) ;
#35786 = CARTESIAN_POINT ( 'NONE',  ( -97.30629616937495996, -209.9999999999999716, 83.29281250086714294 ) ) ;
#35787 = EDGE_CURVE ( 'NONE', #65641, #64543, #57146, .T. ) ;
#35788 = CARTESIAN_POINT ( 'NONE',  ( -97.30629616937501680, 88.66845928578038638, 80.96447916753382401 ) ) ;
#35789 = ORIENTED_EDGE ( 'NONE', *, *, #12569, .F. ) ;
#35790 = CARTESIAN_POINT ( 'NONE',  ( 96.15314808468748708, 91.99731107132950569, 79.90614583420047268 ) ) ;
#35791 = EDGE_LOOP ( 'NONE', ( #47286, #40251 ) ) ;
#35792 = CYLINDRICAL_SURFACE ( 'NONE', #52711, 2.649999999999985700 ) ;
#35793 = LINE ( 'NONE', #18876, #19171 ) ;
#35794 = COLOUR_RGB ( '', 0.09019608, 0.27058824, 0.51372549) ;
#35795 = CARTESIAN_POINT ( 'NONE',  ( -12.50000000000000000, -132.5000000000000000, 40.00000000000000000 ) ) ;
#35796 = CARTESIAN_POINT ( 'NONE',  ( 10.00000000000000000, -50.95692526931286181, -58.39081064771806240 ) ) ;
#35797 = DIRECTION ( 'NONE',  ( -1.000000000000000000, 0.000000000000000000, 0.000000000000000000 ) ) ;
#35798 = CARTESIAN_POINT ( 'NONE',  ( -96.15314808468745866, -211.9973110713294489, 85.93864583420048575 ) ) ;
#35799 = CIRCLE ( 'NONE', #44245, 31.99999999999999645 ) ;
#35800 = DIRECTION ( 'NONE',  ( 1.000000000000000000, 0.000000000000000000, 0.000000000000000000 ) ) ;
#35801 = EDGE_CURVE ( 'NONE', #47809, #50757, #30192, .T. ) ;
#35802 = CARTESIAN_POINT ( 'NONE',  ( -3.000000000000000000, -14.54903810567645195, -22.19967320028775504 ) ) ;
#35803 = CARTESIAN_POINT ( 'NONE',  ( 10.00000000000000000, -49.70050353004846500, -59.46389618802017907 ) ) ;
#35804 = CARTESIAN_POINT ( 'NONE',  ( 11.99999999999999822, 10.30890764327382136, 81.34940948281339956 ) ) ;
#35805 = EDGE_LOOP ( 'NONE', ( #66591, #33736, #32879, #38394 ) ) ;
#35806 = AXIS2_PLACEMENT_3D ( 'NONE', #12881, #29801, #41468 ) ;
#35807 = EDGE_LOOP ( 'NONE', ( #2443, #22040, #37206, #71385 ) ) ;
#35808 = AXIS2_PLACEMENT_3D ( 'NONE', #46115, #57392, #57766 ) ;
#35809 = CARTESIAN_POINT ( 'NONE',  ( -92.35000000000005116, 91.52997821335253548, 75.13041666666666174 ) ) ;
#35810 = DIRECTION ( 'NONE',  ( -1.000000000000000000, 0.000000000000000000, -0.000000000000000000 ) ) ;
#35811 = CARTESIAN_POINT ( 'NONE',  ( 0.000000000000000000, -81.90746397400391743, 3.894527615417586741 ) ) ;
#35812 = DIRECTION ( 'NONE',  ( 1.000000000000000000, -0.000000000000000000, 0.000000000000000000 ) ) ;
#35813 = FACE_OUTER_BOUND ( 'NONE', #53627, .T. ) ;
#35814 = CYLINDRICAL_SURFACE ( 'NONE', #56593, 37.49900000000000233 ) ;
#35815 = CARTESIAN_POINT ( 'NONE',  ( 0.000000000000000000, -14.54903810567676636, 22.19967320028756319 ) ) ;
#35816 = EDGE_CURVE ( 'NONE', #11494, #34058, #4991, .T. ) ;
#35817 = ORIENTED_EDGE ( 'NONE', *, *, #68781, .T. ) ;
#35818 = CARTESIAN_POINT ( 'NONE',  ( -96.15314808468752972, 91.99731107132950569, 74.93197916753379673 ) ) ;
#35819 = CIRCLE ( 'NONE', #45462, 31.99999999999999645 ) ;
#35820 = DIRECTION ( 'NONE',  ( 0.000000000000000000, 0.4539904997395414754, 0.8910065241883706744 ) ) ;
#35821 = CARTESIAN_POINT ( 'NONE',  ( 0.000000000000000000, 0.000000000000000000, 0.000000000000000000 ) ) ;
#35822 = CARTESIAN_POINT ( 'NONE',  ( 92.35000000000002274, -210.0000225213918554, 84.36437578067152288 ) ) ;
#35823 = AXIS2_PLACEMENT_3D ( 'NONE', #2565, #25445, #25813 ) ;
#35824 = DIRECTION ( 'NONE',  ( -1.000000000000000000, 0.000000000000000000, 0.000000000000000000 ) ) ;
#35825 = CARTESIAN_POINT ( 'NONE',  ( -97.30629616937497417, -208.6684592857803011, 86.57364583420047666 ) ) ;
#35826 =( NAMED_UNIT ( * ) PLANE_ANGLE_UNIT ( ) SI_UNIT ( $, .RADIAN. ) );
#35827 = AXIS2_PLACEMENT_3D ( 'NONE', #69223, #50802, #17710 ) ;
#35828 = EDGE_CURVE ( 'NONE', #2059, #19149, #63805, .T. ) ;
#35829 = CARTESIAN_POINT ( 'NONE',  ( 10.00000000000000000, -0.8828120875898013420, -37.48860685352291711 ) ) ;
#35830 = ADVANCED_FACE ( 'NONE', ( #30650 ), #15961, .T. ) ;
#35831 = AXIS2_PLACEMENT_3D ( 'NONE', #43994, #66910, #60551 ) ;
#35832 =( BOUNDED_CURVE ( )  B_SPLINE_CURVE ( 2, ( #72414, #43868, #14536, #3292, #56253, #21659, #73156 ),
 .UNSPECIFIED., .F., .F. ) 
 B_SPLINE_CURVE_WITH_KNOTS ( ( 3, 2, 2, 3 ),
 ( 0.7916666666666669627, 0.7986111111111114935, 0.8055555555555558023, 0.8125000000000002220 ),
 .UNSPECIFIED. ) 
 CURVE ( )  GEOMETRIC_REPRESENTATION_ITEM ( )  RATIONAL_B_SPLINE_CURVE ( ( 0.9999999999999935607, 0.8660254037844451469, 1.000000000000000000, 0.8660254037844387076, 1.000000000000000000, 0.8660254037844343777, 1.000000000000004219 ) ) 
 REPRESENTATION_ITEM ( '' )  );
#35833 = ADVANCED_FACE ( 'NONE', ( #21217, #55073 ), #60364, .F. ) ;
#35834 = CARTESIAN_POINT ( 'NONE',  ( 92.35000000006144205, 90.00001182178868930, 76.10900611559256390 ) ) ;
#35835 = CARTESIAN_POINT ( 'NONE',  ( -92.69370383062498320, -208.6684592857803295, 74.93197916753381094 ) ) ;
#35836 = LINE ( 'NONE', #6545, #27825 ) ;
#35837 = ORIENTED_EDGE ( 'NONE', *, *, #2151, .T. ) ;
#35838 = CARTESIAN_POINT ( 'NONE',  ( 0.000000000000000000, 0.000000000000000000, 0.000000000000000000 ) ) ;
#35839 = CARTESIAN_POINT ( 'NONE',  ( -7.893099573151324044, -11.68370571044642503, 0.000000000000000000 ) ) ;
#35840 = DIRECTION ( 'NONE',  ( -0.000000000000000000, -0.000000000000000000, 1.000000000000000000 ) ) ;
#35841 = CARTESIAN_POINT ( 'NONE',  ( -92.69370383062505425, 88.66845928578038638, 75.46114583420049371 ) ) ;
#35842 = CARTESIAN_POINT ( 'NONE',  ( 97.30629616937498838, -208.6684592857803011, 76.67822916753378593 ) ) ;
#35843 = ORIENTED_EDGE ( 'NONE', *, *, #30473, .F. ) ;
#35844 = CARTESIAN_POINT ( 'NONE',  ( 10.00000000000000000, 0.000000000000000000, 0.000000000000000000 ) ) ;
#35845 = EDGE_LOOP ( 'NONE', ( #23799, #5719 ) ) ;
#35846 = CIRCLE ( 'NONE', #68292, 32.00000000000000000 ) ;
#35847 = DIRECTION ( 'NONE',  ( -0.000000000000000000, -0.000000000000000000, 1.000000000000000000 ) ) ;
#35848 = ORIENTED_EDGE ( 'NONE', *, *, #5879, .F. ) ;
#35849 = CIRCLE ( 'NONE', #69458, 77.49899999999999523 ) ;
#35850 = AXIS2_PLACEMENT_3D ( 'NONE', #24650, #53228, #1763 ) ;
#35851 = CARTESIAN_POINT ( 'NONE',  ( -97.64999999992180335, 90.00001303125199570, 79.28395951162846700 ) ) ;
#35852 = AXIS2_PLACEMENT_3D ( 'NONE', #63590, #18083, #28235 ) ;
#35853 = ORIENTED_EDGE ( 'NONE', *, *, #49533, .F. ) ;
#35854 = VERTEX_POINT ( 'NONE', #3966 ) ;
#35855 = AXIS2_PLACEMENT_3D ( 'NONE', #14667, #31220, #25580 ) ;
#35856 = ORIENTED_EDGE ( 'NONE', *, *, #29375, .F. ) ;
#35857 = CARTESIAN_POINT ( 'NONE',  ( -97.64999999999996305, -209.9999999999999716, 77.29999999999999716 ) ) ;
#35858 = ORIENTED_EDGE ( 'NONE', *, *, #68405, .T. ) ;
#35859 = VERTEX_POINT ( 'NONE', #48692 ) ;
#35860 = CARTESIAN_POINT ( 'NONE',  ( 97.30629616937498838, 88.66845928578037217, 78.63614583420049087 ) ) ;
#35861 = DIRECTION ( 'NONE',  ( -3.061616997868382648E-16, -1.000000000000000000, -5.966227995846078450E-16 ) ) ;
#35862 = CARTESIAN_POINT ( 'NONE',  ( 97.64999999999997726, -208.4700217866474645, 75.76541666666666686 ) ) ;
#35863 = VECTOR ( 'NONE', #46003, 1000.000000000000000 ) ;
#35864 = ORIENTED_EDGE ( 'NONE', *, *, #41951, .T. ) ;
#35866 = EDGE_LOOP ( 'NONE', ( #9428, #62324, #14756, #16633 ) ) ;
#35865 = VECTOR ( 'NONE', #41365, 1000.000000000000114 ) ;
#35867 = EDGE_CURVE ( 'NONE', #15883, #29404, #56615, .T. ) ;
#35868 = ORIENTED_EDGE ( 'NONE', *, *, #49340, .T. ) ;
#35869 = CARTESIAN_POINT ( 'NONE',  ( 0.000000000000000000, 55.19960302592141232, -51.03279382321027668 ) ) ;
#35870 = ORIENTED_EDGE ( 'NONE', *, *, #37665, .F. ) ;
#35871 = AXIS2_PLACEMENT_3D ( 'NONE', #63917, #47351, #12385 ) ;
#35872 = FILL_AREA_STYLE_COLOUR ( '', #33918 ) ;
#35873 = CARTESIAN_POINT ( 'NONE',  ( -11.99999999999999645, 0.000000000000000000, 12.85999999999999943 ) ) ;
#35874 = CARTESIAN_POINT ( 'NONE',  ( 93.67499999999999716, 87.70503267997126784, 83.75583333333332803 ) ) ;
#35875 = CARTESIAN_POINT ( 'NONE',  ( 10.00000000000000000, 80.55351364060589958, 15.33399622253511829 ) ) ;
#35876 = CARTESIAN_POINT ( 'NONE',  ( 0.000000000000000000, -39.78640506895651185, 66.50666863321987421 ) ) ;
#35877 = ADVANCED_FACE ( 'NONE', ( #59996 ), #32870, .F. ) ;
#35878 = DIRECTION ( 'NONE',  ( 0.000000000000000000, -0.000000000000000000, -1.000000000000000000 ) ) ;
#35879 = CARTESIAN_POINT ( 'NONE',  ( 10.00000000000000000, 37.01155633439068282, -6.555932627142014191 ) ) ;
#35880 = CIRCLE ( 'NONE', #3498, 13.71399988598171049 ) ;
#35881 = CARTESIAN_POINT ( 'NONE',  ( -97.64999999999996305, -209.9999999999999716, 79.28437500173430408 ) ) ;
#35882 = EDGE_CURVE ( 'NONE', #39410, #23684, #15595, .T. ) ;
#35883 = FACE_OUTER_BOUND ( 'NONE', #48571, .T. ) ;
#35884 = ORIENTED_EDGE ( 'NONE', *, *, #58666, .T. ) ;
#35886 = CARTESIAN_POINT ( 'NONE',  ( -96.32500000000001705, 92.29496732002878900, 76.00354166840097037 ) ) ;
#35885 = CARTESIAN_POINT ( 'NONE',  ( 94.99999999999998579, 86.94004357329500010, 76.90312500173429555 ) ) ;
#35887 = AXIS2_PLACEMENT_3D ( 'NONE', #67104, #72370, #61481 ) ;
#35888 = VERTEX_POINT ( 'NONE', #14852 ) ;
#35889 = CARTESIAN_POINT ( 'NONE',  ( 93.84685191531248449, 91.99731107132950569, 80.17072916753382117 ) ) ;
#35890 = LINE ( 'NONE', #64853, #18153 ) ;
#35891 = DIRECTION ( 'NONE',  ( 1.000000000000000000, 0.000000000000000000, 0.000000000000000000 ) ) ;
#35892 = DIRECTION ( 'NONE',  ( -0.000000000000000000, -0.8660254037844427044, 0.4999999999999929501 ) ) ;
#35893 = CARTESIAN_POINT ( 'NONE',  ( 5.999999999999999112, -63.97538442413463855, 51.29473840253199057 ) ) ;
#35894 = DIRECTION ( 'NONE',  ( -0.5687579148473752566, 0.8225049752423786442, 0.000000000000000000 ) ) ;
#35895 = ADVANCED_FACE ( 'NONE', ( #26126 ), #27225, .F. ) ;
#35896 = VERTEX_POINT ( 'NONE', #66732 ) ;
#35897 = DIRECTION ( 'NONE',  ( 0.000000000000000000, -0.1045284632676578285, 0.9945218953682729568 ) ) ;
#35898 = LINE ( 'NONE', #12602, #42015 ) ;
#35899 = ORIENTED_EDGE ( 'NONE', *, *, #49841, .T. ) ;
#35900 = ORIENTED_EDGE ( 'NONE', *, *, #67536, .T. ) ;
#35901 = VECTOR ( 'NONE', #42557, 1000.000000000000000 ) ;
#35902 = CARTESIAN_POINT ( 'NONE',  ( 97.64999999999999147, -209.9999999999999716, 90.00000000000000000 ) ) ;
#35904 = EDGE_CURVE ( 'NONE', #58272, #39711, #15221, .T. ) ;
#35903 = CARTESIAN_POINT ( 'NONE',  ( 10.00000000000000000, -26.01480285779885904, 70.53064760720306481 ) ) ;
#35905 = CARTESIAN_POINT ( 'NONE',  ( -1.084202172485504434E-14, -5.773502691896260863, -2.080000000000000071 ) ) ;
#35906 = LINE ( 'NONE', #7355, #54120 ) ;
#35907 = CARTESIAN_POINT ( 'NONE',  ( -96.15314808468745866, -211.9973110713294489, 77.84239583420048803 ) ) ;
#35908 = STYLED_ITEM ( 'NONE', ( #45160 ), #63624 ) ;
#35909 = ADVANCED_FACE ( 'NONE', ( #71986 ), #54346, .F. ) ;
#35910 = ORIENTED_EDGE ( 'NONE', *, *, #59072, .T. ) ;
#35911 = AXIS2_PLACEMENT_3D ( 'NONE', #57606, #62514, #130 ) ;
#35913 = DIRECTION ( 'NONE',  ( 1.000000000000000000, 0.000000000000000000, 0.000000000000000000 ) ) ;
#35912 = CIRCLE ( 'NONE', #9508, 77.49899999999999523 ) ;
#35914 = DIRECTION ( 'NONE',  ( -0.000000000000000000, -0.000000000000000000, 1.000000000000000000 ) ) ;
#35915 = DIRECTION ( 'NONE',  ( -1.000000000000000000, 0.000000000000000000, 0.000000000000000000 ) ) ;
#35916 = DIRECTION ( 'NONE',  ( -0.000000000000000000, -0.000000000000000000, -1.000000000000000000 ) ) ;
#35917 = AXIS2_PLACEMENT_3D ( 'NONE', #52581, #6011, #70224 ) ;
#35918 = CARTESIAN_POINT ( 'NONE',  ( 0.000000000000000000, -34.44570377933549565, -69.42325613327476219 ) ) ;
#35919 = CARTESIAN_POINT ( 'NONE',  ( 0.000000000000000000, 29.01471420065673712, -76.69515212745984911 ) ) ;
#35920 = CARTESIAN_POINT ( 'NONE',  ( -94.99999999999997158, -209.9999999999999716, 90.00000000000000000 ) ) ;
#35921 = CARTESIAN_POINT ( 'NONE',  ( 0.000000000000000000, 73.72996012237440766, 14.67089635893739619 ) ) ;
#35922 = CYLINDRICAL_SURFACE ( 'NONE', #474, 37.49900000000000233 ) ;
#35923 = CARTESIAN_POINT ( 'NONE',  ( 0.000000000000000000, 26.01480285779933510, -70.53064760720289428 ) ) ;
#35924 = EDGE_CURVE ( 'NONE', #41826, #37007, #21771, .T. ) ;
#35925 = ADVANCED_FACE ( 'NONE', ( #4332 ), #20501, .T. ) ;
#35926 = CARTESIAN_POINT ( 'NONE',  ( 97.30629616937498838, 91.33154071421968467, 82.55197916753380127 ) ) ;
#35927 = CIRCLE ( 'NONE', #73106, 12.75000000000265388 ) ;
#35928 = CARTESIAN_POINT ( 'NONE',  ( -97.30629616937497417, -208.6684592857803295, 86.57364583420047666 ) ) ;
#35929 = DIRECTION ( 'NONE',  ( -1.000000000000000000, 0.000000000000000000, 0.000000000000000000 ) ) ;
#35930 = AXIS2_PLACEMENT_3D ( 'NONE', #50322, #42839, #66515 ) ;
#35931 = ORIENTED_EDGE ( 'NONE', *, *, #64439, .F. ) ;
#35932 = DIRECTION ( 'NONE',  ( 1.000000000000000000, 0.000000000000000000, 0.000000000000000000 ) ) ;
#35933 = CARTESIAN_POINT ( 'NONE',  ( -92.34999999999999432, -208.4700217866474645, 81.48041666666665606 ) ) ;
#35934 = CARTESIAN_POINT ( 'NONE',  ( -95.00000000000002842, 92.66308142843932671, 74.87906250086713555 ) ) ;
#35935 = CIRCLE ( 'NONE', #71932, 30.50000000000000000 ) ;
#35936 = AXIS2_PLACEMENT_3D ( 'NONE', #33756, #45804, #63099 ) ;
#35937 = CIRCLE ( 'NONE', #21491, 37.49900000000000944 ) ;
#35938 = AXIS2_PLACEMENT_3D ( 'NONE', #5269, #57129, #62030 ) ;
#35939 = CARTESIAN_POINT ( 'NONE',  ( 97.30629616937498838, -211.3315407142195852, 88.63739583420047552 ) ) ;
#35940 = EDGE_LOOP ( 'NONE', ( #3979, #72535, #25632, #47690, #15453 ) ) ;
#35941 = VERTEX_POINT ( 'NONE', #67094 ) ;
#35942 = ORIENTED_EDGE ( 'NONE', *, *, #22883, .F. ) ;
#35943 = CARTESIAN_POINT ( 'NONE',  ( 0.000000000000000000, 76.69515212746057387, -29.01471420065480089 ) ) ;
#35944 = CARTESIAN_POINT ( 'NONE',  ( 10.00000000000000000, 26.08949754953024325, 27.05870788708241648 ) ) ;
#35945 = ORIENTED_EDGE ( 'NONE', *, *, #42872, .F. ) ;
#35946 = ORIENTED_EDGE ( 'NONE', *, *, #29586, .T. ) ;
#35947 = LINE ( 'NONE', #65281, #70664 ) ;
#35948 = CARTESIAN_POINT ( 'NONE',  ( 97.30629616937498838, -211.3315407142195852, 81.17614583420049712 ) ) ;
#35949 = DIRECTION ( 'NONE',  ( 0.000000000000000000, 0.000000000000000000, 1.000000000000000000 ) ) ;
#35950 = CARTESIAN_POINT ( 'NONE',  ( 96.32499999999997442, 92.29496732002878900, 80.89833333333332632 ) ) ;
#35951 = CARTESIAN_POINT ( 'NONE',  ( 11.99999999999999822, 46.54456581323888997, -59.03342792756214408 ) ) ;
#35952 = DIRECTION ( 'NONE',  ( -1.000000000000000000, 0.000000000000000000, 0.000000000000000000 ) ) ;
#35953 = AXIS2_PLACEMENT_3D ( 'NONE', #31179, #53384, #47736 ) ;
#35954 = CARTESIAN_POINT ( 'NONE',  ( 12.50000000000000000, -120.0000000000000000, 40.00000000000000711 ) ) ;
#35955 = CARTESIAN_POINT ( 'NONE',  ( 92.35000000000002274, -208.4700217866474645, 85.50208333333331723 ) ) ;
#35956 = AXIS2_PLACEMENT_3D ( 'NONE', #38629, #10043, #32599 ) ;
#35957 = EDGE_CURVE ( 'NONE', #73349, #42384, #9209, .T. ) ;
#35958 = ORIENTED_EDGE ( 'NONE', *, *, #70662, .T. ) ;
#35959 = ORIENTED_EDGE ( 'NONE', *, *, #40184, .F. ) ;
#35960 = VERTEX_POINT ( 'NONE', #43074 ) ;
#35961 = ORIENTED_EDGE ( 'NONE', *, *, #22081, .F. ) ;
#35962 = SURFACE_STYLE_USAGE ( .BOTH. , #58525 ) ;
#35963 = ADVANCED_FACE ( 'NONE', ( #72361 ), #38152, .F. ) ;
#35964 = CARTESIAN_POINT ( 'NONE',  ( -92.69370383062502583, 91.33154071421968467, 86.99697916753382287 ) ) ;
#35965 = FACE_OUTER_BOUND ( 'NONE', #72386, .T. ) ;
#35966 = AXIS2_PLACEMENT_3D ( 'NONE', #10305, #16691, #38879 ) ;
#35967 = FACE_OUTER_BOUND ( 'NONE', #70621, .T. ) ;
#35968 = CARTESIAN_POINT ( 'NONE',  ( 92.69370383062501162, -208.6684592857803011, 87.68489583420047495 ) ) ;
#35969 = ADVANCED_FACE ( 'NONE', ( #25763 ), #50159, .T. ) ;
#35970 = CARTESIAN_POINT ( 'NONE',  ( 97.64999999999999147, 90.00000000000002842, 77.61749999999999261 ) ) ;
#35971 = ORIENTED_EDGE ( 'NONE', *, *, #31212, .F. ) ;
#35972 = DIRECTION ( 'NONE',  ( 1.000000000000000000, -0.000000000000000000, -0.000000000000000000 ) ) ;
#35973 = ORIENTED_EDGE ( 'NONE', *, *, #23005, .F. ) ;
#35974 = CARTESIAN_POINT ( 'NONE',  ( 92.35000000000000853, -209.9999999999999716, 79.83999999999998920 ) ) ;
#35975 = ORIENTED_EDGE ( 'NONE', *, *, #12366, .F. ) ;
#35976 = CARTESIAN_POINT ( 'NONE',  ( -97.65000000000001990, 88.47002178664754979, 85.05229166840096866 ) ) ;
#35977 = CARTESIAN_POINT ( 'NONE',  ( 92.69370383062498320, 90.00000000000002842, 75.67281250086713840 ) ) ;
#35978 = VERTEX_POINT ( 'NONE', #71616 ) ;
#35979 = CYLINDRICAL_SURFACE ( 'NONE', #21379, 77.49899999999999523 ) ;
#35980 = CARTESIAN_POINT ( 'NONE',  ( -103.9230484541323705, -180.0000000000004832, 5.500000000000000000 ) ) ;
#35981 = AXIS2_PLACEMENT_3D ( 'NONE', #17512, #28045, #22803 ) ;
#35982 = DIRECTION ( 'NONE',  ( -1.000000000000000000, 0.000000000000000000, 0.000000000000000000 ) ) ;
#35983 = ADVANCED_FACE ( 'NONE', ( #20113 ), #14480, .T. ) ;
#35984 = CARTESIAN_POINT ( 'NONE',  ( -97.64999999980587120, -210.0000198427943587, 86.27002759516035724 ) ) ;
#35985 = ORIENTED_EDGE ( 'NONE', *, *, #15553, .F. ) ;
#35986 = DIRECTION ( 'NONE',  ( -1.000000000000000000, -0.000000000000000000, -0.000000000000000000 ) ) ;
#35987 = CIRCLE ( 'NONE', #50362, 31.99999999999999289 ) ;
#35989 = CARTESIAN_POINT ( 'NONE',  ( -94.99999999999997158, -212.6630814284392557, 75.19656250086714522 ) ) ;
#35988 = CIRCLE ( 'NONE', #32385, 16.00000000000000355 ) ;
#35990 = ORIENTED_EDGE ( 'NONE', *, *, #19196, .F. ) ;
#35991 = ORIENTED_EDGE ( 'NONE', *, *, #62393, .F. ) ;
#35992 = FACE_OUTER_BOUND ( 'NONE', #33079, .T. ) ;
#35993 = AXIS2_PLACEMENT_3D ( 'NONE', #70817, #31336, #8041 ) ;
#35994 = AXIS2_PLACEMENT_3D ( 'NONE', #67198, #19839, #15697 ) ;
#35995 = CARTESIAN_POINT ( 'NONE',  ( -8.826826895187510402, -94.96827758698185562, 5.500000000000000000 ) ) ;
#35996 = EDGE_CURVE ( 'NONE', #63454, #68556, #28346, .T. ) ;
#35997 = CARTESIAN_POINT ( 'NONE',  ( -0.0004442498512760095037, 0.001194404164628348752, -49.00000000000000000 ) ) ;
#35998 = CARTESIAN_POINT ( 'NONE',  ( -97.30629616937497417, -208.6684592857803011, 87.20864583420049598 ) ) ;
#35999 = ORIENTED_EDGE ( 'NONE', *, *, #9495, .T. ) ;
#36000 =( LENGTH_UNIT ( ) NAMED_UNIT ( * ) SI_UNIT ( .MILLI., .METRE. ) );
#36001 = EDGE_CURVE ( 'NONE', #46606, #37162, #46391, .T. ) ;
#36002 = ORIENTED_EDGE ( 'NONE', *, *, #37623, .T. ) ;
#36003 = ORIENTED_EDGE ( 'NONE', *, *, #14097, .F. ) ;
#36004 = CARTESIAN_POINT ( 'NONE',  ( -92.35001333515640454, 91.52998591240866233, 83.46479220096853169 ) ) ;
#36005 = ADVANCED_FACE ( 'NONE', ( #67843 ), #73444, .T. ) ;
#36006 = ADVANCED_FACE ( 'NONE', ( #10694 ), #11788, .T. ) ;
#36007 = CARTESIAN_POINT ( 'NONE',  ( 97.30629616937498838, 91.33154071421968467, 89.53697916753382913 ) ) ;
#36008 = FACE_OUTER_BOUND ( 'NONE', #27572, .T. ) ;
#36009 = CARTESIAN_POINT ( 'NONE',  ( 97.30629616937498838, 90.00000000000002842, 80.43531250086714124 ) ) ;
#36010 = DIRECTION ( 'NONE',  ( -1.000000000000000000, 0.000000000000000000, -0.000000000000000000 ) ) ;
#36011 = CARTESIAN_POINT ( 'NONE',  ( 23.41451323550360186, -132.5004227906269989, -5.500000000000000000 ) ) ;
#36012 = LINE ( 'NONE', #42037, #34907 ) ;
#36013 = DIRECTION ( 'NONE',  ( -0.000000000000000000, 0.9945218953682744001, 0.1045284632676437842 ) ) ;
#36014 = LINE ( 'NONE', #31108, #74081 ) ;
#36015 = DIRECTION ( 'NONE',  ( -1.000000000000000000, -0.000000000000000000, -0.000000000000000000 ) ) ;
#36016 = FACE_OUTER_BOUND ( 'NONE', #21333, .T. ) ;
#36017 = ADVANCED_FACE ( 'NONE', ( #44923 ), #23100, .F. ) ;
#36018 = VECTOR ( 'NONE', #22304, 1000.000000000000000 ) ;
#36019 = CARTESIAN_POINT ( 'NONE',  ( 97.64999999999990621, -209.9999992849081139, 85.31687502647973531 ) ) ;
#36020 = ADVANCED_FACE ( 'NONE', ( #33621 ), #38901, .T. ) ;
#36021 = DIRECTION ( 'NONE',  ( 0.000000000000000000, 0.000000000000000000, 1.000000000000000000 ) ) ;
#36022 = CIRCLE ( 'NONE', #1241, 82.00000000000000000 ) ;
#36023 = CARTESIAN_POINT ( 'NONE',  ( -92.69370383062505425, 88.66845928578038638, 85.46239583420044994 ) ) ;
#36024 = CARTESIAN_POINT ( 'NONE',  ( 0.000000000000000000, 35.92658777277510040, 10.74501242461294659 ) ) ;
#36025 = AXIS2_PLACEMENT_3D ( 'NONE', #54843, #31531, #66506 ) ;
#36026 = CARTESIAN_POINT ( 'NONE',  ( 0.3000000000000016542, 5.755839955992559655E-16, -4.700000000000000178 ) ) ;
#36027 = EDGE_LOOP ( 'NONE', ( #8905, #3833, #9603, #31269 ) ) ;
#36028 = PLANE ( 'NONE',  #64270 ) ;
#36029 = DIRECTION ( 'NONE',  ( 0.000000000000000000, 0.9945218953682742891, -0.1045284632676436315 ) ) ;
#36030 = DIRECTION ( 'NONE',  ( 1.000000000000000000, 0.000000000000000000, 0.000000000000000000 ) ) ;
#36031 = CIRCLE ( 'NONE', #45672, 12.50000000000000000 ) ;
#36032 = CARTESIAN_POINT ( 'NONE',  ( -35.37301231164799731, -117.0000000000000000, 2.500000000000000000 ) ) ;
#36033 = VECTOR ( 'NONE', #9292, 1000.000000000000000 ) ;
#36034 = CIRCLE ( 'NONE', #16677, 77.49899999999999523 ) ;
#36035 = CARTESIAN_POINT ( 'NONE',  ( 97.30629616937498838, -209.9999999999999716, 82.49906250086715431 ) ) ;
#36036 = ORIENTED_EDGE ( 'NONE', *, *, #33926, .T. ) ;
#36037 = CIRCLE ( 'NONE', #12001, 16.00000000000000000 ) ;
#36038 = ORIENTED_EDGE ( 'NONE', *, *, #12546, .F. ) ;
#36039 = VECTOR ( 'NONE', #34278, 1000.000000000000000 ) ;
#36040 = CARTESIAN_POINT ( 'NONE',  ( 2.184357737007946383E-12, -120.0000000000000000, -48.99999999999997158 ) ) ;
#36041 = EDGE_LOOP ( 'NONE', ( #30965, #58437, #53729, #11499 ) ) ;
#36042 = DIRECTION ( 'NONE',  ( 0.000000000000000000, 1.053567635648656885E-14, 1.000000000000000000 ) ) ;
#36043 =( BOUNDED_CURVE ( )  B_SPLINE_CURVE ( 2, ( #26583, #49516, #72438, #20941, #15301, #43897, #38238 ),
 .UNSPECIFIED., .F., .F. ) 
 B_SPLINE_CURVE_WITH_KNOTS ( ( 3, 2, 2, 3 ),
 ( 0.1874999999999999167, 0.1944444444444443365, 0.2013888888888887285, 0.2083333333333331483 ),
 .UNSPECIFIED. ) 
 CURVE ( )  GEOMETRIC_REPRESENTATION_ITEM ( )  RATIONAL_B_SPLINE_CURVE ( ( 1.000000000000001554, 0.8660254037844371533, 1.000000000000000000, 0.8660254037844387076, 1.000000000000000000, 0.8660254037844424824, 0.9999999999999962252 ) ) 
 REPRESENTATION_ITEM ( '' )  );
#36044 = CARTESIAN_POINT ( 'NONE',  ( 97.30629616937498838, -208.6684592857803295, 75.40822916753381833 ) ) ;
#36045 = ORIENTED_EDGE ( 'NONE', *, *, #66628, .F. ) ;
#36046 = CARTESIAN_POINT ( 'NONE',  ( 93.84685191531251292, -211.9973110713294489, 80.38239583420048007 ) ) ;
#36047 = ORIENTED_EDGE ( 'NONE', *, *, #33346, .F. ) ;
#36048 = ADVANCED_FACE ( 'NONE', ( #63326 ), #50915, .T. ) ;
#36049 = DIRECTION ( 'NONE',  ( -1.000000000000000000, -0.000000000000000000, -0.000000000000000000 ) ) ;
#36050 = ORIENTED_EDGE ( 'NONE', *, *, #73186, .F. ) ;
#36051 = AXIS2_PLACEMENT_3D ( 'NONE', #19103, #48055, #2608 ) ;
#36052 = ORIENTED_EDGE ( 'NONE', *, *, #22594, .T. ) ;
#36053 = CARTESIAN_POINT ( 'NONE',  ( 10.00000000000000000, -35.92658777277517856, 10.74501242461269257 ) ) ;
#36054 = EDGE_CURVE ( 'NONE', #33176, #38913, #27613, .T. ) ;
#36055 = DIRECTION ( 'NONE',  ( -1.000000000000000000, 0.000000000000000000, -0.000000000000000000 ) ) ;
#36056 = ORIENTED_EDGE ( 'NONE', *, *, #40560, .F. ) ;
#36057 = DIRECTION ( 'NONE',  ( 1.000000000000000000, -3.061616997868382648E-16, -0.000000000000000000 ) ) ;
#36058 = CARTESIAN_POINT ( 'NONE',  ( 96.32499999999998863, -212.2949673200287179, 82.67104166840096013 ) ) ;
#36059 = EDGE_CURVE ( 'NONE', #38545, #50675, #57683, .T. ) ;
#36060 = CARTESIAN_POINT ( 'NONE',  ( 96.66079198124940319, 88.39975876321993553, 74.80065669543250806 ) ) ;
#36061 = EDGE_CURVE ( 'NONE', #11811, #51313, #59073, .T. ) ;
#36062 = ORIENTED_EDGE ( 'NONE', *, *, #53449, .F. ) ;
#36063 = DIRECTION ( 'NONE',  ( 0.000000000000000000, 0.000000000000000000, -1.000000000000000000 ) ) ;
#36064 = DIRECTION ( 'NONE',  ( -0.000000000000000000, -0.000000000000000000, 1.000000000000000000 ) ) ;
#36065 = ORIENTED_EDGE ( 'NONE', *, *, #41516, .T. ) ;
#36066 = ORIENTED_EDGE ( 'NONE', *, *, #47358, .F. ) ;
#36067 = CARTESIAN_POINT ( 'NONE',  ( -92.69370383062505425, 88.66845928578038638, 86.89114583420048632 ) ) ;
#36068 = ORIENTED_EDGE ( 'NONE', *, *, #62145, .F. ) ;
#36069 = CARTESIAN_POINT ( 'NONE',  ( 93.67499999999999716, 87.70503267997126784, 84.47020833506762472 ) ) ;
#36070 = AXIS2_PLACEMENT_3D ( 'NONE', #36198, #42227, #48592 ) ;
#36071 =( NAMED_UNIT ( * ) PLANE_ANGLE_UNIT ( ) SI_UNIT ( $, .RADIAN. ) );
#36072 = ORIENTED_EDGE ( 'NONE', *, *, #36515, .F. ) ;
#36073 = CARTESIAN_POINT ( 'NONE',  ( 0.000000000000000000, 0.000000000000000000, -6.000000000000000000 ) ) ;
#36074 = VECTOR ( 'NONE', #52855, 1000.000000000000000 ) ;
#36075 = DIRECTION ( 'NONE',  ( -1.000000000000000000, 0.000000000000000000, 0.000000000000000000 ) ) ;
#36076 = ORIENTED_EDGE ( 'NONE', *, *, #70842, .T. ) ;
#36077 = VERTEX_POINT ( 'NONE', #61838 ) ;
#36078 = EDGE_CURVE ( 'NONE', #63015, #61302, #28722, .T. ) ;
#36079 = AXIS2_PLACEMENT_3D ( 'NONE', #20917, #66782, #31077 ) ;
#36080 = VERTEX_POINT ( 'NONE', #33995 ) ;
#36081 = FACE_OUTER_BOUND ( 'NONE', #17310, .T. ) ;
#36082 = CARTESIAN_POINT ( 'NONE',  ( 97.64999999999999147, 90.00000000000002842, 81.42749999999999488 ) ) ;
#36083 = EDGE_CURVE ( 'NONE', #6231, #44562, #62593, .T. ) ;
#36084 = CARTESIAN_POINT ( 'NONE',  ( -92.35000000000005116, 91.52997821335253548, 85.92541666666664923 ) ) ;
#36085 = ORIENTED_EDGE ( 'NONE', *, *, #66207, .T. ) ;
#36086 = CARTESIAN_POINT ( 'NONE',  ( 7.103376864691351012E-17, -120.0000000000000000, -90.00000000000000000 ) ) ;
#36087 = DIRECTION ( 'NONE',  ( -0.000000000000000000, -0.000000000000000000, 1.000000000000000000 ) ) ;
#36088 = EDGE_LOOP ( 'NONE', ( #10157, #29102, #51065, #33547 ) ) ;
#36089 = DIRECTION ( 'NONE',  ( -0.000000000000000000, -0.000000000000000000, 1.000000000000000000 ) ) ;
#36090 = CARTESIAN_POINT ( 'NONE',  ( -92.69370383062498320, -209.9999999999999716, 84.24531250086714351 ) ) ;
#36091 = ORIENTED_EDGE ( 'NONE', *, *, #47979, .T. ) ;
#36092 = CARTESIAN_POINT ( 'NONE',  ( 10.00000000000000000, 0.000000000000000000, 0.000000000000000000 ) ) ;
#36093 = CARTESIAN_POINT ( 'NONE',  ( 0.000000000000000000, 50.23322058963348979, 64.81221759200361987 ) ) ;
#36094 = FACE_OUTER_BOUND ( 'NONE', #26353, .T. ) ;
#36095 = DIRECTION ( 'NONE',  ( -0.9038112904824846527, 0.4279312458752990711, 0.000000000000000000 ) ) ;
#36096 = LINE ( 'NONE', #18072, #18745 ) ;
#36097 = AXIS2_PLACEMENT_3D ( 'NONE', #10934, #804, #58276 ) ;
#36098 = EDGE_CURVE ( 'NONE', #13520, #23087, #61976, .T. ) ;
#36099 = EDGE_CURVE ( 'NONE', #9267, #55524, #45298, .T. ) ;
#36100 = AXIS2_PLACEMENT_3D ( 'NONE', #31173, #54125, #66149 ) ;
#36101 = DIRECTION ( 'NONE',  ( 0.000000000000000000, 0.000000000000000000, 1.000000000000000000 ) ) ;
#36102 = DIRECTION ( 'NONE',  ( 0.000000000000000000, 0.000000000000000000, -1.000000000000000000 ) ) ;
#36103 = DIRECTION ( 'NONE',  ( -1.000000000000000000, 0.000000000000000000, -0.000000000000000000 ) ) ;
#36104 = AXIS2_PLACEMENT_3D ( 'NONE', #52029, #62977, #45682 ) ;
#36105 = CARTESIAN_POINT ( 'NONE',  ( 94.99999999999998579, 93.05995642670504253, 82.93562500173430863 ) ) ;
#36106 = CARTESIAN_POINT ( 'NONE',  ( 0.000000000000000000, 55.16347631943131802, -60.67117009219074930 ) ) ;
#36107 = CARTESIAN_POINT ( 'NONE',  ( -92.69370383062504004, 90.00000000000004263, 74.72031250086713783 ) ) ;
#36108 = DIRECTION ( 'NONE',  ( 0.000000000000000000, 0.000000000000000000, 1.000000000000000000 ) ) ;
#36109 = DIRECTION ( 'NONE',  ( -1.000000000000000000, -0.000000000000000000, -0.000000000000000000 ) ) ;
#36110 = CARTESIAN_POINT ( 'NONE',  ( 0.000000000000000000, 0.000000000000000000, -56.19999999999998863 ) ) ;
#36111 = FACE_OUTER_BOUND ( 'NONE', #23677, .T. ) ;
#36112 = CYLINDRICAL_SURFACE ( 'NONE', #28633, 16.00000000000000000 ) ;
#36113 = DIRECTION ( 'NONE',  ( 0.000000000000000000, 0.000000000000000000, 1.000000000000000000 ) ) ;
#36114 = CARTESIAN_POINT ( 'NONE',  ( 11.99999999999999822, -50.95692526931372157, 58.39081064771733054 ) ) ;
#36115 = DIRECTION ( 'NONE',  ( 0.000000000000000000, 0.9876883405951383255, -0.1564344650402276216 ) ) ;
#36116 = CARTESIAN_POINT ( 'NONE',  ( -92.69370383062498320, -211.3315407142195852, 76.09614583420048461 ) ) ;
#36117 = FACE_OUTER_BOUND ( 'NONE', #26695, .T. ) ;
#36118 = ORIENTED_EDGE ( 'NONE', *, *, #64101, .T. ) ;
#36119 = DIRECTION ( 'NONE',  ( -0.000000000000000000, -0.6691306063588570163, 0.7431448254773953543 ) ) ;
#36120 = DIRECTION ( 'NONE',  ( -0.000000000000000000, 0.9781476007338069101, -0.2079116908177532363 ) ) ;
#36121 = LINE ( 'NONE', #41763, #18574 ) ;
#36122 = AXIS2_PLACEMENT_3D ( 'NONE', #37509, #61551, #31478 ) ;
#36123 = CIRCLE ( 'NONE', #27759, 31.99999999999998934 ) ;
#36124 = VECTOR ( 'NONE', #41553, 1000.000000000000000 ) ;
#36125 = DIRECTION ( 'NONE',  ( -0.000000000000000000, -0.000000000000000000, 1.000000000000000000 ) ) ;
#36126 = ORIENTED_EDGE ( 'NONE', *, *, #11058, .F. ) ;
#36127 = FACE_OUTER_BOUND ( 'NONE', #27070, .T. ) ;
#36128 = LINE ( 'NONE', #53790, #9159 ) ;
#36129 = ORIENTED_EDGE ( 'NONE', *, *, #52531, .F. ) ;
#36130 = CARTESIAN_POINT ( 'NONE',  ( 95.00000000000000000, -212.6630814284392557, 85.99156250086714692 ) ) ;
#36131 = CARTESIAN_POINT ( 'NONE',  ( 95.00000000000000000, -212.6630814284392557, 88.05531250086714579 ) ) ;
#36132 = ORIENTED_EDGE ( 'NONE', *, *, #24464, .T. ) ;
#36133 = EDGE_CURVE ( 'NONE', #28466, #64719, #11072, .T. ) ;
#36134 = CARTESIAN_POINT ( 'NONE',  ( 96.15314808468750130, -211.9973110713294489, 89.37822916753381719 ) ) ;
#36135 = AXIS2_PLACEMENT_3D ( 'NONE', #16883, #23627, #36747 ) ;
#36136 = ORIENTED_EDGE ( 'NONE', *, *, #73582, .F. ) ;
#36137 = FACE_BOUND ( 'NONE', #34591, .T. ) ;
#36138 = ORIENTED_EDGE ( 'NONE', *, *, #15200, .F. ) ;
#36139 = VECTOR ( 'NONE', #16021, 1000.000000000000000 ) ;
#36140 = CARTESIAN_POINT ( 'NONE',  ( -95.00000000000002842, 87.33691857156074434, 81.07031250086716057 ) ) ;
#36141 = AXIS2_PLACEMENT_3D ( 'NONE', #58188, #12322, #58553 ) ;
#36142 = ORIENTED_EDGE ( 'NONE', *, *, #50846, .F. ) ;
#36143 = EDGE_CURVE ( 'NONE', #36383, #8621, #38914, .T. ) ;
#36144 = ORIENTED_EDGE ( 'NONE', *, *, #22838, .F. ) ;
#36145 = DIRECTION ( 'NONE',  ( -1.000000000000000000, -0.000000000000000000, 0.000000000000000000 ) ) ;
#36146 = CIRCLE ( 'NONE', #43367, 82.00000000000000000 ) ;
#36147 = ORIENTED_EDGE ( 'NONE', *, *, #30901, .F. ) ;
#36148 = FACE_OUTER_BOUND ( 'NONE', #41425, .T. ) ;
#36149 = CARTESIAN_POINT ( 'NONE',  ( 10.00000000000000000, 26.08949754953062694, -27.05870788708203989 ) ) ;
#36150 = EDGE_CURVE ( 'NONE', #69052, #71472, #3868, .T. ) ;
#36151 = ORIENTED_EDGE ( 'NONE', *, *, #5936, .F. ) ;
#36152 = DIRECTION ( 'NONE',  ( 1.000000000000000000, 0.000000000000000000, 0.000000000000000000 ) ) ;
#36153 = ORIENTED_EDGE ( 'NONE', *, *, #14094, .F. ) ;
#36154 = CARTESIAN_POINT ( 'NONE',  ( 0.000000000000000000, 0.000000000000000000, -6.000000000000000000 ) ) ;
#36155 = EDGE_CURVE ( 'NONE', #43311, #49534, #17810, .T. ) ;
#36156 = ORIENTED_EDGE ( 'NONE', *, *, #61280, .T. ) ;
#36157 = EDGE_LOOP ( 'NONE', ( #6390, #58057, #13490, #17966 ) ) ;
#36158 = ORIENTED_EDGE ( 'NONE', *, *, #45785, .T. ) ;
#36159 = CARTESIAN_POINT ( 'NONE',  ( 92.69370383062501162, -211.3315407142195852, 77.63072916753380071 ) ) ;
#36160 = DIRECTION ( 'NONE',  ( -1.000000000000000000, -0.000000000000000000, 0.000000000000000000 ) ) ;
#36161 = DIRECTION ( 'NONE',  ( -1.000000000000000000, 0.000000000000000000, -0.000000000000000000 ) ) ;
#36162 = PLANE ( 'NONE',  #72470 ) ;
#36163 = DIRECTION ( 'NONE',  ( -1.000000000000000000, 0.000000000000000000, 0.000000000000000000 ) ) ;
#36164 = DIRECTION ( 'NONE',  ( 0.000000000000000000, 0.1564344650402311743, -0.9876883405951377704 ) ) ;
#36165 = DIRECTION ( 'NONE',  ( -1.000000000000000000, -0.000000000000000000, -0.000000000000000000 ) ) ;
#36166 = FACE_OUTER_BOUND ( 'NONE', #24277, .T. ) ;
#36167 = CARTESIAN_POINT ( 'NONE',  ( -93.84685191531247028, -211.9973110713294489, 82.86947916753379673 ) ) ;
#36168 = EDGE_CURVE ( 'NONE', #68917, #36728, #2424, .T. ) ;
#36169 = CARTESIAN_POINT ( 'NONE',  ( -92.69370383062504004, 90.00000000000004263, 83.13406250086715943 ) ) ;
#36170 = EDGE_CURVE ( 'NONE', #19829, #63637, #41045, .T. ) ;
#36171 = EDGE_LOOP ( 'NONE', ( #50367, #57975, #19447, #74063 ) ) ;
#36172 = CARTESIAN_POINT ( 'NONE',  ( 92.69370383062498320, 91.33154071421968467, 80.06489583420047040 ) ) ;
#36173 = ORIENTED_EDGE ( 'NONE', *, *, #49468, .T. ) ;
#36174 = DIRECTION ( 'NONE',  ( -0.8541291221503275466, 0.5200609990132993854, 0.000000000000000000 ) ) ;
#36175 = LINE ( 'NONE', #19253, #58789 ) ;
#36176 = CARTESIAN_POINT ( 'NONE',  ( -96.32499999999996021, -212.2949673200287179, 83.20020833506764291 ) ) ;
#36177 = DIRECTION ( 'NONE',  ( -1.000000000000000000, 0.000000000000000000, -0.000000000000000000 ) ) ;
#36178 = DIRECTION ( 'NONE',  ( 0.000000000000000000, 0.3090169943749480619, -0.9510565162951533091 ) ) ;
#36179 = CARTESIAN_POINT ( 'NONE',  ( -93.84685191531247028, -211.9973110713294489, 81.59947916753381492 ) ) ;
#36180 = MECHANICAL_DESIGN_GEOMETRIC_PRESENTATION_REPRESENTATION (  '', ( #32576 ), #42256 ) ;
#36181 = AXIS2_PLACEMENT_3D ( 'NONE', #52734, #47104, #17411 ) ;
#36182 = LINE ( 'NONE', #59128, #45884 ) ;
#36183 = DIRECTION ( 'NONE',  ( -1.000000000000000000, 0.000000000000000000, 0.000000000000000000 ) ) ;
#36184 = VECTOR ( 'NONE', #46934, 1000.000000000000000 ) ;
#36185 = LINE ( 'NONE', #29065, #46845 ) ;
#36186 = ORIENTED_EDGE ( 'NONE', *, *, #18105, .T. ) ;
#36187 = EDGE_CURVE ( 'NONE', #23304, #47528, #23829, .T. ) ;
#36188 = EDGE_CURVE ( 'NONE', #25161, #30315, #35836, .T. ) ;
#36189 = CIRCLE ( 'NONE', #3789, 15.99999999999999822 ) ;
#36190 = ORIENTED_EDGE ( 'NONE', *, *, #6161, .F. ) ;
#36191 = CARTESIAN_POINT ( 'NONE',  ( -92.35000000000005116, 88.93104485797731229, 75.04052853044679239 ) ) ;
#36192 = DIRECTION ( 'NONE',  ( 1.000000000000000000, 0.000000000000000000, 0.000000000000000000 ) ) ;
#36193 = AXIS2_PLACEMENT_3D ( 'NONE', #996, #51717, #30256 ) ;
#36194 = CARTESIAN_POINT ( 'NONE',  ( -97.30629616937501680, 90.00000000000004263, 87.73781250086713612 ) ) ;
#36195 = CARTESIAN_POINT ( 'NONE',  ( 5.999999999999999112, 60.67117009219134616, 55.16347631943062879 ) ) ;
#36196 = DIRECTION ( 'NONE',  ( -0.000000000000000000, -0.000000000000000000, -1.000000000000000000 ) ) ;
#36197 = CARTESIAN_POINT ( 'NONE',  ( 10.00000000000000000, -36.88895765772628010, -6.736453364083947015 ) ) ;
#36198 = CARTESIAN_POINT ( 'NONE',  ( 10.00000000000000000, 2.946379043146343246, 75.11764819372150725 ) ) ;
#36199 = VERTEX_POINT ( 'NONE', #46770 ) ;
#36200 = CARTESIAN_POINT ( 'NONE',  ( 0.000000000000000000, -77.32052557432845674, 5.256550761632577284 ) ) ;
#36201 = AXIS2_PLACEMENT_3D ( 'NONE', #5420, #38499, #61438 ) ;
#36202 = DIRECTION ( 'NONE',  ( -1.000000000000000000, 0.000000000000000000, 0.000000000000000000 ) ) ;
#36203 = AXIS2_PLACEMENT_3D ( 'NONE', #25441, #3279, #20158 ) ;
#36204 = CARTESIAN_POINT ( 'NONE',  ( 5.000000000000002665, -81.96053171279903893, 2.543863470248101333 ) ) ;
#36205 = CARTESIAN_POINT ( 'NONE',  ( 11.99999999999999822, -73.44644590900043113, -24.73286445877782924 ) ) ;
#36206 = CARTESIAN_POINT ( 'NONE',  ( -92.69370383062498320, -211.3315407142195852, 86.25614583420048120 ) ) ;
#36207 = AXIS2_PLACEMENT_3D ( 'NONE', #58128, #17904, #23189 ) ;
#36208 = CYLINDRICAL_SURFACE ( 'NONE', #56957, 42.00000000000000000 ) ;
#36209 = CARTESIAN_POINT ( 'NONE',  ( -10.00000000000000000, 0.000000000000000000, 0.000000000000000000 ) ) ;
#36210 = ADVANCED_FACE ( 'NONE', ( #52775 ), #35109, .T. ) ;
#36211 = CARTESIAN_POINT ( 'NONE',  ( -97.30629616937497417, -211.3315407142195852, 77.78947916753381264 ) ) ;
#36212 = CARTESIAN_POINT ( 'NONE',  ( 92.34999999999988063, 91.52997821335246442, 88.67708333333332860 ) ) ;
#36213 = ORIENTED_EDGE ( 'NONE', *, *, #24208, .T. ) ;
#36214 = DIRECTION ( 'NONE',  ( 0.000000000000000000, -0.9945218953682741780, 0.1045284632676447972 ) ) ;
#36215 = CARTESIAN_POINT ( 'NONE',  ( 93.67499999999998295, 92.29496732002878900, 75.92416666666666458 ) ) ;
#36216 = CARTESIAN_POINT ( 'NONE',  ( 10.00000000000000000, -33.17418723428294669, -17.67226234102862747 ) ) ;
#36217 = EDGE_CURVE ( 'NONE', #36312, #39711, #62699, .T. ) ;
#36218 = DIRECTION ( 'NONE',  ( -1.000000000000000000, 0.000000000000000000, 0.000000000000000000 ) ) ;
#36219 = CARTESIAN_POINT ( 'NONE',  ( 96.15314808468748708, -208.0026889286704943, 76.09614583420047040 ) ) ;
#36220 = EDGE_LOOP ( 'NONE', ( #64832, #51868, #10262, #29232 ) ) ;
#36221 = EDGE_CURVE ( 'NONE', #7371, #57888, #33840, .T. ) ;
#36222 = DIRECTION ( 'NONE',  ( 0.000000000000000000, 0.3090169943749480064, -0.9510565162951534202 ) ) ;
#36223 = ORIENTED_EDGE ( 'NONE', *, *, #50937, .T. ) ;
#36224 = EDGE_CURVE ( 'NONE', #14549, #44827, #30242, .T. ) ;
#36225 = CARTESIAN_POINT ( 'NONE',  ( 0.000000000000000000, 0.000000000000000000, 0.000000000000000000 ) ) ;
#36226 = ORIENTED_EDGE ( 'NONE', *, *, #71626, .F. ) ;
#36227 = EDGE_CURVE ( 'NONE', #41513, #44013, #13450, .T. ) ;
#36228 = CIRCLE ( 'NONE', #14653, 16.00000000000000000 ) ;
#36229 = FACE_OUTER_BOUND ( 'NONE', #33522, .T. ) ;
#36230 = AXIS2_PLACEMENT_3D ( 'NONE', #54874, #2681, #24826 ) ;
#36231 = ORIENTED_EDGE ( 'NONE', *, *, #69124, .T. ) ;
#36232 = EDGE_LOOP ( 'NONE', ( #23879, #8364, #23954, #65009 ) ) ;
#36233 = ORIENTED_EDGE ( 'NONE', *, *, #9151, .F. ) ;
#36234 = CARTESIAN_POINT ( 'NONE',  ( 93.67500000000001137, -207.7050326799711968, 76.63854166840096127 ) ) ;
#36235 = AXIS2_PLACEMENT_3D ( 'NONE', #4878, #3755, #38694 ) ;
#36236 = ORIENTED_EDGE ( 'NONE', *, *, #56990, .T. ) ;
#36237 = CIRCLE ( 'NONE', #18271, 42.00000000000000000 ) ;
#36238 = ORIENTED_EDGE ( 'NONE', *, *, #55174, .F. ) ;
#36239 = CARTESIAN_POINT ( 'NONE',  ( 92.69370383062498320, 90.00000000000002842, 79.64156250086715261 ) ) ;
#36240 = FACE_OUTER_BOUND ( 'NONE', #33284, .T. ) ;
#36241 = EDGE_CURVE ( 'NONE', #60133, #7308, #2657, .T. ) ;
#36242 = CARTESIAN_POINT ( 'NONE',  ( 93.67500000000001137, -212.2949673200287179, 76.13583333333333769 ) ) ;
#36243 = EDGE_LOOP ( 'NONE', ( #69673, #54921, #687, #38370 ) ) ;
#36244 = ORIENTED_EDGE ( 'NONE', *, *, #2181, .F. ) ;
#36245 = ORIENTED_EDGE ( 'NONE', *, *, #47381, .F. ) ;
#36246 = DIRECTION ( 'NONE',  ( 0.000000000000000000, 0.000000000000000000, 1.000000000000000000 ) ) ;
#36247 = CIRCLE ( 'NONE', #65085, 77.49900000000002365 ) ;
#36248 = ORIENTED_EDGE ( 'NONE', *, *, #25484, .T. ) ;
#36249 = CIRCLE ( 'NONE', #35087, 12.49999999999999822 ) ;
#36250 = DIRECTION ( 'NONE',  ( 0.7533909544171997208, 0.6575728627325956310, 9.860761315262647568E-31 ) ) ;
#36251 = DIRECTION ( 'NONE',  ( -1.000000000000000000, 0.000000000000000000, 0.000000000000000000 ) ) ;
#36252 = DIRECTION ( 'NONE',  ( 0.000000000000000000, -0.8660254037844432595, 0.4999999999999919509 ) ) ;
#36253 = DIRECTION ( 'NONE',  ( 0.000000000000000000, -0.8910065241883627918, -0.4539904997395567965 ) ) ;
#36254 = AXIS2_PLACEMENT_3D ( 'NONE', #53140, #41130, #58039 ) ;
#36255 = CARTESIAN_POINT ( 'NONE',  ( 10.00000000000000000, 27.13269053701132094, -25.88420570971372570 ) ) ;
#36256 = LINE ( 'NONE', #37387, #53982 ) ;
#36257 = FACE_BOUND ( 'NONE', #22943, .T. ) ;
#36258 = CARTESIAN_POINT ( 'NONE',  ( -96.32499999999996021, -212.2949673200287179, 78.12020833506763040 ) ) ;
#36259 = ADVANCED_FACE ( 'NONE', ( #12903 ), #59154, .T. ) ;
#36260 = CARTESIAN_POINT ( 'NONE',  ( -92.34999999999999432, -209.9999999999999716, 90.00000000000000000 ) ) ;
#36261 = EDGE_CURVE ( 'NONE', #10620, #68386, #66276, .T. ) ;
#36263 = CARTESIAN_POINT ( 'NONE',  ( -95.00000000000002842, 93.05995642670501411, 75.31562500173430408 ) ) ;
#36262 = CARTESIAN_POINT ( 'NONE',  ( 96.32499999999998863, 87.70503267997126784, 77.59104166840097605 ) ) ;
#36264 =( BOUNDED_CURVE ( )  B_SPLINE_CURVE ( 2, ( #42836, #37573, #26268, #1915, #19155, #42106, #2282, #22506, #32651 ),
 .UNSPECIFIED., .F., .F. ) 
 B_SPLINE_CURVE_WITH_KNOTS ( ( 3, 2, 2, 2, 3 ),
 ( 0.9313609857393204683, 0.9313610513964742932, 0.9384168169373562352, 0.9454725824782379551, 0.9525283480321510288 ),
 .UNSPECIFIED. ) 
 CURVE ( )  GEOMETRIC_REPRESENTATION_ITEM ( )  RATIONAL_B_SPLINE_CURVE ( ( 0.9999975066323365525, 0.9999987533045672228, 1.000000000000000000, 0.8660254037844387076, 1.000000000000000000, 0.8660254037844387076, 1.000000000000000000, 0.8660254037844387076, 1.000000000000000000 ) ) 
 REPRESENTATION_ITEM ( '' )  );
#36266 = EDGE_CURVE ( 'NONE', #68149, #7348, #18911, .T. ) ;
#36265 = ORIENTED_EDGE ( 'NONE', *, *, #65438, .F. ) ;
#36267 = CARTESIAN_POINT ( 'NONE',  ( 92.69370383062498320, 91.33154071421968467, 76.41364583420049428 ) ) ;
#36268 = CARTESIAN_POINT ( 'NONE',  ( 94.99999999999998579, 93.05995642670504253, 82.22124999999999773 ) ) ;
#36269 = CARTESIAN_POINT ( 'NONE',  ( 0.000000000000000000, 21.40280677340371795, 36.13751322684426270 ) ) ;
#36270 = CARTESIAN_POINT ( 'NONE',  ( 10.00000000000000000, 46.53671651293948486, 59.03961581697416250 ) ) ;
#36271 = LINE ( 'NONE', #8449, #19437 ) ;
#36272 = FACE_OUTER_BOUND ( 'NONE', #43274, .T. ) ;
#36273 = ORIENTED_EDGE ( 'NONE', *, *, #2942, .T. ) ;
#36274 = CARTESIAN_POINT ( 'NONE',  ( 10.00000000000000000, 37.01155633439068282, -6.555932627142014191 ) ) ;
#36275 = CARTESIAN_POINT ( 'NONE',  ( 10.00000000000000000, -17.80606268964516659, -33.00180498840066434 ) ) ;
#36276 = VERTEX_POINT ( 'NONE', #53510 ) ;
#36277 = ORIENTED_EDGE ( 'NONE', *, *, #60127, .T. ) ;
#36278 = CARTESIAN_POINT ( 'NONE',  ( 0.000000000000000000, -23.16143007188480496, 73.95703589263965227 ) ) ;
#36279 = CARTESIAN_POINT ( 'NONE',  ( -97.65000000000001990, 91.52997821335253548, 86.21645833506764234 ) ) ;
#36280 = CARTESIAN_POINT ( 'NONE',  ( 9.984461079971730157, -95.40710393340120277, 5.500000000000000000 ) ) ;
#36281 = CARTESIAN_POINT ( 'NONE',  ( 10.00000000000000000, -41.91543099594819921, 2.663952781846001816 ) ) ;
#36282 = CARTESIAN_POINT ( 'NONE',  ( -96.15314808468745866, -211.9973110713294489, 79.11239583420048405 ) ) ;
#36283 = ORIENTED_EDGE ( 'NONE', *, *, #60682, .F. ) ;
#36284 = AXIS2_PLACEMENT_3D ( 'NONE', #31371, #54684, #59591 ) ;
#36285 = DIRECTION ( 'NONE',  ( 0.000000000000000000, -0.8526401643540970632, 0.5224985647159409163 ) ) ;
#36286 = DIRECTION ( 'NONE',  ( -1.000000000000000000, -0.000000000000000000, 0.000000000000000000 ) ) ;
#36287 = AXIS2_PLACEMENT_3D ( 'NONE', #46206, #23635, #12344 ) ;
#36288 = DIRECTION ( 'NONE',  ( -0.000000000000000000, -0.000000000000000000, -1.000000000000000000 ) ) ;
#36289 = DIRECTION ( 'NONE',  ( -1.000000000000000000, 0.000000000000000000, 0.000000000000000000 ) ) ;
#36290 = CARTESIAN_POINT ( 'NONE',  ( 0.000000000000000000, 0.000000000000000000, -6.000000000000000000 ) ) ;
#36291 = CARTESIAN_POINT ( 'NONE',  ( 94.99999999999998579, 90.00000000000002842, 90.00000000000000000 ) ) ;
#36292 = DIRECTION ( 'NONE',  ( 0.000000000000000000, -0.8526401643540970632, 0.5224985647159411384 ) ) ;
#36293 = FACE_OUTER_BOUND ( 'NONE', #35569, .T. ) ;
#36294 = CARTESIAN_POINT ( 'NONE',  ( -20.30386590532152979, -102.9045904027214959, -5.500000000000000000 ) ) ;
#36296 = ADVANCED_FACE ( 'NONE', ( #2045 ), #8013, .T. ) ;
#36295 = AXIS2_PLACEMENT_3D ( 'NONE', #39439, #41929, #62385 ) ;
#36297 = VECTOR ( 'NONE', #63471, 1000.000000000000000 ) ;
#36298 = CARTESIAN_POINT ( 'NONE',  ( 92.69370383062498320, 88.66845928578035796, 82.23447916753383424 ) ) ;
#36299 = CARTESIAN_POINT ( 'NONE',  ( -92.69370383062498320, -208.6684592857803295, 85.09197916753380753 ) ) ;
#36300 = DIRECTION ( 'NONE',  ( -1.000000000000000000, 0.000000000000000000, -0.000000000000000000 ) ) ;
#36301 = VERTEX_POINT ( 'NONE', #66642 ) ;
#36302 = CARTESIAN_POINT ( 'NONE',  ( 0.000000000000000000, 0.000000000000000000, 0.000000000000000000 ) ) ;
#36303 = CARTESIAN_POINT ( 'NONE',  ( -97.64999999999994884, -211.5299782133524502, 79.89291666666666458 ) ) ;
#36304 = CARTESIAN_POINT ( 'NONE',  ( -95.00000000000002842, 87.33691857156074434, 77.73656250086713726 ) ) ;
#36305 = VECTOR ( 'NONE', #4079, 1000.000000000000000 ) ;
#36306 = AXIS2_PLACEMENT_3D ( 'NONE', #56462, #32020, #33128 ) ;
#36307 = EDGE_CURVE ( 'NONE', #51749, #7392, #44079, .T. ) ;
#36308 = CARTESIAN_POINT ( 'NONE',  ( 96.15314808468750130, -211.9973110713294489, 86.04447916753380809 ) ) ;
#36309 = ORIENTED_EDGE ( 'NONE', *, *, #70849, .F. ) ;
#36310 = EDGE_CURVE ( 'NONE', #63369, #73482, #49697, .T. ) ;
#36311 = ORIENTED_EDGE ( 'NONE', *, *, #53646, .F. ) ;
#36312 = VERTEX_POINT ( 'NONE', #27133 ) ;
#36313 = EDGE_CURVE ( 'NONE', #14968, #42545, #61537, .T. ) ;
#36314 = EDGE_CURVE ( 'NONE', #2654, #43742, #37709, .T. ) ;
#36315 = DIRECTION ( 'NONE',  ( 0.000000000000000000, 0.7071067811865437980, 0.7071067811865513475 ) ) ;
#36316 = CARTESIAN_POINT ( 'NONE',  ( 10.00000000000000000, -28.89263327155797967, 71.91182617369179297 ) ) ;
#36317 = VERTEX_POINT ( 'NONE', #20765 ) ;
#36318 = ORIENTED_EDGE ( 'NONE', *, *, #20646, .F. ) ;
#36319 = DIRECTION ( 'NONE',  ( -1.000000000000000000, -0.000000000000000000, -0.000000000000000000 ) ) ;
#36320 = CARTESIAN_POINT ( 'NONE',  ( 96.15314808468750130, -211.9973110713294489, 82.39322916753381776 ) ) ;
#36321 = CARTESIAN_POINT ( 'NONE',  ( 5.000000000000002665, 71.87247863392471459, -39.47590169984770370 ) ) ;
#36322 = CARTESIAN_POINT ( 'NONE',  ( 10.00000000000000000, -24.73286445877757345, 73.44644590900053061 ) ) ;
#36323 = CARTESIAN_POINT ( 'NONE',  ( 10.00000000000000000, 75.11725578898467859, 2.956366410620910656 ) ) ;
#36324 = DIRECTION ( 'NONE',  ( -1.000000000000000000, -0.000000000000000000, -0.000000000000000000 ) ) ;
#36325 = ADVANCED_FACE ( 'NONE', ( #9118 ), #54618, .T. ) ;
#36326 = DIRECTION ( 'NONE',  ( -1.000000000000000000, -0.000000000000000000, -0.000000000000000000 ) ) ;
#36327 = CARTESIAN_POINT ( 'NONE',  ( 92.35000000000002274, -208.4700217866474645, 83.59708333333334451 ) ) ;
#36328 = VERTEX_POINT ( 'NONE', #9860 ) ;
#36329 = ORIENTED_EDGE ( 'NONE', *, *, #46491, .T. ) ;
#36330 = ORIENTED_EDGE ( 'NONE', *, *, #30769, .F. ) ;
#36331 = VERTEX_POINT ( 'NONE', #60641 ) ;
#36332 = CARTESIAN_POINT ( 'NONE',  ( 95.00000000000000000, -213.0599564267049857, 86.98374999999998636 ) ) ;
#36333 = CIRCLE ( 'NONE', #50722, 3.299999999999983391 ) ;
#36334 = CARTESIAN_POINT ( 'NONE',  ( -97.30629616937501680, 91.33154071421968467, 85.30364583420048064 ) ) ;
#36335 = DIRECTION ( 'NONE',  ( 0.000000000000000000, 0.4539904997395479702, -0.8910065241883673437 ) ) ;
#36336 = FACE_OUTER_BOUND ( 'NONE', #56956, .T. ) ;
#36337 = CARTESIAN_POINT ( 'NONE',  ( 92.69370383062501162, -209.9999999999999716, 87.10281250086714522 ) ) ;
#36338 = CARTESIAN_POINT ( 'NONE',  ( 11.99999999999999822, 74.74816331893477184, -33.71516098798660011 ) ) ;
#36339 = ORIENTED_EDGE ( 'NONE', *, *, #28248, .T. ) ;
#36340 = CARTESIAN_POINT ( 'NONE',  ( -10.00000000000000000, 0.000000000000000000, 0.000000000000000000 ) ) ;
#36342 = VERTEX_POINT ( 'NONE', #66996 ) ;
#36341 = ADVANCED_FACE ( 'NONE', ( #3505 ), #26409, .F. ) ;
#36343 = EDGE_CURVE ( 'NONE', #40406, #55116, #42603, .T. ) ;
#36344 = FACE_OUTER_BOUND ( 'NONE', #27183, .T. ) ;
#36345 = EDGE_CURVE ( 'NONE', #46234, #305, #57376, .T. ) ;
#36346 = ORIENTED_EDGE ( 'NONE', *, *, #49798, .T. ) ;
#36347 = CARTESIAN_POINT ( 'NONE',  ( -93.67500000000003979, 92.29496732002878900, 86.05770833506763040 ) ) ;
#36348 = CIRCLE ( 'NONE', #73576, 31.99999999999999289 ) ;
#36349 = CARTESIAN_POINT ( 'NONE',  ( 92.69370383062498320, 91.33154071421968467, 87.84364583420048689 ) ) ;
#36350 = CARTESIAN_POINT ( 'NONE',  ( -15.44521549751111422, -137.7748507232956001, 5.500000000000000000 ) ) ;
#36351 = CYLINDRICAL_SURFACE ( 'NONE', #20585, 31.99999999999998579 ) ;
#36352 = CARTESIAN_POINT ( 'NONE',  ( -12.50000000000000000, -107.5000000000000000, 2.500000000000000000 ) ) ;
#36353 = CARTESIAN_POINT ( 'NONE',  ( -92.74366017909925120, 90.55049048501740572, 74.79348190356847681 ) ) ;
#36354 = EDGE_LOOP ( 'NONE', ( #18605, #37487, #74245, #2197 ) ) ;
#36355 = CARTESIAN_POINT ( 'NONE',  ( -21.33958957442910886, -129.9559990355020034, 5.500000000000000000 ) ) ;
#36356 = VECTOR ( 'NONE', #2495, 1000.000000000000000 ) ;
#36357 = AXIS2_PLACEMENT_3D ( 'NONE', #6354, #46564, #28153 ) ;
#36358 = CARTESIAN_POINT ( 'NONE',  ( -96.15314808468745866, -211.9973110713294489, 75.77864583420047495 ) ) ;
#36359 = ORIENTED_EDGE ( 'NONE', *, *, #11640, .T. ) ;
#36360 = ORIENTED_EDGE ( 'NONE', *, *, #64755, .T. ) ;
#36361 = CARTESIAN_POINT ( 'NONE',  ( 11.99999999999999822, 59.46389618802034960, -49.70050353004825894 ) ) ;
#36362 = DIRECTION ( 'NONE',  ( -1.000000000000000000, 1.047380211910311281E-14, 2.618450529775778123E-14 ) ) ;
#36363 = LINE ( 'NONE', #59304, #10083 ) ;
#36364 = CARTESIAN_POINT ( 'NONE',  ( -93.84685191531247028, -211.9973110713294489, 86.20322916753382003 ) ) ;
#36365 = ORIENTED_EDGE ( 'NONE', *, *, #58164, .F. ) ;
#36366 = ORIENTED_EDGE ( 'NONE', *, *, #11228, .F. ) ;
#36367 = ORIENTED_EDGE ( 'NONE', *, *, #10881, .T. ) ;
#36368 = CARTESIAN_POINT ( 'NONE',  ( 92.35000000000000853, -209.9999999999999716, 90.00000000000000000 ) ) ;
#36369 = CARTESIAN_POINT ( 'NONE',  ( 93.84685191531248449, 91.99731107132950569, 89.06072916753382174 ) ) ;
#36370 = CARTESIAN_POINT ( 'NONE',  ( 1.560000000000000053, -1.299038105676658450, 0.7500000000000007772 ) ) ;
#36371 = CARTESIAN_POINT ( 'NONE',  ( 96.15314808468748708, 88.00268892867053694, 80.96447916753380980 ) ) ;
#36372 = DIRECTION ( 'NONE',  ( 0.000000000000000000, -0.2334453638558922628, -0.9723699203976798877 ) ) ;
#36373 = DIRECTION ( 'NONE',  ( 1.000000000000000000, 1.427937372958405461E-15, 7.962523111839130290E-16 ) ) ;
#36374 = LINE ( 'NONE', #70953, #2484 ) ;
#36375 = CARTESIAN_POINT ( 'NONE',  ( 20.07203437053270179, -132.2214334768125354, 2.500000000000000000 ) ) ;
#36376 = LINE ( 'NONE', #13454, #58471 ) ;
#36377 = LINE ( 'NONE', #59324, #46598 ) ;
#36378 = DIRECTION ( 'NONE',  ( -1.000000000000000000, 0.000000000000000000, 0.000000000000000000 ) ) ;
#36379 = EDGE_CURVE ( 'NONE', #52599, #26527, #74213, .T. ) ;
#36380 = EDGE_CURVE ( 'NONE', #12010, #975, #51393, .T. ) ;
#36381 = PRODUCT_DEFINITION_FORMATION_WITH_SPECIFIED_SOURCE ( 'ANY', '', #14543, .NOT_KNOWN. ) ;
#36382 = DIRECTION ( 'NONE',  ( -1.000000000000000000, -0.000000000000000000, 0.000000000000000000 ) ) ;
#36383 = VERTEX_POINT ( 'NONE', #43359 ) ;
#36384 = CARTESIAN_POINT ( 'NONE',  ( -93.84685191531254134, 91.99731107132950569, 87.52614583420047722 ) ) ;
#36385 = CARTESIAN_POINT ( 'NONE',  ( 20.85212586905262100, -130.9402397935870965, 5.500000000000000000 ) ) ;
#36386 = ADVANCED_FACE ( 'NONE', ( #60990 ), #15124, .F. ) ;
#36387 = VECTOR ( 'NONE', #70236, 1000.000000000000000 ) ;
#36388 = EDGE_CURVE ( 'NONE', #62438, #57306, #41794, .T. ) ;
#36389 = CARTESIAN_POINT ( 'NONE',  ( 6.000000000000000000, 81.34940948281351325, -10.30890764327295450 ) ) ;
#36390 = VERTEX_POINT ( 'NONE', #9487 ) ;
#36391 = CARTESIAN_POINT ( 'NONE',  ( 92.34999999999993747, -208.4700217866475214, 83.59708333333334451 ) ) ;
#36393 = LINE ( 'NONE', #64611, #9596 ) ;
#36392 = AXIS2_PLACEMENT_3D ( 'NONE', #46661, #56840, #68863 ) ;
#36394 = CARTESIAN_POINT ( 'NONE',  ( 24.95699195200416654, -110.9640411295978595, 5.500000000000000000 ) ) ;
#36395 = CIRCLE ( 'NONE', #4023, 37.49900000000000233 ) ;
#36396 = ADVANCED_FACE ( 'NONE', ( #32410 ), #3874, .F. ) ;
#36397 = CARTESIAN_POINT ( 'NONE',  ( 11.99999999999999822, 74.18225833017937987, -34.94270380257559339 ) ) ;
#36398 = VECTOR ( 'NONE', #47303, 1000.000000000000000 ) ;
#36399 = AXIS2_PLACEMENT_3D ( 'NONE', #2129, #64885, #53589 ) ;
#36400 = CARTESIAN_POINT ( 'NONE',  ( 96.15314808468748708, -208.0026889286704943, 82.60489583420049087 ) ) ;
#36401 = VERTEX_POINT ( 'NONE', #36955 ) ;
#36402 = ORIENTED_EDGE ( 'NONE', *, *, #14155, .T. ) ;
#36403 = CARTESIAN_POINT ( 'NONE',  ( 0.000000000000000000, 34.94270380257741948, -74.18225833017852722 ) ) ;
#36404 = ORIENTED_EDGE ( 'NONE', *, *, #40467, .T. ) ;
#36405 = EDGE_CURVE ( 'NONE', #52162, #7502, #59904, .T. ) ;
#36406 = CARTESIAN_POINT ( 'NONE',  ( -12.49999999999999645, 0.000000000000000000, 125.0000000000000000 ) ) ;
#36407 = DIRECTION ( 'NONE',  ( 0.000000000000000000, 0.000000000000000000, 1.000000000000000000 ) ) ;
#36409 = ORIENTED_EDGE ( 'NONE', *, *, #35127, .T. ) ;
#36408 = EDGE_CURVE ( 'NONE', #34723, #17107, #28586, .T. ) ;
#36410 = CARTESIAN_POINT ( 'NONE',  ( 97.30629616937498838, -208.6684592857803011, 80.01197916753380923 ) ) ;
#36411 = ORIENTED_EDGE ( 'NONE', *, *, #69944, .F. ) ;
#36412 = CARTESIAN_POINT ( 'NONE',  ( 0.000000000000000000, -29.01471420065506379, -76.69515212746047439 ) ) ;
#36413 = EDGE_LOOP ( 'NONE', ( #56106, #59097, #13478 ) ) ;
#36414 = EDGE_CURVE ( 'NONE', #39032, #57906, #22258, .T. ) ;
#36415 = ORIENTED_EDGE ( 'NONE', *, *, #47878, .T. ) ;
#36416 = CARTESIAN_POINT ( 'NONE',  ( 10.00000000000000000, -21.40280677340398441, 36.13751322684410638 ) ) ;
#36417 = SURFACE_STYLE_FILL_AREA ( #7119 ) ;
#36418 = CARTESIAN_POINT ( 'NONE',  ( 0.000000000000000000, -4.992566952385247170, 37.16516213103275845 ) ) ;
#36419 = ORIENTED_EDGE ( 'NONE', *, *, #8646, .F. ) ;
#36420 = DIRECTION ( 'NONE',  ( -0.000000000000000000, -0.000000000000000000, 1.000000000000000000 ) ) ;
#36421 = CARTESIAN_POINT ( 'NONE',  ( 92.35000000000002274, -211.5299782133524502, 85.05229166840096866 ) ) ;
#36422 = CARTESIAN_POINT ( 'NONE',  ( 93.67499999999999716, 87.70503267997126784, 85.02583333333332405 ) ) ;
#36423 = VERTEX_POINT ( 'NONE', #51568 ) ;
#36424 = CARTESIAN_POINT ( 'NONE',  ( 0.000000000000000000, -55.16347631943085617, 60.67117009219118273 ) ) ;
#36425 = EDGE_CURVE ( 'NONE', #50699, #36763, #23012, .T. ) ;
#36426 = CARTESIAN_POINT ( 'NONE',  ( -92.35000000000005116, 88.47002178664754979, 75.10395833506764518 ) ) ;
#36427 = APPLICATION_CONTEXT ( 'automotive_design' ) ;
#36428 = CIRCLE ( 'NONE', #30411, 77.49899999999999523 ) ;
#36429 = VERTEX_POINT ( 'NONE', #68871 ) ;
#36430 = VERTEX_POINT ( 'NONE', #50813 ) ;
#36431 = CARTESIAN_POINT ( 'NONE',  ( -97.30629616937501680, 90.00000000000004263, 88.53156250086716739 ) ) ;
#36432 = CARTESIAN_POINT ( 'NONE',  ( 92.69370383062498320, 91.33154071421968467, 83.87489583420047268 ) ) ;
#36433 = ORIENTED_EDGE ( 'NONE', *, *, #62141, .F. ) ;
#36434 = CARTESIAN_POINT ( 'NONE',  ( 97.64999999999997726, 91.52997821335252127, 86.00479166840096923 ) ) ;
#36435 = EDGE_CURVE ( 'NONE', #44373, #28756, #45580, .T. ) ;
#36436 = PRODUCT_DEFINITION_FORMATION_WITH_SPECIFIED_SOURCE ( 'ANY', '', #66792, .NOT_KNOWN. ) ;
#36437 = VERTEX_POINT ( 'NONE', #39932 ) ;
#36438 = LINE ( 'NONE', #25901, #30850 ) ;
#36439 = ORIENTED_EDGE ( 'NONE', *, *, #47187, .F. ) ;
#36440 = AXIS2_PLACEMENT_3D ( 'NONE', #27252, #66755, #5105 ) ;
#36441 = ORIENTED_EDGE ( 'NONE', *, *, #55756, .T. ) ;
#36442 = ORIENTED_EDGE ( 'NONE', *, *, #44379, .T. ) ;
#36443 = CARTESIAN_POINT ( 'NONE',  ( 0.000000000000000000, 65.58780272294076497, 36.73666225445916211 ) ) ;
#36444 = CARTESIAN_POINT ( 'NONE',  ( 3.000000000000000000, 2.935248768560057897, -3.252606517456513302E-15 ) ) ;
#36445 = CARTESIAN_POINT ( 'NONE',  ( -97.65000000000001990, 90.00000000000004263, 85.55499999999999261 ) ) ;
#36446 = ORIENTED_EDGE ( 'NONE', *, *, #45611, .T. ) ;
#36447 = DIRECTION ( 'NONE',  ( -0.000000000000000000, -0.000000000000000000, 1.000000000000000000 ) ) ;
#36448 = AXIS2_PLACEMENT_3D ( 'NONE', #43293, #15813, #3808 ) ;
#36449 = DIRECTION ( 'NONE',  ( 0.000000000000000000, 0.000000000000000000, 1.000000000000000000 ) ) ;
#36450 = ORIENTED_EDGE ( 'NONE', *, *, #4522, .T. ) ;
#36451 = DIRECTION ( 'NONE',  ( -1.000000000000000000, -0.000000000000000000, -0.000000000000000000 ) ) ;
#36452 = CARTESIAN_POINT ( 'NONE',  ( -92.69370383062498320, -211.3315407142195852, 82.28739583420048120 ) ) ;
#36453 = ORIENTED_EDGE ( 'NONE', *, *, #66376, .F. ) ;
#36454 = CIRCLE ( 'NONE', #14830, 31.99999999999998579 ) ;
#36455 = DIRECTION ( 'NONE',  ( 0.000000000000000000, 0.000000000000000000, 1.000000000000000000 ) ) ;
#36456 = DIRECTION ( 'NONE',  ( 0.000000000000000000, 0.000000000000000000, 1.000000000000000000 ) ) ;
#36457 = FACE_BOUND ( 'NONE', #55181, .T. ) ;
#36458 = PLANE ( 'NONE',  #39853 ) ;
#36459 = DIRECTION ( 'NONE',  ( 0.000000000000000000, 0.000000000000000000, 1.000000000000000000 ) ) ;
#36460 = AXIS2_PLACEMENT_3D ( 'NONE', #42769, #54785, #65703 ) ;
#36461 = VECTOR ( 'NONE', #28812, 1000.000000000000000 ) ;
#36462 = DIRECTION ( 'NONE',  ( 0.000000000000000000, 0.000000000000000000, 1.000000000000000000 ) ) ;
#36463 = DIRECTION ( 'NONE',  ( -1.000000000000000000, 0.000000000000000000, 0.000000000000000000 ) ) ;
#36464 = CARTESIAN_POINT ( 'NONE',  ( 0.000000000000000000, -39.47590169984898267, 71.87247863392400404 ) ) ;
#36465 = CYLINDRICAL_SURFACE ( 'NONE', #6843, 37.49900000000000233 ) ;
#36466 = CARTESIAN_POINT ( 'NONE',  ( -92.69370383062502583, 88.66845928578038638, 89.43114583420049257 ) ) ;
#36467 = CYLINDRICAL_SURFACE ( 'NONE', #67099, 42.00000000000000000 ) ;
#36468 = CARTESIAN_POINT ( 'NONE',  ( 12.00000000000000000, 9.615535125379096826, 24.73947219025905042 ) ) ;
#36469 = LINE ( 'NONE', #52659, #55795 ) ;
#36470 = AXIS2_PLACEMENT_3D ( 'NONE', #10844, #57085, #16480 ) ;
#36471 = EDGE_CURVE ( 'NONE', #2787, #29107, #46577, .T. ) ;
#36472 = DIRECTION ( 'NONE',  ( 0.000000000000000000, 0.9510565162951503115, 0.3090169943749573878 ) ) ;
#36473 = CARTESIAN_POINT ( 'NONE',  ( 10.00000000000000000, 0.000000000000000000, 0.000000000000000000 ) ) ;
#36474 = CARTESIAN_POINT ( 'NONE',  ( 95.04693102382854875, 87.35041560265749183, 75.00000002508419072 ) ) ;
#36475 = EDGE_CURVE ( 'NONE', #5289, #60548, #34270, .T. ) ;
#36476 = DIRECTION ( 'NONE',  ( 0.000000000000000000, 0.8910065241883655673, 0.4539904997395510233 ) ) ;
#36477 = DIRECTION ( 'NONE',  ( -1.000000000000000000, -0.000000000000000000, 0.000000000000000000 ) ) ;
#36478 = CARTESIAN_POINT ( 'NONE',  ( -96.32499999999996021, -207.7050326799711968, 87.35416666666665719 ) ) ;
#36479 = ADVANCED_FACE ( 'NONE', ( #56847 ), #56483, .F. ) ;
#36480 = DIRECTION ( 'NONE',  ( 0.000000000000000000, 0.000000000000000000, 1.000000000000000000 ) ) ;
#36481 = AXIS2_PLACEMENT_3D ( 'NONE', #8333, #19967, #42922 ) ;
#36482 =( BOUNDED_CURVE ( )  B_SPLINE_CURVE ( 2, ( #405, #57879, #64999, #23297, #12367, #63527, #6381 ),
 .UNSPECIFIED., .F., .F. ) 
 B_SPLINE_CURVE_WITH_KNOTS ( ( 3, 2, 2, 3 ),
 ( 0.2499999999999995837, 0.2569444444444442532, 0.2638888888888890061, 0.2708333333333337034 ),
 .UNSPECIFIED. ) 
 CURVE ( )  GEOMETRIC_REPRESENTATION_ITEM ( )  RATIONAL_B_SPLINE_CURVE ( ( 1.000000000000007994, 0.8660254037844307140, 1.000000000000000000, 0.8660254037844387076, 1.000000000000000000, 0.8660254037844311581, 1.000000000000007550 ) ) 
 REPRESENTATION_ITEM ( '' )  );
#36483 = ORIENTED_EDGE ( 'NONE', *, *, #51725, .F. ) ;
#36484 = DIRECTION ( 'NONE',  ( 0.3311129884571280546, 0.9435911131814402886, 0.000000000000000000 ) ) ;
#36485 = DIRECTION ( 'NONE',  ( -1.000000000000000000, -0.000000000000000000, 0.000000000000000000 ) ) ;
#36486 = CARTESIAN_POINT ( 'NONE',  ( -97.65000000000001990, 90.00000000000004263, 84.92000000000000171 ) ) ;
#36487 = AXIS2_PLACEMENT_3D ( 'NONE', #73307, #11278, #56787 ) ;
#36488 = EDGE_CURVE ( 'NONE', #3181, #42920, #67372, .T. ) ;
#36489 = ORIENTED_EDGE ( 'NONE', *, *, #30270, .T. ) ;
#36490 = DIRECTION ( 'NONE',  ( 1.000000000000000000, -0.000000000000000000, -0.000000000000000000 ) ) ;
#36491 = CARTESIAN_POINT ( 'NONE',  ( 11.99999999999999822, -14.66109333815513160, 73.73191006444567108 ) ) ;
#36492 = ORIENTED_EDGE ( 'NONE', *, *, #20394, .F. ) ;
#36493 = AXIS2_PLACEMENT_3D ( 'NONE', #60122, #55570, #2988 ) ;
#36494 = CARTESIAN_POINT ( 'NONE',  ( 95.00000000000000000, -207.3369185715606307, 83.76906250086715033 ) ) ;
#36495 = CARTESIAN_POINT ( 'NONE',  ( 97.30629616937498838, -211.3315407142195852, 88.79614583420048746 ) ) ;
#36496 = AXIS2_PLACEMENT_3D ( 'NONE', #9211, #43076, #43454 ) ;
#36497 = VERTEX_POINT ( 'NONE', #27519 ) ;
#36498 = CARTESIAN_POINT ( 'NONE',  ( 10.00000000000000000, 26.79245525562761188, -32.34446384429941901 ) ) ;
#36499 = VERTEX_POINT ( 'NONE', #4986 ) ;
#36500 = AXIS2_PLACEMENT_3D ( 'NONE', #73831, #38894, #3959 ) ;
#36501 = LINE ( 'NONE', #59451, #16687 ) ;
#36502 = ORIENTED_EDGE ( 'NONE', *, *, #56477, .F. ) ;
#36503 = ADVANCED_FACE ( 'NONE', ( #63235 ), #45200, .T. ) ;
#36505 = EDGE_CURVE ( 'NONE', #64448, #32364, #53767, .T. ) ;
#36504 = AXIS2_PLACEMENT_3D ( 'NONE', #53407, #8278, #47756 ) ;
#36506 = CARTESIAN_POINT ( 'NONE',  ( -93.84685191531254134, 91.99731107132950569, 81.96989583420048575 ) ) ;
#36507 = ORIENTED_EDGE ( 'NONE', *, *, #10535, .F. ) ;
#36508 = EDGE_LOOP ( 'NONE', ( #48216, #73253, #59273, #65565 ) ) ;
#36509 = DIRECTION ( 'NONE',  ( -1.000000000000000000, 0.000000000000000000, 0.000000000000000000 ) ) ;
#36510 = ORIENTED_EDGE ( 'NONE', *, *, #68708, .F. ) ;
#36511 = CYLINDRICAL_SURFACE ( 'NONE', #26880, 82.00000000000000000 ) ;
#36512 = DIRECTION ( 'NONE',  ( -0.000000000000000000, -0.000000000000000000, -1.000000000000000000 ) ) ;
#36513 = ORIENTED_EDGE ( 'NONE', *, *, #5644, .F. ) ;
#36514 = CARTESIAN_POINT ( 'NONE',  ( 10.00000000000000000, 68.55367621811204515, -44.99326035065983120 ) ) ;
#36515 = EDGE_CURVE ( 'NONE', #34204, #28208, #5356, .T. ) ;
#36516 = AXIS2_PLACEMENT_3D ( 'NONE', #30257, #26467, #37764 ) ;
#36517 = ORIENTED_EDGE ( 'NONE', *, *, #7656, .T. ) ;
#36518 = CARTESIAN_POINT ( 'NONE',  ( -10.00000000000000000, 0.000000000000000000, 0.000000000000000000 ) ) ;
#36519 = EDGE_LOOP ( 'NONE', ( #46637, #16760 ) ) ;
#36520 = VECTOR ( 'NONE', #57259, 1000.000000000000000 ) ;
#36521 = ORIENTED_EDGE ( 'NONE', *, *, #54498, .T. ) ;
#36522 = ORIENTED_EDGE ( 'NONE', *, *, #18491, .T. ) ;
#36523 = CARTESIAN_POINT ( 'NONE',  ( 93.84685191531251292, -211.9973110713294489, 77.04864583420047097 ) ) ;
#36524 = FACE_OUTER_BOUND ( 'NONE', #45228, .T. ) ;
#36525 = CARTESIAN_POINT ( 'NONE',  ( -96.32499999999996021, -212.2949673200287179, 85.74020833506763495 ) ) ;
#36526 = EDGE_LOOP ( 'NONE', ( #9817, #62566, #39022, #45418 ) ) ;
#36527 = CARTESIAN_POINT ( 'NONE',  ( 0.000000000000000000, 6.736453364083555329, 36.88895765772635116 ) ) ;
#36528 = DIRECTION ( 'NONE',  ( -1.000000000000000000, 0.000000000000000000, -0.000000000000000000 ) ) ;
#36529 = DIRECTION ( 'NONE',  ( 0.000000000000000000, 0.000000000000000000, -1.000000000000000000 ) ) ;
#36530 = CARTESIAN_POINT ( 'NONE',  ( -92.35000000005462084, -210.0000170173125014, 88.49187441316038871 ) ) ;
#36531 = CARTESIAN_POINT ( 'NONE',  ( 1.560000000000000053, 0.8660254037844389297, -1.500000000000000000 ) ) ;
#36532 = CARTESIAN_POINT ( 'NONE',  ( -93.84685191531248449, -208.0026889286704943, 81.17614583420048291 ) ) ;
#36533 = CARTESIAN_POINT ( 'NONE',  ( -97.30629616937501680, 91.33154071421968467, 77.68364583420047609 ) ) ;
#36534 = ORIENTED_EDGE ( 'NONE', *, *, #56268, .T. ) ;
#36535 = VECTOR ( 'NONE', #22422, 1000.000000000000000 ) ;
#36536 = CARTESIAN_POINT ( 'NONE',  ( 97.30629616937498838, 91.33154071421968467, 81.75822916753381264 ) ) ;
#36537 = ORIENTED_EDGE ( 'NONE', *, *, #6539, .T. ) ;
#36538 = CARTESIAN_POINT ( 'NONE',  ( -8.826826895187510402, -94.96827758698185562, 5.500000000000000000 ) ) ;
#36539 = DIRECTION ( 'NONE',  ( -1.000000000000000000, -0.000000000000000000, -0.000000000000000000 ) ) ;
#36540 = CARTESIAN_POINT ( 'NONE',  ( 15.00000000000000000, -22.32062822937489344, -14.36278369418800160 ) ) ;
#36541 = CARTESIAN_POINT ( 'NONE',  ( 0.000000000000000000, -37.58145647212455032, 0.6853352020789044152 ) ) ;
#36542 = DIRECTION ( 'NONE',  ( -1.000000000000000000, -0.000000000000000000, -0.000000000000000000 ) ) ;
#36543 = CARTESIAN_POINT ( 'NONE',  ( -97.30629616937497417, -211.3315407142195852, 83.98072916753380923 ) ) ;
#36544 = DIRECTION ( 'NONE',  ( 0.000000000000000000, 0.000000000000000000, 1.000000000000000000 ) ) ;
#36545 = DIRECTION ( 'NONE',  ( -1.000000000000000000, -0.000000000000000000, -0.000000000000000000 ) ) ;
#36546 = CARTESIAN_POINT ( 'NONE',  ( 10.00000000000000000, -33.80338159004273280, -16.23288003029533044 ) ) ;
#36547 = EDGE_LOOP ( 'NONE', ( #40173, #52002, #32619, #71331 ) ) ;
#36548 = AXIS2_PLACEMENT_3D ( 'NONE', #52241, #53350, #64276 ) ;
#36549 = ORIENTED_EDGE ( 'NONE', *, *, #64082, .T. ) ;
#36550 = DIRECTION ( 'NONE',  ( 0.000000000000000000, 0.5877852522924741363, -0.8090169943749465631 ) ) ;
#36551 = CARTESIAN_POINT ( 'NONE',  ( -97.65000000000001990, 91.52997821335253548, 75.34208333333333485 ) ) ;
#36552 = CARTESIAN_POINT ( 'NONE',  ( 0.000000000000000000, 0.000000000000000000, 0.000000000000000000 ) ) ;
#36553 = CARTESIAN_POINT ( 'NONE',  ( -92.69370383062504004, 90.00000000000004263, 84.24531250086714351 ) ) ;
#36554 = DIRECTION ( 'NONE',  ( -1.000000000000000000, 0.000000000000000000, -0.000000000000000000 ) ) ;
#36555 = DIRECTION ( 'NONE',  ( 0.000000000000000000, 0.000000000000000000, 1.000000000000000000 ) ) ;
#36556 = DIRECTION ( 'NONE',  ( 0.08130631524010120681, -0.9966891607226784355, 0.000000000000000000 ) ) ;
#36557 = AXIS2_PLACEMENT_3D ( 'NONE', #6308, #29211, #64550 ) ;
#36558 = CARTESIAN_POINT ( 'NONE',  ( -8.000000000000007105, -1.142349898368590025E-14, -6.370018489464426943E-15 ) ) ;
#36559 = AXIS2_PLACEMENT_3D ( 'NONE', #59157, #42605, #60281 ) ;
#36560 = VERTEX_POINT ( 'NONE', #57218 ) ;
#36561 = CIRCLE ( 'NONE', #57027, 82.00000000000000000 ) ;
#36562 = CARTESIAN_POINT ( 'NONE',  ( -93.84685191531254134, 91.99731107132950569, 76.09614583420047040 ) ) ;
#36563 = EDGE_CURVE ( 'NONE', #15251, #53901, #54991, .T. ) ;
#36564 = VECTOR ( 'NONE', #56946, 1000.000000000000000 ) ;
#36565 = DIRECTION ( 'NONE',  ( -1.000000000000000000, -0.000000000000000000, 0.000000000000000000 ) ) ;
#36566 = DIRECTION ( 'NONE',  ( -1.000000000000000000, 0.000000000000000000, 0.000000000000000000 ) ) ;
#36567 = EDGE_CURVE ( 'NONE', #31031, #4841, #34642, .T. ) ;
#36568 = CARTESIAN_POINT ( 'NONE',  ( 10.00000000000000000, -70.52718814184277107, 26.02418014898285037 ) ) ;
#36569 = CARTESIAN_POINT ( 'NONE',  ( 0.000000000000000000, 0.6853352020790449695, 37.58145647212454321 ) ) ;
#36570 = CARTESIAN_POINT ( 'NONE',  ( -93.84685191531248449, -208.0026889286704943, 84.50989583420049200 ) ) ;
#36571 = VECTOR ( 'NONE', #66266, 1000.000000000000114 ) ;
#36572 = EDGE_CURVE ( 'NONE', #31367, #71534, #52578, .T. ) ;
#36573 = CARTESIAN_POINT ( 'NONE',  ( 10.00000000000000000, 0.000000000000000000, 0.000000000000000000 ) ) ;
#36574 = AXIS2_PLACEMENT_3D ( 'NONE', #771, #46590, #2244 ) ;
#36575 = EDGE_CURVE ( 'NONE', #58103, #18206, #44167, .T. ) ;
#36576 = CARTESIAN_POINT ( 'NONE',  ( 0.000000000000000000, -50.23322058963299241, -64.81221759200397514 ) ) ;
#36577 = AXIS2_PLACEMENT_3D ( 'NONE', #8151, #48013, #70926 ) ;
#36578 = CARTESIAN_POINT ( 'NONE',  ( -96.15314808468745866, -211.9973110713294489, 77.84239583420048803 ) ) ;
#36579 = CARTESIAN_POINT ( 'NONE',  ( 97.65000000000004832, 91.52997821335247863, 88.46541666666664128 ) ) ;
#36580 = ORIENTED_EDGE ( 'NONE', *, *, #27466, .F. ) ;
#36581 = CARTESIAN_POINT ( 'NONE',  ( 99.99999999999998579, 95.00000000000002842, 90.00000000000000000 ) ) ;
#36582 = DIRECTION ( 'NONE',  ( 0.000000000000000000, -8.881784197001252323E-16, 1.000000000000000000 ) ) ;
#36583 = DIRECTION ( 'NONE',  ( 0.000000000000000000, 0.000000000000000000, 1.000000000000000000 ) ) ;
#36584 = EDGE_CURVE ( 'NONE', #15045, #26436, #66958, .T. ) ;
#36585 = CARTESIAN_POINT ( 'NONE',  ( 10.00000000000000000, 14.67089635893819377, -73.72996012237423713 ) ) ;
#36587 = ADVANCED_FACE ( 'NONE', ( #4615 ), #51189, .T. ) ;
#36586 = CARTESIAN_POINT ( 'NONE',  ( 97.30629616937498838, -208.6684592857803011, 89.53697916753382913 ) ) ;
#36588 = EDGE_LOOP ( 'NONE', ( #32178, #43312, #53371, #23030 ) ) ;
#36589 = EDGE_CURVE ( 'NONE', #46178, #16205, #24839, .T. ) ;
#36590 = DIRECTION ( 'NONE',  ( 0.000000000000000000, 0.8660254037844374864, -0.5000000000000019984 ) ) ;
#36591 = PLANE ( 'NONE',  #23962 ) ;
#36592 = DIRECTION ( 'NONE',  ( 0.02332147558787671729, 0.9997280174009349762, -0.000000000000000000 ) ) ;
#36593 = VERTEX_POINT ( 'NONE', #59068 ) ;
#36594 = DIRECTION ( 'NONE',  ( -1.000000000000000000, -0.000000000000000000, -0.000000000000000000 ) ) ;
#36595 = ORIENTED_EDGE ( 'NONE', *, *, #72194, .F. ) ;
#36596 = CYLINDRICAL_SURFACE ( 'NONE', #8189, 37.49900000000000233 ) ;
#36597 = EDGE_CURVE ( 'NONE', #43117, #52875, #3399, .T. ) ;
#36598 = EDGE_CURVE ( 'NONE', #67030, #8551, #8146, .T. ) ;
#36599 = CIRCLE ( 'NONE', #70227, 37.49900000000000233 ) ;
#36600 = ORIENTED_EDGE ( 'NONE', *, *, #56644, .F. ) ;
#36601 = VERTEX_POINT ( 'NONE', #1590 ) ;
#36602 = ORIENTED_EDGE ( 'NONE', *, *, #22094, .T. ) ;
#36603 = CARTESIAN_POINT ( 'NONE',  ( 96.32499999999998863, -207.7050326799711968, 76.53270833506762472 ) ) ;
#36604 = ORIENTED_EDGE ( 'NONE', *, *, #41951, .F. ) ;
#36605 = ORIENTED_EDGE ( 'NONE', *, *, #68281, .F. ) ;
#36606 = CARTESIAN_POINT ( 'NONE',  ( 96.15314808468748708, 91.99731107132950569, 80.06489583420048461 ) ) ;
#36607 = AXIS2_PLACEMENT_3D ( 'NONE', #27049, #26319, #62416 ) ;
#36608 = CYLINDRICAL_SURFACE ( 'NONE', #58806, 2.649999999999985700 ) ;
#36609 = B_SPLINE_CURVE_WITH_KNOTS ( 'NONE', 3,
 ( #9765, #38717, #44739, #20302, #37613, #15028 ),
 .UNSPECIFIED., .F., .F.,
 ( 4, 2, 4 ),
 ( 0.7528176110416704425, 0.8153862273022827178, 0.8779548435628951042 ),
 .UNSPECIFIED. ) ;
#36611 = CARTESIAN_POINT ( 'NONE',  ( 0.000000000000000000, 76.69515212746016175, 29.01471420065590578 ) ) ;
#36610 = VECTOR ( 'NONE', #1909, 1000.000000000000000 ) ;
#36612 = VERTEX_POINT ( 'NONE', #41043 ) ;
#36613 = VERTEX_POINT ( 'NONE', #64705 ) ;
#36614 = ORIENTED_EDGE ( 'NONE', *, *, #6372, .T. ) ;
#36615 = FACE_OUTER_BOUND ( 'NONE', #3790, .T. ) ;
#36616 = ORIENTED_EDGE ( 'NONE', *, *, #59873, .F. ) ;
#36617 = AXIS2_PLACEMENT_3D ( 'NONE', #18554, #13284, #53514 ) ;
#36618 = CARTESIAN_POINT ( 'NONE',  ( -13.49999999999997691, 73.00000000000001421, -255.0000000000000000 ) ) ;
#36619 = CARTESIAN_POINT ( 'NONE',  ( -10.00000000000000000, 0.000000000000000000, 0.000000000000000000 ) ) ;
#36620 = CARTESIAN_POINT ( 'NONE',  ( 10.00000000000000000, 0.000000000000000000, 0.000000000000000000 ) ) ;
#36621 = FACE_OUTER_BOUND ( 'NONE', #54387, .T. ) ;
#36622 = CARTESIAN_POINT ( 'NONE',  ( 0.000000000000000000, 0.000000000000000000, -5.974599999999999689 ) ) ;
#36623 = VECTOR ( 'NONE', #68393, 1000.000000000000000 ) ;
#36624 = CARTESIAN_POINT ( 'NONE',  ( -95.00000000000002842, 86.94004357329504273, 78.09374999999998579 ) ) ;
#36625 = DIRECTION ( 'NONE',  ( 1.000000000000000000, -0.000000000000000000, -0.000000000000000000 ) ) ;
#36626 = CARTESIAN_POINT ( 'NONE',  ( -96.32499999999996021, -207.7050326799711968, 74.73354166840096013 ) ) ;
#36627 = CARTESIAN_POINT ( 'NONE',  ( -96.15314808468751551, 88.00268892867056536, 88.00239583420048461 ) ) ;
#36629 = CARTESIAN_POINT ( 'NONE',  ( -97.65000000000001990, 90.00000000000004263, 76.74437500173429783 ) ) ;
#36628 = CARTESIAN_POINT ( 'NONE',  ( 97.64999999999997726, 91.52997821335252127, 75.84479166840098685 ) ) ;
#36630 = ORIENTED_EDGE ( 'NONE', *, *, #44194, .F. ) ;
#36631 = CARTESIAN_POINT ( 'NONE',  ( 96.15314808468748708, 91.99731107132950569, 78.15989583420049769 ) ) ;
#36632 = CARTESIAN_POINT ( 'NONE',  ( 97.64999999999997726, 91.52997821335253548, 82.11541666666664696 ) ) ;
#36633 = CARTESIAN_POINT ( 'NONE',  ( 10.00000000000000000, -74.65374052328644439, -8.840884882375878107 ) ) ;
#36634 = DIRECTION ( 'NONE',  ( -0.000000000000000000, -0.000000000000000000, 1.000000000000000000 ) ) ;
#36635 = AXIS2_PLACEMENT_3D ( 'NONE', #37484, #3289, #26178 ) ;
#36636 = CYLINDRICAL_SURFACE ( 'NONE', #43519, 16.00000000000000000 ) ;
#36637 = DIRECTION ( 'NONE',  ( -1.000000000000000000, 0.000000000000000000, 0.000000000000000000 ) ) ;
#36638 = EDGE_LOOP ( 'NONE', ( #67737, #54955, #56994, #28944 ) ) ;
#36639 = CYLINDRICAL_SURFACE ( 'NONE', #34927, 1.000000000000000000 ) ;
#36640 = FACE_OUTER_BOUND ( 'NONE', #65849, .T. ) ;
#36641 = ORIENTED_EDGE ( 'NONE', *, *, #33676, .F. ) ;
#36642 = CIRCLE ( 'NONE', #13820, 31.99999999999998224 ) ;
#36643 = ORIENTED_EDGE ( 'NONE', *, *, #9585, .T. ) ;
#36644 = EDGE_CURVE ( 'NONE', #26896, #23517, #20161, .T. ) ;
#36645 = EDGE_CURVE ( 'NONE', #47809, #73223, #71782, .T. ) ;
#36646 = DIRECTION ( 'NONE',  ( 0.000000000000000000, 0.000000000000000000, 1.000000000000000000 ) ) ;
#36647 = CARTESIAN_POINT ( 'NONE',  ( 50.00005079999999680, 0.000000000000000000, 0.000000000000000000 ) ) ;
#36648 = CARTESIAN_POINT ( 'NONE',  ( -3.000000000000000000, -22.67460108101783334, 6.353146135317912169 ) ) ;
#36649 = EDGE_CURVE ( 'NONE', #31828, #73312, #39389, .T. ) ;
#36650 = CYLINDRICAL_SURFACE ( 'NONE', #60370, 12.50000000000000000 ) ;
#36651 = CARTESIAN_POINT ( 'NONE',  ( 10.00000000000000000, -46.53671651293991118, 59.03961581697383565 ) ) ;
#36652 = CARTESIAN_POINT ( 'NONE',  ( -96.15314808468747287, -208.0026889286704943, 75.72572916753382799 ) ) ;
#36653 = MANIFOLD_SOLID_BREP ( 'Cut-Extrude1', #37993 ) ;
#36654 = ORIENTED_EDGE ( 'NONE', *, *, #7083, .F. ) ;
#36655 = EDGE_CURVE ( 'NONE', #32728, #10456, #6813, .T. ) ;
#36656 = LINE ( 'NONE', #54694, #34317 ) ;
#36657 = CIRCLE ( 'NONE', #12661, 42.00000000000000000 ) ;
#36658 = FACE_OUTER_BOUND ( 'NONE', #20888, .T. ) ;
#36659 = ADVANCED_FACE ( 'NONE', ( #70686 ), #69602, .T. ) ;
#36660 = CARTESIAN_POINT ( 'NONE',  ( 10.00000000000000000, 65.64334221924909230, 41.19522573413756561 ) ) ;
#36661 = CARTESIAN_POINT ( 'NONE',  ( 11.99999999999999822, -46.21855187248673502, 62.20884554314003623 ) ) ;
#36662 = FACE_OUTER_BOUND ( 'NONE', #30952, .T. ) ;
#36663 = CARTESIAN_POINT ( 'NONE',  ( -3.000000000000000000, 9.615535125378775305, 24.73947219025917121 ) ) ;
#36664 = DIRECTION ( 'NONE',  ( 0.000000000000000000, 0.000000000000000000, 1.000000000000000000 ) ) ;
#36665 = DIRECTION ( 'NONE',  ( -0.000000000000000000, -0.000000000000000000, 1.000000000000000000 ) ) ;
#36666 = VECTOR ( 'NONE', #18288, 1000.000000000000000 ) ;
#36667 = ADVANCED_FACE ( 'NONE', ( #65083 ), #13555, .F. ) ;
#36668 = VECTOR ( 'NONE', #17501, 1000.000000000000000 ) ;
#36669 = CARTESIAN_POINT ( 'NONE',  ( 96.15314808468748708, 88.00268892867053694, 83.66322916753382799 ) ) ;
#36670 = CARTESIAN_POINT ( 'NONE',  ( -94.99999999999997158, -212.6630814284392557, 86.78531250086713555 ) ) ;
#36671 = CARTESIAN_POINT ( 'NONE',  ( -12.75044424985085634, 0.001194404169697439516, -65.00000000000034106 ) ) ;
#36672 = EDGE_LOOP ( 'NONE', ( #34805, #71340, #9322, #72942 ) ) ;
#36673 = CARTESIAN_POINT ( 'NONE',  ( 10.00000000000000000, -10.96151621346514382, 35.95386929396252640 ) ) ;
#36674 = CARTESIAN_POINT ( 'NONE',  ( -96.32499999999996021, -212.2949673200287179, 79.94583333333332575 ) ) ;
#36675 = CARTESIAN_POINT ( 'NONE',  ( -95.00000000000002842, 87.33691857156074434, 75.19656250086714522 ) ) ;
#36676 = VECTOR ( 'NONE', #15696, 1000.000000000000000 ) ;
#36677 = CIRCLE ( 'NONE', #64332, 16.00000000000000000 ) ;
#36679 = ADVANCED_FACE ( 'NONE', ( #46305 ), #69233, .F. ) ;
#36678 = CARTESIAN_POINT ( 'NONE',  ( 95.00000000000000000, -207.3369185715606307, 84.40406250086712703 ) ) ;
#36680 = VERTEX_POINT ( 'NONE', #12812 ) ;
#36681 = EDGE_CURVE ( 'NONE', #61245, #70917, #4629, .T. ) ;
#36682 = DIRECTION ( 'NONE',  ( 0.000000000000000000, 0.000000000000000000, 1.000000000000000000 ) ) ;
#36683 = ORIENTED_EDGE ( 'NONE', *, *, #48397, .F. ) ;
#36684 = VECTOR ( 'NONE', #15466, 1000.000000000000114 ) ;
#36685 = CIRCLE ( 'NONE', #31851, 31.99999999999998224 ) ;
#36686 = ORIENTED_EDGE ( 'NONE', *, *, #60291, .F. ) ;
#36687 = CARTESIAN_POINT ( 'NONE',  ( -93.67500000000003979, 87.70503267997129626, 79.49604166840096298 ) ) ;
#36688 = DIRECTION ( 'NONE',  ( -1.000000000000000000, -0.000000000000000000, -0.000000000000000000 ) ) ;
#36689 = VECTOR ( 'NONE', #51199, 1000.000000000000000 ) ;
#36690 = ORIENTED_EDGE ( 'NONE', *, *, #2521, .F. ) ;
#36691 = DIRECTION ( 'NONE',  ( 0.000000000000000000, 1.000000000000000000, 3.469446951953614189E-15 ) ) ;
#36692 = CARTESIAN_POINT ( 'NONE',  ( 92.69370383062501162, -211.3315407142195852, 79.05947916753382287 ) ) ;
#36693 = DIRECTION ( 'NONE',  ( -1.000000000000000000, -0.000000000000000000, 0.000000000000000000 ) ) ;
#36694 = DIRECTION ( 'NONE',  ( 1.000000000000000000, -0.000000000000000000, -0.000000000000000000 ) ) ;
#36695 =( BOUNDED_CURVE ( )  B_SPLINE_CURVE ( 2, ( #30331, #29958, #24698, #70174, #52909, #13035, #35974 ),
 .UNSPECIFIED., .F., .F. ) 
 B_SPLINE_CURVE_WITH_KNOTS ( ( 3, 2, 2, 3 ),
 ( 0.6458333333333334814, 0.6527777777777779011, 0.6597222222222223209, 0.6666666666666667407 ),
 .UNSPECIFIED. ) 
 CURVE ( )  GEOMETRIC_REPRESENTATION_ITEM ( )  RATIONAL_B_SPLINE_CURVE ( ( 0.9999999999999978906, 0.8660254037844408170, 1.000000000000000000, 0.8660254037844387076, 1.000000000000000000, 0.8660254037844365982, 1.000000000000002220 ) ) 
 REPRESENTATION_ITEM ( '' )  );
#36696 = DIRECTION ( 'NONE',  ( 0.000000000000000000, 0.000000000000000000, 1.000000000000000000 ) ) ;
#36697 = DIRECTION ( 'NONE',  ( -0.000000000000000000, -0.000000000000000000, 1.000000000000000000 ) ) ;
#36698 = FACE_OUTER_BOUND ( 'NONE', #41602, .T. ) ;
#36699 = CARTESIAN_POINT ( 'NONE',  ( 96.32499999999998863, -207.7050326799711968, 80.26333333333332121 ) ) ;
#36700 = ORIENTED_EDGE ( 'NONE', *, *, #59350, .F. ) ;
#36701 = VERTEX_POINT ( 'NONE', #53054 ) ;
#36702 = ORIENTED_EDGE ( 'NONE', *, *, #17479, .F. ) ;
#36703 = ORIENTED_EDGE ( 'NONE', *, *, #66704, .F. ) ;
#36704 = LINE ( 'NONE', #8130, #21399 ) ;
#36705 = CARTESIAN_POINT ( 'NONE',  ( -97.30629616937501680, 90.00000000000004263, 82.81656250086714977 ) ) ;
#36706 = CARTESIAN_POINT ( 'NONE',  ( 10.00000000000000000, 0.000000000000000000, 0.000000000000000000 ) ) ;
#36707 = CYLINDRICAL_SURFACE ( 'NONE', #15023, 82.00000000000000000 ) ;
#36708 = CARTESIAN_POINT ( 'NONE',  ( 96.32499999999998863, 87.70503267997126784, 76.24166666666666003 ) ) ;
#36709 = EDGE_LOOP ( 'NONE', ( #9171, #2372, #37362, #20314 ) ) ;
#36710 = CARTESIAN_POINT ( 'NONE',  ( 0.000000000000000000, 0.000000000000000000, 20.00000000000000000 ) ) ;
#36711 = EDGE_CURVE ( 'NONE', #12130, #22476, #65454, .T. ) ;
#36712 = ORIENTED_EDGE ( 'NONE', *, *, #31129, .F. ) ;
#36713 = DIRECTION ( 'NONE',  ( 0.000000000000000000, 0.000000000000000000, -1.000000000000000000 ) ) ;
#36714 = VERTEX_POINT ( 'NONE', #2327 ) ;
#36715 = CARTESIAN_POINT ( 'NONE',  ( -92.35000000000005116, 88.47002178664754979, 87.80395833506763381 ) ) ;
#36716 =( BOUNDED_CURVE ( )  B_SPLINE_CURVE ( 2, ( #73642, #51837, #16513, #11597, #56379, #40555, #56755 ),
 .UNSPECIFIED., .F., .F. ) 
 B_SPLINE_CURVE_WITH_KNOTS ( ( 3, 2, 2, 3 ),
 ( 0.7291666666666665186, 0.7361111111111109384, 0.7430555555555553582, 0.7499999999999996669 ),
 .UNSPECIFIED. ) 
 CURVE ( )  GEOMETRIC_REPRESENTATION_ITEM ( )  RATIONAL_B_SPLINE_CURVE ( ( 1.000000000000002220, 0.8660254037844365982, 1.000000000000000000, 0.8660254037844387076, 1.000000000000000000, 0.8660254037844451469, 0.9999999999999935607 ) ) 
 REPRESENTATION_ITEM ( '' )  );
#36717 = CARTESIAN_POINT ( 'NONE',  ( 96.15314808468748708, 91.99731107132950569, 85.14489583420048291 ) ) ;
#36718 = VECTOR ( 'NONE', #7250, 1000.000000000000000 ) ;
#36719 = DIRECTION ( 'NONE',  ( 0.2306669878475637314, 0.9730327541852493711, -0.000000000000000000 ) ) ;
#36720 = DIRECTION ( 'NONE',  ( -0.000000000000000000, -0.000000000000000000, -1.000000000000000000 ) ) ;
#36721 = CARTESIAN_POINT ( 'NONE',  ( 0.000000000000000000, 59.03342792756263435, 46.54456581323825048 ) ) ;
#36722 = CARTESIAN_POINT ( 'NONE',  ( 0.000000000000000000, -20.41045688087876897, 72.35160999960810102 ) ) ;
#36723 = ORIENTED_EDGE ( 'NONE', *, *, #72097, .T. ) ;
#36724 = FACE_OUTER_BOUND ( 'NONE', #68988, .T. ) ;
#36725 = AXIS2_PLACEMENT_3D ( 'NONE', #3184, #37745, #59947 ) ;
#36726 = ORIENTED_EDGE ( 'NONE', *, *, #9402, .T. ) ;
#36727 = CIRCLE ( 'NONE', #55939, 37.49900000000000233 ) ;
#36728 = VERTEX_POINT ( 'NONE', #71062 ) ;
#36729 = EDGE_CURVE ( 'NONE', #49534, #44854, #69219, .T. ) ;
#36731 = CARTESIAN_POINT ( 'NONE',  ( 10.00000000000000000, 0.000000000000000000, 0.000000000000000000 ) ) ;
#36730 = AXIS2_PLACEMENT_3D ( 'NONE', #18985, #48312, #36285 ) ;
#36732 = ADVANCED_FACE ( 'NONE', ( #49251 ), #37030, .T. ) ;
#36733 = PRODUCT_DEFINITION_SHAPE ( 'NONE', 'NONE',  #24681 ) ;
#36734 = DIRECTION ( 'NONE',  ( 2.603472992746261562E-14, 2.546204323184492723E-14, -1.000000000000000000 ) ) ;
#36735 = AXIS2_PLACEMENT_3D ( 'NONE', #916, #24185, #1659 ) ;
#36736 = CIRCLE ( 'NONE', #5585, 37.49900000000000944 ) ;
#36737 = CARTESIAN_POINT ( 'NONE',  ( -95.00000000000002842, 93.05995642670504253, 75.31562500173430408 ) ) ;
#36738 = CARTESIAN_POINT ( 'NONE',  ( -97.30629616937497417, -208.6684592857803011, 84.66864583420047552 ) ) ;
#36739 = ORIENTED_EDGE ( 'NONE', *, *, #31892, .T. ) ;
#36740 = DIRECTION ( 'NONE',  ( 0.000000000000000000, 0.000000000000000000, 1.000000000000000000 ) ) ;
#36741 = ORIENTED_EDGE ( 'NONE', *, *, #29927, .T. ) ;
#36742 = EDGE_CURVE ( 'NONE', #45520, #53848, #25003, .T. ) ;
#36743 = EDGE_CURVE ( 'NONE', #46060, #37710, #36860, .T. ) ;
#36744 = VERTEX_POINT ( 'NONE', #71797 ) ;
#36745 = DIRECTION ( 'NONE',  ( 0.000000000000000000, -0.9510565162951502005, -0.3090169943749581094 ) ) ;
#36746 = DIRECTION ( 'NONE',  ( 0.000000000000000000, 0.9969173337331276308, 0.07845909572784864894 ) ) ;
#36747 = DIRECTION ( 'NONE',  ( 0.000000000000000000, 0.000000000000000000, 1.000000000000000000 ) ) ;
#36748 = CARTESIAN_POINT ( 'NONE',  ( 93.84685191531248449, 88.00268892867053694, 80.22364583420046813 ) ) ;
#36749 = CARTESIAN_POINT ( 'NONE',  ( 0.000000000000000000, 0.000000000000000000, -145.0000000000000000 ) ) ;
#36750 = CARTESIAN_POINT ( 'NONE',  ( -97.64998201403408018, 91.52998859755483352, 80.50145761676020584 ) ) ;
#36751 = CYLINDRICAL_SURFACE ( 'NONE', #31233, 3.299999999999997158 ) ;
#36752 = FACE_OUTER_BOUND ( 'NONE', #74049, .T. ) ;
#36753 = CARTESIAN_POINT ( 'NONE',  ( 21.07894319797337701, -103.8699611390234878, 5.500000000000000000 ) ) ;
#36754 = CARTESIAN_POINT ( 'NONE',  ( 10.00000000000000000, -77.32052557432837148, -5.256550761633697277 ) ) ;
#36755 = ADVANCED_FACE ( 'NONE', ( #48880 ), #22642, .T. ) ;
#36756 = DIRECTION ( 'NONE',  ( -1.000000000000000000, -0.000000000000000000, -0.000000000000000000 ) ) ;
#36757 = DIRECTION ( 'NONE',  ( 0.9135454576426004225, 0.4067366430758009854, 0.000000000000000000 ) ) ;
#36758 = VERTEX_POINT ( 'NONE', #54169 ) ;
#36759 = CARTESIAN_POINT ( 'NONE',  ( -92.69370383062505425, 88.66845928578038638, 87.36739583420047950 ) ) ;
#36760 = DIRECTION ( 'NONE',  ( 0.000000000000000000, 0.6494480483301849905, -0.7604059656000299317 ) ) ;
#36762 = EDGE_CURVE ( 'NONE', #49698, #17551, #15390, .T. ) ;
#36761 = DIRECTION ( 'NONE',  ( 0.000000000000000000, -6.938893903907228378E-15, 1.000000000000000000 ) ) ;
#36763 = VERTEX_POINT ( 'NONE', #25949 ) ;
#36764 = CARTESIAN_POINT ( 'NONE',  ( 0.000000000000000000, -36.88895765772628010, -6.736453364083947015 ) ) ;
#36765 = ADVANCED_FACE ( 'NONE', ( #31954 ), #54891, .T. ) ;
#36766 = MANIFOLD_SOLID_BREP ( 'Thread5', #64417 ) ;
#36767 = CARTESIAN_POINT ( 'NONE',  ( -99.99999999999998579, -124.0000000000000142, -40.00000000000002132 ) ) ;
#36768 = CIRCLE ( 'NONE', #38005, 31.99999999999999289 ) ;
#36769 = CYLINDRICAL_SURFACE ( 'NONE', #50355, 31.99999999999998579 ) ;
#36770 = CARTESIAN_POINT ( 'NONE',  ( 92.69370383062501162, -209.9999999999999716, 82.18156250086715886 ) ) ;
#36771 = AXIS2_PLACEMENT_3D ( 'NONE', #72666, #61041, #67421 ) ;
#36772 = EDGE_LOOP ( 'NONE', ( #69635, #57529, #24064, #12330 ) ) ;
#36773 = AXIS2_PLACEMENT_3D ( 'NONE', #65798, #19911, #20288 ) ;
#36774 = ORIENTED_EDGE ( 'NONE', *, *, #66560, .T. ) ;
#36775 = DIRECTION ( 'NONE',  ( 0.000000000000000000, 0.000000000000000000, 1.000000000000000000 ) ) ;
#36776 = EDGE_LOOP ( 'NONE', ( #21528, #10263, #52116, #8807, #37651, #49073, #57377, #65408 ) ) ;
#36777 = AXIS2_PLACEMENT_3D ( 'NONE', #37319, #8738, #22236 ) ;
#36778 = DIRECTION ( 'NONE',  ( 0.000000000000000000, -0.5877852522924802425, 0.8090169943749422332 ) ) ;
#36779 = CIRCLE ( 'NONE', #51067, 42.00000000000000000 ) ;
#36780 = DIRECTION ( 'NONE',  ( 1.000000000000000000, -5.236901059551556403E-15, -2.618450529775778123E-14 ) ) ;
#36781 = ORIENTED_EDGE ( 'NONE', *, *, #67247, .F. ) ;
#36782 = CYLINDRICAL_SURFACE ( 'NONE', #3336, 77.49899999999999523 ) ;
#36783 = CARTESIAN_POINT ( 'NONE',  ( 95.00000000000000000, -207.3369185715606307, 78.84781250086714977 ) ) ;
#36784 = ORIENTED_EDGE ( 'NONE', *, *, #16442, .F. ) ;
#36785 = CARTESIAN_POINT ( 'NONE',  ( 0.000000000000000000, 0.000000000000000000, 2.500000000000000000 ) ) ;
#36786 = EDGE_LOOP ( 'NONE', ( #58001, #2223, #13209, #19965 ) ) ;
#36787 = VERTEX_POINT ( 'NONE', #65814 ) ;
#36788 = CARTESIAN_POINT ( 'NONE',  ( 0.000000000000000000, 75.16055320797057959, -18.89407956138179046 ) ) ;
#36789 = CIRCLE ( 'NONE', #13983, 42.00000000000000000 ) ;
#36790 = CARTESIAN_POINT ( 'NONE',  ( 95.00000000000000000, -206.9400435732949575, 80.31624999999999659 ) ) ;
#36791 = ORIENTED_EDGE ( 'NONE', *, *, #39108, .T. ) ;
#36792 = CARTESIAN_POINT ( 'NONE',  ( 10.00000000000000000, 10.96151621346540317, -35.95386929396244113 ) ) ;
#36793 = CARTESIAN_POINT ( 'NONE',  ( 93.67500000000001137, -212.2949673200287179, 85.10520833506762983 ) ) ;
#36794 = CARTESIAN_POINT ( 'NONE',  ( 92.34999999999999432, 90.00000000000002842, 83.65000000000000568 ) ) ;
#36795 = ORIENTED_EDGE ( 'NONE', *, *, #2321, .T. ) ;
#36796 = DIRECTION ( 'NONE',  ( 0.000000000000000000, 0.000000000000000000, 1.000000000000000000 ) ) ;
#36797 = CARTESIAN_POINT ( 'NONE',  ( 11.99999999999999822, 76.66974797899852945, -11.30684508768257679 ) ) ;
#36798 = EDGE_LOOP ( 'NONE', ( #42293, #48704, #44686, #65028 ) ) ;
#36799 = VERTEX_POINT ( 'NONE', #19563 ) ;
#36800 = CARTESIAN_POINT ( 'NONE',  ( -97.30629616937501680, 91.33154071421968467, 88.47864583420047779 ) ) ;
#36801 = CARTESIAN_POINT ( 'NONE',  ( 97.30629616937498838, 91.33154071421968467, 81.12322916753382174 ) ) ;
#36802 = ORIENTED_EDGE ( 'NONE', *, *, #7732, .T. ) ;
#36803 = CARTESIAN_POINT ( 'NONE',  ( 94.99999999999998579, 93.05995642670504253, 86.74562500173429669 ) ) ;
#36804 = EDGE_CURVE ( 'NONE', #26168, #3338, #15436, .T. ) ;
#36805 = DIRECTION ( 'NONE',  ( 0.000000000000000000, 0.000000000000000000, 1.000000000000000000 ) ) ;
#36806 = ORIENTED_EDGE ( 'NONE', *, *, #71336, .F. ) ;
#36807 = FACE_OUTER_BOUND ( 'NONE', #66298, .T. ) ;
#36808 = ORIENTED_EDGE ( 'NONE', *, *, #2025, .F. ) ;
#36809 = ORIENTED_EDGE ( 'NONE', *, *, #50689, .T. ) ;
#36810 = ORIENTED_EDGE ( 'NONE', *, *, #13312, .F. ) ;
#36811 = DIRECTION ( 'NONE',  ( 0.000000000000000000, -0.6691306063588672304, 0.7431448254773862505 ) ) ;
#36812 = EDGE_CURVE ( 'NONE', #9094, #13137, #57484, .T. ) ;
#36813 = LINE ( 'NONE', #8630, #4941 ) ;
#36814 = CARTESIAN_POINT ( 'NONE',  ( -97.65000000000001990, 91.52997821335253548, 85.50208333333331723 ) ) ;
#36815 = EDGE_CURVE ( 'NONE', #3022, #38305, #45863, .T. ) ;
#36816 = ORIENTED_EDGE ( 'NONE', *, *, #72291, .F. ) ;
#36817 = CARTESIAN_POINT ( 'NONE',  ( 97.06449789201045064, 91.06393496763742235, 74.79348190356853365 ) ) ;
#36818 = DIRECTION ( 'NONE',  ( 0.000000000000000000, 0.2334453638559058630, -0.9723699203976765570 ) ) ;
#36819 = ORIENTED_EDGE ( 'NONE', *, *, #25985, .F. ) ;
#36820 = DIRECTION ( 'NONE',  ( 0.000000000000000000, -0.4539904997395351471, -0.8910065241883737830 ) ) ;
#36821 = CARTESIAN_POINT ( 'NONE',  ( -93.84685191531247028, -211.9973110713294489, 81.59947916753381492 ) ) ;
#36822 = ORIENTED_EDGE ( 'NONE', *, *, #54428, .F. ) ;
#36823 = LINE ( 'NONE', #1556, #29033 ) ;
#36824 = VECTOR ( 'NONE', #3027, 1000.000000000000114 ) ;
#36825 = LINE ( 'NONE', #24812, #50062 ) ;
#36826 = CARTESIAN_POINT ( 'NONE',  ( 10.00000000000000000, -6.736453364083817341, 36.88895765772630142 ) ) ;
#36827 = DIRECTION ( 'NONE',  ( 0.000000000000000000, 0.000000000000000000, -1.000000000000000000 ) ) ;
#36828 = VECTOR ( 'NONE', #31245, 1000.000000000000000 ) ;
#36829 = EDGE_CURVE ( 'NONE', #2929, #67800, #44222, .T. ) ;
#36830 = CARTESIAN_POINT ( 'NONE',  ( 97.64999999989935020, -209.9999769027737671, 83.41187580057901130 ) ) ;
#36831 = FILL_AREA_STYLE ('',( #8644 ) ) ;
#36832 = CARTESIAN_POINT ( 'NONE',  ( 0.000000000000000000, 75.11764819372149304, -2.946379043146603482 ) ) ;
#36833 = CIRCLE ( 'NONE', #51276, 31.99999999999999645 ) ;
#36834 = CARTESIAN_POINT ( 'NONE',  ( 10.00000000000000000, -21.60688246758641995, 79.10210256391358996 ) ) ;
#36835 = SHAPE_REPRESENTATION ( 'slow gear_ISO - Spur gear 2M 80T 20PA 12FW ---S80A75H50L38.0N', ( #43395 ), #46970 ) ;
#36836 = CARTESIAN_POINT ( 'NONE',  ( 0.000000000000000000, -33.00180498840035170, -17.80606268964575278 ) ) ;
#36837 = LINE ( 'NONE', #42862, #16405 ) ;
#36838 = CARTESIAN_POINT ( 'NONE',  ( -92.69370383062502583, 91.33154071421968467, 74.77322916753379900 ) ) ;
#36839 = CARTESIAN_POINT ( 'NONE',  ( 30.50000000000000000, -120.0000000000000000, 5.500000000000000888 ) ) ;
#36840 = CYLINDRICAL_SURFACE ( 'NONE', #39850, 42.00000000000000000 ) ;
#36841 = AXIS2_PLACEMENT_3D ( 'NONE', #66894, #15386, #38327 ) ;
#36842 = ADVANCED_FACE ( 'NONE', ( #73657 ), #11258, .T. ) ;
#36843 = DIRECTION ( 'NONE',  ( -1.000000000000000000, -0.000000000000000000, -0.000000000000000000 ) ) ;
#36844 = UNCERTAINTY_MEASURE_WITH_UNIT (LENGTH_MEASURE( 1.000000000000000082E-05 ), #18373, 'distance_accuracy_value', 'NONE');
#36845 = ADVANCED_FACE ( 'NONE', ( #68417 ), #28538, .F. ) ;
#36846 = PLANE ( 'NONE',  #24562 ) ;
#36847 = AXIS2_PLACEMENT_3D ( 'NONE', #69146, #754, #22166 ) ;
#36848 = CARTESIAN_POINT ( 'NONE',  ( 11.99999999999999822, 59.03342792756263435, 46.54456581323825048 ) ) ;
#36849 = LINE ( 'NONE', #47757, #64659 ) ;
#36850 = FACE_OUTER_BOUND ( 'NONE', #46994, .T. ) ;
#36851 = DIRECTION ( 'NONE',  ( -0.000000000000000000, -0.000000000000000000, -1.000000000000000000 ) ) ;
#36852 = DIRECTION ( 'NONE',  ( -0.000000000000000000, -0.000000000000000000, 1.000000000000000000 ) ) ;
#36853 = CARTESIAN_POINT ( 'NONE',  ( -92.34999999999999432, -211.5299782133524502, 86.45458333333333201 ) ) ;
#36854 = AXIS2_PLACEMENT_3D ( 'NONE', #24489, #47425, #25591 ) ;
#36855 = CARTESIAN_POINT ( 'NONE',  ( -2.500000000000015543, -73.00000000000001421, -204.9999999999999716 ) ) ;
#36856 = EDGE_CURVE ( 'NONE', #12834, #33300, #57132, .T. ) ;
#36857 = ORIENTED_EDGE ( 'NONE', *, *, #46618, .F. ) ;
#36858 = CYLINDRICAL_SURFACE ( 'NONE', #51563, 16.00000000000000000 ) ;
#36859 = DIRECTION ( 'NONE',  ( 0.000000000000000000, 0.000000000000000000, 1.000000000000000000 ) ) ;
#36860 = LINE ( 'NONE', #15035, #46633 ) ;
#36861 = CARTESIAN_POINT ( 'NONE',  ( -7.499999999999970690, 69.70000000000001705, -204.9999999999999716 ) ) ;
#36862 = ORIENTED_EDGE ( 'NONE', *, *, #8500, .T. ) ;
#36863 = CARTESIAN_POINT ( 'NONE',  ( -92.35000000002557385, 90.00000000000005684, -75.00000000000007105 ) ) ;
#36864 = DIRECTION ( 'NONE',  ( -1.000000000000000000, -0.000000000000000000, -0.000000000000000000 ) ) ;
#36865 = ORIENTED_EDGE ( 'NONE', *, *, #67848, .T. ) ;
#36866 =( REPRESENTATION_RELATIONSHIP ('NONE','NONE', #31117, #36835 ) REPRESENTATION_RELATIONSHIP_WITH_TRANSFORMATION ( #53455 )SHAPE_REPRESENTATION_RELATIONSHIP( ) );
#36867 = CARTESIAN_POINT ( 'NONE',  ( 97.30629616937498838, -211.3315407142195852, 81.65239583420047609 ) ) ;
#36868 = CARTESIAN_POINT ( 'NONE',  ( 92.69370383062501162, -208.6684592857803295, 88.47864583420047779 ) ) ;
#36869 = CIRCLE ( 'NONE', #71697, 31.99999999999999289 ) ;
#36870 = VERTEX_POINT ( 'NONE', #62032 ) ;
#36871 = CARTESIAN_POINT ( 'NONE',  ( 97.30629616937498838, -211.3315407142195852, 88.16114583420048234 ) ) ;
#36872 = AXIS2_PLACEMENT_3D ( 'NONE', #46995, #22964, #16943 ) ;
#36873 = VERTEX_POINT ( 'NONE', #68036 ) ;
#36874 = CARTESIAN_POINT ( 'NONE',  ( 10.00000000000000000, -35.53030884539077050, -12.26510123303296851 ) ) ;
#36875 = ORIENTED_EDGE ( 'NONE', *, *, #33594, .F. ) ;
#36876 = CARTESIAN_POINT ( 'NONE',  ( -97.30629616937501680, 91.33154071421968467, 75.77864583420048916 ) ) ;
#36877 = VERTEX_POINT ( 'NONE', #31 ) ;
#36878 = AXIS2_PLACEMENT_3D ( 'NONE', #15089, #3470, #38031 ) ;
#36879 = ORIENTED_EDGE ( 'NONE', *, *, #60469, .F. ) ;
#36880 = AXIS2_PLACEMENT_3D ( 'NONE', #28337, #73080, #21586 ) ;
#36881 = VERTEX_POINT ( 'NONE', #67664 ) ;
#36882 = CARTESIAN_POINT ( 'NONE',  ( 94.99999999999998579, 93.05995642670504253, 88.01562500173432113 ) ) ;
#36883 = LINE ( 'NONE', #59835, #36828 ) ;
#36884 = ORIENTED_EDGE ( 'NONE', *, *, #18987, .T. ) ;
#36885 = CARTESIAN_POINT ( 'NONE',  ( 12.00000000000000000, -18.13022148937263012, -15.02647892043543898 ) ) ;
#36886 = CIRCLE ( 'NONE', #9254, 12.49999999999999822 ) ;
#36887 = ORIENTED_EDGE ( 'NONE', *, *, #10723, .T. ) ;
#36888 = CARTESIAN_POINT ( 'NONE',  ( 97.64999999999999147, -209.9999999999999716, 86.50750000000000739 ) ) ;
#36889 = MANIFOLD_SOLID_BREP ( 'Hex', #54797 ) ;
#36890 = VERTEX_POINT ( 'NONE', #67289 ) ;
#36891 = EDGE_CURVE ( 'NONE', #35508, #19685, #32223, .T. ) ;
#36892 = ORIENTED_EDGE ( 'NONE', *, *, #6703, .T. ) ;
#36893 = ORIENTED_EDGE ( 'NONE', *, *, #64333, .F. ) ;
#36894 = CARTESIAN_POINT ( 'NONE',  ( 95.00000000000000000, -207.3369185715606307, 77.41906250086714181 ) ) ;
#36895 = CARTESIAN_POINT ( 'NONE',  ( 0.000000000000000000, 27.75498641678742473, 31.52238457039609187 ) ) ;
#36896 = CARTESIAN_POINT ( 'NONE',  ( -97.64999999950698850, -210.0000320324311076, 85.63541623677365067 ) ) ;
#36898 = ADVANCED_FACE ( 'NONE', ( #39093 ), #15786, .F. ) ;
#36897 = ORIENTED_EDGE ( 'NONE', *, *, #29596, .F. ) ;
#36899 = VECTOR ( 'NONE', #21329, 1000.000000000000000 ) ;
#36900 = CARTESIAN_POINT ( 'NONE',  ( -92.35000000053402403, -209.9999467984910382, 78.96687695417375608 ) ) ;
#36901 = ORIENTED_EDGE ( 'NONE', *, *, #46335, .F. ) ;
#36902 = CYLINDRICAL_SURFACE ( 'NONE', #73761, 37.49900000000000233 ) ;
#36903 = EDGE_CURVE ( 'NONE', #44417, #56961, #22928, .T. ) ;
#36904 = CARTESIAN_POINT ( 'NONE',  ( 15.00000000000000000, 14.60985201121729737, 18.46759930825687235 ) ) ;
#36905 = DIRECTION ( 'NONE',  ( 0.000000000000000000, 0.000000000000000000, 1.000000000000000000 ) ) ;
#36906 = ADVANCED_FACE ( 'NONE', ( #32688 ), #73286, .T. ) ;
#36907 = CARTESIAN_POINT ( 'NONE',  ( 13.83832728059186046, -142.6495187161941089, -5.500000000000000000 ) ) ;
#36908 = CARTESIAN_POINT ( 'NONE',  ( -92.69370383062498320, -211.3315407142195852, 82.28739583420048120 ) ) ;
#36909 = AXIS2_PLACEMENT_3D ( 'NONE', #44107, #56515, #21531 ) ;
#36910 = CARTESIAN_POINT ( 'NONE',  ( -97.30629616937501680, 90.00000000000004263, 78.37156250086715659 ) ) ;
#36911 = ORIENTED_EDGE ( 'NONE', *, *, #72531, .F. ) ;
#36912 = CARTESIAN_POINT ( 'NONE',  ( 97.30629616937498838, 91.33154071421968467, 81.12322916753382174 ) ) ;
#36913 = EDGE_CURVE ( 'NONE', #62960, #60376, #9429, .T. ) ;
#36914 = VERTEX_POINT ( 'NONE', #33059 ) ;
#36915 = CARTESIAN_POINT ( 'NONE',  ( 15.00000000000000000, -22.67460108101782978, -6.353146135317906840 ) ) ;
#36916 = FACE_OUTER_BOUND ( 'NONE', #5352, .T. ) ;
#36917 = CARTESIAN_POINT ( 'NONE',  ( -92.34999999999999432, -209.9999999999999716, 76.98250000000000171 ) ) ;
#36918 = DIRECTION ( 'NONE',  ( 0.000000000000000000, 0.000000000000000000, 1.000000000000000000 ) ) ;
#36919 = FACE_OUTER_BOUND ( 'NONE', #20238, .T. ) ;
#36920 = CARTESIAN_POINT ( 'NONE',  ( -92.69370383062498320, -209.9999999999999716, 82.97531250086714749 ) ) ;
#36921 = ADVANCED_FACE ( 'NONE', ( #13742 ), #23288, .T. ) ;
#36922 = CARTESIAN_POINT ( 'NONE',  ( -97.64999999999996305, -209.9999999999999716, 89.36499999999999488 ) ) ;
#36923 = DIRECTION ( 'NONE',  ( -0.08130631524010117905, 0.9966891607226784355, 0.000000000000000000 ) ) ;
#36924 = DIRECTION ( 'NONE',  ( -2.603472992746261562E-14, -2.546204323184492723E-14, 1.000000000000000000 ) ) ;
#36925 = ORIENTED_EDGE ( 'NONE', *, *, #20207, .F. ) ;
#36926 = ORIENTED_EDGE ( 'NONE', *, *, #4169, .F. ) ;
#36927 = DIRECTION ( 'NONE',  ( -1.000000000000000000, 0.000000000000000000, -0.000000000000000000 ) ) ;
#36928 = CARTESIAN_POINT ( 'NONE',  ( -3.000000000000000000, -18.13022148937263012, 15.02647892043544608 ) ) ;
#36929 = CYLINDRICAL_SURFACE ( 'NONE', #58364, 2.649999999999985700 ) ;
#36930 = CARTESIAN_POINT ( 'NONE',  ( -96.15314808468751551, 88.00268892867056536, 85.93864583420048575 ) ) ;
#36931 = DIRECTION ( 'NONE',  ( 0.000000000000000000, 0.000000000000000000, 1.000000000000000000 ) ) ;
#36932 = CARTESIAN_POINT ( 'NONE',  ( 0.000000000000000000, 0.000000000000000000, 0.000000000000000000 ) ) ;
#36933 = CARTESIAN_POINT ( 'NONE',  ( 3.000000000000000000, -1.467624384280027838, 2.542000000000001592 ) ) ;
#36934 =( BOUNDED_CURVE ( )  B_SPLINE_CURVE ( 2, ( #32101, #49023, #55040, #21183, #20081, #71582, #71954 ),
 .UNSPECIFIED., .F., .F. ) 
 B_SPLINE_CURVE_WITH_KNOTS ( ( 3, 2, 2, 3 ),
 ( 0.04166666666666644231, 0.04861111111111085514, 0.05555555555555525410, 0.06249999999999966693 ),
 .UNSPECIFIED. ) 
 CURVE ( )  GEOMETRIC_REPRESENTATION_ITEM ( )  RATIONAL_B_SPLINE_CURVE ( ( 1.000000000000004219, 0.8660254037844343777, 1.000000000000000000, 0.8660254037844387076, 1.000000000000000000, 0.8660254037844451469, 0.9999999999999935607 ) ) 
 REPRESENTATION_ITEM ( '' )  );
#36935 = ORIENTED_EDGE ( 'NONE', *, *, #42435, .T. ) ;
#36936 = ADVANCED_FACE ( 'NONE', ( #14109 ), #46580, .T. ) ;
#36937 = LINE ( 'NONE', #41473, #12814 ) ;
#36938 = EDGE_CURVE ( 'NONE', #72049, #50325, #37059, .T. ) ;
#36939 = AXIS2_PLACEMENT_3D ( 'NONE', #8173, #13447, #52557 ) ;
#36940 = ADVANCED_FACE ( 'NONE', ( #48703 ), #58229, .F. ) ;
#36941 = EDGE_CURVE ( 'NONE', #21073, #74280, #63518, .T. ) ;
#36942 = CARTESIAN_POINT ( 'NONE',  ( -7.469491406282094736, 4.756046723998911929, 52.00000000000002132 ) ) ;
#36943 = DIRECTION ( 'NONE',  ( 0.000000000000000000, 0.000000000000000000, 1.000000000000000000 ) ) ;
#36944 = VECTOR ( 'NONE', #68756, 1000.000000000000000 ) ;
#36945 = CARTESIAN_POINT ( 'NONE',  ( -4.652319770550016109, 3.087484620012986625, -1.687189089856314217 ) ) ;
#36946 = CARTESIAN_POINT ( 'NONE',  ( -97.64999999999996305, -209.9999999999999716, 82.37999999999999545 ) ) ;
#36947 = DIRECTION ( 'NONE',  ( 0.000000000000000000, 1.224646799147347784E-16, 1.000000000000000000 ) ) ;
#36948 = CARTESIAN_POINT ( 'NONE',  ( -94.99999999999997158, -212.6630814284392557, 82.97531250086716170 ) ) ;
#36949 = AXIS2_PLACEMENT_3D ( 'NONE', #33140, #27882, #68111 ) ;
#36950 = FILL_AREA_STYLE_COLOUR ( '', #32618 ) ;
#36951 = CARTESIAN_POINT ( 'NONE',  ( 11.99999999999999822, 15.33399622253600647, -80.55351364060571484 ) ) ;
#36952 = EDGE_CURVE ( 'NONE', #65921, #45237, #48337, .T. ) ;
#36953 = DIRECTION ( 'NONE',  ( 0.000000000000000000, 0.000000000000000000, -1.000000000000000000 ) ) ;
#36954 = CYLINDRICAL_SURFACE ( 'NONE', #40657, 16.00000000000000000 ) ;
#36955 = CARTESIAN_POINT ( 'NONE',  ( 11.99999999999999822, -81.90746397400391743, 3.894527615417590294 ) ) ;
#36956 = ORIENTED_EDGE ( 'NONE', *, *, #4066, .T. ) ;
#36957 = PLANE ( 'NONE',  #55721 ) ;
#36958 = CARTESIAN_POINT ( 'NONE',  ( 12.50000000000000000, 0.000000000000000000, -4.400000000000001243 ) ) ;
#36959 = FACE_OUTER_BOUND ( 'NONE', #36027, .T. ) ;
#36960 = VECTOR ( 'NONE', #2163, 1000.000000000000000 ) ;
#36961 = CIRCLE ( 'NONE', #4565, 15.99999999999999822 ) ;
#36963 = CIRCLE ( 'NONE', #11896, 77.49900000000000944 ) ;
#36962 = DIRECTION ( 'NONE',  ( 0.000000000000000000, 0.000000000000000000, 1.000000000000000000 ) ) ;
#36964 = CARTESIAN_POINT ( 'NONE',  ( 96.15314808468748708, -208.0026889286704943, 88.31989583420048007 ) ) ;
#36965 = ORIENTED_EDGE ( 'NONE', *, *, #23932, .T. ) ;
#36966 = CONICAL_SURFACE ( 'NONE', #3395, 2.541999999999999815, 1.047197551196591858 ) ;
#36967 = CARTESIAN_POINT ( 'NONE',  ( 11.99999999999999822, 6.903761155838878061, -77.19088730480517313 ) ) ;
#36968 = FACE_OUTER_BOUND ( 'NONE', #14342, .T. ) ;
#36969 = ORIENTED_EDGE ( 'NONE', *, *, #67476, .F. ) ;
#36970 = AXIS2_PLACEMENT_3D ( 'NONE', #38061, #55724, #4243 ) ;
#36971 = DIRECTION ( 'NONE',  ( -1.000000000000000000, 0.000000000000000000, 0.000000000000000000 ) ) ;
#36972 = VERTEX_POINT ( 'NONE', #12358 ) ;
#36973 = DIRECTION ( 'NONE',  ( -1.000000000000000000, 0.000000000000000000, 0.000000000000000000 ) ) ;
#36974 = ORIENTED_EDGE ( 'NONE', *, *, #45241, .T. ) ;
#36975 = VERTEX_POINT ( 'NONE', #57867 ) ;
#36976 = ORIENTED_EDGE ( 'NONE', *, *, #51886, .T. ) ;
#36977 = DIRECTION ( 'NONE',  ( 0.6575728627325956310, -0.7533909544171996098, 0.000000000000000000 ) ) ;
#36978 = ORIENTED_EDGE ( 'NONE', *, *, #1585, .T. ) ;
#36979 = ORIENTED_EDGE ( 'NONE', *, *, #1654, .F. ) ;
#36980 = CARTESIAN_POINT ( 'NONE',  ( 94.99999999999998579, 92.66308142843935514, 79.48281250086715488 ) ) ;
#36981 = FACE_BOUND ( 'NONE', #35791, .T. ) ;
#36982 = VECTOR ( 'NONE', #42811, 1000.000000000000114 ) ;
#36983 = CARTESIAN_POINT ( 'NONE',  ( -97.65000000000001990, 90.00000000000004263, 84.92000000000000171 ) ) ;
#36984 = AXIS2_PLACEMENT_3D ( 'NONE', #41942, #7723, #64879 ) ;
#36985 = ORIENTED_EDGE ( 'NONE', *, *, #62775, .T. ) ;
#36986 = CIRCLE ( 'NONE', #22559, 10.00000000000000178 ) ;
#36987 = ORIENTED_EDGE ( 'NONE', *, *, #13832, .F. ) ;
#36988 = ADVANCED_FACE ( 'NONE', ( #35301 ), #54356, .T. ) ;
#36989 = ORIENTED_EDGE ( 'NONE', *, *, #61288, .T. ) ;
#36990 = CARTESIAN_POINT ( 'NONE',  ( 12.00000000000000000, -1.278221433540507768, -26.51162292216071492 ) ) ;
#36991 = ORIENTED_EDGE ( 'NONE', *, *, #5650, .T. ) ;
#36992 = DIRECTION ( 'NONE',  ( 1.000000000000000000, 0.000000000000000000, 0.000000000000000000 ) ) ;
#36993 = CARTESIAN_POINT ( 'NONE',  ( 12.00000000000000000, -13.04903810567675393, -19.60159698893424718 ) ) ;
#36994 = VECTOR ( 'NONE', #8740, 1000.000000000000000 ) ;
#36995 = ADVANCED_FACE ( 'NONE', ( #25032 ), #3501, .T. ) ;
#36996 = CARTESIAN_POINT ( 'NONE',  ( -96.34407192492912486, 92.02656496471897185, 74.86703477254886252 ) ) ;
#36997 = CIRCLE ( 'NONE', #71802, 82.00000000000000000 ) ;
#36998 = PLANE ( 'NONE',  #59471 ) ;
#36999 = DIRECTION ( 'NONE',  ( -1.000000000000000000, 0.000000000000000000, 0.000000000000000000 ) ) ;
#37000 = ADVANCED_FACE ( 'NONE', ( #2878 ), #69508, .T. ) ;
#37001 = CARTESIAN_POINT ( 'NONE',  ( 0.000000000000000000, 5.256550761633951296, -77.32052557432835727 ) ) ;
#37002 = EDGE_CURVE ( 'NONE', #45883, #45327, #25772, .T. ) ;
#37003 = CARTESIAN_POINT ( 'NONE',  ( -94.99999999999997158, -213.0599564267049857, 77.53812500173428646 ) ) ;
#37004 = CARTESIAN_POINT ( 'NONE',  ( 0.000000000000000000, 0.000000000000000000, 0.000000000000000000 ) ) ;
#37006 = CARTESIAN_POINT ( 'NONE',  ( -92.35000000000005116, 91.52997821335253548, 74.57479166840096241 ) ) ;
#37005 = CARTESIAN_POINT ( 'NONE',  ( 94.99999999999998579, 86.94004357329500010, 75.63312500173429953 ) ) ;
#37007 = VERTEX_POINT ( 'NONE', #30661 ) ;
#37008 = CARTESIAN_POINT ( 'NONE',  ( 96.15314808468748708, 91.99731107132950569, 75.61989583420049144 ) ) ;
#37009 = DIRECTION ( 'NONE',  ( -1.000000000000000000, 0.000000000000000000, 0.000000000000000000 ) ) ;
#37010 = DIRECTION ( 'NONE',  ( -0.000000000000000000, -0.000000000000000000, 1.000000000000000000 ) ) ;
#37011 = CARTESIAN_POINT ( 'NONE',  ( -3.000000000000000000, -14.54903810567645195, -22.19967320028775504 ) ) ;
#37012 = LINE ( 'NONE', #53563, #25461 ) ;
#37013 = LINE ( 'NONE', #61437, #59513 ) ;
#37014 = ORIENTED_EDGE ( 'NONE', *, *, #55358, .T. ) ;
#37015 = CARTESIAN_POINT ( 'NONE',  ( -97.64999999999996305, -209.9999999999999716, 79.83999999999998920 ) ) ;
#37016 = CARTESIAN_POINT ( 'NONE',  ( 97.64999999999999147, 90.00000000000002842, 85.23749999999999716 ) ) ;
#37017 = ORIENTED_EDGE ( 'NONE', *, *, #39556, .F. ) ;
#37018 = AXIS2_PLACEMENT_3D ( 'NONE', #64001, #15628, #69629 ) ;
#37019 = ORIENTED_EDGE ( 'NONE', *, *, #31977, .T. ) ;
#37020 = CIRCLE ( 'NONE', #35823, 77.49899999999999523 ) ;
#37021 = AXIS2_PLACEMENT_3D ( 'NONE', #26789, #62520, #32795 ) ;
#37022 = ADVANCED_FACE ( 'NONE', ( #40954 ), #53603, .T. ) ;
#37023 = AXIS2_PLACEMENT_3D ( 'NONE', #47036, #18090, #24466 ) ;
#37024 = CYLINDRICAL_SURFACE ( 'NONE', #30715, 31.99999999999998579 ) ;
#37025 = PLANE ( 'NONE',  #52556 ) ;
#37026 = CARTESIAN_POINT ( 'NONE',  ( 92.69370383062501162, -209.9999999999999716, 89.80156250086714920 ) ) ;
#37027 = CYLINDRICAL_SURFACE ( 'NONE', #38779, 32.00000000000000000 ) ;
#37028 = DIRECTION ( 'NONE',  ( 0.000000000000000000, 0.000000000000000000, 1.000000000000000000 ) ) ;
#37029 = CARTESIAN_POINT ( 'NONE',  ( -94.99999999999997158, -212.6630814284392557, 75.99031250086716227 ) ) ;
#37030 = TOROIDAL_SURFACE ( 'NONE', #23825, 22.90000000000000213, 0.5999999999999937605 ) ;
#37031 = MANIFOLD_SOLID_BREP ( 'CirPattern1', #45204 ) ;
#37032 = ORIENTED_EDGE ( 'NONE', *, *, #14459, .F. ) ;
#37033 = DIRECTION ( 'NONE',  ( 0.000000000000000000, 0.000000000000000000, -1.000000000000000000 ) ) ;
#37034 = EDGE_CURVE ( 'NONE', #20333, #47275, #62315, .T. ) ;
#37035 = EDGE_CURVE ( 'NONE', #60828, #19874, #28706, .T. ) ;
#37036 = CARTESIAN_POINT ( 'NONE',  ( 11.99999999999999822, -58.39081064771713869, -50.95692526931392052 ) ) ;
#37037 = DIRECTION ( 'NONE',  ( 0.000000000000000000, 0.000000000000000000, 1.000000000000000000 ) ) ;
#37038 = LINE ( 'NONE', #65998, #22524 ) ;
#37039 = CARTESIAN_POINT ( 'NONE',  ( 0.000000000000000000, 0.000000000000000000, -125.0000000000000000 ) ) ;
#37040 = CARTESIAN_POINT ( 'NONE',  ( 0.000000000000000000, 0.000000000000000000, -40.00000000000000000 ) ) ;
#37041 = UNCERTAINTY_MEASURE_WITH_UNIT (LENGTH_MEASURE( 1.000000000000000082E-05 ), #49095, 'distance_accuracy_value', 'NONE');
#37042 =( LENGTH_UNIT ( ) NAMED_UNIT ( * ) SI_UNIT ( .MILLI., .METRE. ) );
#37043 = CARTESIAN_POINT ( 'NONE',  ( -96.32499999999996021, -212.2949673200287179, 76.13583333333333769 ) ) ;
#37044 = DIRECTION ( 'NONE',  ( -1.000000000000000000, 0.000000000000000000, -0.000000000000000000 ) ) ;
#37045 = VECTOR ( 'NONE', #69439, 1000.000000000000000 ) ;
#37046 = CARTESIAN_POINT ( 'NONE',  ( 92.69370383062498320, 88.66845928578035796, 84.13947916753383538 ) ) ;
#37047 = CIRCLE ( 'NONE', #2312, 77.49899999999999523 ) ;
#37048 = AXIS2_PLACEMENT_3D ( 'NONE', #11328, #6088, #62870 ) ;
#37049 = CARTESIAN_POINT ( 'NONE',  ( -94.99999999999997158, -212.6630814284392557, 86.15031250086717307 ) ) ;
#37050 = DIRECTION ( 'NONE',  ( -1.000000000000000000, 0.000000000000000000, -0.000000000000000000 ) ) ;
#37051 = ORIENTED_EDGE ( 'NONE', *, *, #62259, .T. ) ;
#37052 = DIRECTION ( 'NONE',  ( 0.000000000000000000, 0.000000000000000000, 1.000000000000000000 ) ) ;
#37053 = CARTESIAN_POINT ( 'NONE',  ( -93.67499999999998295, -207.7050326799711968, 81.53333333333333144 ) ) ;
#37054 = CARTESIAN_POINT ( 'NONE',  ( 10.00000000000000000, -26.02418014898260878, -70.52718814184285634 ) ) ;
#37055 = VECTOR ( 'NONE', #4594, 1000.000000000000000 ) ;
#37056 = VECTOR ( 'NONE', #42508, 1000.000000000000000 ) ;
#37057 = CARTESIAN_POINT ( 'NONE',  ( 97.30629616937498838, -211.3315407142195852, 84.19239583420046813 ) ) ;
#37058 = ORIENTED_EDGE ( 'NONE', *, *, #22263, .T. ) ;
#37059 = LINE ( 'NONE', #42700, #73007 ) ;
#37060 = ORIENTED_EDGE ( 'NONE', *, *, #52327, .T. ) ;
#37061 = ORIENTED_EDGE ( 'NONE', *, *, #60793, .T. ) ;
#37062 = AXIS2_PLACEMENT_3D ( 'NONE', #66364, #43062, #71603 ) ;
#37063 = CARTESIAN_POINT ( 'NONE',  ( 15.00000000000000000, -25.60904388321916159, 6.976881207771517879 ) ) ;
#37064 = AXIS2_PLACEMENT_3D ( 'NONE', #42820, #3359, #43210 ) ;
#37065 = ORIENTED_EDGE ( 'NONE', *, *, #12878, .F. ) ;
#37066 = AXIS2_PLACEMENT_3D ( 'NONE', #63171, #11628, #5290 ) ;
#37067 = FACE_OUTER_BOUND ( 'NONE', #67052, .T. ) ;
#37068 = AXIS2_PLACEMENT_3D ( 'NONE', #18547, #65537, #36953 ) ;
#37069 = CARTESIAN_POINT ( 'NONE',  ( 96.15314808468748708, -208.0026889286704943, 78.79489583420048859 ) ) ;
#37070 = CARTESIAN_POINT ( 'NONE',  ( -93.67499999999998295, -207.7050326799711968, 80.89833333333332632 ) ) ;
#37071 = LINE ( 'NONE', #70899, #52016 ) ;
#37072 = CIRCLE ( 'NONE', #74318, 37.49900000000000944 ) ;
#37073 = DIRECTION ( 'NONE',  ( -0.000000000000000000, 0.9781476007338042455, -0.2079116908177663092 ) ) ;
#37074 = CARTESIAN_POINT ( 'NONE',  ( 93.67499999999999716, 87.70503267997126784, 76.77083333333332860 ) ) ;
#37075 = DIRECTION ( 'NONE',  ( 0.000000000000000000, 0.000000000000000000, 1.000000000000000000 ) ) ;
#37076 = CARTESIAN_POINT ( 'NONE',  ( 97.64999999999997726, -211.5299782133524502, 80.10458333333332348 ) ) ;
#37077 = PRODUCT_DEFINITION ( 'UNKNOWN', '', #25660, #48410 ) ;
#37078 = EDGE_CURVE ( 'NONE', #45162, #63903, #26274, .T. ) ;
#37079 = ORIENTED_EDGE ( 'NONE', *, *, #49071, .T. ) ;
#37080 = ORIENTED_EDGE ( 'NONE', *, *, #41427, .F. ) ;
#37081 = VERTEX_POINT ( 'NONE', #4722 ) ;
#37082 = ORIENTED_EDGE ( 'NONE', *, *, #48443, .F. ) ;
#37083 = CARTESIAN_POINT ( 'NONE',  ( -93.67499999999998295, -212.2949673200287179, 86.48104166840096241 ) ) ;
#37084 = SURFACE_STYLE_USAGE ( .BOTH. , #54014 ) ;
#37085 = CARTESIAN_POINT ( 'NONE',  ( -92.69370383062504004, 90.00000000000004263, 85.67406250086715147 ) ) ;
#37086 = EDGE_CURVE ( 'NONE', #15073, #7371, #72723, .T. ) ;
#37087 = DIRECTION ( 'NONE',  ( -1.000000000000000000, 0.000000000000000000, -0.000000000000000000 ) ) ;
#37088 = FACE_OUTER_BOUND ( 'NONE', #13915, .T. ) ;
#37089 = CARTESIAN_POINT ( 'NONE',  ( 97.64999999999999147, 90.00000000000002842, 75.07749999999998636 ) ) ;
#37090 = CARTESIAN_POINT ( 'NONE',  ( 0.000000000000000000, -22.32062822937469804, -14.36278369418829826 ) ) ;
#37092 = VERTEX_POINT ( 'NONE', #21609 ) ;
#37091 = EDGE_CURVE ( 'NONE', #57268, #41863, #19095, .T. ) ;
#37093 = AXIS2_PLACEMENT_3D ( 'NONE', #19977, #66598, #66237 ) ;
#37094 = CARTESIAN_POINT ( 'NONE',  ( -94.99999999999997158, -213.0599564267049857, 84.52312500173428589 ) ) ;
#37095 = EDGE_LOOP ( 'NONE', ( #26254, #53334, #27374, #73395 ) ) ;
#37096 = CARTESIAN_POINT ( 'NONE',  ( 12.00000000000000000, 5.835314593368470248, -22.81335362449854642 ) ) ;
#37097 = ORIENTED_EDGE ( 'NONE', *, *, #23333, .F. ) ;
#37098 = CARTESIAN_POINT ( 'NONE',  ( -97.65000000000001990, 90.00000000000004263, 85.63437500173431260 ) ) ;
#37099 = ADVANCED_FACE ( 'NONE', ( #54716 ), #32137, .F. ) ;
#37100 = VECTOR ( 'NONE', #63358, 1000.000000000000000 ) ;
#37101 = ORIENTED_EDGE ( 'NONE', *, *, #63347, .T. ) ;
#37102 = CARTESIAN_POINT ( 'NONE',  ( 94.99999999999998579, 87.33691857156068750, 87.42031250086715488 ) ) ;
#37103 = CARTESIAN_POINT ( 'NONE',  ( 0.000000000000000000, -120.0000000000000000, -125.0000000000000000 ) ) ;
#37104 = AXIS2_PLACEMENT_3D ( 'NONE', #21236, #44191, #61491 ) ;
#37105 = CIRCLE ( 'NONE', #38271, 82.00000000000000000 ) ;
#37106 = FACE_OUTER_BOUND ( 'NONE', #28280, .T. ) ;
#37107 = FACE_OUTER_BOUND ( 'NONE', #45533, .T. ) ;
#37108 = DIRECTION ( 'NONE',  ( 0.000000000000000000, 0.000000000000000000, 1.000000000000000000 ) ) ;
#37109 = ORIENTED_EDGE ( 'NONE', *, *, #34461, .F. ) ;
#37110 = CARTESIAN_POINT ( 'NONE',  ( 12.00000000000000000, -0.9646360437375370855, -23.52805723605590060 ) ) ;
#37111 = DIRECTION ( 'NONE',  ( -0.000000000000000000, -0.000000000000000000, -1.000000000000000000 ) ) ;
#37112 = ORIENTED_EDGE ( 'NONE', *, *, #27227, .T. ) ;
#37113 = AXIS2_PLACEMENT_3D ( 'NONE', #8270, #3040, #18440 ) ;
#37114 = ORIENTED_EDGE ( 'NONE', *, *, #27410, .T. ) ;
#37115 = CIRCLE ( 'NONE', #16721, 32.00000000000000000 ) ;
#37116 = CARTESIAN_POINT ( 'NONE',  ( 10.00000000000000000, -37.22597642581161637, 5.202137450156258502 ) ) ;
#37117 = EDGE_CURVE ( 'NONE', #7584, #54778, #50550, .T. ) ;
#37118 = EDGE_CURVE ( 'NONE', #67395, #8860, #26132, .T. ) ;
#37119 = CARTESIAN_POINT ( 'NONE',  ( 11.99999999999999822, 62.50329211542494789, -41.76937507738723099 ) ) ;
#37120 = PLANE ( 'NONE',  #64147 ) ;
#37121 = CARTESIAN_POINT ( 'NONE',  ( -97.30629616937497417, -211.3315407142195852, 82.86947916753382515 ) ) ;
#37122 = ORIENTED_EDGE ( 'NONE', *, *, #1401, .T. ) ;
#37123 = CARTESIAN_POINT ( 'NONE',  ( 92.34999999999999432, 90.00000000000002842, 90.00000000000000000 ) ) ;
#37124 = VERTEX_POINT ( 'NONE', #66745 ) ;
#37125 = AXIS2_PLACEMENT_3D ( 'NONE', #51357, #17158, #63046 ) ;
#37126 = VECTOR ( 'NONE', #31679, 1000.000000000000000 ) ;
#37127 = ORIENTED_EDGE ( 'NONE', *, *, #52910, .T. ) ;
#37128 = DIRECTION ( 'NONE',  ( -1.000000000000000000, 0.000000000000000000, 0.000000000000000000 ) ) ;
#37129 = VECTOR ( 'NONE', #14306, 1000.000000000000000 ) ;
#37130 = EDGE_CURVE ( 'NONE', #28860, #42708, #59901, .T. ) ;
#37131 = AXIS2_PLACEMENT_3D ( 'NONE', #31523, #28476, #339 ) ;
#37132 = CARTESIAN_POINT ( 'NONE',  ( 97.30629616937498838, 88.66845928578037217, 89.43114583420049257 ) ) ;
#37133 = DIRECTION ( 'NONE',  ( 0.000000000000000000, 0.000000000000000000, 1.000000000000000000 ) ) ;
#37134 = CARTESIAN_POINT ( 'NONE',  ( 97.30629616937498838, 90.00000000000002842, 78.53031250086714010 ) ) ;
#37135 = DIRECTION ( 'NONE',  ( -1.000000000000000000, -0.000000000000000000, -0.000000000000000000 ) ) ;
#37136 = DIRECTION ( 'NONE',  ( -1.000000000000000000, 0.000000000000000000, -0.000000000000000000 ) ) ;
#37137 = DIRECTION ( 'NONE',  ( 0.000000000000000000, -0.8910065241883722287, 0.4539904997395383113 ) ) ;
#37138 = VECTOR ( 'NONE', #53343, 1000.000000000000000 ) ;
#37139 = CARTESIAN_POINT ( 'NONE',  ( 94.68886060456908638, 92.37342585364821446, 74.84415580543370083 ) ) ;
#37140 = AXIS2_PLACEMENT_3D ( 'NONE', #58687, #7188, #47767 ) ;
#37141 = DIRECTION ( 'NONE',  ( 2.603472992746261562E-14, 2.546204323184492723E-14, -1.000000000000000000 ) ) ;
#37142 = DIRECTION ( 'NONE',  ( 1.000000000000000000, 0.000000000000000000, 0.000000000000000000 ) ) ;
#37143 = CIRCLE ( 'NONE', #56355, 77.49900000000000944 ) ;
#37144 = CARTESIAN_POINT ( 'NONE',  ( -5.565113727472242644, 10.17789316117535137, 52.00000000000002132 ) ) ;
#37145 = CARTESIAN_POINT ( 'NONE',  ( 97.64999999999999147, 90.00000000000002842, 82.69749999999999091 ) ) ;
#37146 = ORIENTED_EDGE ( 'NONE', *, *, #70682, .T. ) ;
#37147 = CARTESIAN_POINT ( 'NONE',  ( -93.84685191531252713, 88.00268892867056536, 86.04447916753380809 ) ) ;
#37148 = CYLINDRICAL_SURFACE ( 'NONE', #62401, 35.50000000000000711 ) ;
#37149 = DIRECTION ( 'NONE',  ( -1.000000000000000000, 0.000000000000000000, 0.000000000000000000 ) ) ;
#37150 = ORIENTED_EDGE ( 'NONE', *, *, #60218, .T. ) ;
#37151 =( BOUNDED_CURVE ( )  B_SPLINE_CURVE ( 2, ( #41162, #1356, #69725, #63733, #11466, #52812, #24247, #977, #68634 ),
 .UNSPECIFIED., .F., .F. ) 
 B_SPLINE_CURVE_WITH_KNOTS ( ( 3, 2, 2, 2, 3 ),
 ( 0.9313609857438962525, 0.9313610514010480790, 0.9384168169419646599, 0.9454725824828811298, 0.9525283480368235134 ),
 .UNSPECIFIED. ) 
 CURVE ( )  GEOMETRIC_REPRESENTATION_ITEM ( )  RATIONAL_B_SPLINE_CURVE ( ( 0.9999975066324136019, 0.9999987533046057475, 1.000000000000000000, 0.8660254037844387076, 1.000000000000000000, 0.8660254037844387076, 1.000000000000000000, 0.8660254037844387076, 1.000000000000000000 ) ) 
 REPRESENTATION_ITEM ( '' )  );
#37153 = DIRECTION ( 'NONE',  ( 1.000000000000000000, -0.000000000000000000, -0.000000000000000000 ) ) ;
#37152 = VECTOR ( 'NONE', #17771, 1000.000000000000114 ) ;
#37154 = CYLINDRICAL_SURFACE ( 'NONE', #34766, 11.59999999999999787 ) ;
#37155 = DIRECTION ( 'NONE',  ( -1.000000000000000000, 0.000000000000000000, -0.000000000000000000 ) ) ;
#37156 = AXIS2_PLACEMENT_3D ( 'NONE', #44856, #55379, #9517 ) ;
#37157 = EDGE_CURVE ( 'NONE', #59272, #68833, #25047, .T. ) ;
#37158 = VECTOR ( 'NONE', #53685, 1000.000000000000000 ) ;
#37159 = VECTOR ( 'NONE', #18147, 1000.000000000000114 ) ;
#37160 = CARTESIAN_POINT ( 'NONE',  ( 95.00000000000000000, -212.6630814284392557, 80.43531250086715545 ) ) ;
#37161 = AXIS2_PLACEMENT_3D ( 'NONE', #19301, #65184, #53890 ) ;
#37162 = VERTEX_POINT ( 'NONE', #43463 ) ;
#37163 = EDGE_CURVE ( 'NONE', #35072, #3438, #61121, .T. ) ;
#37164 = ORIENTED_EDGE ( 'NONE', *, *, #5278, .F. ) ;
#37165 = EDGE_CURVE ( 'NONE', #24000, #62600, #23885, .T. ) ;
#37166 = DIRECTION ( 'NONE',  ( -1.000000000000000000, 0.000000000000000000, -0.000000000000000000 ) ) ;
#37167 = CARTESIAN_POINT ( 'NONE',  ( 7.103376864691351012E-17, -120.0000000000000000, -64.00000000000000000 ) ) ;
#37168 = CARTESIAN_POINT ( 'NONE',  ( -94.99999999999997158, -209.9999999999999716, 90.00000000000000000 ) ) ;
#37169 = EDGE_LOOP ( 'NONE', ( #19942, #64267, #50603, #22177 ) ) ;
#37170 = CARTESIAN_POINT ( 'NONE',  ( 97.30629616937498838, -209.9999999999999716, 76.14906250086716000 ) ) ;
#37171 = EDGE_CURVE ( 'NONE', #5952, #24150, #64130, .T. ) ;
#37172 = CIRCLE ( 'NONE', #70751, 77.49900000000000944 ) ;
#37173 = ORIENTED_EDGE ( 'NONE', *, *, #37078, .T. ) ;
#37174 = CARTESIAN_POINT ( 'NONE',  ( -14.87942725330654348, -141.9795960975983178, -2.500000000000000000 ) ) ;
#37175 = ORIENTED_EDGE ( 'NONE', *, *, #7901, .F. ) ;
#37176 = ORIENTED_EDGE ( 'NONE', *, *, #12053, .F. ) ;
#37177 = CARTESIAN_POINT ( 'NONE',  ( -92.34999999999992326, 88.47002178664760663, 83.27958333333332064 ) ) ;
#37178 = VECTOR ( 'NONE', #52427, 1000.000000000000000 ) ;
#37179 = CIRCLE ( 'NONE', #6016, 2.649999999999985700 ) ;
#37180 = LINE ( 'NONE', #31517, #34094 ) ;
#37181 = VECTOR ( 'NONE', #44491, 1000.000000000000000 ) ;
#37182 = EDGE_LOOP ( 'NONE', ( #46069, #47886, #45780, #15982 ) ) ;
#37183 = CARTESIAN_POINT ( 'NONE',  ( 4.999999999999999112, -10.41901085202050581, -40.68715046381939970 ) ) ;
#37184 = CARTESIAN_POINT ( 'NONE',  ( 92.35000000000002274, -211.5299782133524502, 83.78229166840095843 ) ) ;
#37185 = CARTESIAN_POINT ( 'NONE',  ( 96.32499999999998863, 87.70503267997126784, 85.13166666666666060 ) ) ;
#37186 = ORIENTED_EDGE ( 'NONE', *, *, #33272, .F. ) ;
#37187 = FACE_OUTER_BOUND ( 'NONE', #31951, .T. ) ;
#37188 = DIRECTION ( 'NONE',  ( -1.000000000000000000, -0.000000000000000000, 0.000000000000000000 ) ) ;
#37189 = ORIENTED_EDGE ( 'NONE', *, *, #64858, .T. ) ;
#37190 = ORIENTED_EDGE ( 'NONE', *, *, #41163, .F. ) ;
#37191 = CARTESIAN_POINT ( 'NONE',  ( -95.00000000000002842, 92.66308142843932671, 86.46781250086714010 ) ) ;
#37192 = EDGE_CURVE ( 'NONE', #50665, #53082, #55096, .T. ) ;
#37193 = CARTESIAN_POINT ( 'NONE',  ( 96.15314808468748708, 88.00268892867053694, 82.23447916753380582 ) ) ;
#37194 = ORIENTED_EDGE ( 'NONE', *, *, #22670, .F. ) ;
#37195 = CARTESIAN_POINT ( 'NONE',  ( 93.67499999999999716, 87.70503267997126784, 83.20020833506764291 ) ) ;
#37196 = FACE_OUTER_BOUND ( 'NONE', #21471, .T. ) ;
#37197 = ORIENTED_EDGE ( 'NONE', *, *, #44073, .F. ) ;
#37198 = CARTESIAN_POINT ( 'NONE',  ( 96.32499999999998863, -212.2949673200287179, 78.14666666666667538 ) ) ;
#37199 = EDGE_LOOP ( 'NONE', ( #22569, #67496, #49998, #1470 ) ) ;
#37200 = ORIENTED_EDGE ( 'NONE', *, *, #17382, .T. ) ;
#37201 = ORIENTED_EDGE ( 'NONE', *, *, #61454, .F. ) ;
#37202 = CARTESIAN_POINT ( 'NONE',  ( -93.67500000000003979, 92.29496732002878900, 85.97833333333332462 ) ) ;
#37203 = DIRECTION ( 'NONE',  ( -0.4796670183876317051, 0.8774505977381971134, 0.000000000000000000 ) ) ;
#37204 = CARTESIAN_POINT ( 'NONE',  ( -96.32500000000001705, 92.29496732002878900, 85.44916666666665606 ) ) ;
#37205 = EDGE_CURVE ( 'NONE', #41131, #24664, #60374, .T. ) ;
#37206 = ORIENTED_EDGE ( 'NONE', *, *, #35075, .T. ) ;
#37207 = EDGE_CURVE ( 'NONE', #41508, #34514, #20870, .T. ) ;
#37208 = FACE_OUTER_BOUND ( 'NONE', #62217, .T. ) ;
#37209 = FACE_OUTER_BOUND ( 'NONE', #16747, .T. ) ;
#37210 = EDGE_LOOP ( 'NONE', ( #26625, #69002, #53239, #64472 ) ) ;
#37211 = DIRECTION ( 'NONE',  ( -1.000000000000000000, 3.061616997868382648E-16, 0.000000000000000000 ) ) ;
#37212 = CARTESIAN_POINT ( 'NONE',  ( -97.30629616937497417, -208.6684592857803011, 79.42989583420046529 ) ) ;
#37213 = ORIENTED_EDGE ( 'NONE', *, *, #58767, .T. ) ;
#37214 = AXIS2_PLACEMENT_3D ( 'NONE', #34238, #62843, #51528 ) ;
#37215 = EDGE_CURVE ( 'NONE', #31963, #62638, #2516, .T. ) ;
#37216 = LINE ( 'NONE', #19531, #72283 ) ;
#37217 = CARTESIAN_POINT ( 'NONE',  ( 0.000000000000000000, 0.000000000000000000, -6.000000000000000000 ) ) ;
#37218 = CARTESIAN_POINT ( 'NONE',  ( 10.00000000000000000, -75.16055320797043748, 18.89407956138229494 ) ) ;
#37219 = CARTESIAN_POINT ( 'NONE',  ( -11.59999999999999787, 0.000000000000000000, -54.99999999999998579 ) ) ;
#37220 = CIRCLE ( 'NONE', #46827, 12.49999999999999822 ) ;
#37221 = AXIS2_PLACEMENT_3D ( 'NONE', #7267, #12884, #17432 ) ;
#37222 = CARTESIAN_POINT ( 'NONE',  ( 0.000000000000000000, -22.67460108101783334, 6.353146135317912169 ) ) ;
#37223 = CARTESIAN_POINT ( 'NONE',  ( 10.00000000000000000, 0.000000000000000000, 0.000000000000000000 ) ) ;
#37224 = CARTESIAN_POINT ( 'NONE',  ( -10.00000000000000000, 0.000000000000000000, 0.000000000000000000 ) ) ;
#37225 = CARTESIAN_POINT ( 'NONE',  ( -92.35000000000007958, -211.5299782133525071, 85.81958333333332689 ) ) ;
#37226 = DIRECTION ( 'NONE',  ( -1.000000000000000000, 0.000000000000000000, 0.000000000000000000 ) ) ;
#37227 = CARTESIAN_POINT ( 'NONE',  ( 96.32499999999998863, 87.70503267997126784, 86.48104166840096241 ) ) ;
#37228 = CARTESIAN_POINT ( 'NONE',  ( -93.84685191531252713, 88.00268892867056536, 76.51947916753380241 ) ) ;
#37229 = DIRECTION ( 'NONE',  ( -1.000000000000000000, 0.000000000000000000, 0.000000000000000000 ) ) ;
#37230 = CARTESIAN_POINT ( 'NONE',  ( 0.000000000000000000, 2.956366410621684260, -75.11725578898465017 ) ) ;
#37231 = DIRECTION ( 'NONE',  ( -1.000000000000000000, 0.000000000000000000, 0.000000000000000000 ) ) ;
#37232 = DIRECTION ( 'NONE',  ( -0.000000000000000000, -0.000000000000000000, 1.000000000000000000 ) ) ;
#37233 = CIRCLE ( 'NONE', #56446, 31.99999999999998934 ) ;
#37234 = VECTOR ( 'NONE', #52925, 1000.000000000000000 ) ;
#37235 = AXIS2_PLACEMENT_3D ( 'NONE', #37513, #72076, #60450 ) ;
#37236 = DIRECTION ( 'NONE',  ( 0.000000000000000000, 0.3090169943749573878, -0.9510565162951503115 ) ) ;
#37237 = LINE ( 'NONE', #61929, #51456 ) ;
#37238 = AXIS2_PLACEMENT_3D ( 'NONE', #47475, #53483, #24904 ) ;
#37239 = DIRECTION ( 'NONE',  ( 0.000000000000000000, 0.000000000000000000, -1.000000000000000000 ) ) ;
#37240 = DIRECTION ( 'NONE',  ( 0.000000000000000000, -1.000000000000000000, 0.000000000000000000 ) ) ;
#37241 = LINE ( 'NONE', #48143, #7642 ) ;
#37242 = CARTESIAN_POINT ( 'NONE',  ( -96.32499999999996021, -207.7050326799711968, 88.62416666666665321 ) ) ;
#37243 = CIRCLE ( 'NONE', #40846, 31.99999999999998579 ) ;
#37244 = AXIS2_PLACEMENT_3D ( 'NONE', #63977, #52683, #6818 ) ;
#37245 = CARTESIAN_POINT ( 'NONE',  ( 0.000000000000000000, 16.00000000000000000, -2.500000000000000000 ) ) ;
#37246 = EDGE_LOOP ( 'NONE', ( #45527, #11393, #33863, #435 ) ) ;
#37247 = DIRECTION ( 'NONE',  ( -1.000000000000000000, -0.000000000000000000, 0.000000000000000000 ) ) ;
#37248 = DIRECTION ( 'NONE',  ( -1.000000000000000000, 0.000000000000000000, 0.000000000000000000 ) ) ;
#37249 = SURFACE_SIDE_STYLE ('',( #38344 ) ) ;
#37250 = DIRECTION ( 'NONE',  ( 0.000000000000000000, 0.000000000000000000, 1.000000000000000000 ) ) ;
#37251 = EDGE_CURVE ( 'NONE', #14220, #2716, #40028, .T. ) ;
#37252 = EDGE_CURVE ( 'NONE', #57613, #30770, #16696, .T. ) ;
#37253 = VERTEX_POINT ( 'NONE', #74224 ) ;
#37255 = EDGE_CURVE ( 'NONE', #32997, #68921, #68605, .T. ) ;
#37254 = DIRECTION ( 'NONE',  ( -1.000000000000000000, 0.000000000000000000, -0.000000000000000000 ) ) ;
#37256 = CARTESIAN_POINT ( 'NONE',  ( 0.000000000000000000, 37.01155633439068282, -6.555932627142014191 ) ) ;
#37257 = ORIENTED_EDGE ( 'NONE', *, *, #46212, .F. ) ;
#37258 = CARTESIAN_POINT ( 'NONE',  ( 95.00000000000000000, -212.6630814284392557, 80.27656250086714351 ) ) ;
#37259 = CARTESIAN_POINT ( 'NONE',  ( 95.00000000000000000, -212.6630814284392557, 88.69031250086716511 ) ) ;
#37260 = ORIENTED_EDGE ( 'NONE', *, *, #70512, .F. ) ;
#37261 = CARTESIAN_POINT ( 'NONE',  ( 97.30629616937498838, -208.6684592857803011, 86.36197916753383197 ) ) ;
#37262 = EDGE_CURVE ( 'NONE', #48721, #66932, #34655, .T. ) ;
#37263 = CIRCLE ( 'NONE', #60089, 82.00000000000000000 ) ;
#37264 = ADVANCED_BREP_SHAPE_REPRESENTATION ( '', ( #36889, #43395 ), #56756 ) ;
#37265 = ORIENTED_EDGE ( 'NONE', *, *, #12711, .T. ) ;
#37266 = CARTESIAN_POINT ( 'NONE',  ( 0.000000000000000000, 26.08949754953024325, 27.05870788708241648 ) ) ;
#37267 = ORIENTED_EDGE ( 'NONE', *, *, #32334, .T. ) ;
#37268 = AXIS2_PLACEMENT_3D ( 'NONE', #67180, #3681, #31477 ) ;
#37269 = CARTESIAN_POINT ( 'NONE',  ( -97.30629616937501680, 90.00000000000004263, 77.73656250086715147 ) ) ;
#37270 = ORIENTED_EDGE ( 'NONE', *, *, #21629, .F. ) ;
#37271 = ORIENTED_EDGE ( 'NONE', *, *, #10709, .F. ) ;
#37272 = CIRCLE ( 'NONE', #51655, 37.49900000000000944 ) ;
#37273 = DIRECTION ( 'NONE',  ( 0.000000000000000000, 0.000000000000000000, 1.000000000000000000 ) ) ;
#37274 = ORIENTED_EDGE ( 'NONE', *, *, #32909, .T. ) ;
#37275 = CARTESIAN_POINT ( 'NONE',  ( 10.00000000000000000, 62.20884554314020676, 46.21855187248652896 ) ) ;
#37276 = CARTESIAN_POINT ( 'NONE',  ( 0.000000000000000000, -44.88180994100329713, -63.18004540533077318 ) ) ;
#37277 = VERTEX_POINT ( 'NONE', #11439 ) ;
#37278 = CARTESIAN_POINT ( 'NONE',  ( 15.00000000000000000, -18.13022148937263012, -15.02647892043543898 ) ) ;
#37279 = ORIENTED_EDGE ( 'NONE', *, *, #64443, .F. ) ;
#37280 = CARTESIAN_POINT ( 'NONE',  ( 95.00000000000000000, -209.9999999999999716, 90.00000000000000000 ) ) ;
#37281 = ADVANCED_FACE ( 'NONE', ( #34004 ), #62603, .T. ) ;
#37282 = ORIENTED_EDGE ( 'NONE', *, *, #66287, .F. ) ;
#37283 = VECTOR ( 'NONE', #30905, 1000.000000000000000 ) ;
#37284 = ORIENTED_EDGE ( 'NONE', *, *, #21892, .T. ) ;
#37285 = ORIENTED_EDGE ( 'NONE', *, *, #6109, .F. ) ;
#37286 = CIRCLE ( 'NONE', #50420, 42.00000000000000000 ) ;
#37287 = CARTESIAN_POINT ( 'NONE',  ( 92.69370383062501162, -211.3315407142195852, 76.99572916753380980 ) ) ;
#37288 = VECTOR ( 'NONE', #13517, 1000.000000000000000 ) ;
#37289 = LINE ( 'NONE', #70351, #13672 ) ;
#37290 = CARTESIAN_POINT ( 'NONE',  ( -97.65000000000001990, 90.00000000000004263, 81.74500000000000455 ) ) ;
#37291 = ORIENTED_EDGE ( 'NONE', *, *, #35168, .F. ) ;
#37292 = ORIENTED_EDGE ( 'NONE', *, *, #21049, .F. ) ;
#37293 = DIRECTION ( 'NONE',  ( -1.000000000000000000, -0.000000000000000000, -0.000000000000000000 ) ) ;
#37294 = CARTESIAN_POINT ( 'NONE',  ( 11.59999999999999787, 1.420590287010929336E-15, 42.00000000000001421 ) ) ;
#37295 = ORIENTED_EDGE ( 'NONE', *, *, #12660, .F. ) ;
#37296 = CARTESIAN_POINT ( 'NONE',  ( -17.26469406256017791, -140.1601175325492648, -2.500000000000000444 ) ) ;
#37297 = AXIS2_PLACEMENT_3D ( 'NONE', #40025, #29453, #68602 ) ;
#37298 = DIRECTION ( 'NONE',  ( 0.000000000000000000, 0.9510565162951536422, 0.3090169943749471182 ) ) ;
#37299 = CARTESIAN_POINT ( 'NONE',  ( -92.69370383062498320, -211.3315407142195852, 79.74739583420047495 ) ) ;
#37300 = CARTESIAN_POINT ( 'NONE',  ( -95.00000000000002842, 92.66308142843932671, 80.11781250086714579 ) ) ;
#37301 = EDGE_CURVE ( 'NONE', #10228, #21580, #5917, .T. ) ;
#37302 = ORIENTED_EDGE ( 'NONE', *, *, #9533, .T. ) ;
#37303 = ADVANCED_FACE ( 'NONE', ( #73478 ), #67854, .T. ) ;
#37304 = CARTESIAN_POINT ( 'NONE',  ( 97.30629616937498838, 90.00000000000002842, 79.80031250086713612 ) ) ;
#37305 = ORIENTED_EDGE ( 'NONE', *, *, #39739, .T. ) ;
#37306 = CARTESIAN_POINT ( 'NONE',  ( 0.000000000000000000, 33.80338159004307386, -16.23288003029461279 ) ) ;
#37307 = CARTESIAN_POINT ( 'NONE',  ( -92.69370383062498320, -208.6684592857803011, 89.37822916753381719 ) ) ;
#37308 = DIRECTION ( 'NONE',  ( 1.000000000000000000, 0.000000000000000000, 0.000000000000000000 ) ) ;
#37309 = CARTESIAN_POINT ( 'NONE',  ( -2.977765906491215642, 15.77977592589476608, 0.000000000000000000 ) ) ;
#37310 = DIRECTION ( 'NONE',  ( -1.000000000000000000, 0.000000000000000000, -0.000000000000000000 ) ) ;
#37311 = CARTESIAN_POINT ( 'NONE',  ( -93.84685191531248449, -208.0026889286704943, 84.35114583420048007 ) ) ;
#37312 = CYLINDRICAL_SURFACE ( 'NONE', #25373, 31.99999999999999289 ) ;
#37313 = LINE ( 'NONE', #31279, #43943 ) ;
#37314 = CARTESIAN_POINT ( 'NONE',  ( -10.00000000000000000, 0.000000000000000000, 0.000000000000000000 ) ) ;
#37315 = VERTEX_POINT ( 'NONE', #28733 ) ;
#37316 = VERTEX_POINT ( 'NONE', #22743 ) ;
#37317 = CARTESIAN_POINT ( 'NONE',  ( 0.000000000000000000, 0.000000000000000000, 0.000000000000000000 ) ) ;
#37318 = CARTESIAN_POINT ( 'NONE',  ( -92.35000000000003695, 90.00000000000004263, 75.07749999999998636 ) ) ;
#37319 = CARTESIAN_POINT ( 'NONE',  ( 10.00000000000000000, 51.03279382321088065, 55.19960302592086521 ) ) ;
#37320 = CARTESIAN_POINT ( 'NONE',  ( -93.84685191531254134, 91.99731107132950569, 84.98614583420047097 ) ) ;
#37321 = CARTESIAN_POINT ( 'NONE',  ( -97.42291288542703853, -209.3980460039468596, 74.90604073465185309 ) ) ;
#37322 = CYLINDRICAL_SURFACE ( 'NONE', #227, 16.00000000000000000 ) ;
#37323 = LINE ( 'NONE', #61633, #58889 ) ;
#37324 = VERTEX_POINT ( 'NONE', #40771 ) ;
#37325 = CARTESIAN_POINT ( 'NONE',  ( 11.99999999999999822, -23.16143007188479430, 73.95703589263968070 ) ) ;
#37326 = CIRCLE ( 'NONE', #46929, 31.99999999999999289 ) ;
#37327 = VECTOR ( 'NONE', #35458, 1000.000000000000000 ) ;
#37328 = CARTESIAN_POINT ( 'NONE',  ( -32.50000000000000000, -120.0000000000000000, 2.500000000000000000 ) ) ;
#37329 = LINE ( 'NONE', #72256, #19056 ) ;
#37330 = DIRECTION ( 'NONE',  ( 0.000000000000000000, 0.000000000000000000, 1.000000000000000000 ) ) ;
#37331 = CARTESIAN_POINT ( 'NONE',  ( 97.64999999999999147, -209.9999999999999716, 84.60249999999999204 ) ) ;
#37332 = DIRECTION ( 'NONE',  ( 0.000000000000000000, 0.000000000000000000, 1.000000000000000000 ) ) ;
#37333 = CARTESIAN_POINT ( 'NONE',  ( -94.99999999999997158, -207.3369185715606307, 82.65781250086715204 ) ) ;
#37334 = PLANE ( 'NONE',  #26878 ) ;
#37335 = EDGE_CURVE ( 'NONE', #29463, #23135, #22717, .T. ) ;
#37336 = CARTESIAN_POINT ( 'NONE',  ( 97.30629616937498838, 91.33154071421968467, 74.93197916753381094 ) ) ;
#37337 = EDGE_CURVE ( 'NONE', #6591, #26875, #27989, .T. ) ;
#37338 = DIRECTION ( 'NONE',  ( -1.000000000000000000, -0.000000000000000000, 0.000000000000000000 ) ) ;
#37339 = DIRECTION ( 'NONE',  ( 0.000000000000000000, -0.7071067811865536790, 0.7071067811865414665 ) ) ;
#37340 = VECTOR ( 'NONE', #45839, 1000.000000000000000 ) ;
#37341 = ORIENTED_EDGE ( 'NONE', *, *, #62470, .T. ) ;
#37342 = DIRECTION ( 'NONE',  ( 0.000000000000000000, 0.000000000000000000, -1.000000000000000000 ) ) ;
#37343 = CARTESIAN_POINT ( 'NONE',  ( -95.00000000000002842, 93.05995642670504253, 78.41125000000000966 ) ) ;
#37344 = CARTESIAN_POINT ( 'NONE',  ( 0.000000000000000000, 81.34940948281351325, -10.30890764327295450 ) ) ;
#37345 = CIRCLE ( 'NONE', #9747, 37.49900000000000944 ) ;
#37346 = ADVANCED_FACE ( 'NONE', ( #63336 ), #34754, .T. ) ;
#37347 = AXIS2_PLACEMENT_3D ( 'NONE', #71021, #20643, #14252 ) ;
#37348 = VECTOR ( 'NONE', #46945, 1000.000000000000000 ) ;
#37349 = EDGE_CURVE ( 'NONE', #70803, #43515, #6194, .T. ) ;
#37350 = CARTESIAN_POINT ( 'NONE',  ( 11.99999999999999822, 69.42325613327489009, -34.44570377933524696 ) ) ;
#37351 = CARTESIAN_POINT ( 'NONE',  ( 95.00000000000000000, -212.6630814284392557, 75.19656250086714522 ) ) ;
#37352 = ORIENTED_EDGE ( 'NONE', *, *, #2882, .T. ) ;
#37353 = CARTESIAN_POINT ( 'NONE',  ( 94.99999999999998579, 86.94004357329502852, 87.06312500173429214 ) ) ;
#37354 = DIRECTION ( 'NONE',  ( -1.000000000000000000, 0.000000000000000000, 0.000000000000000000 ) ) ;
#37355 = ORIENTED_EDGE ( 'NONE', *, *, #27160, .F. ) ;
#37356 = LINE ( 'NONE', #72277, #67636 ) ;
#37357 = ORIENTED_EDGE ( 'NONE', *, *, #69450, .F. ) ;
#37358 = EDGE_CURVE ( 'NONE', #47235, #26707, #37072, .T. ) ;
#37359 = LINE ( 'NONE', #19672, #12965 ) ;
#37360 = EDGE_LOOP ( 'NONE', ( #39560, #37079, #60476, #29643 ) ) ;
#37361 = ORIENTED_EDGE ( 'NONE', *, *, #63025, .T. ) ;
#37362 = ORIENTED_EDGE ( 'NONE', *, *, #43218, .T. ) ;
#37363 = ORIENTED_EDGE ( 'NONE', *, *, #71182, .T. ) ;
#37364 = CARTESIAN_POINT ( 'NONE',  ( 97.64999999999602665, -210.0000045800691737, 76.42687486206342840 ) ) ;
#37365 = EDGE_LOOP ( 'NONE', ( #57007, #14128, #3826, #62525 ) ) ;
#37366 = PRODUCT ( 'Sliding Dog Clutch Collar', 'Sliding Dog Clutch Collar', '', ( #51972 ) ) ;
#37367 = EDGE_CURVE ( 'NONE', #31034, #19670, #31048, .T. ) ;
#37368 = VERTEX_POINT ( 'NONE', #35118 ) ;
#37369 = CARTESIAN_POINT ( 'NONE',  ( 92.69370383062498320, 88.66845928578037217, 79.05947916753382287 ) ) ;
#37370 = LINE ( 'NONE', #60309, #2399 ) ;
#37371 = ADVANCED_FACE ( 'NONE', ( #580 ), #23112, .F. ) ;
#37372 = DIRECTION ( 'NONE',  ( 0.000000000000000000, -0.9969173337331270757, -0.07845909572785580988 ) ) ;
#37373 = ORIENTED_EDGE ( 'NONE', *, *, #43722, .F. ) ;
#37374 = VERTEX_POINT ( 'NONE', #39287 ) ;
#37375 = STYLED_ITEM ( 'NONE', ( #21590 ), #68699 ) ;
#37376 = AXIS2_PLACEMENT_3D ( 'NONE', #61805, #27946, #62554 ) ;
#37377 = VERTEX_POINT ( 'NONE', #2437 ) ;
#37378 = DIRECTION ( 'NONE',  ( 0.000000000000000000, 0.2079116908177545131, -0.9781476007338066880 ) ) ;
#37380 = ORIENTED_EDGE ( 'NONE', *, *, #57036, .T. ) ;
#37379 = EDGE_CURVE ( 'NONE', #15888, #47617, #1912, .T. ) ;
#37381 = CARTESIAN_POINT ( 'NONE',  ( 1.163636965939583898E-11, -1.165934815928031957E-12, 81.99999999999994316 ) ) ;
#37382 = CARTESIAN_POINT ( 'NONE',  ( 10.00000000000000000, -37.22597642581153821, -5.202137450156795850 ) ) ;
#37384 = AXIS2_PLACEMENT_3D ( 'NONE', #32024, #49317, #13992 ) ;
#37383 = LINE ( 'NONE', #2085, #35172 ) ;
#37385 = CARTESIAN_POINT ( 'NONE',  ( 15.00000000000000000, -1.278221433540145391, 26.51162292216073979 ) ) ;
#37386 = LINE ( 'NONE', #26079, #30635 ) ;
#37387 = CARTESIAN_POINT ( 'NONE',  ( 5.999999999999999112, 63.97538442413426907, 51.29473840253246664 ) ) ;
#37388 = CARTESIAN_POINT ( 'NONE',  ( -10.00000000000000000, 0.000000000000000000, 0.000000000000000000 ) ) ;
#37389 = CARTESIAN_POINT ( 'NONE',  ( -94.99999999999997158, -213.0599564267049857, 75.63312500173429953 ) ) ;
#37390 = CARTESIAN_POINT ( 'NONE',  ( 10.00000000000000000, 0.000000000000000000, 0.000000000000000000 ) ) ;
#37391 = EDGE_CURVE ( 'NONE', #15251, #18236, #41869, .T. ) ;
#37392 = EDGE_LOOP ( 'NONE', ( #55074, #24758, #19688, #27273 ) ) ;
#37394 = CARTESIAN_POINT ( 'NONE',  ( -96.15314808468751551, 88.00268892867056536, 88.47864583420047779 ) ) ;
#37393 = CARTESIAN_POINT ( 'NONE',  ( 96.32499999999998863, 87.70503267997126784, 75.68604166840097491 ) ) ;
#37395 =( BOUNDED_CURVE ( )  B_SPLINE_CURVE ( 2, ( #3269, #8134, #25798, #48362, #54743, #55109, #32542 ),
 .UNSPECIFIED., .F., .F. ) 
 B_SPLINE_CURVE_WITH_KNOTS ( ( 3, 2, 2, 3 ),
 ( 0.06350193517735322479, 0.07055765540882333320, 0.07761342094970606620, 0.08466915177892317401 ),
 .UNSPECIFIED. ) 
 CURVE ( )  GEOMETRIC_REPRESENTATION_ITEM ( )  RATIONAL_B_SPLINE_CURVE ( ( 0.9999982793443895623, 0.8660262641177686183, 1.000000000000000000, 0.8660254037844387076, 1.000000000000000000, 0.8660260628881687461, 0.9999986817990250687 ) ) 
 REPRESENTATION_ITEM ( '' )  );
#37396 = ORIENTED_EDGE ( 'NONE', *, *, #7386, .F. ) ;
#37397 = CARTESIAN_POINT ( 'NONE',  ( 94.99999999999998579, 87.33691857156068750, 75.35531250086715715 ) ) ;
#37398 = DIRECTION ( 'NONE',  ( 0.000000000000000000, 0.000000000000000000, 1.000000000000000000 ) ) ;
#37399 = DIRECTION ( 'NONE',  ( 0.000000000000000000, 0.8910065241883688980, -0.4539904997395445840 ) ) ;
#37400 = CARTESIAN_POINT ( 'NONE',  ( 92.35000000000000853, -209.9999999999999716, 77.37937500173428873 ) ) ;
#37401 = DIRECTION ( 'NONE',  ( -1.000000000000000000, 0.000000000000000000, -0.000000000000000000 ) ) ;
#37402 = ADVANCED_FACE ( 'NONE', ( #36968 ), #949, .F. ) ;
#37403 = DIRECTION ( 'NONE',  ( -0.000000000000000000, -0.000000000000000000, -1.000000000000000000 ) ) ;
#37404 = ORIENTED_EDGE ( 'NONE', *, *, #24556, .F. ) ;
#37405 = CARTESIAN_POINT ( 'NONE',  ( -8.452893869119503023, -12.51233732111638375, -1.199999999999999956 ) ) ;
#37406 = VECTOR ( 'NONE', #61060, 1000.000000000000000 ) ;
#37407 = CARTESIAN_POINT ( 'NONE',  ( 0.000000000000000000, -72.35160999960831418, 20.41045688087797672 ) ) ;
#37408 = ORIENTED_EDGE ( 'NONE', *, *, #58638, .F. ) ;
#37409 = AXIS2_PLACEMENT_3D ( 'NONE', #7434, #60426, #54769 ) ;
#37410 = VERTEX_POINT ( 'NONE', #48252 ) ;
#37411 = AXIS2_PLACEMENT_3D ( 'NONE', #21688, #49518, #16055 ) ;
#37412 = LINE ( 'NONE', #60339, #28304 ) ;
#37413 = DIRECTION ( 'NONE',  ( 0.000000000000000000, 0.000000000000000000, 1.000000000000000000 ) ) ;
#37414 = CARTESIAN_POINT ( 'NONE',  ( 0.000000000000000000, -37.22597642581153821, 10.79786254984320415 ) ) ;
#37415 = DIRECTION ( 'NONE',  ( 0.000000000000000000, 0.000000000000000000, -1.000000000000000000 ) ) ;
#37416 = DIRECTION ( 'NONE',  ( -1.000000000000000000, -0.000000000000000000, -0.000000000000000000 ) ) ;
#37417 = CARTESIAN_POINT ( 'NONE',  ( 0.000000000000000000, 74.65491531819105830, 8.830959090343693418 ) ) ;
#37418 = CIRCLE ( 'NONE', #28966, 31.99999999999999289 ) ;
#37419 = MANIFOLD_SOLID_BREP ( 'Boss-Extrude3', #2035 ) ;
#37420 = ORIENTED_EDGE ( 'NONE', *, *, #47066, .F. ) ;
#37421 = DIRECTION ( 'NONE',  ( 0.000000000000000000, 0.8090169943749445647, 0.5877852522924771339 ) ) ;
#37422 = DIRECTION ( 'NONE',  ( -0.000000000000000000, 0.000000000000000000, 1.000000000000000000 ) ) ;
#37423 = CARTESIAN_POINT ( 'NONE',  ( -97.65000000000001990, 90.00000000000004263, 79.20499999999999829 ) ) ;
#37424 = LINE ( 'NONE', #26114, #56104 ) ;
#37425 = DIRECTION ( 'NONE',  ( -1.000000000000000000, 0.000000000000000000, -0.000000000000000000 ) ) ;
#37426 = CARTESIAN_POINT ( 'NONE',  ( 96.32499999999998863, -207.7050326799711968, 80.34270833506762699 ) ) ;
#37427 = DIRECTION ( 'NONE',  ( 0.000000000000000000, 0.8090169943749432324, 0.5877852522924789103 ) ) ;
#37428 = CARTESIAN_POINT ( 'NONE',  ( 0.000000000000000000, 0.000000000000000000, 0.000000000000000000 ) ) ;
#37429 = CARTESIAN_POINT ( 'NONE',  ( 0.000000000000000000, 0.000000000000000000, 0.000000000000000000 ) ) ;
#37430 = CARTESIAN_POINT ( 'NONE',  ( 94.99999999999998579, 92.66308142843932671, 83.92781250086716227 ) ) ;
#37431 = CARTESIAN_POINT ( 'NONE',  ( -96.15314808468745866, -211.9973110713294489, 81.65239583420049030 ) ) ;
#37432 = CARTESIAN_POINT ( 'NONE',  ( 10.00000000000000000, 0.000000000000000000, 0.000000000000000000 ) ) ;
#37433 = ORIENTED_EDGE ( 'NONE', *, *, #70672, .F. ) ;
#37434 = FACE_OUTER_BOUND ( 'NONE', #42078, .T. ) ;
#37435 = UNCERTAINTY_MEASURE_WITH_UNIT (LENGTH_MEASURE( 1.000000000000000082E-05 ), #51404, 'distance_accuracy_value', 'NONE');
#37436 = AXIS2_PLACEMENT_3D ( 'NONE', #69924, #63571, #28224 ) ;
#37437 = CARTESIAN_POINT ( 'NONE',  ( -93.67499999999998295, -207.7050326799711968, 78.35833333333333428 ) ) ;
#37438 = ADVANCED_FACE ( 'NONE', ( #7658 ), #19666, .T. ) ;
#37439 = FACE_OUTER_BOUND ( 'NONE', #51799, .T. ) ;
#37440 = EDGE_CURVE ( 'NONE', #48661, #11723, #52401, .T. ) ;
#37441 = EDGE_CURVE ( 'NONE', #66307, #60509, #5487, .T. ) ;
#37442 = EDGE_CURVE ( 'NONE', #16864, #24357, #736, .T. ) ;
#37443 = CARTESIAN_POINT ( 'NONE',  ( 97.30629616937498838, -211.3315407142195852, 83.55739583420047722 ) ) ;
#37444 = ORIENTED_EDGE ( 'NONE', *, *, #10185, .F. ) ;
#37445 = DIRECTION ( 'NONE',  ( 0.000000000000000000, 0.000000000000000000, 1.000000000000000000 ) ) ;
#37446 = ORIENTED_EDGE ( 'NONE', *, *, #20110, .T. ) ;
#37447 = ORIENTED_EDGE ( 'NONE', *, *, #1597, .T. ) ;
#37448 = AXIS2_PLACEMENT_3D ( 'NONE', #62714, #28094, #27729 ) ;
#37449 = FACE_OUTER_BOUND ( 'NONE', #48226, .T. ) ;
#37450 = CIRCLE ( 'NONE', #2653, 16.00000000000000000 ) ;
#37451 = ADVANCED_FACE ( 'NONE', ( #6913 ), #47874, .T. ) ;
#37452 = VECTOR ( 'NONE', #12171, 999.9999999999998863 ) ;
#37453 = ORIENTED_EDGE ( 'NONE', *, *, #64889, .F. ) ;
#37454 = EDGE_CURVE ( 'NONE', #37974, #57971, #2058, .T. ) ;
#37455 = CARTESIAN_POINT ( 'NONE',  ( 92.69370383062501162, -208.6684592857803295, 77.68364583420047609 ) ) ;
#37456 = DIRECTION ( 'NONE',  ( -1.000000000000000000, 0.000000000000000000, -0.000000000000000000 ) ) ;
#37457 = CARTESIAN_POINT ( 'NONE',  ( 10.00000000000000000, 0.000000000000000000, 0.000000000000000000 ) ) ;
#37458 = DIRECTION ( 'NONE',  ( -1.000000000000000000, -0.000000000000000000, -0.000000000000000000 ) ) ;
#37459 = DIRECTION ( 'NONE',  ( -1.000000000000000000, -0.000000000000000000, -0.000000000000000000 ) ) ;
#37460 = FACE_OUTER_BOUND ( 'NONE', #36772, .T. ) ;
#37461 = CARTESIAN_POINT ( 'NONE',  ( 97.64999999999997726, -208.4700217866474645, 81.48041666666665606 ) ) ;
#37462 = VERTEX_POINT ( 'NONE', #64075 ) ;
#37463 = EDGE_LOOP ( 'NONE', ( #56708, #61014, #72541, #28308 ) ) ;
#37464 = ORIENTED_EDGE ( 'NONE', *, *, #57542, .F. ) ;
#37465 = ORIENTED_EDGE ( 'NONE', *, *, #67078, .T. ) ;
#37466 = CARTESIAN_POINT ( 'NONE',  ( 10.00000000000000000, 22.64427369931212297, -30.00120703465181293 ) ) ;
#37467 = ADVANCED_FACE ( 'NONE', ( #35484 ), #24221, .T. ) ;
#37468 = ADVANCED_FACE ( 'NONE', ( #64438 ), #18558, .T. ) ;
#37469 = CARTESIAN_POINT ( 'NONE',  ( -93.84685191531254134, 91.99731107132950569, 83.23989583420049598 ) ) ;
#37470 = DIRECTION ( 'NONE',  ( 0.000000000000000000, 0.000000000000000000, 1.000000000000000000 ) ) ;
#37471 = CARTESIAN_POINT ( 'NONE',  ( 0.000000000000000000, -50.95692526931287603, -58.39081064771804819 ) ) ;
#37472 = CARTESIAN_POINT ( 'NONE',  ( 97.64999999999997726, 91.52997821335252127, 75.76541666666666686 ) ) ;
#37473 = DIRECTION ( 'NONE',  ( 0.000000000000000000, 1.000000000000000000, 3.469446951953614189E-15 ) ) ;
#37474 = ORIENTED_EDGE ( 'NONE', *, *, #17594, .T. ) ;
#37475 = CARTESIAN_POINT ( 'NONE',  ( -92.34999999999999432, -209.9999999999999716, 87.22187500173430408 ) ) ;
#37476 = ORIENTED_EDGE ( 'NONE', *, *, #14589, .T. ) ;
#37477 = LINE ( 'NONE', #19787, #30237 ) ;
#37478 = VERTEX_POINT ( 'NONE', #14766 ) ;
#37479 = CARTESIAN_POINT ( 'NONE',  ( -93.67500000000003979, 92.29496732002878900, 82.88270833506763324 ) ) ;
#37480 = ORIENTED_EDGE ( 'NONE', *, *, #38718, .T. ) ;
#37481 = CARTESIAN_POINT ( 'NONE',  ( 94.99999999999998579, 92.66308142843935514, 85.19781250086714408 ) ) ;
#37482 = DIRECTION ( 'NONE',  ( -1.000000000000000000, 0.000000000000000000, 0.000000000000000000 ) ) ;
#37483 = CARTESIAN_POINT ( 'NONE',  ( -96.32500000000001705, 87.70503267997129626, 85.74020833506763495 ) ) ;
#37484 = CARTESIAN_POINT ( 'NONE',  ( 3.000000000000000000, 0.000000000000000000, 0.000000000000000000 ) ) ;
#37485 =( GEOMETRIC_REPRESENTATION_CONTEXT ( 3 ) GLOBAL_UNCERTAINTY_ASSIGNED_CONTEXT ( ( #20295 ) ) GLOBAL_UNIT_ASSIGNED_CONTEXT ( ( #44678, #5204, #39776 ) ) REPRESENTATION_CONTEXT ( 'NONE', 'WORKASPACE' ) );
#37486 = DIRECTION ( 'NONE',  ( -1.000000000000000000, 0.000000000000000000, 0.000000000000000000 ) ) ;
#37487 = ORIENTED_EDGE ( 'NONE', *, *, #46762, .F. ) ;
#37488 = DIRECTION ( 'NONE',  ( 0.000000000000000000, 0.9723699203976756689, 0.2334453638559094157 ) ) ;
#37489 = CARTESIAN_POINT ( 'NONE',  ( 2.499999999999979572, 80.00000000000000000, -280.0000000000000000 ) ) ;
#37490 = ORIENTED_EDGE ( 'NONE', *, *, #73825, .T. ) ;
#37491 = VECTOR ( 'NONE', #72885, 1000.000000000000000 ) ;
#37492 = ORIENTED_EDGE ( 'NONE', *, *, #27988, .T. ) ;
#37493 = CARTESIAN_POINT ( 'NONE',  ( 92.34999999999999432, 90.00001683226676619, 78.64937441956428188 ) ) ;
#37494 = CIRCLE ( 'NONE', #36235, 82.00000000000000000 ) ;
#37495 = CARTESIAN_POINT ( 'NONE',  ( 35.50000000000000711, -120.0000000000000000, 5.500000000000000000 ) ) ;
#37496 = DIRECTION ( 'NONE',  ( -1.000000000000000000, -0.000000000000000000, -0.000000000000000000 ) ) ;
#37497 = VECTOR ( 'NONE', #40906, 1000.000000000000000 ) ;
#37498 = CARTESIAN_POINT ( 'NONE',  ( -92.69370383062498320, -209.9999999999999716, 85.67406250086715147 ) ) ;
#37499 = ORIENTED_EDGE ( 'NONE', *, *, #16062, .F. ) ;
#37500 = CARTESIAN_POINT ( 'NONE',  ( 0.000000000000000000, 0.000000000000000000, -175.0000000000000000 ) ) ;
#37501 = ORIENTED_EDGE ( 'NONE', *, *, #57833, .T. ) ;
#37502 = CARTESIAN_POINT ( 'NONE',  ( 10.00000000000000000, 35.95386929396241271, 10.96151621346552751 ) ) ;
#37503 = AXIS2_PLACEMENT_3D ( 'NONE', #15174, #14437, #55402 ) ;
#37504 = DIRECTION ( 'NONE',  ( -0.000000000000000000, -0.9510565162951506446, -0.3090169943749562220 ) ) ;
#37505 = FACE_OUTER_BOUND ( 'NONE', #50436, .T. ) ;
#37506 = CARTESIAN_POINT ( 'NONE',  ( 97.30629616937498838, 88.66845928578035796, 76.57239583420046358 ) ) ;
#37507 = DIRECTION ( 'NONE',  ( -0.2306669878475648139, -0.9730327541852491491, 0.000000000000000000 ) ) ;
#37508 = CARTESIAN_POINT ( 'NONE',  ( 0.000000000000000000, -29.01471420065617224, 76.69515212746007649 ) ) ;
#37509 = CARTESIAN_POINT ( 'NONE',  ( 10.00000000000000000, -68.26794271651239399, -31.47745569255214093 ) ) ;
#37510 = DIRECTION ( 'NONE',  ( -1.000000000000000000, 0.000000000000000000, 0.000000000000000000 ) ) ;
#37511 = CYLINDRICAL_SURFACE ( 'NONE', #62875, 2.500000000000000000 ) ;
#37512 = CARTESIAN_POINT ( 'NONE',  ( 97.65000000000000568, -211.5299782133524502, 84.54958333333334508 ) ) ;
#37513 = CARTESIAN_POINT ( 'NONE',  ( -94.99999999999997158, -209.9999999999999716, 75.00000000000000000 ) ) ;
#37514 = CARTESIAN_POINT ( 'NONE',  ( 3.000000000000000000, -1.467624384280027838, 2.542000000000001592 ) ) ;
#37515 = ORIENTED_EDGE ( 'NONE', *, *, #34296, .T. ) ;
#37516 = EDGE_CURVE ( 'NONE', #14919, #41093, #4252, .T. ) ;
#37517 = CARTESIAN_POINT ( 'NONE',  ( -95.00000000000002842, 92.66308142843932671, 81.86406250086713499 ) ) ;
#37518 = FACE_OUTER_BOUND ( 'NONE', #73140, .T. ) ;
#37519 = EDGE_CURVE ( 'NONE', #70184, #62512, #72632, .T. ) ;
#37520 = ADVANCED_FACE ( 'NONE', ( #73005 ), #8768, .F. ) ;
#37521 = DIRECTION ( 'NONE',  ( -0.9827303690289285187, -0.1850432970638656860, 0.000000000000000000 ) ) ;
#37522 = ORIENTED_EDGE ( 'NONE', *, *, #17143, .F. ) ;
#37523 = EDGE_CURVE ( 'NONE', #23039, #65417, #24669, .T. ) ;
#37524 = DIRECTION ( 'NONE',  ( 1.000000000000000000, 0.000000000000000000, 0.000000000000000000 ) ) ;
#37525 = MANIFOLD_SOLID_BREP ( 'Cut-Extrude-Thin1', #35575 ) ;
#37526 = FACE_OUTER_BOUND ( 'NONE', #31281, .T. ) ;
#37527 = DIRECTION ( 'NONE',  ( -1.000000000000000000, 0.000000000000000000, 0.000000000000000000 ) ) ;
#37528 = PRESENTATION_LAYER_ASSIGNMENT (  '', '', ( #57968 ) ) ;
#37529 = DIRECTION ( 'NONE',  ( 0.000000000000000000, 0.000000000000000000, 1.000000000000000000 ) ) ;
#37530 = CARTESIAN_POINT ( 'NONE',  ( 97.30629616937498838, -209.9999999999999716, 79.32406250086715715 ) ) ;
#37531 = AXIS2_PLACEMENT_3D ( 'NONE', #35121, #29461, #6915 ) ;
#37532 = ORIENTED_EDGE ( 'NONE', *, *, #6720, .T. ) ;
#37533 = ORIENTED_EDGE ( 'NONE', *, *, #26636, .T. ) ;
#37534 = EDGE_CURVE ( 'NONE', #3726, #26049, #25685, .T. ) ;
#37535 = AXIS2_PLACEMENT_3D ( 'NONE', #4128, #9366, #27020 ) ;
#37536 = EDGE_CURVE ( 'NONE', #41131, #68149, #49887, .T. ) ;
#37537 = DIRECTION ( 'NONE',  ( -0.3311129884571280546, -0.9435911131814402886, 0.000000000000000000 ) ) ;
#37538 = DIRECTION ( 'NONE',  ( -1.000000000000000000, -0.000000000000000000, -0.000000000000000000 ) ) ;
#37539 = AXIS2_PLACEMENT_3D ( 'NONE', #9503, #55370, #3885 ) ;
#37540 = FACE_OUTER_BOUND ( 'NONE', #3281, .T. ) ;
#37541 = ORIENTED_EDGE ( 'NONE', *, *, #64442, .F. ) ;
#37542 = CARTESIAN_POINT ( 'NONE',  ( 92.35000000000000853, -209.9999999999999716, 90.00000000000000000 ) ) ;
#37543 = CARTESIAN_POINT ( 'NONE',  ( 96.66079198124938898, -211.6002412367799934, 74.80065669543249385 ) ) ;
#37544 = VERTEX_POINT ( 'NONE', #38072 ) ;
#37545 = DIRECTION ( 'NONE',  ( -0.000000000000000000, -0.000000000000000000, 1.000000000000000000 ) ) ;
#37546 = ORIENTED_EDGE ( 'NONE', *, *, #71173, .T. ) ;
#37547 = AXIS2_PLACEMENT_3D ( 'NONE', #55051, #4318, #21195 ) ;
#37548 = VERTEX_POINT ( 'NONE', #26421 ) ;
#37549 = CARTESIAN_POINT ( 'NONE',  ( -93.67499999999998295, -207.7050326799711968, 82.24770833506762813 ) ) ;
#37550 = EDGE_CURVE ( 'NONE', #58611, #26913, #9870, .T. ) ;
#37552 = ADVANCED_FACE ( 'NONE', ( #66652 ), #15132, .T. ) ;
#37551 = AXIS2_PLACEMENT_3D ( 'NONE', #4219, #73351, #72242 ) ;
#37553 = CARTESIAN_POINT ( 'NONE',  ( 5.999999999999999112, 33.71516098798849015, -74.74816331893393340 ) ) ;
#37554 = VERTEX_POINT ( 'NONE', #55734 ) ;
#37555 = CARTESIAN_POINT ( 'NONE',  ( 5.000000000000002665, 79.10210256391398786, -21.60688246758503084 ) ) ;
#37556 = CARTESIAN_POINT ( 'NONE',  ( 92.35000000000002274, -208.4700217866474645, 79.23145833506762870 ) ) ;
#37557 = CARTESIAN_POINT ( 'NONE',  ( 93.67499999999998295, 92.29496732002878900, 83.54416666666666913 ) ) ;
#37558 = VERTEX_POINT ( 'NONE', #21506 ) ;
#37559 = CARTESIAN_POINT ( 'NONE',  ( 52.50000000000002132, 7.041719095097282063E-15, -175.0000000000000000 ) ) ;
#37560 = CARTESIAN_POINT ( 'NONE',  ( 10.00000000000000000, -16.65560815589439159, 38.55633173627004595 ) ) ;
#37561 = ORIENTED_EDGE ( 'NONE', *, *, #12068, .T. ) ;
#37562 = ORIENTED_EDGE ( 'NONE', *, *, #13419, .T. ) ;
#37563 = CARTESIAN_POINT ( 'NONE',  ( -92.69370383062505425, 91.33154071421968467, 89.53697916753382913 ) ) ;
#37564 = CARTESIAN_POINT ( 'NONE',  ( 96.15314808468748708, 91.99731107132950569, 80.54114583420046358 ) ) ;
#37565 = ORIENTED_EDGE ( 'NONE', *, *, #25450, .F. ) ;
#37566 = CARTESIAN_POINT ( 'NONE',  ( 94.99999999999998579, 93.05995642670504253, 81.66562500173431260 ) ) ;
#37567 = DIRECTION ( 'NONE',  ( 0.000000000000000000, -0.2079116908177532363, -0.9781476007338069101 ) ) ;
#37568 = ORIENTED_EDGE ( 'NONE', *, *, #11301, .T. ) ;
#37569 = CARTESIAN_POINT ( 'NONE',  ( 15.00000000000000000, 5.835314593368777558, 22.81335362449846471 ) ) ;
#37570 = ORIENTED_EDGE ( 'NONE', *, *, #48491, .T. ) ;
#37571 = ORIENTED_EDGE ( 'NONE', *, *, #66459, .T. ) ;
#37572 = EDGE_LOOP ( 'NONE', ( #66786, #50870, #34208, #24579 ) ) ;
#37573 = CARTESIAN_POINT ( 'NONE',  ( 92.34999999999999432, 89.99998767024830215, 75.47437542817786493 ) ) ;
#37574 = CARTESIAN_POINT ( 'NONE',  ( -96.32500000000001705, 87.70503267997129626, 85.02583333333332405 ) ) ;
#37575 = ORIENTED_EDGE ( 'NONE', *, *, #15261, .F. ) ;
#37576 = DIRECTION ( 'NONE',  ( 0.000000000000000000, 0.7071067811865436870, 0.7071067811865512365 ) ) ;
#37577 = DIRECTION ( 'NONE',  ( -0.7273375899149812085, 0.6862798483830533369, 0.000000000000000000 ) ) ;
#37578 = ORIENTED_EDGE ( 'NONE', *, *, #57967, .F. ) ;
#37579 = CARTESIAN_POINT ( 'NONE',  ( 10.00000000000000000, 21.53537804866081373, 30.80686688397018358 ) ) ;
#37580 = CARTESIAN_POINT ( 'NONE',  ( -93.84685191531248449, -208.0026889286704943, 79.27114583420046756 ) ) ;
#37581 = VERTEX_POINT ( 'NONE', #9498 ) ;
#37582 = DIRECTION ( 'NONE',  ( -1.000000000000000000, -0.000000000000000000, -0.000000000000000000 ) ) ;
#37583 = DIRECTION ( 'NONE',  ( -1.000000000000000000, 0.000000000000000000, 0.000000000000000000 ) ) ;
#37584 = CARTESIAN_POINT ( 'NONE',  ( 11.99999999999999822, 2.543863470248389103, 81.96053171279902472 ) ) ;
#37585 = DIRECTION ( 'NONE',  ( -1.000000000000000000, 0.000000000000000000, -0.000000000000000000 ) ) ;
#37586 = AXIS2_PLACEMENT_3D ( 'NONE', #65952, #2819, #36250 ) ;
#37587 = FACE_BOUND ( 'NONE', #20255, .T. ) ;
#37588 = VECTOR ( 'NONE', #64622, 1000.000000000000000 ) ;
#37589 = LINE ( 'NONE', #3388, #9685 ) ;
#37590 = CARTESIAN_POINT ( 'NONE',  ( 93.84685191531248449, 91.99731107132950569, 86.99697916753380866 ) ) ;
#37591 = EDGE_CURVE ( 'NONE', #31970, #12223, #44467, .T. ) ;
#37592 = CARTESIAN_POINT ( 'NONE',  ( -12.49999999999999645, 0.000000000000000000, 20.00000000000000000 ) ) ;
#37593 = CARTESIAN_POINT ( 'NONE',  ( 11.99999999999999822, 3.894527615417885169, 81.90746397400390322 ) ) ;
#37594 = EDGE_CURVE ( 'NONE', #55761, #15852, #70269, .T. ) ;
#37595 = DIRECTION ( 'NONE',  ( 0.000000000000000000, 0.000000000000000000, 1.000000000000000000 ) ) ;
#37596 = CARTESIAN_POINT ( 'NONE',  ( 10.00000000000000000, -76.66974797899830207, -11.30684508768422170 ) ) ;
#37597 = DIRECTION ( 'NONE',  ( 7.705842312279274921E-15, -1.000000000000000000, 2.546204323184492723E-14 ) ) ;
#37598 = EDGE_CURVE ( 'NONE', #7305, #1988, #55366, .T. ) ;
#37599 = VECTOR ( 'NONE', #49712, 1000.000000000000000 ) ;
#37600 =( BOUNDED_CURVE ( )  B_SPLINE_CURVE ( 2, ( #38780, #61716, #10199, #16586, #27487, #33491, #10567 ),
 .UNSPECIFIED., .F., .F. ) 
 B_SPLINE_CURVE_WITH_KNOTS ( ( 3, 2, 2, 3 ),
 ( 0.6875000000000000000, 0.6944444444444443088, 0.7013888888888887285, 0.7083333333333331483 ),
 .UNSPECIFIED. ) 
 CURVE ( )  GEOMETRIC_REPRESENTATION_ITEM ( )  RATIONAL_B_SPLINE_CURVE ( ( 1.000000000000000000, 0.8660254037844387076, 1.000000000000000000, 0.8660254037844387076, 1.000000000000000000, 0.8660254037844430375, 0.9999999999999956701 ) ) 
 REPRESENTATION_ITEM ( '' )  );
#37601 = DIRECTION ( 'NONE',  ( -1.000000000000000000, -0.000000000000000000, -0.000000000000000000 ) ) ;
#37602 = AXIS2_PLACEMENT_3D ( 'NONE', #3495, #66989, #72258 ) ;
#37603 = LINE ( 'NONE', #20668, #32796 ) ;
#37604 = ADVANCED_FACE ( 'NONE', ( #48619 ), #14402, .F. ) ;
#37605 = UNCERTAINTY_MEASURE_WITH_UNIT (LENGTH_MEASURE( 1.000000000000000082E-05 ), #34955, 'distance_accuracy_value', 'NONE');
#37606 = CARTESIAN_POINT ( 'NONE',  ( 11.99999999999999822, -44.88180994100329713, -63.18004540533077318 ) ) ;
#37607 = DIRECTION ( 'NONE',  ( 0.000000000000000000, 0.9510565162951544194, -0.3090169943749446757 ) ) ;
#37608 = CIRCLE ( 'NONE', #5203, 3.299999999999969624 ) ;
#37609 = DIRECTION ( 'NONE',  ( -1.000000000000000000, -0.000000000000000000, -0.000000000000000000 ) ) ;
#37610 = ADVANCED_FACE ( 'NONE', ( #34653 ), #40296, .T. ) ;
#37611 = DIRECTION ( 'NONE',  ( -1.000000000000000000, -0.000000000000000000, -0.000000000000000000 ) ) ;
#37612 = CARTESIAN_POINT ( 'NONE',  ( -97.64999999999994884, -211.5299782133524502, 88.14791666666666003 ) ) ;
#37613 = CARTESIAN_POINT ( 'NONE',  ( -93.33265519076742578, 87.91120745868269637, 75.00000000000000000 ) ) ;
#37614 = VERTEX_POINT ( 'NONE', #73383 ) ;
#37615 = EDGE_CURVE ( 'NONE', #26264, #5742, #22324, .T. ) ;
#37616 = LINE ( 'NONE', #66553, #44322 ) ;
#37617 = LINE ( 'NONE', #66909, #44294 ) ;
#37618 = DIRECTION ( 'NONE',  ( -1.000000000000000000, 0.000000000000000000, 0.000000000000000000 ) ) ;
#37619 = ORIENTED_EDGE ( 'NONE', *, *, #19758, .T. ) ;
#37620 = VERTEX_POINT ( 'NONE', #51941 ) ;
#37621 = EDGE_CURVE ( 'NONE', #41342, #30420, #73937, .T. ) ;
#37622 = LINE ( 'NONE', #55272, #4728 ) ;
#37623 = EDGE_CURVE ( 'NONE', #54593, #69330, #63243, .T. ) ;
#37624 = FACE_OUTER_BOUND ( 'NONE', #48394, .T. ) ;
#37625 = VERTEX_POINT ( 'NONE', #10989 ) ;
#37626 = AXIS2_PLACEMENT_3D ( 'NONE', #6268, #63053, #34078 ) ;
#37627 = CARTESIAN_POINT ( 'NONE',  ( 92.69370383062501162, -208.6684592857803295, 80.06489583420047040 ) ) ;
#37628 = CARTESIAN_POINT ( 'NONE',  ( 92.69370383062501162, -208.6684592857803295, 86.57364583420047666 ) ) ;
#37629 = VERTEX_POINT ( 'NONE', #68128 ) ;
#37630 = CARTESIAN_POINT ( 'NONE',  ( 95.00000000000000000, -207.3369185715606307, 85.19781250086714408 ) ) ;
#37631 = ORIENTED_EDGE ( 'NONE', *, *, #71010, .F. ) ;
#37632 = DIRECTION ( 'NONE',  ( 0.000000000000000000, 0.000000000000000000, 1.000000000000000000 ) ) ;
#37633 = ORIENTED_EDGE ( 'NONE', *, *, #57980, .F. ) ;
#37634 = CARTESIAN_POINT ( 'NONE',  ( -96.15314808468751551, 88.00268892867056536, 78.47739583420049314 ) ) ;
#37635 = AXIS2_PLACEMENT_3D ( 'NONE', #30310, #31425, #54731 ) ;
#37636 = ORIENTED_EDGE ( 'NONE', *, *, #63123, .T. ) ;
#37637 = ORIENTED_EDGE ( 'NONE', *, *, #61371, .F. ) ;
#37638 = DIRECTION ( 'NONE',  ( -1.000000000000000000, 0.000000000000000000, -0.000000000000000000 ) ) ;
#37639 = ORIENTED_EDGE ( 'NONE', *, *, #30474, .F. ) ;
#37640 = CARTESIAN_POINT ( 'NONE',  ( 0.000000000000000000, 0.000000000000000000, 0.000000000000000000 ) ) ;
#37641 = CARTESIAN_POINT ( 'NONE',  ( 0.000000000000000000, 37.48860685352291000, 0.8828120875901893649 ) ) ;
#37642 = EDGE_LOOP ( 'NONE', ( #27995, #32537, #28455, #69435 ) ) ;
#37643 = CARTESIAN_POINT ( 'NONE',  ( 0.000000000000000000, 0.000000000000000000, 0.000000000000000000 ) ) ;
#37644 = AXIS2_PLACEMENT_3D ( 'NONE', #33261, #41061, #28374 ) ;
#37645 = VERTEX_POINT ( 'NONE', #23021 ) ;
#37646 = DIRECTION ( 'NONE',  ( 1.000000000000000000, 0.000000000000000000, 0.000000000000000000 ) ) ;
#37647 = AXIS2_PLACEMENT_3D ( 'NONE', #41214, #35932, #7737 ) ;
#37648 = ORIENTED_EDGE ( 'NONE', *, *, #60536, .F. ) ;
#37649 = ORIENTED_EDGE ( 'NONE', *, *, #59532, .F. ) ;
#37650 = AXIS2_PLACEMENT_3D ( 'NONE', #14557, #48769, #31102 ) ;
#37651 = ORIENTED_EDGE ( 'NONE', *, *, #66868, .F. ) ;
#37652 = CARTESIAN_POINT ( 'NONE',  ( 96.15314808468748708, -208.0026889286704943, 79.90614583420047268 ) ) ;
#37653 = VECTOR ( 'NONE', #67278, 1000.000000000000000 ) ;
#37654 = DIRECTION ( 'NONE',  ( 0.000000000000000000, 0.000000000000000000, 1.000000000000000000 ) ) ;
#37655 = AXIS2_PLACEMENT_3D ( 'NONE', #27699, #50623, #5163 ) ;
#37656 = ITEM_DEFINED_TRANSFORMATION ( 'NONE', 'NONE', #23200,  #43395 ) ;
#37657 = CYLINDRICAL_SURFACE ( 'NONE', #30590, 82.00000000000000000 ) ;
#37658 = EDGE_LOOP ( 'NONE', ( #64114, #31063, #46073, #31334 ) ) ;
#37659 = ORIENTED_EDGE ( 'NONE', *, *, #31323, .T. ) ;
#37660 = CARTESIAN_POINT ( 'NONE',  ( -93.67500000000003979, 87.70503267997129626, 80.68666666666665321 ) ) ;
#37661 = ORIENTED_EDGE ( 'NONE', *, *, #70796, .T. ) ;
#37662 = DIRECTION ( 'NONE',  ( 1.000000000000000000, 0.000000000000000000, 0.000000000000000000 ) ) ;
#37663 = DIRECTION ( 'NONE',  ( -1.000000000000000000, 0.000000000000000000, 0.000000000000000000 ) ) ;
#37664 = CARTESIAN_POINT ( 'NONE',  ( -92.69370383062502583, 91.33154071421968467, 78.74197916753382742 ) ) ;
#37665 = EDGE_CURVE ( 'NONE', #8585, #24685, #57109, .T. ) ;
#37666 = VERTEX_POINT ( 'NONE', #23385 ) ;
#37667 = CARTESIAN_POINT ( 'NONE',  ( 92.69370383062498320, 91.33154071421968467, 76.25489583420049655 ) ) ;
#37668 = ORIENTED_EDGE ( 'NONE', *, *, #72526, .T. ) ;
#37669 = PLANE ( 'NONE',  #1127 ) ;
#37670 = DIRECTION ( 'NONE',  ( 0.000000000000000000, -0.7604059656000369261, 0.6494480483301766638 ) ) ;
#37671 = CARTESIAN_POINT ( 'NONE',  ( 97.65000000000000568, 88.47002178664752137, 77.64395833506762301 ) ) ;
#37672 = CARTESIAN_POINT ( 'NONE',  ( 92.35000000039376289, -209.9999706925934504, 76.74344264317686282 ) ) ;
#37673 = CARTESIAN_POINT ( 'NONE',  ( 0.000000000000000000, 33.79645857604513992, 16.45098606841138178 ) ) ;
#37674 = CARTESIAN_POINT ( 'NONE',  ( -92.69370383062498320, -211.3315407142195852, 83.55739583420047722 ) ) ;
#37675 = VECTOR ( 'NONE', #58735, 1000.000000000000000 ) ;
#37676 = LINE ( 'NONE', #30168, #44586 ) ;
#37677 = CARTESIAN_POINT ( 'NONE',  ( 0.000000000000000000, -35.53030884539094103, 12.26510123303246935 ) ) ;
#37678 = CARTESIAN_POINT ( 'NONE',  ( 11.99999999999999822, -10.30890764327441289, 81.34940948281332851 ) ) ;
#37679 = EDGE_LOOP ( 'NONE', ( #30046, #72119, #53078, #47672 ) ) ;
#37680 = ORIENTED_EDGE ( 'NONE', *, *, #63437, .F. ) ;
#37681 = CARTESIAN_POINT ( 'NONE',  ( -26.53422223201112828, -120.6595836127786043, 5.500000000000000000 ) ) ;
#37682 = ADVANCED_FACE ( 'NONE', ( #11707 ), #40674, .T. ) ;
#37683 = CARTESIAN_POINT ( 'NONE',  ( 0.000000000000000000, 59.75363087400153006, -56.15606465354897381 ) ) ;
#37684 = EDGE_CURVE ( 'NONE', #20714, #54372, #4627, .T. ) ;
#37685 = DIRECTION ( 'NONE',  ( -1.000000000000000000, -0.000000000000000000, -0.000000000000000000 ) ) ;
#37686 = CARTESIAN_POINT ( 'NONE',  ( -97.30629616937501680, 91.33154071421968467, 85.77989583420048803 ) ) ;
#37687 = CARTESIAN_POINT ( 'NONE',  ( -96.90895014231831794, -208.4386293813703901, 74.88237134757153513 ) ) ;
#37688 = FACE_OUTER_BOUND ( 'NONE', #9530, .T. ) ;
#37689 = VECTOR ( 'NONE', #74340, 1000.000000000000000 ) ;
#37690 = ORIENTED_EDGE ( 'NONE', *, *, #31391, .T. ) ;
#37691 = CARTESIAN_POINT ( 'NONE',  ( -0.2999999999999964362, 0.000000000000000000, 0.000000000000000000 ) ) ;
#37692 = VECTOR ( 'NONE', #24205, 1000.000000000000000 ) ;
#37693 = ADVANCED_FACE ( 'NONE', ( #57602 ), #27897, .F. ) ;
#37694 = ADVANCED_FACE ( 'NONE', ( #488 ), #44836, .T. ) ;
#37695 = CARTESIAN_POINT ( 'NONE',  ( 97.64999999999999147, 89.99999998014077107, 85.95187500101400246 ) ) ;
#37696 = DIRECTION ( 'NONE',  ( -1.000000000000000000, 0.000000000000000000, -0.000000000000000000 ) ) ;
#37697 = VECTOR ( 'NONE', #32614, 1000.000000000000000 ) ;
#37698 = DIRECTION ( 'NONE',  ( 0.000000000000000000, 0.000000000000000000, 1.000000000000000000 ) ) ;
#37699 = CARTESIAN_POINT ( 'NONE',  ( -2.381231458764688558, 4.398698068175660225, -0.5078976954042897507 ) ) ;
#37700 = CARTESIAN_POINT ( 'NONE',  ( 93.67500000000001137, -212.2949673200287179, 82.48583333333333201 ) ) ;
#37701 = CARTESIAN_POINT ( 'NONE',  ( -97.30629616937497417, -208.6684592857803011, 81.49364583420047836 ) ) ;
#37702 = SURFACE_SIDE_STYLE ('',( #19283 ) ) ;
#37703 = DIRECTION ( 'NONE',  ( 0.000000000000000000, 0.9135454576426058626, 0.4067366430757889950 ) ) ;
#37704 = CONICAL_SURFACE ( 'NONE', #67693, 17.45460580326810174, 1.361356816555583826 ) ;
#37705 = VECTOR ( 'NONE', #940, 1000.000000000000114 ) ;
#37706 = ADVANCED_FACE ( 'NONE', ( #10234 ), #62511, .F. ) ;
#37707 = CARTESIAN_POINT ( 'NONE',  ( 10.00000000000000000, -0.6853352020787742971, -37.58145647212455032 ) ) ;
#37708 = CARTESIAN_POINT ( 'NONE',  ( 3.250000000000000444, -13.95926121303099343, -1.199999999999999956 ) ) ;
#37709 = LINE ( 'NONE', #3142, #30945 ) ;
#37710 = VERTEX_POINT ( 'NONE', #27526 ) ;
#37711 = DIRECTION ( 'NONE',  ( -1.000000000000000000, -0.000000000000000000, 0.000000000000000000 ) ) ;
#37712 = CARTESIAN_POINT ( 'NONE',  ( 10.00000000000000000, 15.33399622253600292, -80.55351364060572905 ) ) ;
#37713 = CARTESIAN_POINT ( 'NONE',  ( 0.000000000000000000, 1.467624384280025174, -2.542000000000001592 ) ) ;
#37714 = CIRCLE ( 'NONE', #28084, 77.49899999999999523 ) ;
#37715 = CIRCLE ( 'NONE', #61692, 16.00000000000000000 ) ;
#37716 = DIRECTION ( 'NONE',  ( -1.000000000000000000, 0.000000000000000000, 0.000000000000000000 ) ) ;
#37717 = ORIENTED_EDGE ( 'NONE', *, *, #58135, .F. ) ;
#37718 = EDGE_CURVE ( 'NONE', #13389, #40893, #5367, .T. ) ;
#37719 = LINE ( 'NONE', #20776, #24038 ) ;
#37720 = DIRECTION ( 'NONE',  ( 0.8541291221503265474, -0.5200609990133007177, 0.000000000000000000 ) ) ;
#37721 = ORIENTED_EDGE ( 'NONE', *, *, #6798, .T. ) ;
#37722 = LINE ( 'NONE', #59918, #44831 ) ;
#37723 = ADVANCED_FACE ( 'NONE', ( #74131 ), #22640, .T. ) ;
#37724 = VERTEX_POINT ( 'NONE', #68878 ) ;
#37725 = ORIENTED_EDGE ( 'NONE', *, *, #53060, .T. ) ;
#37726 = DIRECTION ( 'NONE',  ( 0.000000000000000000, 0.8526401643540897357, 0.5224985647159527957 ) ) ;
#37727 = ORIENTED_EDGE ( 'NONE', *, *, #41679, .T. ) ;
#37728 = VERTEX_POINT ( 'NONE', #39937 ) ;
#37729 = VERTEX_POINT ( 'NONE', #11344 ) ;
#37730 = VERTEX_POINT ( 'NONE', #34279 ) ;
#37731 = LINE ( 'NONE', #20048, #34738 ) ;
#37732 = ORIENTED_EDGE ( 'NONE', *, *, #69096, .T. ) ;
#37733 = VECTOR ( 'NONE', #72424, 1000.000000000000000 ) ;
#37734 = VERTEX_POINT ( 'NONE', #57224 ) ;
#37735 = CARTESIAN_POINT ( 'NONE',  ( 96.15314808468748708, 88.00268892867053694, 75.40822916753381833 ) ) ;
#37736 = CARTESIAN_POINT ( 'NONE',  ( 11.99999999999999822, -0.8261519478425843888, -77.49459641780887864 ) ) ;
#37737 = DIRECTION ( 'NONE',  ( -7.632783294297813165E-16, -1.065814103640131188E-14, -1.000000000000000000 ) ) ;
#37738 = ORIENTED_EDGE ( 'NONE', *, *, #70927, .T. ) ;
#37739 = VERTEX_POINT ( 'NONE', #5735 ) ;
#37740 = ORIENTED_EDGE ( 'NONE', *, *, #134, .T. ) ;
#37741 = CARTESIAN_POINT ( 'NONE',  ( 94.99999999999998579, 92.66308142843935514, 88.84906250086713442 ) ) ;
#37742 = ORIENTED_EDGE ( 'NONE', *, *, #12053, .T. ) ;
#37743 = CARTESIAN_POINT ( 'NONE',  ( 92.69370383062501162, -209.9999999999999716, 89.64281250086713726 ) ) ;
#37744 = DIRECTION ( 'NONE',  ( 1.000000000000000000, 0.000000000000000000, 0.000000000000000000 ) ) ;
#37745 = DIRECTION ( 'NONE',  ( -1.000000000000000000, 0.000000000000000000, 0.000000000000000000 ) ) ;
#37746 = CARTESIAN_POINT ( 'NONE',  ( 10.00000000000000000, 0.000000000000000000, 0.000000000000000000 ) ) ;
#37747 = CARTESIAN_POINT ( 'NONE',  ( 10.00000000000000000, 22.90783923731629912, 78.73519480814962890 ) ) ;
#37748 = CARTESIAN_POINT ( 'NONE',  ( 10.00000000000000000, 0.000000000000000000, 0.000000000000000000 ) ) ;
#37749 = CARTESIAN_POINT ( 'NONE',  ( 10.00000000000000000, 0.000000000000000000, 0.000000000000000000 ) ) ;
#37750 = CARTESIAN_POINT ( 'NONE',  ( -7.500000000000015099, -73.00000000000001421, -204.9999999999999716 ) ) ;
#37751 = CARTESIAN_POINT ( 'NONE',  ( -93.67499999999998295, -207.7050326799711968, 77.16770833506762983 ) ) ;
#37752 = CARTESIAN_POINT ( 'NONE',  ( -93.84685191531252713, 88.00268892867056536, 88.10822916753382117 ) ) ;
#37753 = EDGE_LOOP ( 'NONE', ( #13403, #56018, #18885, #43282 ) ) ;
#37754 = UNCERTAINTY_MEASURE_WITH_UNIT (LENGTH_MEASURE( 1.000000000000000082E-05 ), #47260, 'distance_accuracy_value', 'NONE');
#37755 = ADVANCED_FACE ( 'NONE', ( #17364 ), #30480, .F. ) ;
#37757 = CARTESIAN_POINT ( 'NONE',  ( -95.00000000000002842, 92.66308142843932671, 88.84906250086713442 ) ) ;
#37756 = CARTESIAN_POINT ( 'NONE',  ( 92.69370383062498320, 90.00000000000002842, 86.46781250086714010 ) ) ;
#37758 = ORIENTED_EDGE ( 'NONE', *, *, #24271, .T. ) ;
#37759 = CARTESIAN_POINT ( 'NONE',  ( 92.69370383062498320, 88.66845928578037217, 76.51947916753381662 ) ) ;
#37760 = CARTESIAN_POINT ( 'NONE',  ( 11.99999999999999822, 0.000000000000000000, 0.000000000000000000 ) ) ;
#37761 = CARTESIAN_POINT ( 'NONE',  ( 92.35000000000000853, -211.5299782133524218, 87.51291666666666913 ) ) ;
#37762 = CARTESIAN_POINT ( 'NONE',  ( 0.000000000000000000, 0.000000000000000000, 0.000000000000000000 ) ) ;
#37763 = DIRECTION ( 'NONE',  ( -0.6862798483830533369, -0.7273375899149812085, 0.000000000000000000 ) ) ;
#37764 = DIRECTION ( 'NONE',  ( 0.000000000000000000, -0.5877852522924625900, -0.8090169943749551118 ) ) ;
#37766 = DIRECTION ( 'NONE',  ( -1.000000000000000000, 0.000000000000000000, 0.000000000000000000 ) ) ;
#37765 = CIRCLE ( 'NONE', #1623, 31.99999999999999645 ) ;
#37767 = CIRCLE ( 'NONE', #41352, 82.00000000000000000 ) ;
#37768 = CARTESIAN_POINT ( 'NONE',  ( 0.000000000000000000, 6.736453364084091788, -36.88895765772625879 ) ) ;
#37769 = ORIENTED_EDGE ( 'NONE', *, *, #25057, .T. ) ;
#37770 = EDGE_CURVE ( 'NONE', #14685, #11557, #46680, .T. ) ;
#37771 = VERTEX_POINT ( 'NONE', #23739 ) ;
#37772 = EDGE_CURVE ( 'NONE', #26530, #63730, #29545, .T. ) ;
#37773 = CIRCLE ( 'NONE', #1788, 42.00000000000000000 ) ;
#37774 = CARTESIAN_POINT ( 'NONE',  ( -92.35000000000005116, 91.52997821335253548, 80.84541666666666515 ) ) ;
#37775 = CARTESIAN_POINT ( 'NONE',  ( 0.000000000000000000, -73.44644590900077219, 24.73286445877677764 ) ) ;
#37776 = DIRECTION ( 'NONE',  ( -1.000000000000000000, -0.000000000000000000, -0.000000000000000000 ) ) ;
#37777 = DIRECTION ( 'NONE',  ( 0.000000000000000000, -0.9781476007338065770, -0.2079116908177544853 ) ) ;
#37778 = VECTOR ( 'NONE', #8204, 1000.000000000000000 ) ;
#37779 = FACE_OUTER_BOUND ( 'NONE', #52145, .T. ) ;
#37780 = CARTESIAN_POINT ( 'NONE',  ( -92.35000000000400178, 89.99999541993113894, 76.42687486206344261 ) ) ;
#37781 = FACE_OUTER_BOUND ( 'NONE', #39896, .T. ) ;
#37782 = MANIFOLD_SOLID_BREP ( 'Revolve1', #44012 ) ;
#37783 = VERTEX_POINT ( 'NONE', #1961 ) ;
#37784 = CARTESIAN_POINT ( 'NONE',  ( -95.00000000000002842, 92.66308142843932671, 81.22906250086715829 ) ) ;
#37785 = EDGE_CURVE ( 'NONE', #68051, #66576, #12746, .T. ) ;
#37786 = CARTESIAN_POINT ( 'NONE',  ( 12.49999999999999822, -120.0000000000000000, 125.0000000000000000 ) ) ;
#37787 = CARTESIAN_POINT ( 'NONE',  ( 0.000000000000000000, -18.13022148937243472, -15.02647892043568767 ) ) ;
#37788 = CARTESIAN_POINT ( 'NONE',  ( -92.35000000000006537, 90.00000034979574082, 77.69687501385438111 ) ) ;
#37789 = CARTESIAN_POINT ( 'NONE',  ( -19.90058851926621131, -132.5883508287165853, 5.500000000000000000 ) ) ;
#37790 = DIRECTION ( 'NONE',  ( 1.000000000000000000, 0.000000000000000000, 0.000000000000000000 ) ) ;
#37791 = DIRECTION ( 'NONE',  ( 0.000000000000000000, 0.000000000000000000, 1.000000000000000000 ) ) ;
#37792 = DIRECTION ( 'NONE',  ( 0.000000000000000000, 0.000000000000000000, 1.000000000000000000 ) ) ;
#37793 = DIRECTION ( 'NONE',  ( -1.000000000000000000, 0.000000000000000000, 0.000000000000000000 ) ) ;
#37794 = EDGE_CURVE ( 'NONE', #18706, #39724, #58380, .T. ) ;
#37795 = ADVANCED_FACE ( 'NONE', ( #52684 ), #47060, .T. ) ;
#37796 = CARTESIAN_POINT ( 'NONE',  ( 94.99999999999998579, 87.33691857156068750, 79.16531250086715943 ) ) ;
#37797 = EDGE_CURVE ( 'NONE', #57437, #13520, #70698, .T. ) ;
#37798 = CARTESIAN_POINT ( 'NONE',  ( -97.30629616937497417, -211.3315407142195852, 82.86947916753379673 ) ) ;
#37799 = CARTESIAN_POINT ( 'NONE',  ( -20.30386590532152979, -102.9045904027214959, 5.500000000000000000 ) ) ;
#37800 = ORIENTED_EDGE ( 'NONE', *, *, #18727, .F. ) ;
#37801 = LINE ( 'NONE', #72363, #2894 ) ;
#37802 = CARTESIAN_POINT ( 'NONE',  ( -94.99999999999997158, -213.0599564267049857, 76.82374999999998977 ) ) ;
#37803 = DIRECTION ( 'NONE',  ( -1.000000000000000000, 0.000000000000000000, 0.000000000000000000 ) ) ;
#37804 = ADVANCED_FACE ( 'NONE', ( #64348 ), #30112, .T. ) ;
#37805 = AXIS2_PLACEMENT_3D ( 'NONE', #39778, #11552, #11195 ) ;
#37806 = CARTESIAN_POINT ( 'NONE',  ( 95.00000000000000000, -212.6630814284392557, 82.81656250086713555 ) ) ;
#37807 = ORIENTED_EDGE ( 'NONE', *, *, #46423, .T. ) ;
#37808 = ADVANCED_FACE ( 'NONE', ( #59442 ), #53063, .T. ) ;
#37809 = DIRECTION ( 'NONE',  ( -0.2079116908177431888, 1.197885328332322634E-16, -0.9781476007338091305 ) ) ;
#37810 = ORIENTED_EDGE ( 'NONE', *, *, #28203, .T. ) ;
#37811 = AXIS2_PLACEMENT_3D ( 'NONE', #39721, #28046, #20925 ) ;
#37812 = DIRECTION ( 'NONE',  ( 0.000000000000000000, 0.000000000000000000, 1.000000000000000000 ) ) ;
#37813 = AXIS2_PLACEMENT_3D ( 'NONE', #29040, #63649, #12118 ) ;
#37814 = EDGE_LOOP ( 'NONE', ( #62826, #73441 ) ) ;
#37815 = LINE ( 'NONE', #72374, #52758 ) ;
#37816 = CIRCLE ( 'NONE', #64227, 31.99999999999998224 ) ;
#37817 = EDGE_LOOP ( 'NONE', ( #71731, #33544, #25053, #64458, #52185, #29307 ) ) ;
#37818 = CARTESIAN_POINT ( 'NONE',  ( 97.30629616937498838, -208.6684592857803295, 79.37697916753381833 ) ) ;
#37819 = CARTESIAN_POINT ( 'NONE',  ( -10.00000000000000000, 0.000000000000000000, 0.000000000000000000 ) ) ;
#37820 = CYLINDRICAL_SURFACE ( 'NONE', #49596, 77.49899999999999523 ) ;
#37821 = CARTESIAN_POINT ( 'NONE',  ( -97.40333747838809586, 89.15460556225126254, 74.93511027845775629 ) ) ;
#37822 =( BOUNDED_CURVE ( )  B_SPLINE_CURVE ( 2, ( #2708, #1965, #59081, #14312, #47782, #71441, #25589, #13201, #13565, #54536, #70702, #42897, #7569, #3065, #19210, #35751, #18831, #70327, #65463, #36495, #42160, #37259, #7199, #65093, #59445, #36868, #7931, #19941, #30845, #60198, #71071, #65825, #53793, #36131, #53066, #30484, #1601, #18468, #8682, #41410, #64351, #19572, #2342, #31593, #47421, #12823, #48161, #24487, #58702, #42521, #13928, #30117, #41773, #64718, #59818, #8306, #26334, #61664, #5558, #15047, #15413, #37628, #55645, #33073, #26692, #17191, #54903, #21415, #57051, #10149, #45784, #44375, #57415, #28458, #60917, #51390, #74329, #22843, #9786, #67302, #15800, #28836, #68706, #49993, #40123, #43281, #38735, #21054, #63078, #44005, #66204, #61297, #11535, #72186, #14679, #9407, #32333, #34471, #38361, #32699, #60563, #49619, #55277, #72548, #37986, #5927, #9041, #72911, #20693, #31962, #71810, #3426, #27060, #20323, #49260, #43644, #66567, #3797, #66918, #4163, #18654, #52883, #63807, #1425, #70514, #40871, #29190, #12277, #41594, #69792, #51772, #17924, #40487, #23942, #47241, #24673, #58149, #41228, #17554, #19026, #36320, #35213, #58514, #52134, #53251, #1790, #64910, #6647, #24313, #64534, #679, #35578, #13391, #7758, #70150, #7008, #7394, #13014, #29556, #59260, #47604, #316, #23565, #35948, #52494, #46498, #69425, #41977, #58899, #46878, #30305, #23209, #63436, #1051, #46138, #69068, #11907, #34850, #12646, #57788, #18291, #29932, #64172, #6292, #19398, #59633, #66393, #60748, #42345, #70897, #42710, #14118, #53999, #65282, #25782, #30671, #38174, #37818, #48343, #13753, #15238, #66023, #54727, #36692, #53612, #8117, #14496, #60018, #37069, #66752, #8502, #20517, #14872, #2538, #31420, #54362, #2887, #31045, #25423, #9225, #61118, #71256, #55091, #19763, #3253, #48713, #25044, #32148, #65645, #37455, #71632, #20132, #43095, #43475, #60383, #8866, #2157, #47983, #72377, #3621, #26520, #49453, #20878, #31779, #26141, #49082, #43834, #72007, #50181, #5472, #67493, #62615, #22372, #4353, #4734, #45694, #38923, #34013, #73115, #68618, #10344, #67117, #40036, #68242, #9606, #17106, #44943, #38552, #21619, #62232, #49815, #67866, #45316, #61859, #28372, #15620, #33645, #16738, #73862, #56964, #56598, #15981, #39674, #11092, #32526, #5101, #16357 ),
 .UNSPECIFIED., .F., .F. ) 
 B_SPLINE_CURVE_WITH_KNOTS ( ( 3, 2, 2, 2, 2, 2, 2, 2, 2, 2, 2, 2, 2, 2, 2, 2, 2, 2, 2, 2, 2, 2, 2, 2, 2, 2, 2, 2, 2, 2, 2, 2, 2, 2, 2, 2, 2, 2, 2, 2, 2, 2, 2, 2, 2, 2, 2, 2, 2, 2, 2, 2, 2, 2, 2, 2, 2, 2, 2, 2, 2, 2, 2, 2, 2, 2, 2, 2, 2, 2, 2, 2, 2, 2, 2, 2, 2, 2, 2, 2, 2, 2, 2, 2, 2, 2, 2, 2, 2, 2, 2, 2, 2, 2, 2, 2, 2, 2, 2, 2, 2, 2, 2, 2, 2, 2, 2, 2, 2, 2, 2, 2, 2, 2, 2, 2, 2, 2, 2, 2, 2, 2, 2, 2, 2, 2, 2, 2, 2, 2, 2, 2, 2, 2, 2, 2, 2, 2, 2, 2, 2, 2, 2, 3 ),
 ( 0.000000000000000000, 0.007055764916269565389, 0.01411152983253913078, 0.02116729474880869530, 0.02822305966507826155, 0.03527882458134783128, 0.04233458949761739060, 0.04939035441388696379, 0.05644611933015652311, 0.06350188424642609630, 0.07055764916269566256, 0.07761341407896522882, 0.08466917899523478119, 0.09172494391150436133, 0.09878070882777392758, 0.1058364737440434938, 0.1128922386603130462, 0.1199480035765826125, 0.1270037684928521926, 0.1340595334091217450, 0.1411152983253913251, 0.1481710632416609053, 0.1552268281579304576, 0.1622825930742000100, 0.1693383579904695624, 0.1763941229067391425, 0.1834498878230087227, 0.1905056527392782750, 0.1975614176555478552, 0.2046171825718174075, 0.2116729474880869877, 0.2187287124043565678, 0.2257844773206260924, 0.2328402422368956726, 0.2398960071531652249, 0.2469517720694348051, 0.2540075369857043852, 0.2610633019019739098, 0.2681190668182434900, 0.2751748317345130701, 0.2822305966507826502, 0.2892863615670521749, 0.2963421264833218105, 0.3033978913995913351, 0.3104536563158609153, 0.3175094212321304399, 0.3245651861484000200, 0.3316209510646696002, 0.3386767159809391248, 0.3457324808972087604, 0.3527882458134782850, 0.3598440107297478652, 0.3668997756460174453, 0.3739555405622870254, 0.3810113054785565501, 0.3880670703948260747, 0.3951228353110957103, 0.4021786002273652350, 0.4092343651436348151, 0.4162901300599043952, 0.4233458949761739754, 0.4304016598924435000, 0.4374574248087131356, 0.4445131897249826602, 0.4515689546412521849, 0.4586247195575217650, 0.4656804844737913451, 0.4727362493900609253, 0.4797920143063304499, 0.4868477792226000855, 0.4939035441388696102, 0.5009593090551391903, 0.5080150739714087704, 0.5150708388876782395, 0.5221266038039478197, 0.5291823687202175108, 0.5362381336364869799, 0.5432938985527565601, 0.5503496634690261402, 0.5574054283852957203, 0.5644611933015653005, 0.5715169582178348806, 0.5785727231341043497, 0.5856284880503739299, 0.5926842529666436210, 0.5997400178829130901, 0.6067957827991826703, 0.6138515477154522504, 0.6209073126317218305, 0.6279630775479914107, 0.6350188424642608798, 0.6420746073805304599, 0.6491303722968000400, 0.6561861372130696202, 0.6632419021293392003, 0.6702976670456087804, 0.6773534319618782495, 0.6844091968781479407, 0.6914649617944175208, 0.6985207267106869899, 0.7055764916269565701, 0.7126322565432261502, 0.7196880214594957303, 0.7267437863757653105, 0.7337995512920348906, 0.7408553162083043597, 0.7479110811245740509, 0.7549668460408436310, 0.7620226109571131001, 0.7690783758733826803, 0.7761341407896521494, 0.7831899057059218405, 0.7902456706221914207, 0.7973014355384608898, 0.8043572004547304699, 0.8114129653710001611, 0.8184687302872696302, 0.8255244952035392103, 0.8325802601198087904, 0.8396360250360782596, 0.8466917899523479507, 0.8537475548686175308, 0.8608033197848870000, 0.8678590847011565801, 0.8749148496174262712, 0.8819706145336957404, 0.8890263794499653205, 0.8960821443662349006, 0.9031379092825043697, 0.9101936741987740609, 0.9172494391150435300, 0.9243052040313131101, 0.9313609689475826903, 0.9384167338638522704, 0.9454724987801218505, 0.9525282636963914307, 0.9595840286126608998, 0.9666397935289304799, 0.9736955584452001711, 0.9807513233614696402, 0.9878070882777392203, 0.9948628531940088005, 0.9999999123559569769, 1.000000000000000000 ),
 .UNSPECIFIED. ) 
 CURVE ( )  GEOMETRIC_REPRESENTATION_ITEM ( )  RATIONAL_B_SPLINE_CURVE ( ( 1.000000000000000000, 0.8660254037844387076, 1.000000000000000000, 0.8660254037844387076, 1.000000000000000000, 0.8660254037844387076, 1.000000000000000000, 0.8660254037844387076, 1.000000000000000000, 0.8660254037844387076, 1.000000000000000000, 0.8660254037844387076, 1.000000000000000000, 0.8660254037844387076, 1.000000000000000000, 0.8660254037844387076, 1.000000000000000000, 0.8660254037844387076, 1.000000000000000000, 0.8660254037844387076, 1.000000000000000000, 0.8660254037844387076, 1.000000000000000000, 0.8660254037844387076, 1.000000000000000000, 0.8660254037844387076, 1.000000000000000000, 0.8660254037844387076, 1.000000000000000000, 0.8660254037844387076, 1.000000000000000000, 0.8660254037844387076, 1.000000000000000000, 0.8660254037844387076, 1.000000000000000000, 0.8660254037844387076, 1.000000000000000000, 0.8660254037844387076, 1.000000000000000000, 0.8660254037844387076, 1.000000000000000000, 0.8660254037844387076, 1.000000000000000000, 0.8660254037844387076, 1.000000000000000000, 0.8660254037844387076, 1.000000000000000000, 0.8660254037844387076, 1.000000000000000000, 0.8660254037844387076, 1.000000000000000000, 0.8660254037844387076, 1.000000000000000000, 0.8660254037844387076, 1.000000000000000000, 0.8660254037844387076, 1.000000000000000000, 0.8660254037844387076, 1.000000000000000000, 0.8660254037844387076, 1.000000000000000000, 0.8660254037844387076, 1.000000000000000000, 0.8660254037844387076, 1.000000000000000000, 0.8660254037844387076, 1.000000000000000000, 0.8660254037844387076, 1.000000000000000000, 0.8660254037844387076, 1.000000000000000000, 0.8660254037844387076, 1.000000000000000000, 0.8660254037844387076, 1.000000000000000000, 0.8660254037844387076, 1.000000000000000000, 0.8660254037844387076, 1.000000000000000000, 0.8660254037844387076, 1.000000000000000000, 0.8660254037844387076, 1.000000000000000000, 0.8660254037844387076, 1.000000000000000000, 0.8660254037844387076, 1.000000000000000000, 0.8660254037844387076, 1.000000000000000000, 0.8660254037844387076, 1.000000000000000000, 0.8660254037844387076, 1.000000000000000000, 0.8660254037844387076, 1.000000000000000000, 0.8660254037844387076, 1.000000000000000000, 0.8660254037844387076, 1.000000000000000000, 0.8660254037844387076, 1.000000000000000000, 0.8660254037844387076, 1.000000000000000000, 0.8660254037844387076, 1.000000000000000000, 0.8660254037844387076, 1.000000000000000000, 0.8660254037844387076, 1.000000000000000000, 0.8660254037844387076, 1.000000000000000000, 0.8660254037844387076, 1.000000000000000000, 0.8660254037844387076, 1.000000000000000000, 0.8660254037844387076, 1.000000000000000000, 0.8660254037844387076, 1.000000000000000000, 0.8660254037844387076, 1.000000000000000000, 0.8660254037844387076, 1.000000000000000000, 0.8660254037844387076, 1.000000000000000000, 0.8660254037844387076, 1.000000000000000000, 0.8660254037844387076, 1.000000000000000000, 0.8660254037844387076, 1.000000000000000000, 0.8660254037844387076, 1.000000000000000000, 0.8660254037844387076, 1.000000000000000000, 0.8660254037844387076, 1.000000000000000000, 0.8660254037844387076, 1.000000000000000000, 0.8660254037844387076, 1.000000000000000000, 0.8660254037844387076, 1.000000000000000000, 0.8660254037844387076, 1.000000000000000000, 0.8660254037844387076, 1.000000000000000000, 0.8660254037844387076, 1.000000000000000000, 0.8660254037844387076, 1.000000000000000000, 0.8660254037844387076, 1.000000000000000000, 0.8660254037844387076, 1.000000000000000000, 0.8660254037844387076, 1.000000000000000000, 0.8660254037844387076, 1.000000000000000000, 0.8660254037844387076, 1.000000000000000000, 0.8660254037844387076, 1.000000000000000000, 0.8660254037844387076, 1.000000000000000000, 0.8660254037844387076, 1.000000000000000000, 0.8660254037844387076, 1.000000000000000000, 0.8660254037844387076, 1.000000000000000000, 0.8660254037844387076, 1.000000000000000000, 0.8660254037844387076, 1.000000000000000000, 0.8660254037844387076, 1.000000000000000000, 0.8660254037844387076, 1.000000000000000000, 0.8660254037844387076, 1.000000000000000000, 0.8660254037844387076, 1.000000000000000000, 0.8660254037844387076, 1.000000000000000000, 0.8660254037844387076, 1.000000000000000000, 0.8660254037844387076, 1.000000000000000000, 0.8660254037844387076, 1.000000000000000000, 0.8660254037844387076, 1.000000000000000000, 0.8660254037844387076, 1.000000000000000000, 0.8660254037844387076, 1.000000000000000000, 0.8660254037844387076, 1.000000000000000000, 0.8660254037844387076, 1.000000000000000000, 0.8660254037844387076, 1.000000000000000000, 0.8660254037844387076, 1.000000000000000000, 0.8660254037844387076, 1.000000000000000000, 0.8660254037844387076, 1.000000000000000000, 0.8660254037844387076, 1.000000000000000000, 0.8660254037844387076, 1.000000000000000000, 0.8660254037844387076, 1.000000000000000000, 0.8660254037844387076, 1.000000000000000000, 0.8660254037844387076, 1.000000000000000000, 0.8660254037844387076, 1.000000000000000000, 0.8660254037844387076, 1.000000000000000000, 0.8660254037844387076, 1.000000000000000000, 0.8660254037844387076, 1.000000000000000000, 0.8660254037844387076, 1.000000000000000000, 0.8660254037844387076, 1.000000000000000000, 0.8660254037844387076, 1.000000000000000000, 0.8660254037844387076, 1.000000000000000000, 0.8660254037844387076, 1.000000000000000000, 0.8660254037844387076, 1.000000000000000000, 0.8660254037844387076, 1.000000000000000000, 0.8660254037844387076, 1.000000000000000000, 0.8660254037844387076, 1.000000000000000000, 0.8660254037844387076, 1.000000000000000000, 0.8660254037844387076, 1.000000000000000000, 0.8660254037844387076, 1.000000000000000000, 0.8660254037844387076, 1.000000000000000000, 0.8660254037844387076, 1.000000000000000000, 0.8660254037844387076, 1.000000000000000000, 0.8660254037844387076, 1.000000000000000000, 0.8660254037844387076, 1.000000000000000000, 0.8660254037844387076, 1.000000000000000000, 0.8660254037844387076, 1.000000000000000000, 0.8660254037844387076, 1.000000000000000000, 0.8660254037844387076, 1.000000000000000000, 0.8660254037844387076, 1.000000000000000000, 0.8660254037844387076, 1.000000000000000000, 0.8660254037844387076, 1.000000000000000000, 0.8660254037844387076, 1.000000000000000000, 0.8660254037844387076, 1.000000000000000000, 0.8660254037844387076, 1.000000000000000000, 0.8660254037844387076, 1.000000000000000000, 0.9024577157650929271, 0.9469497795711361299, 0.9469497795711361299, 0.9469497795711361299 ) ) 
 REPRESENTATION_ITEM ( '' )  );
#37823 = CARTESIAN_POINT ( 'NONE',  ( 93.84685191531248449, 91.99731107132950569, 88.42572916753381662 ) ) ;
#37824 = CARTESIAN_POINT ( 'NONE',  ( 97.64999999999999147, -209.9999999999999716, 90.00000000000000000 ) ) ;
#37825 = CARTESIAN_POINT ( 'NONE',  ( 95.00000000000000000, -206.9400435732949575, 81.58624999999999261 ) ) ;
#37826 = VECTOR ( 'NONE', #18604, 1000.000000000000000 ) ;
#37827 = ORIENTED_EDGE ( 'NONE', *, *, #45504, .T. ) ;
#37828 = EDGE_LOOP ( 'NONE', ( #23941, #47691, #21644, #10300 ) ) ;
#37829 = ORIENTED_EDGE ( 'NONE', *, *, #19786, .T. ) ;
#37830 = ORIENTED_EDGE ( 'NONE', *, *, #63263, .F. ) ;
#37831 = DIRECTION ( 'NONE',  ( 1.000000000000000000, 0.000000000000000000, 0.000000000000000000 ) ) ;
#37832 = CARTESIAN_POINT ( 'NONE',  ( -97.30629616937501680, 88.66845928578038638, 85.40947916753380298 ) ) ;
#37833 = AXIS2_PLACEMENT_3D ( 'NONE', #6177, #69308, #56934 ) ;
#37834 = CYLINDRICAL_SURFACE ( 'NONE', #33828, 2.649999999999985700 ) ;
#37835 = CARTESIAN_POINT ( 'NONE',  ( 0.000000000000000000, -65.59268652807183742, -36.72794159290312166 ) ) ;
#37836 = CARTESIAN_POINT ( 'NONE',  ( 94.99999999999998579, 90.00000000000002842, 90.00000000000000000 ) ) ;
#37837 = DIRECTION ( 'NONE',  ( 0.000000000000000000, 1.000000000000000000, 3.469446951953614189E-15 ) ) ;
#37838 = ORIENTED_EDGE ( 'NONE', *, *, #38720, .T. ) ;
#37839 = CARTESIAN_POINT ( 'NONE',  ( -92.34999999999999432, -208.4700217866474645, 87.27479166840096525 ) ) ;
#37840 = ORIENTED_EDGE ( 'NONE', *, *, #67565, .F. ) ;
#37841 = CYLINDRICAL_SURFACE ( 'NONE', #59024, 16.00000000000000000 ) ;
#37842 = ORIENTED_EDGE ( 'NONE', *, *, #31568, .T. ) ;
#37843 = CARTESIAN_POINT ( 'NONE',  ( -92.35000000000005116, 88.47002178664754979, 82.08895833506764461 ) ) ;
#37844 = ORIENTED_EDGE ( 'NONE', *, *, #22953, .T. ) ;
#37845 = CARTESIAN_POINT ( 'NONE',  ( 97.30629616937498838, 88.66845928578037217, 86.25614583420048120 ) ) ;
#37846 = CARTESIAN_POINT ( 'NONE',  ( 0.000000000000000000, -37.22597642581161637, 5.202137450156258502 ) ) ;
#37847 = CARTESIAN_POINT ( 'NONE',  ( 0.000000000000000000, -46.21855187248583974, -62.20884554314070414 ) ) ;
#37848 = EDGE_CURVE ( 'NONE', #12223, #2654, #36128, .T. ) ;
#37849 = CARTESIAN_POINT ( 'NONE',  ( -92.69370383062504004, 89.70433482669615444, 74.79348190356851944 ) ) ;
#37850 = DIRECTION ( 'NONE',  ( -1.000000000000000000, -0.000000000000000000, 0.000000000000000000 ) ) ;
#37851 = ADVANCED_FACE ( 'NONE', ( #57961 ), #2338, .T. ) ;
#37852 = LINE ( 'NONE', #32185, #51539 ) ;
#37853 = EDGE_LOOP ( 'NONE', ( #40921, #44573, #41486, #69960 ) ) ;
#37854 = CARTESIAN_POINT ( 'NONE',  ( -96.32500000000001705, 92.29496732002878900, 81.08354166840096866 ) ) ;
#37855 = CARTESIAN_POINT ( 'NONE',  ( 0.000000000000000000, 77.19088730480524418, 6.903761155838049390 ) ) ;
#37856 = ORIENTED_EDGE ( 'NONE', *, *, #18856, .F. ) ;
#37857 = EDGE_CURVE ( 'NONE', #50325, #30840, #42766, .T. ) ;
#37858 = VERTEX_POINT ( 'NONE', #26689 ) ;
#37859 = CARTESIAN_POINT ( 'NONE',  ( -0.0004442498525516064278, 0.001194404164626844313, -80.00000000000000000 ) ) ;
#37860 = ADVANCED_FACE ( 'NONE', ( #3062 ), #71437, .T. ) ;
#37861 = CARTESIAN_POINT ( 'NONE',  ( 15.00000000000000000, 16.61724383029390140, 20.69703378468902955 ) ) ;
#37862 = DIRECTION ( 'NONE',  ( -1.000000000000000000, 0.000000000000000000, 0.000000000000000000 ) ) ;
#37863 = EDGE_CURVE ( 'NONE', #11526, #29066, #10338, .T. ) ;
#37864 = CARTESIAN_POINT ( 'NONE',  ( -96.15314808468747287, -208.0026889286704943, 83.34572916753383254 ) ) ;
#37865 = VERTEX_POINT ( 'NONE', #42517 ) ;
#37866 = CARTESIAN_POINT ( 'NONE',  ( 95.00000000000000000, -209.9999999999999716, 90.00000000000000000 ) ) ;
#37867 = VECTOR ( 'NONE', #60591, 1000.000000000000000 ) ;
#37868 = EDGE_LOOP ( 'NONE', ( #71283, #61240, #26266, #41591 ) ) ;
#37869 = DIRECTION ( 'NONE',  ( 0.000000000000000000, 0.9510565162951544194, -0.3090169943749447867 ) ) ;
#37870 = FACE_BOUND ( 'NONE', #39771, .T. ) ;
#37871 = CARTESIAN_POINT ( 'NONE',  ( -96.32499999999996021, -212.2949673200287179, 76.21520833506762926 ) ) ;
#37872 = CARTESIAN_POINT ( 'NONE',  ( 96.15314808468748708, 88.00268892867053694, 77.15447916753380753 ) ) ;
#37873 = DIRECTION ( 'NONE',  ( 1.000000000000000000, 0.000000000000000000, 0.000000000000000000 ) ) ;
#37874 = DIRECTION ( 'NONE',  ( 0.000000000000000000, 0.000000000000000000, -1.000000000000000000 ) ) ;
#37875 = CARTESIAN_POINT ( 'NONE',  ( 10.00000000000000000, -0.8261519478425671803, -77.49459641780887864 ) ) ;
#37876 = DIRECTION ( 'NONE',  ( 0.000000000000000000, -0.2334453638558921795, -0.9723699203976797767 ) ) ;
#37877 = DIRECTION ( 'NONE',  ( 2.603472992746261562E-14, 2.546204323184492723E-14, -1.000000000000000000 ) ) ;
#37878 = CARTESIAN_POINT ( 'NONE',  ( 0.000000000000000000, 0.000000000000000000, 0.000000000000000000 ) ) ;
#37879 =( REPRESENTATION_RELATIONSHIP ('NONE','NONE', #31117, #10045 ) REPRESENTATION_RELATIONSHIP_WITH_TRANSFORMATION ( #22207 )SHAPE_REPRESENTATION_RELATIONSHIP( ) );
#37880 = CARTESIAN_POINT ( 'NONE',  ( 92.35000000030107969, -209.9999754409356854, 87.53856274002261273 ) ) ;
#37881 = EDGE_CURVE ( 'NONE', #6415, #50378, #17539, .T. ) ;
#37882 = PRODUCT_DEFINITION_CONTEXT ( 'detailed design', #44125, 'design' ) ;
#37883 = VECTOR ( 'NONE', #41822, 1000.000000000000000 ) ;
#37884 = CARTESIAN_POINT ( 'NONE',  ( -95.00000000000002842, 86.94004357329504273, 78.17312500173430578 ) ) ;
#37885 = ORIENTED_EDGE ( 'NONE', *, *, #39255, .F. ) ;
#37886 = CARTESIAN_POINT ( 'NONE',  ( -96.15314808468751551, 88.00268892867056536, 82.12864583420046927 ) ) ;
#37887 = EDGE_CURVE ( 'NONE', #27626, #26875, #15044, .T. ) ;
#37888 = ADVANCED_FACE ( 'NONE', ( #27056 ), #32330, .T. ) ;
#37889 = DIRECTION ( 'NONE',  ( 0.000000000000000000, -0.1564344650402382242, 0.9876883405951366601 ) ) ;
#37890 = VECTOR ( 'NONE', #65550, 1000.000000000000000 ) ;
#37891 = DIRECTION ( 'NONE',  ( -1.000000000000000000, 0.000000000000000000, -0.000000000000000000 ) ) ;
#37892 = ADVANCED_FACE ( 'NONE', ( #54178 ), #43640, .T. ) ;
#37893 = EDGE_LOOP ( 'NONE', ( #36893, #58625, #32604, #30156 ) ) ;
#37894 = CYLINDRICAL_SURFACE ( 'NONE', #12631, 77.49899999999999523 ) ;
#37895 = CARTESIAN_POINT ( 'NONE',  ( 92.35000000000000853, -209.9999999999999716, 90.00000000000000000 ) ) ;
#37896 = CARTESIAN_POINT ( 'NONE',  ( 0.000000000000000000, 0.000000000000000000, 0.000000000000000000 ) ) ;
#37897 = DIRECTION ( 'NONE',  ( 0.000000000000000000, 0.000000000000000000, -1.000000000000000000 ) ) ;
#37898 = CARTESIAN_POINT ( 'NONE',  ( 93.84685191531249870, -208.0026889286704943, 78.26572916753382003 ) ) ;
#37899 = EDGE_LOOP ( 'NONE', ( #25848, #49476, #35541, #4931 ) ) ;
#37900 = ORIENTED_EDGE ( 'NONE', *, *, #60951, .T. ) ;
#37901 = CARTESIAN_POINT ( 'NONE',  ( 10.00000000000000000, 8.840884882375075193, 74.65374052328651544 ) ) ;
#37902 = CARTESIAN_POINT ( 'NONE',  ( -11.59517495878806947, -96.12423995607481686, 5.500000000000000000 ) ) ;
#37903 = CARTESIAN_POINT ( 'NONE',  ( 99.99999999999998579, 95.00000000000002842, -90.00000000000000000 ) ) ;
#37904 = CIRCLE ( 'NONE', #46288, 82.00000000000000000 ) ;
#37905 = CARTESIAN_POINT ( 'NONE',  ( -3.000000000000000000, -19.89357724624987256, -12.59942793731086041 ) ) ;
#37906 = CARTESIAN_POINT ( 'NONE',  ( 94.26574316504959938, -214.0859151322040645, 74.64692065633562379 ) ) ;
#37907 = ORIENTED_EDGE ( 'NONE', *, *, #20454, .F. ) ;
#37908 = DIRECTION ( 'NONE',  ( 0.000000000000000000, 0.000000000000000000, -1.000000000000000000 ) ) ;
#37909 = EDGE_LOOP ( 'NONE', ( #44241, #63100, #8759, #64372 ) ) ;
#37910 = AXIS2_PLACEMENT_3D ( 'NONE', #42283, #65209, #13683 ) ;
#37911 = ORIENTED_EDGE ( 'NONE', *, *, #20876, .F. ) ;
#37912 = CARTESIAN_POINT ( 'NONE',  ( -96.32500000000001705, 87.70503267997129626, 83.12083333333332291 ) ) ;
#37913 = SURFACE_SIDE_STYLE ('',( #13848 ) ) ;
#37914 = AXIS2_PLACEMENT_3D ( 'NONE', #58694, #55178, #37529 ) ;
#37915 = DIRECTION ( 'NONE',  ( 0.2867529058022035837, -0.9580045777625452175, 0.000000000000000000 ) ) ;
#37916 = ORIENTED_EDGE ( 'NONE', *, *, #54399, .T. ) ;
#37917 = DIRECTION ( 'NONE',  ( -0.5687579148473752566, 0.8225049752423786442, 0.000000000000000000 ) ) ;
#37918 = CARTESIAN_POINT ( 'NONE',  ( 92.35000000000002274, -208.4700217866474645, 80.50145833506765314 ) ) ;
#37919 = CARTESIAN_POINT ( 'NONE',  ( 92.34999999999999432, 88.47002178664753558, 86.24291666666665890 ) ) ;
#37920 = EDGE_LOOP ( 'NONE', ( #62242, #19627, #2715, #18214 ) ) ;
#37921 = CARTESIAN_POINT ( 'NONE',  ( 0.000000000000000000, 0.000000000000000000, 0.000000000000000000 ) ) ;
#37922 = CARTESIAN_POINT ( 'NONE',  ( 10.00000000000000000, 4.992566952384984269, 37.16516213103279398 ) ) ;
#37923 = AXIS2_PLACEMENT_3D ( 'NONE', #72338, #61068, #14076 ) ;
#37924 = VERTEX_POINT ( 'NONE', #13925 ) ;
#37925 = AXIS2_PLACEMENT_3D ( 'NONE', #539, #51990, #23436 ) ;
#37926 = CARTESIAN_POINT ( 'NONE',  ( -10.00000000000000000, 0.000000000000000000, 0.000000000000000000 ) ) ;
#37927 = CARTESIAN_POINT ( 'NONE',  ( -97.30629616937501680, 88.66845928578038638, 84.77447916753381207 ) ) ;
#37928 = CARTESIAN_POINT ( 'NONE',  ( 96.15314808468748708, 91.99731107132950569, 83.08114583420048405 ) ) ;
#37929 = ORIENTED_EDGE ( 'NONE', *, *, #16290, .F. ) ;
#37930 = CARTESIAN_POINT ( 'NONE',  ( 23.11608002360578240, -124.4885236261218182, 5.500000000000000000 ) ) ;
#37931 = ORIENTED_EDGE ( 'NONE', *, *, #5710, .F. ) ;
#37932 = FACE_OUTER_BOUND ( 'NONE', #40534, .T. ) ;
#37933 = VERTEX_POINT ( 'NONE', #31226 ) ;
#37934 = VERTEX_POINT ( 'NONE', #49990 ) ;
#37935 = EDGE_CURVE ( 'NONE', #58363, #29480, #55965, .T. ) ;
#37936 = ORIENTED_EDGE ( 'NONE', *, *, #56017, .F. ) ;
#37937 = PLANE ( 'NONE',  #26492 ) ;
#37938 = ADVANCED_FACE ( 'NONE', ( #19938 ), #31588, .T. ) ;
#37939 = ORIENTED_EDGE ( 'NONE', *, *, #59021, .F. ) ;
#37940 = CARTESIAN_POINT ( 'NONE',  ( 2.369999999999999662, 0.000000000000000000, 0.000000000000000000 ) ) ;
#37941 = ORIENTED_EDGE ( 'NONE', *, *, #25740, .F. ) ;
#37942 = CARTESIAN_POINT ( 'NONE',  ( 0.000000000000000000, 0.000000000000000000, 0.000000000000000000 ) ) ;
#37943 = CARTESIAN_POINT ( 'NONE',  ( -94.99999999999997158, -212.6630814284392557, 79.64156250086713840 ) ) ;
#37945 = ORIENTED_EDGE ( 'NONE', *, *, #23292, .F. ) ;
#37944 = EDGE_CURVE ( 'NONE', #72597, #43377, #15115, .T. ) ;
#37946 = CARTESIAN_POINT ( 'NONE',  ( -97.64999999999993463, 88.47002178664749295, 86.24291666666667311 ) ) ;
#37947 = LINE ( 'NONE', #54862, #69303 ) ;
#37948 = LINE ( 'NONE', #21012, #72920 ) ;
#37949 = CARTESIAN_POINT ( 'NONE',  ( -12.50000000000000000, -132.5000000000000000, -40.00000000000000000 ) ) ;
#37950 = CARTESIAN_POINT ( 'NONE',  ( 0.000000000000000000, -0.8660254037844384856, 1.500000000000000000 ) ) ;
#37951 = LINE ( 'NONE', #61629, #28905 ) ;
#37952 = CARTESIAN_POINT ( 'NONE',  ( 96.15314808468748708, 91.99731107132950569, 88.79614583420047325 ) ) ;
#37953 = FACE_OUTER_BOUND ( 'NONE', #53939, .T. ) ;
#37954 = CARTESIAN_POINT ( 'NONE',  ( 92.34999999999999432, 90.00000000000002842, 81.18937500173430521 ) ) ;
#37955 = CARTESIAN_POINT ( 'NONE',  ( 10.00000000000000000, 0.000000000000000000, 0.000000000000000000 ) ) ;
#37956 = ADVANCED_FACE ( 'NONE', ( #37624 ), #61294, .T. ) ;
#37957 = CARTESIAN_POINT ( 'NONE',  ( 0.000000000000000000, 8.688484142253939169, 21.88630264137371029 ) ) ;
#37958 = ADVANCED_FACE ( 'NONE', ( #9037 ), #37983, .T. ) ;
#37959 = CYLINDRICAL_SURFACE ( 'NONE', #43135, 16.00000000000000000 ) ;
#37960 = DIRECTION ( 'NONE',  ( -1.000000000000000000, -0.000000000000000000, 0.000000000000000000 ) ) ;
#37961 = PLANE ( 'NONE',  #19923 ) ;
#37962 = AXIS2_PLACEMENT_3D ( 'NONE', #38494, #5043, #9913 ) ;
#37963 = DIRECTION ( 'NONE',  ( 0.000000000000000000, 0.000000000000000000, 1.000000000000000000 ) ) ;
#37964 = EDGE_CURVE ( 'NONE', #32596, #28941, #32696, .T. ) ;
#37965 = EDGE_CURVE ( 'NONE', #41146, #59272, #72182, .T. ) ;
#37966 = CARTESIAN_POINT ( 'NONE',  ( 0.000000000000000000, -20.40083707022829174, -72.35432306680507963 ) ) ;
#37967 = CARTESIAN_POINT ( 'NONE',  ( -10.00000000000000000, 0.000000000000000000, 0.000000000000000000 ) ) ;
#37968 = CARTESIAN_POINT ( 'NONE',  ( -96.32499999999996021, -212.2949673200287179, 89.47083333333333144 ) ) ;
#37969 = AXIS2_PLACEMENT_3D ( 'NONE', #21583, #38140, #27602 ) ;
#37970 = DIRECTION ( 'NONE',  ( -1.000000000000000000, 0.000000000000000000, 0.000000000000000000 ) ) ;
#37971 = PRODUCT ( 'taper roller bearing_iso_ISO 355-2 - 2BD25 - 22,SI,NC,22', 'taper roller bearing_iso_ISO 355-2 - 2BD25 - 22,SI,NC,22', '', ( #887 ) ) ;
#37972 = CIRCLE ( 'NONE', #21155, 31.99999999999998579 ) ;
#37973 = VECTOR ( 'NONE', #7893, 1000.000000000000227 ) ;
#37974 = VERTEX_POINT ( 'NONE', #9783 ) ;
#37975 = DIRECTION ( 'NONE',  ( 0.000000000000000000, -0.5877852522924797984, -0.8090169943749426773 ) ) ;
#37976 = CARTESIAN_POINT ( 'NONE',  ( 11.99999999999999822, 46.21855187248630870, 62.20884554314035597 ) ) ;
#37977 = DIRECTION ( 'NONE',  ( 2.603472992746261562E-14, 2.546204323184492723E-14, -1.000000000000000000 ) ) ;
#37978 = CARTESIAN_POINT ( 'NONE',  ( 0.000000000000000000, 0.000000000000000000, -4.400000000000001243 ) ) ;
#37979 = AXIS2_PLACEMENT_3D ( 'NONE', #72907, #36864, #66200 ) ;
#37980 = ORIENTED_EDGE ( 'NONE', *, *, #72199, .F. ) ;
#37981 = ORIENTED_EDGE ( 'NONE', *, *, #63413, .T. ) ;
#37982 = LINE ( 'NONE', #4158, #13116 ) ;
#37983 = CYLINDRICAL_SURFACE ( 'NONE', #41580, 31.99999999999999289 ) ;
#37984 = ORIENTED_EDGE ( 'NONE', *, *, #28697, .F. ) ;
#37985 = CARTESIAN_POINT ( 'NONE',  ( 97.30629616937498838, -209.9999999999999716, 82.97531250086714749 ) ) ;
#37986 = CARTESIAN_POINT ( 'NONE',  ( 96.15314808468750130, -211.9973110713294489, 84.29822916753381890 ) ) ;
#37987 = ORIENTED_EDGE ( 'NONE', *, *, #52995, .T. ) ;
#37988 = CARTESIAN_POINT ( 'NONE',  ( 97.30629616937498838, -209.9999999999999716, 85.67406250086715147 ) ) ;
#37989 = VERTEX_POINT ( 'NONE', #55641 ) ;
#37990 = CARTESIAN_POINT ( 'NONE',  ( 11.99999999999999822, -62.50884508063453637, 41.76106447765467777 ) ) ;
#37991 = ORIENTED_EDGE ( 'NONE', *, *, #71010, .T. ) ;
#37992 = CARTESIAN_POINT ( 'NONE',  ( -96.15314808468752972, 91.99731107132950569, 78.90072916753382515 ) ) ;
#37993 = CLOSED_SHELL ( 'NONE', ( #66476, #56216, #17894, #66074, #15532, #4301, #48387, #21749, #44820, #11605, #18923, #26469, #25398, #38375, #40994, #55186, #13644, #38028, #31747, #29893, #31800, #55649, #15808, #17722, #19574, #54596, #54246, #68021, #72532, #5055, #2193, #53997, #30657, #43219, #60434, #19589, #6615, #24979, #31982, #73129, #55791, #34968 ) ) ;
#37994 = ORIENTED_EDGE ( 'NONE', *, *, #11186, .T. ) ;
#37995 = VERTEX_POINT ( 'NONE', #4160 ) ;
#37996 = CARTESIAN_POINT ( 'NONE',  ( -95.00000000000002842, 90.00000000000004263, 90.00000000000000000 ) ) ;
#37997 = VERTEX_POINT ( 'NONE', #8302 ) ;
#37998 = CARTESIAN_POINT ( 'NONE',  ( 23.50000000000000355, -120.0000000000000000, -80.00000000000000000 ) ) ;
#37999 = CARTESIAN_POINT ( 'NONE',  ( 93.67500000000001137, -207.7050326799711968, 89.33854166840096411 ) ) ;
#38000 = ORIENTED_EDGE ( 'NONE', *, *, #44122, .F. ) ;
#38001 = CARTESIAN_POINT ( 'NONE',  ( 5.000000000000000000, 51.29473840253223926, 63.97538442413444670 ) ) ;
#38002 = EDGE_CURVE ( 'NONE', #49491, #13197, #57157, .T. ) ;
#38003 = ORIENTED_EDGE ( 'NONE', *, *, #48192, .F. ) ;
#38004 = CARTESIAN_POINT ( 'NONE',  ( 11.99999999999999822, 26.02418014898407961, -70.52718814184231633 ) ) ;
#38005 = AXIS2_PLACEMENT_3D ( 'NONE', #19255, #42206, #65141 ) ;
#38006 = ORIENTED_EDGE ( 'NONE', *, *, #24630, .F. ) ;
#38007 = EDGE_CURVE ( 'NONE', #10617, #23374, #34338, .T. ) ;
#38008 = VERTEX_POINT ( 'NONE', #45119 ) ;
#38009 = ORIENTED_EDGE ( 'NONE', *, *, #64429, .F. ) ;
#38010 = CARTESIAN_POINT ( 'NONE',  ( -2.925285743277526329, -4.084588180558410109, -5.989444439476605986 ) ) ;
#38011 = DIRECTION ( 'NONE',  ( 0.000000000000000000, 0.9723699203976756689, 0.2334453638559095823 ) ) ;
#38012 = ORIENTED_EDGE ( 'NONE', *, *, #26509, .F. ) ;
#38013 = VERTEX_POINT ( 'NONE', #11264 ) ;
#38014 = AXIS2_PLACEMENT_3D ( 'NONE', #51626, #34698, #41098 ) ;
#38015 = ADVANCED_FACE ( 'NONE', ( #16531 ), #15796, .F. ) ;
#38016 = VERTEX_POINT ( 'NONE', #22935 ) ;
#38017 = AXIS2_PLACEMENT_3D ( 'NONE', #42868, #14281, #3042 ) ;
#38018 = DIRECTION ( 'NONE',  ( -1.000000000000000000, -0.000000000000000000, -0.000000000000000000 ) ) ;
#38019 = LINE ( 'NONE', #20361, #35901 ) ;
#38020 = EDGE_CURVE ( 'NONE', #18128, #46834, #28924, .T. ) ;
#38021 = CARTESIAN_POINT ( 'NONE',  ( -95.00000000000002842, 87.33691857156074434, 77.89531250086714920 ) ) ;
#38022 = EDGE_LOOP ( 'NONE', ( #20890, #49713, #61782, #56444 ) ) ;
#38023 = CARTESIAN_POINT ( 'NONE',  ( 97.30629616937498838, 90.00000000000002842, 78.53031250086714010 ) ) ;
#38024 =( BOUNDED_CURVE ( )  B_SPLINE_CURVE ( 2, ( #20115, #20503, #54708, #61093, #32130, #65263, #13736 ),
 .UNSPECIFIED., .F., .F. ) 
 B_SPLINE_CURVE_WITH_KNOTS ( ( 3, 2, 2, 3 ),
 ( 0.5624999999999997780, 0.5694444444444440867, 0.5763888888888885065, 0.5833333333333329263 ),
 .UNSPECIFIED. ) 
 CURVE ( )  GEOMETRIC_REPRESENTATION_ITEM ( )  RATIONAL_B_SPLINE_CURVE ( ( 1.000000000000004219, 0.8660254037844343777, 1.000000000000000000, 0.8660254037844387076, 1.000000000000000000, 0.8660254037844472563, 0.9999999999999914513 ) ) 
 REPRESENTATION_ITEM ( '' )  );
#38025 = ORIENTED_EDGE ( 'NONE', *, *, #47419, .F. ) ;
#38026 = DIRECTION ( 'NONE',  ( -0.000000000000000000, -0.000000000000000000, -1.000000000000000000 ) ) ;
#38027 = CARTESIAN_POINT ( 'NONE',  ( -97.30629616937497417, -211.3315407142195852, 88.42572916753380241 ) ) ;
#38028 = ADVANCED_FACE ( 'NONE', ( #38732 ), #73663, .F. ) ;
#38029 = DIRECTION ( 'NONE',  ( -8.119982227976398872E-16, -1.065814103640131188E-14, -1.000000000000000000 ) ) ;
#38030 = DIRECTION ( 'NONE',  ( -1.000000000000000000, 0.000000000000000000, 0.000000000000000000 ) ) ;
#38031 = DIRECTION ( 'NONE',  ( 1.000000000000000000, 0.000000000000000000, 0.000000000000000000 ) ) ;
#38032 = CARTESIAN_POINT ( 'NONE',  ( -92.69370383062498320, -209.9999999999999716, 81.07031250086714635 ) ) ;
#38033 = DIRECTION ( 'NONE',  ( 0.000000000000000000, 0.3826834323650905589, -0.9238795325112864054 ) ) ;
#38034 = LINE ( 'NONE', #32381, #54718 ) ;
#38035 = DIRECTION ( 'NONE',  ( 0.000000000000000000, -0.1045284632676570791, -0.9945218953682730678 ) ) ;
#38036 = ORIENTED_EDGE ( 'NONE', *, *, #44509, .T. ) ;
#38037 = AXIS2_PLACEMENT_3D ( 'NONE', #58238, #6737, #52586 ) ;
#38038 = ORIENTED_EDGE ( 'NONE', *, *, #12890, .T. ) ;
#38039 = PLANE ( 'NONE',  #39709 ) ;
#38040 = CARTESIAN_POINT ( 'NONE',  ( -92.34999999999999432, -209.9999999999999716, 89.04749999999999943 ) ) ;
#38041 = EDGE_CURVE ( 'NONE', #24429, #63558, #42812, .T. ) ;
#38042 = AXIS2_PLACEMENT_3D ( 'NONE', #19315, #54647, #53912 ) ;
#38043 = CARTESIAN_POINT ( 'NONE',  ( 0.000000000000000000, 20.40083707022987625, -72.35432306680462489 ) ) ;
#38044 = EDGE_CURVE ( 'NONE', #24954, #23224, #33441, .T. ) ;
#38045 = CARTESIAN_POINT ( 'NONE',  ( -93.84685191531252713, 88.00268892867056536, 84.77447916753381207 ) ) ;
#38046 = DIRECTION ( 'NONE',  ( -1.000000000000000000, 0.000000000000000000, -0.000000000000000000 ) ) ;
#38047 = DIRECTION ( 'NONE',  ( -1.000000000000000000, 0.000000000000000000, -0.000000000000000000 ) ) ;
#38048 = VERTEX_POINT ( 'NONE', #62425 ) ;
#38049 = DIRECTION ( 'NONE',  ( 0.000000000000000000, 0.9969173337331276308, 0.07845909572784874608 ) ) ;
#38050 = DIRECTION ( 'NONE',  ( -1.000000000000000000, -0.000000000000000000, -0.000000000000000000 ) ) ;
#38051 = DIRECTION ( 'NONE',  ( 1.000000000000000000, -0.000000000000000000, -0.000000000000000000 ) ) ;
#38052 = VECTOR ( 'NONE', #6673, 1000.000000000000000 ) ;
#38053 = DIRECTION ( 'NONE',  ( -1.000000000000000000, 0.000000000000000000, -0.000000000000000000 ) ) ;
#38054 = CARTESIAN_POINT ( 'NONE',  ( -3.675296855064184687, 3.651569063273166993, -0.8655517945778067324 ) ) ;
#38055 = CARTESIAN_POINT ( 'NONE',  ( 11.99999999999999822, 0.000000000000000000, 0.000000000000000000 ) ) ;
#38056 = CARTESIAN_POINT ( 'NONE',  ( -96.15314808468745866, -211.9973110713294489, 82.92239583420048632 ) ) ;
#38057 = CARTESIAN_POINT ( 'NONE',  ( 4.999999999999999112, -2.663952781845850826, -41.91543099594819921 ) ) ;
#38058 = AXIS2_PLACEMENT_3D ( 'NONE', #3753, #26655, #38317 ) ;
#38059 = DIRECTION ( 'NONE',  ( 0.000000000000000000, 0.000000000000000000, 1.000000000000000000 ) ) ;
#38060 = LINE ( 'NONE', #72265, #56213 ) ;
#38061 = CARTESIAN_POINT ( 'NONE',  ( 0.000000000000000000, 0.000000000000000000, 0.000000000000000000 ) ) ;
#38062 = AXIS2_PLACEMENT_3D ( 'NONE', #41064, #62908, #24149 ) ;
#38063 = ORIENTED_EDGE ( 'NONE', *, *, #62397, .T. ) ;
#38064 = DIRECTION ( 'NONE',  ( -0.000000000000000000, -0.000000000000000000, -1.000000000000000000 ) ) ;
#38065 = CYLINDRICAL_SURFACE ( 'NONE', #74310, 31.99999999999998579 ) ;
#38066 = CARTESIAN_POINT ( 'NONE',  ( 6.782329983125270800, 10.49999999999999467, 20.00000000000000000 ) ) ;
#38067 = AXIS2_PLACEMENT_3D ( 'NONE', #12050, #40633, #23346 ) ;
#38068 = AXIS2_PLACEMENT_3D ( 'NONE', #64469, #19331, #65214 ) ;
#38069 = DIRECTION ( 'NONE',  ( 7.962523111839282146E-16, -1.065814103640130873E-14, -1.000000000000000000 ) ) ;
#38070 = ORIENTED_EDGE ( 'NONE', *, *, #32216, .F. ) ;
#38071 = LINE ( 'NONE', #9497, #48069 ) ;
#38072 = CARTESIAN_POINT ( 'NONE',  ( 0.000000000000000000, 18.89407956138257205, 75.16055320797038064 ) ) ;
#38073 = ORIENTED_EDGE ( 'NONE', *, *, #2246, .F. ) ;
#38074 = DIRECTION ( 'NONE',  ( 1.000000000000000000, 0.000000000000000000, -0.000000000000000000 ) ) ;
#38075 = FACE_OUTER_BOUND ( 'NONE', #33482, .T. ) ;
#38076 = ORIENTED_EDGE ( 'NONE', *, *, #53215, .F. ) ;
#38077 = ADVANCED_FACE ( 'NONE', ( #16162 ), #39099, .F. ) ;
#38078 = FACE_OUTER_BOUND ( 'NONE', #34775, .T. ) ;
#38079 = VERTEX_POINT ( 'NONE', #27432 ) ;
#38080 = CYLINDRICAL_SURFACE ( 'NONE', #47795, 31.99999999999999289 ) ;
#38081 = AXIS2_PLACEMENT_3D ( 'NONE', #19764, #36693, #30672 ) ;
#38082 = ORIENTED_EDGE ( 'NONE', *, *, #11773, .F. ) ;
#38083 = ORIENTED_EDGE ( 'NONE', *, *, #49527, .F. ) ;
#38084 = EDGE_CURVE ( 'NONE', #49570, #52969, #62802, .T. ) ;
#38085 = VERTEX_POINT ( 'NONE', #4533 ) ;
#38086 = ORIENTED_EDGE ( 'NONE', *, *, #35385, .T. ) ;
#38087 = LINE ( 'NONE', #27156, #46767 ) ;
#38089 = ADVANCED_FACE ( 'NONE', ( #73291 ), #56013, .T. ) ;
#38088 = CIRCLE ( 'NONE', #30886, 31.99999999999999289 ) ;
#38090 = ORIENTED_EDGE ( 'NONE', *, *, #39408, .T. ) ;
#38091 = ORIENTED_EDGE ( 'NONE', *, *, #49422, .F. ) ;
#38092 = CARTESIAN_POINT ( 'NONE',  ( 92.69370383062498320, 91.33154071421968467, 77.68364583420047609 ) ) ;
#38093 = CARTESIAN_POINT ( 'NONE',  ( 10.00000000000000000, 37.22597642581150268, 5.202137450157037435 ) ) ;
#38094 = CARTESIAN_POINT ( 'NONE',  ( -92.35000000000009379, 88.47002178664753558, 85.18458333333332178 ) ) ;
#38095 = EDGE_LOOP ( 'NONE', ( #16398, #3420, #7776, #62450 ) ) ;
#38096 = EDGE_CURVE ( 'NONE', #31369, #30416, #5651, .T. ) ;
#38097 = ORIENTED_EDGE ( 'NONE', *, *, #23041, .T. ) ;
#38098 = ORIENTED_EDGE ( 'NONE', *, *, #10003, .T. ) ;
#38099 = DIRECTION ( 'NONE',  ( -1.000000000000000000, 0.000000000000000000, 0.000000000000000000 ) ) ;
#38100 = VERTEX_POINT ( 'NONE', #51483 ) ;
#38101 = CARTESIAN_POINT ( 'NONE',  ( 97.30629616937498838, -211.3315407142195852, 87.36739583420047950 ) ) ;
#38102 = DIRECTION ( 'NONE',  ( -1.000000000000000000, 0.000000000000000000, -0.000000000000000000 ) ) ;
#38103 = DIRECTION ( 'NONE',  ( 0.000000000000000000, 0.2334453638558990629, 0.9723699203976782224 ) ) ;
#38104 = CARTESIAN_POINT ( 'NONE',  ( 93.67499999999998295, 92.29496732002878900, 77.90854166840097150 ) ) ;
#38105 = FACE_OUTER_BOUND ( 'NONE', #6477, .T. ) ;
#38106 = DIRECTION ( 'NONE',  ( 1.000000000000000000, 0.000000000000000000, 0.000000000000000000 ) ) ;
#38107 = CYLINDRICAL_SURFACE ( 'NONE', #15626, 82.00000000000000000 ) ;
#38108 = CARTESIAN_POINT ( 'NONE',  ( -97.64999999999994884, -208.4700217866474645, 77.32645833506762756 ) ) ;
#38109 = CYLINDRICAL_SURFACE ( 'NONE', #69889, 77.49899999999999523 ) ;
#38110 = ORIENTED_EDGE ( 'NONE', *, *, #43882, .F. ) ;
#38112 = CARTESIAN_POINT ( 'NONE',  ( -95.00000000000002842, 87.33691857156074434, 87.26156250086714294 ) ) ;
#38111 = CARTESIAN_POINT ( 'NONE',  ( 97.30629616937498838, 91.33154071421968467, 86.83822916753381094 ) ) ;
#38113 = ORIENTED_EDGE ( 'NONE', *, *, #65481, .F. ) ;
#38114 = DIRECTION ( 'NONE',  ( 0.000000000000000000, -0.5877852522924787992, -0.8090169943749434545 ) ) ;
#38115 = ADVANCED_FACE ( 'NONE', ( #27811 ), #56773, .F. ) ;
#38116 = DIRECTION ( 'NONE',  ( 0.000000000000000000, 0.6494480483301848794, -0.7604059656000299317 ) ) ;
#38117 = DIRECTION ( 'NONE',  ( -1.000000000000000000, -0.000000000000000000, -0.000000000000000000 ) ) ;
#38118 = DIRECTION ( 'NONE',  ( -1.000000000000000000, -0.000000000000000000, -0.000000000000000000 ) ) ;
#38119 = CARTESIAN_POINT ( 'NONE',  ( -92.69370383062498320, -211.3315407142195852, 88.63739583420047552 ) ) ;
#38120 = AXIS2_PLACEMENT_3D ( 'NONE', #43590, #4479, #26639 ) ;
#38121 = CARTESIAN_POINT ( 'NONE',  ( -4.653126046682595884, -146.1313684676804314, -2.500000000000000000 ) ) ;
#38122 = LINE ( 'NONE', #16306, #10983 ) ;
#38123 = DIRECTION ( 'NONE',  ( 0.000000000000000000, 0.000000000000000000, 1.000000000000000000 ) ) ;
#38124 = ORIENTED_EDGE ( 'NONE', *, *, #13058, .T. ) ;
#38125 = ORIENTED_EDGE ( 'NONE', *, *, #54631, .T. ) ;
#38126 = AXIS2_PLACEMENT_3D ( 'NONE', #58030, #53502, #47131 ) ;
#38127 = CARTESIAN_POINT ( 'NONE',  ( -92.35000000000003695, 90.00000000000004263, 80.79249999999998977 ) ) ;
#38128 = EDGE_CURVE ( 'NONE', #14220, #21993, #51232, .T. ) ;
#38129 = CYLINDRICAL_SURFACE ( 'NONE', #37923, 77.49899999999999523 ) ;
#38130 = EDGE_CURVE ( 'NONE', #71136, #47765, #28179, .T. ) ;
#38131 = DIRECTION ( 'NONE',  ( 1.000000000000000000, 0.000000000000000000, 0.000000000000000000 ) ) ;
#38132 = CARTESIAN_POINT ( 'NONE',  ( 11.99999999999999822, 0.8261519478431255115, 77.49459641780886443 ) ) ;
#38133 = CARTESIAN_POINT ( 'NONE',  ( 11.99999999999999822, -65.64334221924882229, -41.19522573413803457 ) ) ;
#38134 = LINE ( 'NONE', #72343, #32523 ) ;
#38135 = FACE_OUTER_BOUND ( 'NONE', #50005, .T. ) ;
#38136 = EDGE_CURVE ( 'NONE', #45028, #65292, #69226, .T. ) ;
#38137 = MANIFOLD_SOLID_BREP ( 'M5 Clearance Hole1', #40409 ) ;
#38138 = ORIENTED_EDGE ( 'NONE', *, *, #52515, .T. ) ;
#38139 = CARTESIAN_POINT ( 'NONE',  ( -96.15314808468751551, 88.00268892867056536, 81.49364583420047836 ) ) ;
#38140 = DIRECTION ( 'NONE',  ( -1.000000000000000000, 0.000000000000000000, 0.000000000000000000 ) ) ;
#38141 = CARTESIAN_POINT ( 'NONE',  ( -97.65000000000007674, 88.47002178664759242, 85.60791666666665378 ) ) ;
#38142 = MECHANICAL_DESIGN_GEOMETRIC_PRESENTATION_REPRESENTATION (  '', ( #28528 ), #34485 ) ;
#38143 = CARTESIAN_POINT ( 'NONE',  ( 15.00000000000000000, -23.29833615347104470, 3.418703333116808629 ) ) ;
#38144 = DIRECTION ( 'NONE',  ( 0.000000000000000000, -0.5877852522924803536, 0.8090169943749422332 ) ) ;
#38145 = CYLINDRICAL_SURFACE ( 'NONE', #12465, 31.99999999999998579 ) ;
#38146 = CARTESIAN_POINT ( 'NONE',  ( 11.99999999999999822, 80.28980883073781172, -16.65972982744850128 ) ) ;
#38147 =( LENGTH_UNIT ( ) NAMED_UNIT ( * ) SI_UNIT ( .MILLI., .METRE. ) );
#38148 = CARTESIAN_POINT ( 'NONE',  ( 0.000000000000000000, 0.000000000000000000, 0.000000000000000000 ) ) ;
#38149 = VECTOR ( 'NONE', #2774, 999.9999999999998863 ) ;
#38150 = CARTESIAN_POINT ( 'NONE',  ( 97.30629616937498838, 90.00000000000002842, 79.95906250086714806 ) ) ;
#38151 = CARTESIAN_POINT ( 'NONE',  ( -92.69370383062498320, -208.6684592857803295, 81.91697916753383879 ) ) ;
#38152 = PLANE ( 'NONE',  #44651 ) ;
#38153 = EDGE_LOOP ( 'NONE', ( #66666, #69901, #39324, #57265 ) ) ;
#38154 = DIRECTION ( 'NONE',  ( -0.000000000000000000, -0.000000000000000000, -1.000000000000000000 ) ) ;
#38155 = CARTESIAN_POINT ( 'NONE',  ( -92.34999999999999432, -208.4700217866474645, 76.40041666666667197 ) ) ;
#38156 = CARTESIAN_POINT ( 'NONE',  ( 93.67500000000001137, -207.7050326799711968, 78.46416666666667084 ) ) ;
#38157 = CARTESIAN_POINT ( 'NONE',  ( -95.00000000000002842, 92.66308142843932671, 76.94281250086714863 ) ) ;
#38158 = CARTESIAN_POINT ( 'NONE',  ( 97.30629616937498838, -211.3315407142195852, 82.28739583420048120 ) ) ;
#38159 = ORIENTED_EDGE ( 'NONE', *, *, #3433, .F. ) ;
#38160 = CARTESIAN_POINT ( 'NONE',  ( 97.30629616937497417, 89.70433482669608338, 74.79348190356854786 ) ) ;
#38161 = ORIENTED_EDGE ( 'NONE', *, *, #37615, .F. ) ;
#38162 = CIRCLE ( 'NONE', #20124, 31.99999999999999289 ) ;
#38163 = DIRECTION ( 'NONE',  ( -1.000000000000000000, 0.000000000000000000, 0.000000000000000000 ) ) ;
#38164 = ORIENTED_EDGE ( 'NONE', *, *, #68139, .F. ) ;
#38165 = VECTOR ( 'NONE', #28427, 999.9999999999998863 ) ;
#38166 = AXIS2_PLACEMENT_3D ( 'NONE', #38990, #10034, #8928 ) ;
#38167 = EDGE_CURVE ( 'NONE', #9432, #53104, #36482, .T. ) ;
#38168 = CYLINDRICAL_SURFACE ( 'NONE', #65969, 2.649999999999985700 ) ;
#38169 = VECTOR ( 'NONE', #35812, 1000.000000000000000 ) ;
#38170 = EDGE_LOOP ( 'NONE', ( #27815, #15066, #60407, #44978 ) ) ;
#38171 = ORIENTED_EDGE ( 'NONE', *, *, #25300, .T. ) ;
#38172 = AXIS2_PLACEMENT_3D ( 'NONE', #42590, #49686, #30922 ) ;
#38173 = EDGE_CURVE ( 'NONE', #41269, #73384, #70423, .T. ) ;
#38174 = CARTESIAN_POINT ( 'NONE',  ( 96.15314808468748708, -208.0026889286704943, 79.42989583420049371 ) ) ;
#38175 = ADVANCED_FACE ( 'NONE', ( #59351 ), #41681, .F. ) ;
#38176 = CARTESIAN_POINT ( 'NONE',  ( 10.00000000000000000, 71.91182617369230456, -28.89263327155667938 ) ) ;
#38177 = CARTESIAN_POINT ( 'NONE',  ( -95.12556226663434700, 87.35320520944279110, 74.99648857272262603 ) ) ;
#38178 = CARTESIAN_POINT ( 'NONE',  ( 97.30629616937498838, 91.33154071421968467, 85.09197916753380753 ) ) ;
#38179 = CARTESIAN_POINT ( 'NONE',  ( 0.000000000000000000, 26.08949754953024325, 27.05870788708241648 ) ) ;
#38180 = CARTESIAN_POINT ( 'NONE',  ( 97.64999999999999147, -209.9999999999999716, 82.06250000000000000 ) ) ;
#38181 = ORIENTED_EDGE ( 'NONE', *, *, #48698, .T. ) ;
#38182 = ADVANCED_FACE ( 'NONE', ( #58600 ), #35310, .T. ) ;
#38183 = EDGE_LOOP ( 'NONE', ( #9061, #44940, #45235, #65413 ) ) ;
#38184 = ORIENTED_EDGE ( 'NONE', *, *, #37857, .T. ) ;
#38185 = ORIENTED_EDGE ( 'NONE', *, *, #802, .F. ) ;
#38186 = CYLINDRICAL_SURFACE ( 'NONE', #33374, 82.00000000000000000 ) ;
#38187 = AXIS2_PLACEMENT_3D ( 'NONE', #20522, #20137, #42351 ) ;
#38188 =( LENGTH_UNIT ( ) NAMED_UNIT ( * ) SI_UNIT ( .MILLI., .METRE. ) );
#38189 = PLANE ( 'NONE',  #45066 ) ;
#38190 = AXIS2_PLACEMENT_3D ( 'NONE', #349, #57084, #33764 ) ;
#38191 = FACE_OUTER_BOUND ( 'NONE', #48909, .T. ) ;
#38192 = CARTESIAN_POINT ( 'NONE',  ( 0.000000000000000000, 65.59268652807263322, -36.72794159290169347 ) ) ;
#38193 = AXIS2_PLACEMENT_3D ( 'NONE', #67392, #16632, #10243 ) ;
#38194 = DIRECTION ( 'NONE',  ( -1.000000000000000000, 0.000000000000000000, 0.000000000000000000 ) ) ;
#38195 = CIRCLE ( 'NONE', #28582, 16.00000000000000000 ) ;
#38196 = VERTEX_POINT ( 'NONE', #52223 ) ;
#38197 = CARTESIAN_POINT ( 'NONE',  ( -93.67499999999998295, -212.2949673200287179, 85.84604166840097150 ) ) ;
#38198 = VERTEX_POINT ( 'NONE', #70602 ) ;
#38199 = DIRECTION ( 'NONE',  ( -1.000000000000000000, 0.000000000000000000, 0.000000000000000000 ) ) ;
#38200 = ORIENTED_EDGE ( 'NONE', *, *, #51365, .T. ) ;
#38201 = CARTESIAN_POINT ( 'NONE',  ( -95.00000000000002842, 93.05995642670501411, 81.66562500173431260 ) ) ;
#38202 = ORIENTED_EDGE ( 'NONE', *, *, #11193, .T. ) ;
#38203 = CARTESIAN_POINT ( 'NONE',  ( 96.15314808468748708, 91.99731107132950569, 82.60489583420049087 ) ) ;
#38204 = ADVANCED_FACE ( 'NONE', ( #12732 ), #40960, .T. ) ;
#38205 = DIRECTION ( 'NONE',  ( 0.000000000000000000, 0.000000000000000000, -1.000000000000000000 ) ) ;
#38206 = CARTESIAN_POINT ( 'NONE',  ( -96.32499999999996021, -207.7050326799711968, 75.28916666666665947 ) ) ;
#38207 = CARTESIAN_POINT ( 'NONE',  ( 10.00000000000000000, -22.74946021919110706, -29.81001611431033282 ) ) ;
#38208 = DIRECTION ( 'NONE',  ( 0.000000000000000000, -0.6494480483301739993, -0.7604059656000390355 ) ) ;
#38209 = DIRECTION ( 'NONE',  ( 0.000000000000000000, 0.5877852522924684742, 0.8090169943749506709 ) ) ;
#38210 = ORIENTED_EDGE ( 'NONE', *, *, #65536, .T. ) ;
#38211 = DIRECTION ( 'NONE',  ( 0.000000000000000000, 0.000000000000000000, 1.000000000000000000 ) ) ;
#38212 = CYLINDRICAL_SURFACE ( 'NONE', #71933, 12.49999999999999645 ) ;
#38213 = VERTEX_POINT ( 'NONE', #30025 ) ;
#38214 = ORIENTED_EDGE ( 'NONE', *, *, #8579, .T. ) ;
#38215 = EDGE_CURVE ( 'NONE', #14708, #31218, #7987, .T. ) ;
#38216 = DIRECTION ( 'NONE',  ( 0.000000000000000000, 0.000000000000000000, 1.000000000000000000 ) ) ;
#38217 = EDGE_CURVE ( 'NONE', #52520, #70963, #74038, .T. ) ;
#38218 = LINE ( 'NONE', #26931, #72652 ) ;
#38219 = CARTESIAN_POINT ( 'NONE',  ( 11.99999999999999822, 65.64334221924964652, -41.19522573413665611 ) ) ;
#38220 = CARTESIAN_POINT ( 'NONE',  ( -94.99999999999997158, -207.3369185715606307, 84.56281250086716739 ) ) ;
#38221 = ORIENTED_EDGE ( 'NONE', *, *, #56377, .F. ) ;
#38222 = PRESENTATION_LAYER_ASSIGNMENT (  '', '', ( #28606 ) ) ;
#38223 = CARTESIAN_POINT ( 'NONE',  ( 0.000000000000000000, 0.000000000000000000, 0.000000000000000000 ) ) ;
#38224 = ORIENTED_EDGE ( 'NONE', *, *, #40834, .F. ) ;
#38225 = CIRCLE ( 'NONE', #34567, 37.49900000000001654 ) ;
#38226 = VECTOR ( 'NONE', #12802, 1000.000000000000000 ) ;
#38227 = CARTESIAN_POINT ( 'NONE',  ( 2.500000000000030198, 65.00000000000000000, -90.00000000000000000 ) ) ;
#38228 = FACE_OUTER_BOUND ( 'NONE', #41975, .T. ) ;
#38229 = AXIS2_PLACEMENT_3D ( 'NONE', #65237, #49034, #13710 ) ;
#38230 = CARTESIAN_POINT ( 'NONE',  ( 57.50000000000000000, 7.041719095097280485E-15, -270.0000000000000000 ) ) ;
#38231 = CARTESIAN_POINT ( 'NONE',  ( 97.30629616937498838, 90.00000000000002842, 77.26031250086714408 ) ) ;
#38232 = CIRCLE ( 'NONE', #33388, 16.00000000000000000 ) ;
#38233 = DIRECTION ( 'NONE',  ( 1.000000000000000000, 0.000000000000000000, -0.000000000000000000 ) ) ;
#38234 = CARTESIAN_POINT ( 'NONE',  ( 96.32499999999997442, 92.29496732002878900, 86.69270833506763552 ) ) ;
#38235 = CARTESIAN_POINT ( 'NONE',  ( -12.50000000000000000, 1.530808498934191521E-15, -4.400000000000001243 ) ) ;
#38236 = CYLINDRICAL_SURFACE ( 'NONE', #68848, 77.49899999999999523 ) ;
#38237 = FACE_OUTER_BOUND ( 'NONE', #45137, .T. ) ;
#38238 = CARTESIAN_POINT ( 'NONE',  ( -97.64999999999996305, -209.9999999999999716, 86.82500000000000284 ) ) ;
#38239 = DIRECTION ( 'NONE',  ( -1.000000000000000000, -0.000000000000000000, 0.000000000000000000 ) ) ;
#38240 = PLANE ( 'NONE',  #69790 ) ;
#38241 = AXIS2_PLACEMENT_3D ( 'NONE', #37040, #8840, #43446 ) ;
#38242 = ORIENTED_EDGE ( 'NONE', *, *, #55783, .T. ) ;
#38243 = CARTESIAN_POINT ( 'NONE',  ( -97.30629616937501680, 90.00000000000004263, 81.38781250086714181 ) ) ;
#38244 = CARTESIAN_POINT ( 'NONE',  ( -10.00000000000000000, 0.000000000000000000, 0.000000000000000000 ) ) ;
#38245 = AXIS2_PLACEMENT_3D ( 'NONE', #64734, #48177, #47802 ) ;
#38246 = AXIS2_PLACEMENT_3D ( 'NONE', #71816, #54909, #25965 ) ;
#38247 = AXIS2_PLACEMENT_3D ( 'NONE', #14288, #67937, #37607 ) ;
#38248 = CARTESIAN_POINT ( 'NONE',  ( -12.50000000000000000, -132.5000000000000000, 40.00000000000000000 ) ) ;
#38249 = EDGE_LOOP ( 'NONE', ( #73167, #50799, #50969, #41603, #25375 ) ) ;
#38250 = AXIS2_PLACEMENT_3D ( 'NONE', #42149, #41398, #479 ) ;
#38251 =( BOUNDED_CURVE ( )  B_SPLINE_CURVE ( 2, ( #26438, #14034, #36234, #13668, #36603, #14417, #37364 ),
 .UNSPECIFIED., .F., .F. ) 
 B_SPLINE_CURVE_WITH_KNOTS ( ( 3, 2, 2, 3 ),
 ( 0.8466920362367558184, 0.8537476304467666033, 0.8608033959876488783, 0.8678591737214820245 ),
 .UNSPECIFIED. ) 
 CURVE ( )  GEOMETRIC_REPRESENTATION_ITEM ( )  RATIONAL_B_SPLINE_CURVE ( ( 0.9999934937104038024, 0.8660286570082328383, 1.000000000000000000, 0.8660254037844387076, 1.000000000000000000, 0.8660254037844387076, 1.000000000000000000 ) ) 
 REPRESENTATION_ITEM ( '' )  );
#38252 = DIRECTION ( 'NONE',  ( -1.000000000000000000, 0.000000000000000000, -0.000000000000000000 ) ) ;
#38253 = CARTESIAN_POINT ( 'NONE',  ( 10.00000000000000000, 0.000000000000000000, 0.000000000000000000 ) ) ;
#38254 = CARTESIAN_POINT ( 'NONE',  ( 26.50000000000000355, -120.0000000000000000, -80.00000000000000000 ) ) ;
#38255 = ADVANCED_FACE ( 'NONE', ( #17650 ), #52968, .F. ) ;
#38256 = CARTESIAN_POINT ( 'NONE',  ( 97.64999999989933599, 90.00002309722570715, 83.41187580057898288 ) ) ;
#38257 = CARTESIAN_POINT ( 'NONE',  ( 95.00000000000000000, -212.6630814284392557, 77.26031250086714408 ) ) ;
#38258 = EDGE_CURVE ( 'NONE', #25904, #54110, #63228, .T. ) ;
#38259 = EDGE_LOOP ( 'NONE', ( #72373, #24496, #15783, #62746 ) ) ;
#38260 = EDGE_CURVE ( 'NONE', #49339, #7677, #39226, .T. ) ;
#38261 = EDGE_LOOP ( 'NONE', ( #64048, #55284, #71930, #62910 ) ) ;
#38262 = AXIS2_PLACEMENT_3D ( 'NONE', #48284, #3922, #21171 ) ;
#38263 = FACE_OUTER_BOUND ( 'NONE', #73681, .T. ) ;
#38264 = CARTESIAN_POINT ( 'NONE',  ( 0.000000000000000000, 29.81001611431009479, 22.74946021919143391 ) ) ;
#38265 = DIRECTION ( 'NONE',  ( -0.9966891607226785466, -0.08130631524010122069, 0.000000000000000000 ) ) ;
#38266 = CYLINDRICAL_SURFACE ( 'NONE', #26684, 31.99999999999999289 ) ;
#38267 = CIRCLE ( 'NONE', #64687, 3.299999999999983391 ) ;
#38268 = CARTESIAN_POINT ( 'NONE',  ( 10.00000000000000000, -71.87247863392443037, 39.47590169984818687 ) ) ;
#38269 = CARTESIAN_POINT ( 'NONE',  ( 96.15314808468750130, -211.9973110713294489, 77.31322916753381946 ) ) ;
#38270 = VECTOR ( 'NONE', #63247, 1000.000000000000000 ) ;
#38271 = AXIS2_PLACEMENT_3D ( 'NONE', #40943, #46571, #17266 ) ;
#38272 = EDGE_CURVE ( 'NONE', #42183, #7988, #45242, .T. ) ;
#38273 = VERTEX_POINT ( 'NONE', #36403 ) ;
#38274 = LINE ( 'NONE', #4832, #14303 ) ;
#38275 = ORIENTED_EDGE ( 'NONE', *, *, #19019, .F. ) ;
#38276 = ORIENTED_EDGE ( 'NONE', *, *, #71288, .T. ) ;
#38277 = CYLINDRICAL_SURFACE ( 'NONE', #30960, 31.99999999999999289 ) ;
#38278 = VECTOR ( 'NONE', #24457, 1000.000000000000000 ) ;
#38279 = CARTESIAN_POINT ( 'NONE',  ( 10.00000000000000000, 20.41045688087930898, -72.35160999960793049 ) ) ;
#38280 = AXIS2_PLACEMENT_3D ( 'NONE', #31953, #66554, #3415 ) ;
#38281 = ORIENTED_EDGE ( 'NONE', *, *, #55423, .T. ) ;
#38282 = DIRECTION ( 'NONE',  ( -1.000000000000000000, -0.000000000000000000, 0.000000000000000000 ) ) ;
#38283 = CARTESIAN_POINT ( 'NONE',  ( 93.67500000000001137, -207.7050326799711968, 80.44854166840097776 ) ) ;
#38284 = CARTESIAN_POINT ( 'NONE',  ( 96.32499999999997442, 92.29496732002878900, 82.16833333333332234 ) ) ;
#38285 = ORIENTED_EDGE ( 'NONE', *, *, #6317, .T. ) ;
#38286 = CARTESIAN_POINT ( 'NONE',  ( -4.653126046682595884, -146.1313684676804314, 5.500000000000000000 ) ) ;
#38287 = ORIENTED_EDGE ( 'NONE', *, *, #73845, .T. ) ;
#38288 = ADVANCED_FACE ( 'NONE', ( #12004 ), #2242, .F. ) ;
#38289 = EDGE_LOOP ( 'NONE', ( #49681, #18286, #19143, #47099 ) ) ;
#38290 = CARTESIAN_POINT ( 'NONE',  ( 97.65000000000000568, 91.52997821335252127, 84.09979166840098230 ) ) ;
#38291 = CARTESIAN_POINT ( 'NONE',  ( -97.30629616937501680, 88.66845928578038638, 85.40947916753381719 ) ) ;
#38292 = CARTESIAN_POINT ( 'NONE',  ( 96.15314808468748708, 88.00268892867053694, 80.96447916753380980 ) ) ;
#38293 = ADVANCED_FACE ( 'NONE', ( #48431 ), #53703, .F. ) ;
#38294 = ORIENTED_EDGE ( 'NONE', *, *, #29369, .T. ) ;
#38295 = LINE ( 'NONE', #19239, #34070 ) ;
#38296 = CIRCLE ( 'NONE', #9472, 77.49900000000000944 ) ;
#38297 = CARTESIAN_POINT ( 'NONE',  ( -94.99999999999997158, -209.9999999999999716, 90.00000000000000000 ) ) ;
#38298 = ORIENTED_EDGE ( 'NONE', *, *, #42427, .T. ) ;
#38299 = CARTESIAN_POINT ( 'NONE',  ( 10.00000000000000000, 71.87247863392470038, -39.47590169984768238 ) ) ;
#38300 = ADVANCED_FACE ( 'NONE', ( #9694 ), #25139, .T. ) ;
#38301 = EDGE_CURVE ( 'NONE', #70504, #66872, #16416, .T. ) ;
#38302 = VECTOR ( 'NONE', #37254, 1000.000000000000000 ) ;
#38303 = AXIS2_PLACEMENT_3D ( 'NONE', #18763, #48452, #40980 ) ;
#38304 = ORIENTED_EDGE ( 'NONE', *, *, #1925, .F. ) ;
#38305 = VERTEX_POINT ( 'NONE', #43560 ) ;
#38306 = CARTESIAN_POINT ( 'NONE',  ( 10.00000000000000000, 0.000000000000000000, 0.000000000000000000 ) ) ;
#38307 = ORIENTED_EDGE ( 'NONE', *, *, #50908, .T. ) ;
#38308 = EDGE_CURVE ( 'NONE', #43291, #64554, #26011, .T. ) ;
#38309 = CARTESIAN_POINT ( 'NONE',  ( -96.32499999999996021, -207.7050326799711968, 81.08354166840096866 ) ) ;
#38310 = COLOUR_RGB ( '', 0.40784314, 0.44705882, 0.49803922) ;
#38311 = CARTESIAN_POINT ( 'NONE',  ( 97.64999999999997726, 88.47002178664753558, 87.80395833506763381 ) ) ;
#38312 = VERTEX_POINT ( 'NONE', #72098 ) ;
#38313 = DIRECTION ( 'NONE',  ( 0.000000000000000000, 0.000000000000000000, 1.000000000000000000 ) ) ;
#38314 = CARTESIAN_POINT ( 'NONE',  ( -97.30629616937497417, -208.6684592857803011, 78.15989583420048348 ) ) ;
#38315 = ORIENTED_EDGE ( 'NONE', *, *, #10771, .T. ) ;
#38316 = CARTESIAN_POINT ( 'NONE',  ( -97.65000000000001990, 90.00000000000004263, 86.18999999999999773 ) ) ;
#38317 = DIRECTION ( 'NONE',  ( 0.000000000000000000, 0.000000000000000000, 1.000000000000000000 ) ) ;
#38318 = CYLINDRICAL_SURFACE ( 'NONE', #29728, 42.00000000000000000 ) ;
#38319 = DIRECTION ( 'NONE',  ( 0.000000000000000000, 0.3090169943749482839, -0.9510565162951533091 ) ) ;
#38320 = EDGE_CURVE ( 'NONE', #29404, #20435, #56009, .T. ) ;
#38321 = CARTESIAN_POINT ( 'NONE',  ( 0.000000000000000000, 0.000000000000000000, 20.00000000000000000 ) ) ;
#38322 = CARTESIAN_POINT ( 'NONE',  ( -92.35000000000003695, 90.00000000000004263, 90.00000000000000000 ) ) ;
#38323 = CARTESIAN_POINT ( 'NONE',  ( 92.69370383062498320, 91.33154071421968467, 87.68489583420047495 ) ) ;
#38324 = DIRECTION ( 'NONE',  ( -1.000000000000000000, -0.000000000000000000, -0.000000000000000000 ) ) ;
#38325 = CARTESIAN_POINT ( 'NONE',  ( 11.99999999999999822, 75.11764819372142199, 2.946379043147685728 ) ) ;
#38326 = CARTESIAN_POINT ( 'NONE',  ( -97.64999999960637922, 90.00002930319634231, 82.45844277051273252 ) ) ;
#38327 = DIRECTION ( 'NONE',  ( 0.000000000000000000, 0.1564344650402244852, 0.9876883405951387696 ) ) ;
#38328 = AXIS2_PLACEMENT_3D ( 'NONE', #17765, #70000, #29046 ) ;
#38329 = FACE_OUTER_BOUND ( 'NONE', #36041, .T. ) ;
#38330 = CARTESIAN_POINT ( 'NONE',  ( 15.00000000000000000, 18.84667830672579569, -18.68964196561269375 ) ) ;
#38331 = CARTESIAN_POINT ( 'NONE',  ( 97.64999999999999147, -209.9999999999999716, 75.07749999999998636 ) ) ;
#38332 = AXIS2_PLACEMENT_3D ( 'NONE', #36915, #13611, #48926 ) ;
#38333 = CARTESIAN_POINT ( 'NONE',  ( 92.35001469846373823, 91.52998669951453792, 76.05645774805350356 ) ) ;
#38334 = CIRCLE ( 'NONE', #71908, 16.00000000000000000 ) ;
#38335 = AXIS2_PLACEMENT_3D ( 'NONE', #60454, #32963, #61561 ) ;
#38336 = DIRECTION ( 'NONE',  ( -1.000000000000000000, 0.000000000000000000, 0.000000000000000000 ) ) ;
#38338 = VECTOR ( 'NONE', #63873, 1000.000000000000000 ) ;
#38337 = FACE_OUTER_BOUND ( 'NONE', #4650, .T. ) ;
#38339 = CARTESIAN_POINT ( 'NONE',  ( -92.34999999999999432, -211.5299782133524502, 83.91458333333333997 ) ) ;
#38340 = CIRCLE ( 'NONE', #7099, 12.79999999999999893 ) ;
#38341 = CARTESIAN_POINT ( 'NONE',  ( 11.99999999999999822, 0.000000000000000000, 0.000000000000000000 ) ) ;
#38342 = DIRECTION ( 'NONE',  ( 0.000000000000000000, -0.9876883405951359940, -0.1564344650402420822 ) ) ;
#38343 = CARTESIAN_POINT ( 'NONE',  ( 5.000000000000002665, 71.21200624218852226, -40.65526001592539984 ) ) ;
#38344 = SURFACE_STYLE_FILL_AREA ( #9392 ) ;
#38345 = CARTESIAN_POINT ( 'NONE',  ( 0.000000000000000000, 0.000000000000000000, 0.000000000000000000 ) ) ;
#38346 = CIRCLE ( 'NONE', #57578, 0.5999999999999928724 ) ;
#38347 = EDGE_CURVE ( 'NONE', #44140, #58013, #57209, .T. ) ;
#38348 = AXIS2_PLACEMENT_3D ( 'NONE', #8438, #36999, #8798 ) ;
#38349 = VECTOR ( 'NONE', #41630, 1000.000000000000227 ) ;
#38350 = EDGE_CURVE ( 'NONE', #27866, #42410, #54827, .T. ) ;
#38351 = ORIENTED_EDGE ( 'NONE', *, *, #31815, .F. ) ;
#38352 = AXIS2_PLACEMENT_3D ( 'NONE', #50095, #38838, #57248 ) ;
#38353 = EDGE_CURVE ( 'NONE', #975, #30680, #13833, .T. ) ;
#38354 = ORIENTED_EDGE ( 'NONE', *, *, #11612, .F. ) ;
#38355 = VECTOR ( 'NONE', #54525, 1000.000000000000000 ) ;
#38356 = EDGE_CURVE ( 'NONE', #67975, #63433, #36789, .T. ) ;
#38357 = DIRECTION ( 'NONE',  ( 0.000000000000000000, 0.9876883405951382144, -0.1564344650402276493 ) ) ;
#38358 = DIRECTION ( 'NONE',  ( 0.000000000000000000, 0.000000000000000000, 1.000000000000000000 ) ) ;
#38359 = ORIENTED_EDGE ( 'NONE', *, *, #20009, .T. ) ;
#38360 = CARTESIAN_POINT ( 'NONE',  ( 97.30629616937498838, -211.3315407142195852, 81.01739583420048518 ) ) ;
#38361 = CARTESIAN_POINT ( 'NONE',  ( 93.84685191531249870, -208.0026889286704943, 84.61572916753381435 ) ) ;
#38362 = VERTEX_POINT ( 'NONE', #2619 ) ;
#38363 = CARTESIAN_POINT ( 'NONE',  ( 97.30629616937498838, -209.9999999999999716, 85.03906250086714635 ) ) ;
#38364 = ORIENTED_EDGE ( 'NONE', *, *, #49729, .F. ) ;
#38365 = DIRECTION ( 'NONE',  ( 1.000000000000000000, -7.571541139944063212E-15, -2.603472992745718826E-14 ) ) ;
#38366 = ORIENTED_EDGE ( 'NONE', *, *, #24208, .F. ) ;
#38367 = CARTESIAN_POINT ( 'NONE',  ( -96.15314808468752972, 91.99731107132950569, 76.99572916753382401 ) ) ;
#38368 = ORIENTED_EDGE ( 'NONE', *, *, #44652, .T. ) ;
#38369 = EDGE_CURVE ( 'NONE', #53279, #14313, #20217, .T. ) ;
#38370 = ORIENTED_EDGE ( 'NONE', *, *, #63581, .F. ) ;
#38371 = CARTESIAN_POINT ( 'NONE',  ( 10.00000000000000000, 6.903761155837774943, 77.19088730480525840 ) ) ;
#38372 = ORIENTED_EDGE ( 'NONE', *, *, #43333, .T. ) ;
#38373 = CARTESIAN_POINT ( 'NONE',  ( -10.00000000000000000, 0.000000000000000000, 0.000000000000000000 ) ) ;
#38374 = DIRECTION ( 'NONE',  ( -1.000000000000000000, -0.000000000000000000, 0.000000000000000000 ) ) ;
#38375 = ADVANCED_FACE ( 'NONE', ( #59723 ), #3711, .T. ) ;
#38376 = ORIENTED_EDGE ( 'NONE', *, *, #3249, .T. ) ;
#38377 = CYLINDRICAL_SURFACE ( 'NONE', #2278, 32.00000000000000000 ) ;
#38378 = ORIENTED_EDGE ( 'NONE', *, *, #16245, .T. ) ;
#38379 = CARTESIAN_POINT ( 'NONE',  ( 0.000000000000000000, -15.48615015657556171, -39.04073710021360455 ) ) ;
#38380 = AXIS2_PLACEMENT_3D ( 'NONE', #49577, #48841, #66876 ) ;
#38381 = ORIENTED_EDGE ( 'NONE', *, *, #26203, .F. ) ;
#38382 = CIRCLE ( 'NONE', #66032, 82.00000000000000000 ) ;
#38383 = AXIS2_PLACEMENT_3D ( 'NONE', #2852, #65242, #49417 ) ;
#38384 = ORIENTED_EDGE ( 'NONE', *, *, #73580, .T. ) ;
#38385 = VERTEX_POINT ( 'NONE', #14586 ) ;
#38386 = DIRECTION ( 'NONE',  ( 1.000000000000000000, 0.000000000000000000, 0.000000000000000000 ) ) ;
#38387 = EDGE_CURVE ( 'NONE', #43278, #39841, #42797, .T. ) ;
#38388 = ADVANCED_FACE ( 'NONE', ( #65731 ), #31870, .F. ) ;
#38389 = CONTEXT_DEPENDENT_SHAPE_REPRESENTATION ( #31590, #7463 ) ;
#38390 = DIRECTION ( 'NONE',  ( -1.000000000000000000, -0.000000000000000000, -0.000000000000000000 ) ) ;
#38391 = ORIENTED_EDGE ( 'NONE', *, *, #23887, .F. ) ;
#38392 = VERTEX_POINT ( 'NONE', #49171 ) ;
#38393 = AXIS2_PLACEMENT_3D ( 'NONE', #21573, #1203, #62184 ) ;
#38394 = ORIENTED_EDGE ( 'NONE', *, *, #30619, .T. ) ;
#38395 = DIRECTION ( 'NONE',  ( -0.000000000000000000, -0.000000000000000000, 1.000000000000000000 ) ) ;
#38396 = DIRECTION ( 'NONE',  ( -1.000000000000000000, -0.000000000000000000, 0.000000000000000000 ) ) ;
#38397 = CARTESIAN_POINT ( 'NONE',  ( -95.00000000000002842, 92.66308142843932671, 75.67281250086716682 ) ) ;
#38398 = ORIENTED_EDGE ( 'NONE', *, *, #61828, .F. ) ;
#38399 = CARTESIAN_POINT ( 'NONE',  ( 92.69370383062498320, 90.00000000000002842, 77.57781250086713953 ) ) ;
#38400 = EDGE_LOOP ( 'NONE', ( #3166, #26835, #55459, #63660 ) ) ;
#38401 = DIRECTION ( 'NONE',  ( -1.000000000000000000, 0.000000000000000000, -0.000000000000000000 ) ) ;
#38402 = DIRECTION ( 'NONE',  ( 0.000000000000000000, 0.000000000000000000, 1.000000000000000000 ) ) ;
#38403 = CARTESIAN_POINT ( 'NONE',  ( 96.82636346428390084, -211.7597761561304708, 74.93163452119475210 ) ) ;
#38404 = CYLINDRICAL_SURFACE ( 'NONE', #65610, 31.99999999999998579 ) ;
#38405 = CARTESIAN_POINT ( 'NONE',  ( 10.00000000000000000, 59.03961581697465277, -46.53671651293886669 ) ) ;
#38406 = CARTESIAN_POINT ( 'NONE',  ( -94.99999999999997158, -212.6630814284392557, 80.27656250086714351 ) ) ;
#38407 = AXIS2_PLACEMENT_3D ( 'NONE', #32192, #31461, #71678 ) ;
#38408 = CYLINDRICAL_SURFACE ( 'NONE', #6277, 31.99999999999998579 ) ;
#38409 = DIRECTION ( 'NONE',  ( -3.061616997868382648E-16, -1.000000000000000000, 0.000000000000000000 ) ) ;
#38410 = CARTESIAN_POINT ( 'NONE',  ( 0.000000000000000000, 0.000000000000000000, -175.0000000000000000 ) ) ;
#38411 = VERTEX_POINT ( 'NONE', #49537 ) ;
#38412 = AXIS2_PLACEMENT_3D ( 'NONE', #13962, #25628, #41440 ) ;
#38413 = VECTOR ( 'NONE', #5509, 1000.000000000000114 ) ;
#38414 = EDGE_LOOP ( 'NONE', ( #52671, #47345, #15468, #34517 ) ) ;
#38415 = CARTESIAN_POINT ( 'NONE',  ( 100.0010000000000474, -65.00000000000002842, -290.0000000000000568 ) ) ;
#38416 = AXIS2_PLACEMENT_3D ( 'NONE', #41429, #12110, #35049 ) ;
#38417 = CIRCLE ( 'NONE', #52798, 77.49900000000000944 ) ;
#38418 = FACE_OUTER_BOUND ( 'NONE', #5597, .T. ) ;
#38419 = CARTESIAN_POINT ( 'NONE',  ( 93.26435506835497335, -208.2604367189442769, 74.87701898318914573 ) ) ;
#38420 = CARTESIAN_POINT ( 'NONE',  ( -93.84685191531254134, 91.99731107132950569, 83.08114583420048405 ) ) ;
#38421 = DIRECTION ( 'NONE',  ( -1.000000000000000000, 0.000000000000000000, -0.000000000000000000 ) ) ;
#38422 = DIRECTION ( 'NONE',  ( 0.000000000000000000, 0.3826834323650840086, 0.9238795325112891810 ) ) ;
#38423 = ORIENTED_EDGE ( 'NONE', *, *, #37454, .T. ) ;
#38424 = CARTESIAN_POINT ( 'NONE',  ( 10.00000000000000000, 22.48208911017500355, 35.47612816024531668 ) ) ;
#38425 = DIRECTION ( 'NONE',  ( -1.000000000000000000, 0.000000000000000000, 0.000000000000000000 ) ) ;
#38426 = LINE ( 'NONE', #49684, #34545 ) ;
#38427 = CARTESIAN_POINT ( 'NONE',  ( 0.000000000000000000, -34.94270380257692921, 74.18225833017875459 ) ) ;
#38428 = DIRECTION ( 'NONE',  ( 0.000000000000000000, -0.9723699203976789995, 0.2334453638558956212 ) ) ;
#38429 = CARTESIAN_POINT ( 'NONE',  ( -93.84685191531247028, -211.9973110713294489, 78.58322916753382970 ) ) ;
#38430 = CARTESIAN_POINT ( 'NONE',  ( -10.00000000000000000, 0.000000000000000000, 0.000000000000000000 ) ) ;
#38431 = AXIS2_PLACEMENT_3D ( 'NONE', #37750, #61424, #49745 ) ;
#38432 = ORIENTED_EDGE ( 'NONE', *, *, #15502, .F. ) ;
#38433 = CARTESIAN_POINT ( 'NONE',  ( 2.369999999999999662, 0.000000000000000000, 0.000000000000000000 ) ) ;
#38434 = ADVANCED_FACE ( 'NONE', ( #72463 ), #20967, .T. ) ;
#38435 = DIRECTION ( 'NONE',  ( 0.000000000000000000, -0.9781476007338043566, 0.2079116908177651712 ) ) ;
#38436 = DIRECTION ( 'NONE',  ( -1.000000000000000000, 0.000000000000000000, 0.000000000000000000 ) ) ;
#38437 = ORIENTED_EDGE ( 'NONE', *, *, #28839, .F. ) ;
#38438 = CARTESIAN_POINT ( 'NONE',  ( 94.99999999999998579, 93.05995642670504253, 77.22062500173429100 ) ) ;
#38439 = CIRCLE ( 'NONE', #44399, 77.49900000000000944 ) ;
#38441 = ADVANCED_FACE ( 'NONE', ( #38263 ), #61204, .F. ) ;
#38440 = DIRECTION ( 'NONE',  ( 0.000000000000000000, 0.000000000000000000, 1.000000000000000000 ) ) ;
#38442 = EDGE_CURVE ( 'NONE', #24481, #32344, #13439, .T. ) ;
#38443 = VECTOR ( 'NONE', #20996, 1000.000000000000000 ) ;
#38444 = CARTESIAN_POINT ( 'NONE',  ( 10.00000000000000000, 55.19960302592141232, -51.03279382321027668 ) ) ;
#38445 = VERTEX_POINT ( 'NONE', #10060 ) ;
#38446 = EDGE_CURVE ( 'NONE', #20162, #46914, #27342, .T. ) ;
#38447 = DIRECTION ( 'NONE',  ( 0.000000000000000000, -0.7071067811865536790, 0.7071067811865414665 ) ) ;
#38448 = EDGE_LOOP ( 'NONE', ( #28734, #69445, #49837, #72772 ) ) ;
#38449 = EDGE_CURVE ( 'NONE', #63015, #57727, #72834, .T. ) ;
#38450 = DIRECTION ( 'NONE',  ( -1.000000000000000000, -0.000000000000000000, -0.000000000000000000 ) ) ;
#38451 = PLANE ( 'NONE',  #12354 ) ;
#38452 = ORIENTED_EDGE ( 'NONE', *, *, #17223, .T. ) ;
#38453 = DIRECTION ( 'NONE',  ( -0.3853207896976547642, 0.9227826878668540234, 0.000000000000000000 ) ) ;
#38454 = AXIS2_PLACEMENT_3D ( 'NONE', #53851, #14370, #63767 ) ;
#38455 = ORIENTED_EDGE ( 'NONE', *, *, #34614, .F. ) ;
#38456 = CARTESIAN_POINT ( 'NONE',  ( -12.50000000000000000, -107.5000000000000000, -40.00000000000000000 ) ) ;
#38457 = VECTOR ( 'NONE', #53739, 1000.000000000000114 ) ;
#38458 = CYLINDRICAL_SURFACE ( 'NONE', #57666, 31.99999999999998579 ) ;
#38459 = VERTEX_POINT ( 'NONE', #57052 ) ;
#38460 = ORIENTED_EDGE ( 'NONE', *, *, #23084, .F. ) ;
#38461 = VECTOR ( 'NONE', #48974, 1000.000000000000000 ) ;
#38462 = ORIENTED_EDGE ( 'NONE', *, *, #25299, .F. ) ;
#38463 = CARTESIAN_POINT ( 'NONE',  ( 0.000000000000000000, -59.46389618801929089, -49.70050353004953081 ) ) ;
#38464 = EDGE_CURVE ( 'NONE', #5801, #49572, #27054, .T. ) ;
#38465 = EDGE_CURVE ( 'NONE', #72369, #34053, #4824, .T. ) ;
#38466 = VERTEX_POINT ( 'NONE', #26972 ) ;
#38467 = ORIENTED_EDGE ( 'NONE', *, *, #74077, .T. ) ;
#38468 =( BOUNDED_CURVE ( )  B_SPLINE_CURVE ( 2, ( #65642, #26138, #55467, #25036, #47977, #48340, #71628 ),
 .UNSPECIFIED., .F., .F. ) 
 B_SPLINE_CURVE_WITH_KNOTS ( ( 3, 2, 2, 3 ),
 ( 0.3749999999999998335, 0.3819444444444441977, 0.3888888888888886730, 0.3958333333333330373 ),
 .UNSPECIFIED. ) 
 CURVE ( )  GEOMETRIC_REPRESENTATION_ITEM ( )  RATIONAL_B_SPLINE_CURVE ( ( 1.000000000000003109, 0.8660254037844354880, 1.000000000000000000, 0.8660254037844387076, 1.000000000000000000, 0.8660254037844440367, 0.9999999999999946709 ) ) 
 REPRESENTATION_ITEM ( '' )  );
#38469 = CARTESIAN_POINT ( 'NONE',  ( 92.69370383062498320, 88.66845928578037217, 77.15447916753382174 ) ) ;
#38470 = DIRECTION ( 'NONE',  ( -1.000000000000000000, 0.000000000000000000, 0.000000000000000000 ) ) ;
#38471 = CARTESIAN_POINT ( 'NONE',  ( -6.782329983125270800, 10.49999999999999467, -145.0000000000000000 ) ) ;
#38472 = VERTEX_POINT ( 'NONE', #55926 ) ;
#38473 = ORIENTED_EDGE ( 'NONE', *, *, #39207, .T. ) ;
#38474 = ORIENTED_EDGE ( 'NONE', *, *, #41843, .F. ) ;
#38475 = CARTESIAN_POINT ( 'NONE',  ( 96.15314808468748708, 91.99731107132950569, 86.89114583420047211 ) ) ;
#38476 = ORIENTED_EDGE ( 'NONE', *, *, #5244, .F. ) ;
#38477 = CARTESIAN_POINT ( 'NONE',  ( 96.15314808468750130, -211.9973110713294489, 84.13947916753380696 ) ) ;
#38478 = ADVANCED_FACE ( 'NONE', ( #68331 ), #72822, .T. ) ;
#38479 = ADVANCED_FACE ( 'NONE', ( #56307 ), #73206, .T. ) ;
#38480 = DIRECTION ( 'NONE',  ( 1.000000000000000000, 0.000000000000000000, 0.000000000000000000 ) ) ;
#38481 = DIRECTION ( 'NONE',  ( 0.000000000000000000, 0.000000000000000000, 1.000000000000000000 ) ) ;
#38482 = CARTESIAN_POINT ( 'NONE',  ( -94.99999999999997158, -206.9400435732949575, 80.31624999999999659 ) ) ;
#38483 = DIRECTION ( 'NONE',  ( 0.000000000000000000, -0.9510565162951500895, -0.3090169943749583314 ) ) ;
#38484 = DIRECTION ( 'NONE',  ( -1.000000000000000000, -0.000000000000000000, -0.000000000000000000 ) ) ;
#38485 = DIRECTION ( 'NONE',  ( 1.000000000000000000, 0.000000000000000000, 0.000000000000000000 ) ) ;
#38486 = DIRECTION ( 'NONE',  ( 0.000000000000000000, -0.5877852522924802425, 0.8090169943749422332 ) ) ;
#38487 = CARTESIAN_POINT ( 'NONE',  ( -97.30629616937495996, -209.9999999999999716, 87.10281250086714522 ) ) ;
#38488 = CARTESIAN_POINT ( 'NONE',  ( -96.15314808468751551, 88.00268892867056536, 86.73239583420048859 ) ) ;
#38489 = ORIENTED_EDGE ( 'NONE', *, *, #46795, .F. ) ;
#38491 = CARTESIAN_POINT ( 'NONE',  ( -97.30629616937501680, 90.00000000000004263, 88.37281250086715545 ) ) ;
#38490 = CARTESIAN_POINT ( 'NONE',  ( 96.15314808468748708, 88.00268892867053694, 88.58447916753381435 ) ) ;
#38492 = VERTEX_POINT ( 'NONE', #51391 ) ;
#38493 = CARTESIAN_POINT ( 'NONE',  ( -10.00000000000000000, 0.000000000000000000, 0.000000000000000000 ) ) ;
#38494 = CARTESIAN_POINT ( 'NONE',  ( -1.734723475976807094E-14, 1.040834085586084257E-14, -45.00000000000000000 ) ) ;
#38495 = CARTESIAN_POINT ( 'NONE',  ( 0.000000000000000000, -12.93880638057260590, -76.41127070299285151 ) ) ;
#38496 = CARTESIAN_POINT ( 'NONE',  ( -97.65000000000007674, 91.52997821335253548, 86.77208333333334167 ) ) ;
#38497 = LINE ( 'NONE', #3204, #71508 ) ;
#38498 = CIRCLE ( 'NONE', #40863, 82.00000000000000000 ) ;
#38499 = DIRECTION ( 'NONE',  ( -1.000000000000000000, 0.000000000000000000, -0.000000000000000000 ) ) ;
#38500 = AXIS2_PLACEMENT_3D ( 'NONE', #59606, #46471, #7727 ) ;
#38501 = CARTESIAN_POINT ( 'NONE',  ( 0.000000000000000000, -22.64427369931148348, -30.00120703465229965 ) ) ;
#38502 = EDGE_LOOP ( 'NONE', ( #63674, #5303, #51820, #49720 ) ) ;
#38503 = ORIENTED_EDGE ( 'NONE', *, *, #4932, .T. ) ;
#38504 = CARTESIAN_POINT ( 'NONE',  ( -92.35000000000005116, 88.47002178664754979, 82.64458333333331552 ) ) ;
#38505 = FACE_OUTER_BOUND ( 'NONE', #65916, .T. ) ;
#38506 = LINE ( 'NONE', #5428, #20187 ) ;
#38507 = CYLINDRICAL_SURFACE ( 'NONE', #61263, 32.50000000000000000 ) ;
#38508 = DIRECTION ( 'NONE',  ( 1.000000000000000000, -7.571541139944063212E-15, -2.603472992745718826E-14 ) ) ;
#38509 = LINE ( 'NONE', #27594, #47154 ) ;
#38510 = CARTESIAN_POINT ( 'NONE',  ( 11.99999999999999822, 0.000000000000000000, 0.000000000000000000 ) ) ;
#38511 = CARTESIAN_POINT ( 'NONE',  ( 2.949999999999999734, 0.000000000000000000, 0.000000000000000000 ) ) ;
#38512 = VERTEX_POINT ( 'NONE', #67208 ) ;
#38513 = CARTESIAN_POINT ( 'NONE',  ( -97.30629616937501680, 90.00000000000004263, 82.02281250086714692 ) ) ;
#38514 = ADVANCED_FACE ( 'NONE', ( #74330 ), #61946, .T. ) ;
#38515 = DIRECTION ( 'NONE',  ( -1.000000000000000000, 0.000000000000000000, 0.000000000000000000 ) ) ;
#38516 = VECTOR ( 'NONE', #34419, 1000.000000000000000 ) ;
#38517 = LINE ( 'NONE', #61456, #24627 ) ;
#38518 = AXIS2_PLACEMENT_3D ( 'NONE', #73992, #55219, #9731 ) ;
#38519 = DIRECTION ( 'NONE',  ( 0.000000000000000000, 0.7431448254773862505, 0.6691306063588671194 ) ) ;
#38520 = CARTESIAN_POINT ( 'NONE',  ( 11.99999999999999822, -2.543863470248965086, 81.96053171279902472 ) ) ;
#38521 = DIRECTION ( 'NONE',  ( -0.000000000000000000, 0.4067366430757998752, 0.9135454576426010886 ) ) ;
#38522 = DIRECTION ( 'NONE',  ( -0.7585478161175723821, -0.6516173805718057377, 0.000000000000000000 ) ) ;
#38523 = EDGE_CURVE ( 'NONE', #16853, #26601, #38644, .T. ) ;
#38524 =( LENGTH_UNIT ( ) NAMED_UNIT ( * ) SI_UNIT ( .MILLI., .METRE. ) );
#38525 = AXIS2_PLACEMENT_3D ( 'NONE', #60087, #8567, #31485 ) ;
#38526 = DIRECTION ( 'NONE',  ( 0.000000000000000000, 0.000000000000000000, 1.000000000000000000 ) ) ;
#38527 = EDGE_CURVE ( 'NONE', #9035, #49393, #32060, .T. ) ;
#38528 = EDGE_CURVE ( 'NONE', #2356, #50224, #70999, .T. ) ;
#38529 = CARTESIAN_POINT ( 'NONE',  ( 93.84685191531248449, 91.99731107132950569, 81.44072916753381719 ) ) ;
#38530 = ADVANCED_FACE ( 'NONE', ( #4443 ), #16446, .T. ) ;
#38531 = CARTESIAN_POINT ( 'NONE',  ( -97.30629616937495996, -209.9999999999999716, 84.08656250086716000 ) ) ;
#38532 = DIRECTION ( 'NONE',  ( -1.000000000000000000, -0.000000000000000000, -0.000000000000000000 ) ) ;
#38533 = ORIENTED_EDGE ( 'NONE', *, *, #15302, .T. ) ;
#38534 = CARTESIAN_POINT ( 'NONE',  ( 10.00000000000000000, 0.000000000000000000, 0.000000000000000000 ) ) ;
#38535 = CARTESIAN_POINT ( 'NONE',  ( -94.99999999999997158, -206.9400435732949575, 78.41125000000000966 ) ) ;
#38536 = CARTESIAN_POINT ( 'NONE',  ( 96.32499999999998863, -207.7050326799711968, 78.35833333333333428 ) ) ;
#38537 = ADVANCED_FACE ( 'NONE', ( #16826 ), #10812, .T. ) ;
#38538 = CARTESIAN_POINT ( 'NONE',  ( -97.30629616937501680, 91.33154071421968467, 77.68364583420047609 ) ) ;
#38539 = CARTESIAN_POINT ( 'NONE',  ( 92.69370383062501162, -211.3315407142195852, 82.07572916753380809 ) ) ;
#38540 = ORIENTED_EDGE ( 'NONE', *, *, #19522, .F. ) ;
#38541 = CARTESIAN_POINT ( 'NONE',  ( 0.000000000000000000, 0.000000000000000000, 0.000000000000000000 ) ) ;
#38542 = EDGE_LOOP ( 'NONE', ( #41068, #47161, #22718, #24254 ) ) ;
#38543 = EDGE_CURVE ( 'NONE', #52056, #14449, #34473, .T. ) ;
#38544 = CARTESIAN_POINT ( 'NONE',  ( 10.00000000000000000, 71.27951684758026829, 30.41916302227139113 ) ) ;
#38545 = VERTEX_POINT ( 'NONE', #18292 ) ;
#38546 = AXIS2_PLACEMENT_3D ( 'NONE', #44253, #55533, #10030 ) ;
#38547 = AXIS2_PLACEMENT_3D ( 'NONE', #67805, #10286, #28310 ) ;
#38549 = AXIS2_PLACEMENT_3D ( 'NONE', #61822, #28326, #34345 ) ;
#38548 = CARTESIAN_POINT ( 'NONE',  ( 0.000000000000000000, -80.28980883073747066, -16.65972982745018172 ) ) ;
#38550 = ORIENTED_EDGE ( 'NONE', *, *, #38792, .T. ) ;
#38551 = EDGE_LOOP ( 'NONE', ( #31408, #2833, #24350, #22579, #67400 ) ) ;
#38552 = CARTESIAN_POINT ( 'NONE',  ( 95.00000000000000000, -207.3369185715606307, 75.67281250086715261 ) ) ;
#38553 = EDGE_CURVE ( 'NONE', #30220, #7439, #54883, .T. ) ;
#38554 = CARTESIAN_POINT ( 'NONE',  ( 0.000000000000000000, 0.000000000000000000, 0.000000000000000000 ) ) ;
#38555 = EDGE_CURVE ( 'NONE', #70364, #70056, #24883, .T. ) ;
#38556 = CARTESIAN_POINT ( 'NONE',  ( 0.000000000000000000, -27.75498641678720446, -31.52238457039628727 ) ) ;
#38557 = FACE_OUTER_BOUND ( 'NONE', #19152, .T. ) ;
#38558 = CARTESIAN_POINT ( 'NONE',  ( 93.84685191531248449, 88.00268892867053694, 86.73239583420048859 ) ) ;
#38559 = ADVANCED_FACE ( 'NONE', ( #69426 ), #318, .T. ) ;
#38560 = CARTESIAN_POINT ( 'NONE',  ( 92.35000000009272014, 90.00001381026685010, 80.55392363656929433 ) ) ;
#38561 = CARTESIAN_POINT ( 'NONE',  ( 95.00000000000000000, -206.9400435732949575, 78.41125000000000966 ) ) ;
#38562 =( GEOMETRIC_REPRESENTATION_CONTEXT ( 3 ) GLOBAL_UNCERTAINTY_ASSIGNED_CONTEXT ( ( #23309 ) ) GLOBAL_UNIT_ASSIGNED_CONTEXT ( ( #52190, #27783, #372 ) ) REPRESENTATION_CONTEXT ( 'NONE', 'WORKASPACE' ) );
#38563 = VERTEX_POINT ( 'NONE', #7009 ) ;
#38564 = VERTEX_POINT ( 'NONE', #58515 ) ;
#38565 = VERTEX_POINT ( 'NONE', #30307 ) ;
#38566 = ORIENTED_EDGE ( 'NONE', *, *, #38446, .T. ) ;
#38567 = CARTESIAN_POINT ( 'NONE',  ( 0.000000000000000000, 23.50000000000000000, 1.499999999999997780 ) ) ;
#38568 = VECTOR ( 'NONE', #20831, 1000.000000000000000 ) ;
#38569 = AXIS2_PLACEMENT_3D ( 'NONE', #1464, #28880, #52538 ) ;
#38570 = DIRECTION ( 'NONE',  ( -1.000000000000000000, -0.000000000000000000, 0.000000000000000000 ) ) ;
#38571 = DIRECTION ( 'NONE',  ( -1.000000000000000000, -0.000000000000000000, -0.000000000000000000 ) ) ;
#38572 = AXIS2_PLACEMENT_3D ( 'NONE', #32507, #55447, #8849 ) ;
#38573 = CARTESIAN_POINT ( 'NONE',  ( 10.00000000000000000, -75.11764819372145041, -2.946379043147127064 ) ) ;
#38574 = DIRECTION ( 'NONE',  ( 1.000000000000000000, 0.000000000000000000, 0.000000000000000000 ) ) ;
#38575 = DIRECTION ( 'NONE',  ( -1.000000000000000000, -0.000000000000000000, -0.000000000000000000 ) ) ;
#38576 = EDGE_LOOP ( 'NONE', ( #46324, #46928, #38462, #51857 ) ) ;
#38577 = CARTESIAN_POINT ( 'NONE',  ( -94.99999999999997158, -213.0599564267049857, 85.15812500173430521 ) ) ;
#38578 = ORIENTED_EDGE ( 'NONE', *, *, #19614, .T. ) ;
#38579 = CARTESIAN_POINT ( 'NONE',  ( 0.000000000000000000, -33.17418723428319538, 17.67226234102814431 ) ) ;
#38580 = ORIENTED_EDGE ( 'NONE', *, *, #29537, .T. ) ;
#38581 = CARTESIAN_POINT ( 'NONE',  ( -93.67500000000003979, 92.29496732002878900, 84.15270833506762926 ) ) ;
#38582 = AXIS2_PLACEMENT_3D ( 'NONE', #65808, #30099, #35386 ) ;
#38583 = ORIENTED_EDGE ( 'NONE', *, *, #13005, .F. ) ;
#38584 = CARTESIAN_POINT ( 'NONE',  ( 94.99999999999998579, 87.33691857156068750, 83.61031250086716682 ) ) ;
#38585 = CARTESIAN_POINT ( 'NONE',  ( 96.32499999999997442, 92.29496732002878900, 83.43833333333333258 ) ) ;
#38586 = DIRECTION ( 'NONE',  ( 0.000000000000000000, 0.2334453638559058908, -0.9723699203976764460 ) ) ;
#38587 = PLANE ( 'NONE',  #8611 ) ;
#38588 = LINE ( 'NONE', #61520, #13814 ) ;
#38589 = FACE_OUTER_BOUND ( 'NONE', #63715, .T. ) ;
#38590 = ORIENTED_EDGE ( 'NONE', *, *, #43989, .T. ) ;
#38591 = CARTESIAN_POINT ( 'NONE',  ( 0.000000000000000000, 0.000000000000000000, 0.000000000000000000 ) ) ;
#38592 = CARTESIAN_POINT ( 'NONE',  ( 8.700667342345820288, -98.11853780484867116, -5.500000000000000000 ) ) ;
#38593 = DIRECTION ( 'NONE',  ( -0.000000000000000000, -0.000000000000000000, 1.000000000000000000 ) ) ;
#38594 = ORIENTED_EDGE ( 'NONE', *, *, #23544, .F. ) ;
#38595 = ORIENTED_EDGE ( 'NONE', *, *, #71858, .T. ) ;
#38596 = EDGE_CURVE ( 'NONE', #44409, #74237, #17821, .T. ) ;
#38597 = PRODUCT_DEFINITION_SHAPE ( 'NONE', 'NONE',  #8124 ) ;
#38598 = DIRECTION ( 'NONE',  ( 0.000000000000000000, 0.000000000000000000, 1.000000000000000000 ) ) ;
#38599 = LINE ( 'NONE', #58111, #53473 ) ;
#38600 = CARTESIAN_POINT ( 'NONE',  ( 1.233757462863572574, -119.1468631277289347, 2.500000000000000000 ) ) ;
#38601 = CARTESIAN_POINT ( 'NONE',  ( -97.30629616937497417, -208.6684592857803011, 81.49364583420047836 ) ) ;
#38602 = EDGE_LOOP ( 'NONE', ( #8876, #45930, #59171, #13577 ) ) ;
#38603 = DIRECTION ( 'NONE',  ( -1.000000000000000000, 0.000000000000000000, 0.000000000000000000 ) ) ;
#38604 = VERTEX_POINT ( 'NONE', #18655 ) ;
#38605 = AXIS2_PLACEMENT_3D ( 'NONE', #21460, #72227, #39145 ) ;
#38606 = DIRECTION ( 'NONE',  ( -1.000000000000000000, 0.000000000000000000, 0.000000000000000000 ) ) ;
#38607 = VECTOR ( 'NONE', #28516, 1000.000000000000000 ) ;
#38608 = CARTESIAN_POINT ( 'NONE',  ( 93.67499999999999716, 87.70503267997126784, 81.93020833506763267 ) ) ;
#38609 = AXIS2_PLACEMENT_3D ( 'NONE', #2769, #42959, #60259 ) ;
#38610 = CARTESIAN_POINT ( 'NONE',  ( 10.00000000000000000, 35.53030884539102630, -12.26510123303222599 ) ) ;
#38611 = CARTESIAN_POINT ( 'NONE',  ( 97.30629616937498838, 88.66845928578035796, 79.11239583420046984 ) ) ;
#38612 = DIRECTION ( 'NONE',  ( 0.000000000000000000, 0.000000000000000000, 1.000000000000000000 ) ) ;
#38613 = CARTESIAN_POINT ( 'NONE',  ( 32.50000000000000000, -120.0000000000000000, 2.500000000000000000 ) ) ;
#38614 = EDGE_CURVE ( 'NONE', #59685, #57988, #51289, .T. ) ;
#38615 = DIRECTION ( 'NONE',  ( -1.000000000000000000, 0.000000000000000000, 0.000000000000000000 ) ) ;
#38616 = CARTESIAN_POINT ( 'NONE',  ( 92.49008991410269687, 90.12150787501455795, 74.91582548749272519 ) ) ;
#38617 = LINE ( 'NONE', #56281, #17237 ) ;
#38618 = EDGE_CURVE ( 'NONE', #3181, #40171, #60901, .T. ) ;
#38619 = CARTESIAN_POINT ( 'NONE',  ( 96.32499999999998863, -212.2949673200287179, 84.49666666666666970 ) ) ;
#38620 = VECTOR ( 'NONE', #24263, 1000.000000000000000 ) ;
#38621 = FACE_OUTER_BOUND ( 'NONE', #58429, .T. ) ;
#38622 = EDGE_CURVE ( 'NONE', #34951, #38411, #64173, .T. ) ;
#38623 = FACE_OUTER_BOUND ( 'NONE', #52894, .T. ) ;
#38624 = CARTESIAN_POINT ( 'NONE',  ( 10.00000000000000000, 76.69515212746016175, 29.01471420065591289 ) ) ;
#38625 = VERTEX_POINT ( 'NONE', #64535 ) ;
#38626 = ADVANCED_FACE ( 'NONE', ( #53252 ), #680, .F. ) ;
#38627 = CARTESIAN_POINT ( 'NONE',  ( -97.30629616937501680, 91.33154071421968467, 84.50989583420049200 ) ) ;
#38628 = AXIS2_PLACEMENT_3D ( 'NONE', #20739, #73715, #66610 ) ;
#38629 = CARTESIAN_POINT ( 'NONE',  ( 10.00000000000000000, 65.58780272294076497, 36.73666225445916211 ) ) ;
#38630 = CIRCLE ( 'NONE', #18221, 77.49899999999999523 ) ;
#38631 = CIRCLE ( 'NONE', #62632, 31.99999999999998579 ) ;
#38632 = CARTESIAN_POINT ( 'NONE',  ( 3.035766082959412415E-15, 5.773502691896260863, -2.080000000000000071 ) ) ;
#38633 = VERTEX_POINT ( 'NONE', #19027 ) ;
#38634 = CYLINDRICAL_SURFACE ( 'NONE', #19815, 2.649999999999999467 ) ;
#38635 = CARTESIAN_POINT ( 'NONE',  ( 10.00000000000000000, -33.17418723428294669, -17.67226234102862747 ) ) ;
#38636 = EDGE_CURVE ( 'NONE', #8415, #58803, #71674, .T. ) ;
#38637 = DIRECTION ( 'NONE',  ( -0.8090169943749426773, -0.5877852522924797984, 0.000000000000000000 ) ) ;
#38638 = LINE ( 'NONE', #33733, #68212 ) ;
#38639 = CARTESIAN_POINT ( 'NONE',  ( 93.84685191531251292, -211.9973110713294489, 79.74739583420048916 ) ) ;
#38640 = ORIENTED_EDGE ( 'NONE', *, *, #22132, .F. ) ;
#38641 = VERTEX_POINT ( 'NONE', #12647 ) ;
#38642 = EDGE_CURVE ( 'NONE', #70171, #5010, #23652, .T. ) ;
#38643 = EDGE_CURVE ( 'NONE', #67018, #23136, #52495, .T. ) ;
#38644 = LINE ( 'NONE', #17192, #62091 ) ;
#38645 = CARTESIAN_POINT ( 'NONE',  ( 0.000000000000000000, 23.59884966291538078, -12.14883922797231541 ) ) ;
#38646 = CARTESIAN_POINT ( 'NONE',  ( -92.34999999999999432, -208.4700217866474645, 85.36979166840096411 ) ) ;
#38647 = DIRECTION ( 'NONE',  ( 0.000000000000000000, 0.000000000000000000, 1.000000000000000000 ) ) ;
#38648 = EDGE_CURVE ( 'NONE', #3546, #52788, #29641, .T. ) ;
#38649 = CARTESIAN_POINT ( 'NONE',  ( 22.94323693612312454, -114.6983135802921083, -2.500000000000000000 ) ) ;
#38650 = CARTESIAN_POINT ( 'NONE',  ( 95.00000000000000000, -207.3369185715606307, 75.67281250086716682 ) ) ;
#38651 = CIRCLE ( 'NONE', #11075, 31.99999999999999645 ) ;
#38652 = VERTEX_POINT ( 'NONE', #23566 ) ;
#38653 = DIRECTION ( 'NONE',  ( -1.000000000000000000, 0.000000000000000000, 0.000000000000000000 ) ) ;
#38654 = EDGE_LOOP ( 'NONE', ( #44235, #31597, #7313, #20182 ) ) ;
#38655 = VERTEX_POINT ( 'NONE', #1052 ) ;
#38656 = LINE ( 'NONE', #68346, #40583 ) ;
#38657 = VECTOR ( 'NONE', #14280, 1000.000000000000000 ) ;
#38658 = ORIENTED_EDGE ( 'NONE', *, *, #11353, .T. ) ;
#38659 = DIRECTION ( 'NONE',  ( -0.000000000000000000, 0.8660254037844389297, 0.4999999999999995559 ) ) ;
#38660 = CARTESIAN_POINT ( 'NONE',  ( 97.64999999999999147, -209.9999999999999716, 81.50687500173430067 ) ) ;
#38661 = CARTESIAN_POINT ( 'NONE',  ( 97.64999999999997726, 91.52997821335252127, 80.21041666666666003 ) ) ;
#38662 = ORIENTED_EDGE ( 'NONE', *, *, #45201, .T. ) ;
#38663 = CARTESIAN_POINT ( 'NONE',  ( -3.000000000000000000, 8.688484142254221609, -21.88630264137359660 ) ) ;
#38664 = VECTOR ( 'NONE', #27949, 1000.000000000000000 ) ;
#38665 = VERTEX_POINT ( 'NONE', #7395 ) ;
#38666 = CARTESIAN_POINT ( 'NONE',  ( 0.000000000000000000, -36.88895765772628010, -6.736453364083947015 ) ) ;
#38667 = ORIENTED_EDGE ( 'NONE', *, *, #15215, .F. ) ;
#38668 = CYLINDRICAL_SURFACE ( 'NONE', #29609, 31.99999999999999289 ) ;
#38669 = CIRCLE ( 'NONE', #39857, 3.299999999999983391 ) ;
#38670 = CARTESIAN_POINT ( 'NONE',  ( -96.15314808468752972, 91.99731107132950569, 83.34572916753383254 ) ) ;
#38671 = CARTESIAN_POINT ( 'NONE',  ( 96.15314808468748708, 88.00268892867053694, 79.69447916753379957 ) ) ;
#38672 = ORIENTED_EDGE ( 'NONE', *, *, #72245, .T. ) ;
#38673 = FACE_OUTER_BOUND ( 'NONE', #41873, .T. ) ;
#38674 = CARTESIAN_POINT ( 'NONE',  ( 15.00000000000000000, 20.85821328998756385, 10.92862929874494249 ) ) ;
#38675 = EDGE_LOOP ( 'NONE', ( #4912, #41053, #60066, #72139 ) ) ;
#38676 = DIRECTION ( 'NONE',  ( 0.000000000000000000, 0.000000000000000000, -1.000000000000000000 ) ) ;
#38677 = CIRCLE ( 'NONE', #67438, 42.00000000000000000 ) ;
#38678 = AXIS2_PLACEMENT_3D ( 'NONE', #34787, #29133, #52070 ) ;
#38679 = CARTESIAN_POINT ( 'NONE',  ( -94.99999999999997158, -207.3369185715606307, 81.22906250086715829 ) ) ;
#38680 = ORIENTED_EDGE ( 'NONE', *, *, #61188, .F. ) ;
#38681 = ORIENTED_EDGE ( 'NONE', *, *, #38369, .T. ) ;
#38682 = LINE ( 'NONE', #15746, #28910 ) ;
#38683 = ORIENTED_EDGE ( 'NONE', *, *, #7456, .F. ) ;
#38684 = DIRECTION ( 'NONE',  ( -0.02332147558787823344, -0.9997280174009349762, 0.000000000000000000 ) ) ;
#38685 = EDGE_CURVE ( 'NONE', #56878, #3617, #3364, .T. ) ;
#38686 =( BOUNDED_CURVE ( )  B_SPLINE_CURVE ( 2, ( #16115, #28131, #72500, #43953, #66870, #4866, #72858 ),
 .UNSPECIFIED., .F., .F. ) 
 B_SPLINE_CURVE_WITH_KNOTS ( ( 3, 2, 2, 3 ),
 ( 0.6458333333333334814, 0.6527777777777779011, 0.6597222222222223209, 0.6666666666666667407 ),
 .UNSPECIFIED. ) 
 CURVE ( )  GEOMETRIC_REPRESENTATION_ITEM ( )  RATIONAL_B_SPLINE_CURVE ( ( 0.9999999999999978906, 0.8660254037844408170, 1.000000000000000000, 0.8660254037844387076, 1.000000000000000000, 0.8660254037844365982, 1.000000000000002220 ) ) 
 REPRESENTATION_ITEM ( '' )  );
#38687 = LINE ( 'NONE', #3377, #64707 ) ;
#38688 = ORIENTED_EDGE ( 'NONE', *, *, #49505, .F. ) ;
#38689 = CARTESIAN_POINT ( 'NONE',  ( -96.15314808468745866, -211.9973110713294489, 80.85864583420047325 ) ) ;
#38690 = EDGE_LOOP ( 'NONE', ( #9238, #8635, #53657, #12915 ) ) ;
#38691 = DIRECTION ( 'NONE',  ( -1.000000000000000000, 0.000000000000000000, -0.000000000000000000 ) ) ;
#38692 = CARTESIAN_POINT ( 'NONE',  ( 15.00000000000000000, 16.83928648764945635, 16.46020748918027010 ) ) ;
#38693 = DIRECTION ( 'NONE',  ( 0.000000000000000000, 0.000000000000000000, 1.000000000000000000 ) ) ;
#38694 = DIRECTION ( 'NONE',  ( 0.000000000000000000, 0.000000000000000000, 1.000000000000000000 ) ) ;
#38695 = LINE ( 'NONE', #27022, #45071 ) ;
#38696 = EDGE_CURVE ( 'NONE', #3338, #45145, #74095, .T. ) ;
#38697 = CARTESIAN_POINT ( 'NONE',  ( 0.000000000000000000, -0.9646360437372163421, -23.52805723605591126 ) ) ;
#38698 = CARTESIAN_POINT ( 'NONE',  ( 97.30629616937498838, 91.33154071421968467, 87.47322916753380184 ) ) ;
#38699 = CARTESIAN_POINT ( 'NONE',  ( -92.34999999999999432, -209.9999999999999716, 83.96750000000000114 ) ) ;
#38700 = DIRECTION ( 'NONE',  ( 0.000000000000000000, 0.000000000000000000, 1.000000000000000000 ) ) ;
#38701 = ADVANCED_FACE ( 'NONE', ( #20518 ), #60384, .T. ) ;
#38702 = DIRECTION ( 'NONE',  ( 0.000000000000000000, 0.000000000000000000, 1.000000000000000000 ) ) ;
#38703 = CARTESIAN_POINT ( 'NONE',  ( -25.50183398199384754, -112.6408924756582053, 5.500000000000000000 ) ) ;
#38704 = CARTESIAN_POINT ( 'NONE',  ( 11.99999999999999822, 46.11716303203283474, -67.80270845531838120 ) ) ;
#38705 = DIRECTION ( 'NONE',  ( 1.000000000000000000, 0.000000000000000000, 0.000000000000000000 ) ) ;
#38706 = CARTESIAN_POINT ( 'NONE',  ( 10.00000000000000000, 12.93880638057426502, -76.41127070299258150 ) ) ;
#38707 = CARTESIAN_POINT ( 'NONE',  ( -18.12185313557660038, -104.9634299478706794, -5.500000000000000000 ) ) ;
#38708 = CARTESIAN_POINT ( 'NONE',  ( -97.64999999999996305, -209.9999999999999716, 90.00000000000000000 ) ) ;
#38709 = EDGE_CURVE ( 'NONE', #961, #5747, #11615, .T. ) ;
#38710 = COLOUR_RGB ( '', 0.66274510, 0.83137255, 0.94901961) ;
#38711 = DIRECTION ( 'NONE',  ( 0.000000000000000000, -0.5877852522924625900, -0.8090169943749551118 ) ) ;
#38712 = DIRECTION ( 'NONE',  ( -0.7585478161175716050, -0.6516173805718067369, 0.000000000000000000 ) ) ;
#38713 = CARTESIAN_POINT ( 'NONE',  ( 10.00000000000000000, -8.840884882375609877, 74.65374052328647281 ) ) ;
#38714 = VECTOR ( 'NONE', #45475, 1000.000000000000000 ) ;
#38715 = CARTESIAN_POINT ( 'NONE',  ( -92.34999999999999432, -211.5299782133524502, 85.18458333333332178 ) ) ;
#38716 = AXIS2_PLACEMENT_3D ( 'NONE', #60341, #61070, #71590 ) ;
#38717 = CARTESIAN_POINT ( 'NONE',  ( -94.60587738269765623, 87.35656277621949073, 75.00000000000001421 ) ) ;
#38718 = EDGE_CURVE ( 'NONE', #38841, #64894, #3622, .T. ) ;
#38719 = CARTESIAN_POINT ( 'NONE',  ( 15.00000000000000000, 0.000000000000000000, 0.000000000000000000 ) ) ;
#38720 = EDGE_CURVE ( 'NONE', #17753, #70426, #70479, .T. ) ;
#38721 = FACE_OUTER_BOUND ( 'NONE', #48464, .T. ) ;
#38722 = PRESENTATION_STYLE_ASSIGNMENT (( #4525 ) ) ;
#38723 = CARTESIAN_POINT ( 'NONE',  ( -3.000000000000000000, -0.9646360437375307573, 23.52805723605590060 ) ) ;
#38724 = AXIS2_PLACEMENT_3D ( 'NONE', #71262, #13396, #54366 ) ;
#38725 = ADVANCED_FACE ( 'NONE', ( #14497 ), #60019, .T. ) ;
#38726 = AXIS2_PLACEMENT_3D ( 'NONE', #1205, #7170, #35718 ) ;
#38727 = CARTESIAN_POINT ( 'NONE',  ( 96.15314808468748708, -208.0026889286704943, 87.68489583420048916 ) ) ;
#38728 = VERTEX_POINT ( 'NONE', #20133 ) ;
#38729 = ORIENTED_EDGE ( 'NONE', *, *, #52128, .T. ) ;
#38730 = LINE ( 'NONE', #9403, #32271 ) ;
#38731 = ADVANCED_FACE ( 'NONE', ( #54000 ), #2158, .T. ) ;
#38732 = FACE_OUTER_BOUND ( 'NONE', #59095, .T. ) ;
#38733 = EDGE_LOOP ( 'NONE', ( #22637, #72630, #67528, #48623 ) ) ;
#38734 = CARTESIAN_POINT ( 'NONE',  ( 97.30629616937498838, -211.3315407142195852, 79.74739583420047495 ) ) ;
#38735 = CARTESIAN_POINT ( 'NONE',  ( 93.84685191531249870, -208.0026889286704943, 85.25072916753381946 ) ) ;
#38736 = ADVANCED_FACE ( 'NONE', ( #66394 ), #14873, .T. ) ;
#38737 = ORIENTED_EDGE ( 'NONE', *, *, #69944, .T. ) ;
#38738 = CARTESIAN_POINT ( 'NONE',  ( 92.69370383062501162, -211.3315407142195852, 84.77447916753381207 ) ) ;
#38739 = ORIENTED_EDGE ( 'NONE', *, *, #59773, .T. ) ;
#38740 = LINE ( 'NONE', #49266, #2283 ) ;
#38741 = VERTEX_POINT ( 'NONE', #65283 ) ;
#38742 = CARTESIAN_POINT ( 'NONE',  ( -92.69370383062504004, 90.00000000000004263, 75.51406250086715488 ) ) ;
#38743 = ORIENTED_EDGE ( 'NONE', *, *, #18607, .T. ) ;
#38744 = FACE_OUTER_BOUND ( 'NONE', #32844, .T. ) ;
#38745 = ORIENTED_EDGE ( 'NONE', *, *, #42681, .F. ) ;
#38746 = FACE_OUTER_BOUND ( 'NONE', #62055, .T. ) ;
#38747 = CARTESIAN_POINT ( 'NONE',  ( 92.35000000000002274, -211.5299782133524502, 88.86229166840097093 ) ) ;
#38748 = ORIENTED_EDGE ( 'NONE', *, *, #49895, .T. ) ;
#38749 = DIRECTION ( 'NONE',  ( 0.000000000000000000, 0.000000000000000000, 1.000000000000000000 ) ) ;
#38750 = VERTEX_POINT ( 'NONE', #72008 ) ;
#38751 = CARTESIAN_POINT ( 'NONE',  ( 10.00000000000000000, 5.256550761632864166, 77.32052557432842832 ) ) ;
#38752 = ORIENTED_EDGE ( 'NONE', *, *, #11231, .F. ) ;
#38753 = MECHANICAL_DESIGN_GEOMETRIC_PRESENTATION_REPRESENTATION (  '', ( #23159 ), #35165 ) ;
#38754 = ORIENTED_EDGE ( 'NONE', *, *, #6887, .F. ) ;
#38755 = ORIENTED_EDGE ( 'NONE', *, *, #70585, .F. ) ;
#38756 = CARTESIAN_POINT ( 'NONE',  ( -12.49999999999999645, 0.000000000000000000, -56.19999999999998863 ) ) ;
#38757 = LINE ( 'NONE', #73698, #67858 ) ;
#38758 = EDGE_LOOP ( 'NONE', ( #6602, #28551, #6517, #67252 ) ) ;
#38759 = CIRCLE ( 'NONE', #30375, 82.00000000000000000 ) ;
#38760 = ORIENTED_EDGE ( 'NONE', *, *, #60793, .F. ) ;
#38761 = ORIENTED_EDGE ( 'NONE', *, *, #17060, .T. ) ;
#38762 = DIRECTION ( 'NONE',  ( 0.000000000000000000, 0.000000000000000000, 1.000000000000000000 ) ) ;
#38763 = DIRECTION ( 'NONE',  ( -1.000000000000000000, 0.000000000000000000, 0.000000000000000000 ) ) ;
#38764 = CARTESIAN_POINT ( 'NONE',  ( -95.00000000000002842, 87.33691857156074434, 77.26031250086714408 ) ) ;
#38765 = EDGE_LOOP ( 'NONE', ( #68426, #53750, #5306, #71913 ) ) ;
#38766 = CARTESIAN_POINT ( 'NONE',  ( 92.69370383062498320, 91.33154071421968467, 77.52489583420046415 ) ) ;
#38767 = AXIS2_PLACEMENT_3D ( 'NONE', #68655, #39712, #52084 ) ;
#38768 = ORIENTED_EDGE ( 'NONE', *, *, #50053, .T. ) ;
#38769 = CARTESIAN_POINT ( 'NONE',  ( 10.00000000000000000, 33.17418723428333749, -17.67226234102790272 ) ) ;
#38770 = CARTESIAN_POINT ( 'NONE',  ( 10.00000000000000000, 0.000000000000000000, 0.000000000000000000 ) ) ;
#38771 = EDGE_LOOP ( 'NONE', ( #14414, #32930, #71803, #72298, #13872, #61340, #36226, #68229 ) ) ;
#38772 = DIRECTION ( 'NONE',  ( -1.000000000000000000, 0.000000000000000000, 0.000000000000000000 ) ) ;
#38773 = CARTESIAN_POINT ( 'NONE',  ( -3.000000000000002665, 0.000000000000000000, 0.000000000000000000 ) ) ;
#38774 = CARTESIAN_POINT ( 'NONE',  ( 0.000000000000000000, 0.000000000000000000, 0.000000000000000000 ) ) ;
#38775 = CARTESIAN_POINT ( 'NONE',  ( -97.30629616937497417, -211.3315407142195852, 80.80572916753379786 ) ) ;
#38776 = EDGE_CURVE ( 'NONE', #71846, #43844, #21223, .T. ) ;
#38777 = FACE_OUTER_BOUND ( 'NONE', #23661, .T. ) ;
#38778 = FACE_OUTER_BOUND ( 'NONE', #33356, .T. ) ;
#38779 = AXIS2_PLACEMENT_3D ( 'NONE', #14080, #30629, #65986 ) ;
#38780 = CARTESIAN_POINT ( 'NONE',  ( -92.34999999999999432, -209.9999999999999716, 79.52249999999999375 ) ) ;
#38781 = ORIENTED_EDGE ( 'NONE', *, *, #61604, .F. ) ;
#38782 = CIRCLE ( 'NONE', #25571, 31.99999999999998579 ) ;
#38783 = EDGE_CURVE ( 'NONE', #28467, #26369, #17645, .T. ) ;
#38784 = ORIENTED_EDGE ( 'NONE', *, *, #47679, .F. ) ;
#38785 = DIRECTION ( 'NONE',  ( 0.000000000000000000, 0.000000000000000000, 1.000000000000000000 ) ) ;
#38786 = EDGE_CURVE ( 'NONE', #14607, #26543, #66024, .T. ) ;
#38787 = CARTESIAN_POINT ( 'NONE',  ( -97.64999999999996305, -209.9999999999999716, 88.73000000000000398 ) ) ;
#38788 = CARTESIAN_POINT ( 'NONE',  ( 95.77009744696167104, -207.7668333712726962, 74.81945665767624121 ) ) ;
#38789 = CARTESIAN_POINT ( 'NONE',  ( -97.30629616937501680, 88.66845928578038638, 82.07572916753380809 ) ) ;
#38790 = DIRECTION ( 'NONE',  ( 0.000000000000000000, 0.9723699203976756689, 0.2334453638559094157 ) ) ;
#38791 = DIRECTION ( 'NONE',  ( 0.000000000000000000, 0.000000000000000000, 1.000000000000000000 ) ) ;
#38792 = EDGE_CURVE ( 'NONE', #54369, #17536, #8867, .T. ) ;
#38793 = ORIENTED_EDGE ( 'NONE', *, *, #32143, .F. ) ;
#38794 = DIRECTION ( 'NONE',  ( 0.000000000000000000, -0.7431448254773856954, -0.6691306063588676745 ) ) ;
#38795 = CARTESIAN_POINT ( 'NONE',  ( 10.00000000000000000, -68.67312586194971402, -35.91791733033549860 ) ) ;
#38796 = DIRECTION ( 'NONE',  ( -1.000000000000000000, 0.000000000000000000, -0.000000000000000000 ) ) ;
#38797 = DIRECTION ( 'NONE',  ( -1.000000000000000000, -0.000000000000000000, 0.000000000000000000 ) ) ;
#38798 = FACE_OUTER_BOUND ( 'NONE', #35033, .T. ) ;
#38799 = CARTESIAN_POINT ( 'NONE',  ( -97.30629616937495996, -209.9999999999999716, 79.00656250086716170 ) ) ;
#38800 = CARTESIAN_POINT ( 'NONE',  ( 10.00000000000000000, 21.40280677340421533, -36.13751322684397138 ) ) ;
#38801 = VECTOR ( 'NONE', #16423, 1000.000000000000227 ) ;
#38802 = VERTEX_POINT ( 'NONE', #8118 ) ;
#38803 = DIRECTION ( 'NONE',  ( 1.000000000000000000, 0.000000000000000000, 0.000000000000000000 ) ) ;
#38804 = DIRECTION ( 'NONE',  ( -0.9997280174009349762, 0.02332147558787671729, 0.000000000000000000 ) ) ;
#38805 = DIRECTION ( 'NONE',  ( -1.000000000000000000, -0.000000000000000000, 0.000000000000000000 ) ) ;
#38806 = ORIENTED_EDGE ( 'NONE', *, *, #34990, .T. ) ;
#38807 = PRODUCT_DEFINITION_FORMATION_WITH_SPECIFIED_SOURCE ( 'ANY', '', #66185, .NOT_KNOWN. ) ;
#38808 = DIRECTION ( 'NONE',  ( 0.000000000000000000, 0.000000000000000000, -1.000000000000000000 ) ) ;
#38809 = CARTESIAN_POINT ( 'NONE',  ( 10.00000000000000000, 0.000000000000000000, 0.000000000000000000 ) ) ;
#38810 = EDGE_CURVE ( 'NONE', #52162, #44097, #3254, .T. ) ;
#38811 = ADVANCED_FACE ( 'NONE', ( #9227 ), #32149, .F. ) ;
#38812 = AXIS2_PLACEMENT_3D ( 'NONE', #1334, #70059, #47152 ) ;
#38813 = LINE ( 'NONE', #39186, #25191 ) ;
#38814 = ORIENTED_EDGE ( 'NONE', *, *, #6612, .F. ) ;
#38815 = CARTESIAN_POINT ( 'NONE',  ( 12.50000000000000000, -132.5000000000000000, -40.00000000000000000 ) ) ;
#38816 = EDGE_CURVE ( 'NONE', #24049, #27539, #17699, .T. ) ;
#38817 = CARTESIAN_POINT ( 'NONE',  ( 0.000000000000000000, 0.000000000000000000, 0.000000000000000000 ) ) ;
#38818 = ORIENTED_EDGE ( 'NONE', *, *, #54865, .F. ) ;
#38819 = VECTOR ( 'NONE', #47073, 1000.000000000000000 ) ;
#38820 = CARTESIAN_POINT ( 'NONE',  ( 96.15314808468748708, -208.0026889286704943, 87.52614583420047722 ) ) ;
#38821 = CARTESIAN_POINT ( 'NONE',  ( -92.35000000000003695, 90.00000000000004263, 77.61749999999999261 ) ) ;
#38822 = AXIS2_PLACEMENT_3D ( 'NONE', #58682, #42143, #53411 ) ;
#38823 = VERTEX_POINT ( 'NONE', #19399 ) ;
#38824 = DIRECTION ( 'NONE',  ( -1.000000000000000000, -0.000000000000000000, -0.000000000000000000 ) ) ;
#38825 = ORIENTED_EDGE ( 'NONE', *, *, #52822, .T. ) ;
#38826 = VECTOR ( 'NONE', #23629, 1000.000000000000114 ) ;
#38827 = CARTESIAN_POINT ( 'NONE',  ( -97.65000000000001990, 90.00000000000004263, 83.01499999999998636 ) ) ;
#38828 = CIRCLE ( 'NONE', #6434, 31.99999999999998224 ) ;
#38829 = CIRCLE ( 'NONE', #20848, 37.49900000000000233 ) ;
#38830 = DIRECTION ( 'NONE',  ( 0.000000000000000000, -0.1564344650402170744, -0.9876883405951399908 ) ) ;
#38831 = ORIENTED_EDGE ( 'NONE', *, *, #57917, .T. ) ;
#38832 = ORIENTED_EDGE ( 'NONE', *, *, #6858, .T. ) ;
#38833 = ORIENTED_EDGE ( 'NONE', *, *, #153, .T. ) ;
#38834 = DIRECTION ( 'NONE',  ( 0.000000000000000000, 0.5877852522924684742, 0.8090169943749507819 ) ) ;
#38835 = ORIENTED_EDGE ( 'NONE', *, *, #29359, .T. ) ;
#38836 = ORIENTED_EDGE ( 'NONE', *, *, #1597, .F. ) ;
#38837 = CARTESIAN_POINT ( 'NONE',  ( 92.69370383062498320, 90.00000000000002842, 77.73656250086715147 ) ) ;
#38838 = DIRECTION ( 'NONE',  ( -1.000000000000000000, 0.000000000000000000, -0.000000000000000000 ) ) ;
#38839 = FACE_OUTER_BOUND ( 'NONE', #11711, .T. ) ;
#38840 = ORIENTED_EDGE ( 'NONE', *, *, #27702, .T. ) ;
#38841 = VERTEX_POINT ( 'NONE', #51213 ) ;
#38842 = ORIENTED_EDGE ( 'NONE', *, *, #23929, .T. ) ;
#38843 = CARTESIAN_POINT ( 'NONE',  ( 93.84685191531248449, 88.00268892867053694, 89.11364583420048291 ) ) ;
#38844 = ORIENTED_EDGE ( 'NONE', *, *, #41493, .F. ) ;
#38845 = CARTESIAN_POINT ( 'NONE',  ( 97.30629616937498838, -209.9999999999999716, 83.61031250086713840 ) ) ;
#38846 = CARTESIAN_POINT ( 'NONE',  ( 95.00000000002722800, -210.0000000000009379, 102.7500000000000142 ) ) ;
#38847 = DIRECTION ( 'NONE',  ( 1.000000000000000000, 0.000000000000000000, 0.000000000000000000 ) ) ;
#38848 = DIRECTION ( 'NONE',  ( -1.000000000000000000, 0.000000000000000000, -0.000000000000000000 ) ) ;
#38849 = CARTESIAN_POINT ( 'NONE',  ( 15.00000000000000000, -22.67460108101782978, -6.353146135317906840 ) ) ;
#38850 = FACE_OUTER_BOUND ( 'NONE', #3248, .T. ) ;
#38851 = DIRECTION ( 'NONE',  ( -1.000000000000000000, 0.000000000000000000, 0.000000000000000000 ) ) ;
#38852 = CARTESIAN_POINT ( 'NONE',  ( 10.00000000000000000, 41.19522573413826194, -65.64334221924865176 ) ) ;
#38853 = CARTESIAN_POINT ( 'NONE',  ( -92.69370383062498320, -208.6684592857803011, 88.10822916753380696 ) ) ;
#38854 = CARTESIAN_POINT ( 'NONE',  ( -93.84685191531252713, 88.00268892867056536, 86.83822916753382515 ) ) ;
#38855 = ORIENTED_EDGE ( 'NONE', *, *, #29175, .F. ) ;
#38856 = AXIS2_PLACEMENT_3D ( 'NONE', #48687, #47581, #48321 ) ;
#38858 = CARTESIAN_POINT ( 'NONE',  ( -97.30629616937501680, 91.33154071421968467, 88.95489583420048518 ) ) ;
#38857 = CARTESIAN_POINT ( 'NONE',  ( 97.30629616937498838, 91.33154071421968467, 88.74322916753379786 ) ) ;
#38859 = EDGE_LOOP ( 'NONE', ( #37101, #26221, #17820, #35756 ) ) ;
#38860 = CARTESIAN_POINT ( 'NONE',  ( 12.02279259712643622, 0.000000000000000000, 0.000000000000000000 ) ) ;
#38861 = CARTESIAN_POINT ( 'NONE',  ( 3.000000000000000000, 0.000000000000000000, 0.000000000000000000 ) ) ;
#38862 = CARTESIAN_POINT ( 'NONE',  ( -3.000000000000000000, -3.948201729842348850, 23.21447184625293048 ) ) ;
#38863 = DIRECTION ( 'NONE',  ( -0.000000000000000000, -0.000000000000000000, 1.000000000000000000 ) ) ;
#38864 = DIRECTION ( 'NONE',  ( 0.000000000000000000, 0.3826834323650842862, 0.9238795325112890700 ) ) ;
#38865 = AXIS2_PLACEMENT_3D ( 'NONE', #48958, #44821, #15873 ) ;
#38866 = CARTESIAN_POINT ( 'NONE',  ( 97.64999999999997726, -208.4700217866474929, 82.11541666666664696 ) ) ;
#38867 = ORIENTED_EDGE ( 'NONE', *, *, #21613, .F. ) ;
#38868 = EDGE_CURVE ( 'NONE', #44570, #62914, #9310, .T. ) ;
#38869 = CARTESIAN_POINT ( 'NONE',  ( 0.000000000000000000, 44.88180994100376608, 63.18004540533043922 ) ) ;
#38870 = DIRECTION ( 'NONE',  ( -1.000000000000000000, -0.000000000000000000, -0.000000000000000000 ) ) ;
#38871 = ORIENTED_EDGE ( 'NONE', *, *, #51013, .F. ) ;
#38872 = AXIS2_PLACEMENT_3D ( 'NONE', #39390, #28461, #74333 ) ;
#38873 = EDGE_CURVE ( 'NONE', #64448, #33698, #12907, .T. ) ;
#38874 = ORIENTED_EDGE ( 'NONE', *, *, #4790, .F. ) ;
#38875 = EDGE_CURVE ( 'NONE', #38492, #67492, #17015, .T. ) ;
#38876 = CARTESIAN_POINT ( 'NONE',  ( -97.65000000000001990, 90.00000000000004263, 81.74500000000000455 ) ) ;
#38877 = CARTESIAN_POINT ( 'NONE',  ( 10.00000000000000000, -21.53537804866103045, 30.80686688397002371 ) ) ;
#38878 = CARTESIAN_POINT ( 'NONE',  ( 11.99999999999999822, -24.73286445877757345, 73.44644590900053061 ) ) ;
#38879 = DIRECTION ( 'NONE',  ( 0.000000000000000000, -0.8090169943749403458, -0.5877852522924830181 ) ) ;
#38880 = FACE_BOUND ( 'NONE', #31261, .T. ) ;
#38881 = DIRECTION ( 'NONE',  ( -1.000000000000000000, -0.000000000000000000, -0.000000000000000000 ) ) ;
#38882 = CIRCLE ( 'NONE', #34043, 12.49999999999999822 ) ;
#38883 = CARTESIAN_POINT ( 'NONE',  ( 0.000000000000000000, 12.93880638057315302, 76.41127070299275204 ) ) ;
#38884 = ADVANCED_FACE ( 'NONE', ( #34665 ), #61119, .T. ) ;
#38885 = CIRCLE ( 'NONE', #56928, 82.00000000000000000 ) ;
#38886 = ORIENTED_EDGE ( 'NONE', *, *, #39737, .F. ) ;
#38887 = CARTESIAN_POINT ( 'NONE',  ( -93.84685191531252713, 88.00268892867056536, 82.23447916753380582 ) ) ;
#38888 = DIRECTION ( 'NONE',  ( 0.000000000000000000, 0.9723699203976773342, -0.2334453638559023381 ) ) ;
#38889 = VECTOR ( 'NONE', #48401, 1000.000000000000000 ) ;
#38890 = CIRCLE ( 'NONE', #4132, 82.00000000000000000 ) ;
#38891 = CARTESIAN_POINT ( 'NONE',  ( -97.65000000000001990, 90.00000000000004263, 85.55499999999999261 ) ) ;
#38892 = DIRECTION ( 'NONE',  ( 0.000000000000000000, 0.000000000000000000, 1.000000000000000000 ) ) ;
#38893 = LINE ( 'NONE', #67834, #9300 ) ;
#38894 = DIRECTION ( 'NONE',  ( -1.000000000000000000, 0.000000000000000000, 0.000000000000000000 ) ) ;
#38895 = CARTESIAN_POINT ( 'NONE',  ( -93.84685191531247028, -211.9973110713294489, 88.74322916753382628 ) ) ;
#38896 = EDGE_CURVE ( 'NONE', #57897, #63122, #40310, .T. ) ;
#38897 = EDGE_CURVE ( 'NONE', #16169, #25977, #29021, .T. ) ;
#38898 = CARTESIAN_POINT ( 'NONE',  ( 92.69370383062498320, 88.66845928578035796, 79.69447916753381378 ) ) ;
#38899 = AXIS2_PLACEMENT_3D ( 'NONE', #56722, #21741, #56339 ) ;
#38900 = CARTESIAN_POINT ( 'NONE',  ( -96.15314808468745866, -211.9973110713294489, 80.38239583420048007 ) ) ;
#38901 = CYLINDRICAL_SURFACE ( 'NONE', #12210, 31.99999999999999289 ) ;
#38902 = ORIENTED_EDGE ( 'NONE', *, *, #6160, .F. ) ;
#38903 = CARTESIAN_POINT ( 'NONE',  ( -93.67500000000003979, 87.70503267997129626, 87.11604166840096752 ) ) ;
#38904 = CARTESIAN_POINT ( 'NONE',  ( 0.000000000000000000, 0.000000000000000000, 0.000000000000000000 ) ) ;
#38905 = CARTESIAN_POINT ( 'NONE',  ( 92.35000000000000853, -209.9999999999999716, 78.64937500173429896 ) ) ;
#38906 = ADVANCED_FACE ( 'NONE', ( #17377 ), #44192, .F. ) ;
#38907 = EDGE_CURVE ( 'NONE', #8315, #69599, #52509, .T. ) ;
#38908 = CARTESIAN_POINT ( 'NONE',  ( -97.30629616937501680, 90.00000000000004263, 79.00656250086716170 ) ) ;
#38909 = CARTESIAN_POINT ( 'NONE',  ( 97.30629616937498838, -211.3315407142195852, 81.65239583420049030 ) ) ;
#38910 = ORIENTED_EDGE ( 'NONE', *, *, #40685, .T. ) ;
#38911 = AXIS2_PLACEMENT_3D ( 'NONE', #28796, #51733, #69029 ) ;
#38912 = CARTESIAN_POINT ( 'NONE',  ( 6.000000000000000000, 44.99326035066052043, 68.55367621811159040 ) ) ;
#38913 = VERTEX_POINT ( 'NONE', #15621 ) ;
#38914 =( BOUNDED_CURVE ( )  B_SPLINE_CURVE ( 2, ( #13280, #36212, #1680, #64803, #47863, #36579, #6905 ),
 .UNSPECIFIED., .F., .F. ) 
 B_SPLINE_CURVE_WITH_KNOTS ( ( 3, 2, 2, 3 ),
 ( 0.08333333333333288462, 0.09027777777777759582, 0.09722222222222230703, 0.1041666666666670182 ),
 .UNSPECIFIED. ) 
 CURVE ( )  GEOMETRIC_REPRESENTATION_ITEM ( )  RATIONAL_B_SPLINE_CURVE ( ( 1.000000000000008660, 0.8660254037844301589, 1.000000000000000000, 0.8660254037844387076, 1.000000000000000000, 0.8660254037844320463, 1.000000000000006661 ) ) 
 REPRESENTATION_ITEM ( '' )  );
#38915 = DIRECTION ( 'NONE',  ( 0.000000000000000000, 0.000000000000000000, 1.000000000000000000 ) ) ;
#38916 = ORIENTED_EDGE ( 'NONE', *, *, #36598, .F. ) ;
#38917 = VECTOR ( 'NONE', #19285, 1000.000000000000000 ) ;
#38918 = CARTESIAN_POINT ( 'NONE',  ( 11.99999999999999822, 41.19522573413733113, 65.64334221924924861 ) ) ;
#38919 = CIRCLE ( 'NONE', #70138, 35.50000000000000711 ) ;
#38920 = ORIENTED_EDGE ( 'NONE', *, *, #35572, .T. ) ;
#38921 = ORIENTED_EDGE ( 'NONE', *, *, #40951, .F. ) ;
#38922 = ORIENTED_EDGE ( 'NONE', *, *, #10687, .T. ) ;
#38923 = CARTESIAN_POINT ( 'NONE',  ( 96.15314808468748708, -208.0026889286704943, 76.25489583420049655 ) ) ;
#38924 = ORIENTED_EDGE ( 'NONE', *, *, #11893, .F. ) ;
#38925 = CARTESIAN_POINT ( 'NONE',  ( 10.00000000000000000, 39.47590169984845687, 71.87247863392427405 ) ) ;
#38926 = AXIS2_PLACEMENT_3D ( 'NONE', #5205, #40503, #35233 ) ;
#38927 = DIRECTION ( 'NONE',  ( -1.000000000000000000, -0.000000000000000000, -0.000000000000000000 ) ) ;
#38928 = CARTESIAN_POINT ( 'NONE',  ( 92.69370383062498320, 90.00000000000002842, 87.89656250086714806 ) ) ;
#38929 = AXIS2_PLACEMENT_3D ( 'NONE', #3877, #21130, #44082 ) ;
#38930 = CARTESIAN_POINT ( 'NONE',  ( 2.047646702416564768, -96.54137380445985173, 5.500000000000000000 ) ) ;
#38931 = CARTESIAN_POINT ( 'NONE',  ( 93.67500000000001137, -207.7050326799711968, 78.46416666666667084 ) ) ;
#38932 = VERTEX_POINT ( 'NONE', #38176 ) ;
#38933 = ORIENTED_EDGE ( 'NONE', *, *, #39338, .T. ) ;
#38934 = ORIENTED_EDGE ( 'NONE', *, *, #54341, .T. ) ;
#38935 = CIRCLE ( 'NONE', #12526, 5.315148208181397216 ) ;
#38936 = ORIENTED_EDGE ( 'NONE', *, *, #37684, .F. ) ;
#38937 = DIRECTION ( 'NONE',  ( 0.000000000000000000, 0.000000000000000000, 1.000000000000000000 ) ) ;
#38938 = CIRCLE ( 'NONE', #58144, 16.00000000000000000 ) ;
#38939 = CARTESIAN_POINT ( 'NONE',  ( 0.000000000000000000, 0.000000000000000000, 0.000000000000000000 ) ) ;
#38940 = DIRECTION ( 'NONE',  ( 1.000000000000000000, 0.000000000000000000, 0.000000000000000000 ) ) ;
#38941 = DIRECTION ( 'NONE',  ( 0.000000000000000000, -6.982962677686267499E-15, 1.000000000000000000 ) ) ;
#38942 = CARTESIAN_POINT ( 'NONE',  ( 1.560000000000000053, 0.000000000000000000, 0.000000000000000000 ) ) ;
#38943 = CARTESIAN_POINT ( 'NONE',  ( 97.65000000000000568, 88.47002178664752137, 83.99395833506763154 ) ) ;
#38944 = EDGE_CURVE ( 'NONE', #72748, #33646, #5746, .T. ) ;
#38945 = VERTEX_POINT ( 'NONE', #9968 ) ;
#38946 = CARTESIAN_POINT ( 'NONE',  ( -93.67499999999998295, -207.7050326799711968, 83.51770833506763836 ) ) ;
#38947 = ORIENTED_EDGE ( 'NONE', *, *, #50023, .T. ) ;
#38948 = CARTESIAN_POINT ( 'NONE',  ( 0.000000000000000000, -120.0000000000000000, -2.500000000000000000 ) ) ;
#38949 = AXIS2_PLACEMENT_3D ( 'NONE', #72464, #66840, #31503 ) ;
#38951 = EDGE_LOOP ( 'NONE', ( #7593, #71559, #20459, #15425 ) ) ;
#38950 = EDGE_CURVE ( 'NONE', #63017, #1988, #504, .T. ) ;
#38953 = CARTESIAN_POINT ( 'NONE',  ( -96.32500000000001705, 87.70503267997129626, 83.83520833506763381 ) ) ;
#38952 = CARTESIAN_POINT ( 'NONE',  ( 94.99999999999998579, 86.94004357329500010, 81.98312500173430806 ) ) ;
#38954 = ORIENTED_EDGE ( 'NONE', *, *, #17822, .F. ) ;
#38955 = CARTESIAN_POINT ( 'NONE',  ( 96.15314808468748708, 88.00268892867053694, 83.02822916753380866 ) ) ;
#38956 = CARTESIAN_POINT ( 'NONE',  ( -92.35000000000003695, 90.00000000000004263, 76.34749999999999659 ) ) ;
#38957 = CARTESIAN_POINT ( 'NONE',  ( 0.000000000000000000, 12.42422080174688404, -35.38097989696498047 ) ) ;
#38958 = AXIS2_PLACEMENT_3D ( 'NONE', #19694, #20063, #20451 ) ;
#38959 = EDGE_CURVE ( 'NONE', #54442, #9139, #56119, .T. ) ;
#38960 = DIRECTION ( 'NONE',  ( 0.000000000000000000, -0.000000000000000000, 1.000000000000000000 ) ) ;
#38961 = CARTESIAN_POINT ( 'NONE',  ( 93.67499999999998295, 92.29496732002878900, 81.71854166840095957 ) ) ;
#38962 = CARTESIAN_POINT ( 'NONE',  ( -97.64999999999996305, -209.9999999999999716, 80.47499999999999432 ) ) ;
#38963 = ORIENTED_EDGE ( 'NONE', *, *, #32932, .T. ) ;
#38964 = CARTESIAN_POINT ( 'NONE',  ( -97.64995694994087216, 91.53000306831579280, 81.13645661577284329 ) ) ;
#38965 = CARTESIAN_POINT ( 'NONE',  ( -97.65000000000001990, 90.00003216987890653, 82.45937388908920695 ) ) ;
#38966 = CARTESIAN_POINT ( 'NONE',  ( -10.90076147243505211, 1.679431090506078290E-15, -13.71319123027096865 ) ) ;
#38967 = VERTEX_POINT ( 'NONE', #142 ) ;
#38968 = EDGE_CURVE ( 'NONE', #6231, #27626, #32527, .T. ) ;
#38969 = VERTEX_POINT ( 'NONE', #28276 ) ;
#38970 = CARTESIAN_POINT ( 'NONE',  ( -3.000000000000000000, 8.688484142253939169, 21.88630264137371029 ) ) ;
#38971 = VECTOR ( 'NONE', #70474, 1000.000000000000000 ) ;
#38972 = DIRECTION ( 'NONE',  ( -1.000000000000000000, -0.000000000000000000, -0.000000000000000000 ) ) ;
#38973 = LINE ( 'NONE', #63040, #52111 ) ;
#38974 = CARTESIAN_POINT ( 'NONE',  ( -92.69370383062498320, -209.9999999999999716, 82.49906250086715431 ) ) ;
#38975 = VERTEX_POINT ( 'NONE', #51587 ) ;
#38976 = EDGE_CURVE ( 'NONE', #32694, #67486, #26886, .T. ) ;
#38977 = FACE_OUTER_BOUND ( 'NONE', #69606, .T. ) ;
#38978 = ORIENTED_EDGE ( 'NONE', *, *, #12730, .T. ) ;
#38979 = DIRECTION ( 'NONE',  ( 0.000000000000000000, 0.000000000000000000, 1.000000000000000000 ) ) ;
#38980 = VECTOR ( 'NONE', #9710, 1000.000000000000000 ) ;
#38981 = DIRECTION ( 'NONE',  ( 1.000000000000000000, 0.000000000000000000, 0.000000000000000000 ) ) ;
#38982 = DIRECTION ( 'NONE',  ( -1.000000000000000000, 0.000000000000000000, 0.000000000000000000 ) ) ;
#38983 = CARTESIAN_POINT ( 'NONE',  ( 96.15314808468748708, 91.99731107132950569, 75.46114583420047950 ) ) ;
#38984 = DIRECTION ( 'NONE',  ( 0.000000000000000000, 0.000000000000000000, 1.000000000000000000 ) ) ;
#38985 = CARTESIAN_POINT ( 'NONE',  ( 0.000000000000000000, 0.000000000000000000, 0.000000000000000000 ) ) ;
#38986 = DIRECTION ( 'NONE',  ( 0.000000000000000000, 0.000000000000000000, 1.000000000000000000 ) ) ;
#38987 = CARTESIAN_POINT ( 'NONE',  ( 10.00000000000000000, -44.99326035066101781, 68.55367621811129197 ) ) ;
#38988 = CARTESIAN_POINT ( 'NONE',  ( 11.99999999999999822, -68.67312586195022561, 35.91791733033451806 ) ) ;
#38989 = ADVANCED_FACE ( 'NONE', ( #72737 ), #55843, .T. ) ;
#38990 = CARTESIAN_POINT ( 'NONE',  ( 0.000000000000000000, 0.000000000000000000, 0.000000000000000000 ) ) ;
#38991 = EDGE_CURVE ( 'NONE', #36331, #4121, #20971, .T. ) ;
#38992 = FACE_OUTER_BOUND ( 'NONE', #40905, .T. ) ;
#38993 = AXIS2_PLACEMENT_3D ( 'NONE', #48554, #25263, #30877 ) ;
#38994 = DIRECTION ( 'NONE',  ( -1.000000000000000000, -0.000000000000000000, 0.000000000000000000 ) ) ;
#38995 = FACE_OUTER_BOUND ( 'NONE', #63384, .T. ) ;
#38996 = DIRECTION ( 'NONE',  ( -1.000000000000000000, 0.000000000000000000, -0.000000000000000000 ) ) ;
#38997 = VERTEX_POINT ( 'NONE', #25871 ) ;
#38998 = CARTESIAN_POINT ( 'NONE',  ( -93.84685191531252713, 88.00268892867056536, 82.23447916753380582 ) ) ;
#38999 = CIRCLE ( 'NONE', #73808, 31.99999999999999289 ) ;
#39000 = DIRECTION ( 'NONE',  ( -1.000000000000000000, 0.000000000000000000, -0.000000000000000000 ) ) ;
#39001 = AXIS2_PLACEMENT_3D ( 'NONE', #50863, #66682, #16660 ) ;
#39002 = VERTEX_POINT ( 'NONE', #38268 ) ;
#39003 = FACE_OUTER_BOUND ( 'NONE', #73094, .T. ) ;
#39004 = MANIFOLD_SOLID_BREP ( 'CirPattern1', #4367 ) ;
#39005 = LINE ( 'NONE', #74320, #29981 ) ;
#39006 = DIRECTION ( 'NONE',  ( 0.000000000000000000, 0.5877852522924685852, 0.8090169943749508930 ) ) ;
#39007 = AXIS2_PLACEMENT_3D ( 'NONE', #46533, #56723, #11568 ) ;
#39008 = DIRECTION ( 'NONE',  ( 0.000000000000000000, 0.9876883405951371042, 0.1564344650402347547 ) ) ;
#39009 = CARTESIAN_POINT ( 'NONE',  ( 97.30629616937498838, -209.9999999999999716, 75.51406250086715488 ) ) ;
#39010 = ORIENTED_EDGE ( 'NONE', *, *, #29100, .T. ) ;
#39011 = ORIENTED_EDGE ( 'NONE', *, *, #45332, .T. ) ;
#39012 = EDGE_CURVE ( 'NONE', #4009, #73251, #9700, .T. ) ;
#39013 = DIRECTION ( 'NONE',  ( -1.000000000000000000, -0.000000000000000000, 0.000000000000000000 ) ) ;
#39014 = DIRECTION ( 'NONE',  ( -0.000000000000000000, -0.4067366430757898277, -0.9135454576426055295 ) ) ;
#39015 = DIRECTION ( 'NONE',  ( 0.000000000000000000, 0.9510565162951503115, 0.3090169943749573878 ) ) ;
#39016 = FACE_OUTER_BOUND ( 'NONE', #56122, .T. ) ;
#39017 = LINE ( 'NONE', #34478, #2123 ) ;
#39018 = CARTESIAN_POINT ( 'NONE',  ( 92.35000000000002274, -208.4700217866474645, 86.77208333333334167 ) ) ;
#39019 = ORIENTED_EDGE ( 'NONE', *, *, #22838, .T. ) ;
#39020 = CARTESIAN_POINT ( 'NONE',  ( 0.000000000000000000, -15.48615015657610527, 39.04073710021338428 ) ) ;
#39021 = ORIENTED_EDGE ( 'NONE', *, *, #10682, .T. ) ;
#39022 = ORIENTED_EDGE ( 'NONE', *, *, #35315, .T. ) ;
#39023 = CYLINDRICAL_SURFACE ( 'NONE', #46550, 2.649999999999985700 ) ;
#39024 =( NAMED_UNIT ( * ) PLANE_ANGLE_UNIT ( ) SI_UNIT ( $, .RADIAN. ) );
#39025 = DIRECTION ( 'NONE',  ( -1.000000000000000000, -0.000000000000000000, -0.000000000000000000 ) ) ;
#39026 = EDGE_CURVE ( 'NONE', #39661, #6755, #15326, .T. ) ;
#39027 = VERTEX_POINT ( 'NONE', #66843 ) ;
#39028 = CARTESIAN_POINT ( 'NONE',  ( 95.00000000000000000, -206.9400435732949575, 78.49062500173430124 ) ) ;
#39029 = CARTESIAN_POINT ( 'NONE',  ( 95.00000000000000000, -213.0599564267049857, 80.71312500173431204 ) ) ;
#39030 = CARTESIAN_POINT ( 'NONE',  ( 97.64999999999999147, 90.00000000000002842, 83.33250000000001023 ) ) ;
#39031 = ADVANCED_FACE ( 'NONE', ( #54819 ), #36782, .T. ) ;
#39032 = VERTEX_POINT ( 'NONE', #8957 ) ;
#39033 = CARTESIAN_POINT ( 'NONE',  ( 93.67500000000001137, -207.7050326799711968, 75.36854166840096525 ) ) ;
#39034 = ORIENTED_EDGE ( 'NONE', *, *, #39255, .T. ) ;
#39035 = DIRECTION ( 'NONE',  ( -1.000000000000000000, -0.000000000000000000, -0.000000000000000000 ) ) ;
#39036 = ORIENTED_EDGE ( 'NONE', *, *, #61280, .F. ) ;
#39037 = CARTESIAN_POINT ( 'NONE',  ( 10.00000000000000000, 10.30890764327382847, 81.34940948281339956 ) ) ;
#39038 = CARTESIAN_POINT ( 'NONE',  ( -93.84685191531254134, 91.99731107132950569, 83.87489583420048689 ) ) ;
#39039 = VECTOR ( 'NONE', #4633, 1000.000000000000000 ) ;
#39040 = CARTESIAN_POINT ( 'NONE',  ( 94.99999999999998579, 87.33691857156068750, 79.00656250086713328 ) ) ;
#39041 = AXIS2_PLACEMENT_3D ( 'NONE', #6051, #39510, #798 ) ;
#39042 = ORIENTED_EDGE ( 'NONE', *, *, #72567, .T. ) ;
#39043 = CARTESIAN_POINT ( 'NONE',  ( 11.99999999999999822, 36.73666225445894185, 65.58780272294090707 ) ) ;
#39044 = EDGE_CURVE ( 'NONE', #68345, #13774, #59728, .T. ) ;
#39045 = PLANE ( 'NONE',  #52097 ) ;
#39046 = CARTESIAN_POINT ( 'NONE',  ( 10.00000000000000000, 0.000000000000000000, 0.000000000000000000 ) ) ;
#39047 = DIRECTION ( 'NONE',  ( 0.000000000000000000, -0.9510565162951565288, 0.3090169943749382364 ) ) ;
#39048 = ORIENTED_EDGE ( 'NONE', *, *, #73940, .T. ) ;
#39049 = CYLINDRICAL_SURFACE ( 'NONE', #66885, 31.99999999999998579 ) ;
#39050 = VECTOR ( 'NONE', #22452, 1000.000000000000000 ) ;
#39051 = CARTESIAN_POINT ( 'NONE',  ( -92.69370383062498320, -208.6684592857803011, 81.75822916753381264 ) ) ;
#39052 = ORIENTED_EDGE ( 'NONE', *, *, #30687, .F. ) ;
#39053 = VERTEX_POINT ( 'NONE', #60477 ) ;
#39055 = DIRECTION ( 'NONE',  ( -1.000000000000000000, 0.000000000000000000, 0.000000000000000000 ) ) ;
#39054 = AXIS2_PLACEMENT_3D ( 'NONE', #37502, #42031, #43149 ) ;
#39056 = ORIENTED_EDGE ( 'NONE', *, *, #71596, .F. ) ;
#39057 = DIRECTION ( 'NONE',  ( 1.000000000000000000, 0.000000000000000000, 0.000000000000000000 ) ) ;
#39058 = CARTESIAN_POINT ( 'NONE',  ( 93.67499999999999716, 87.70503267997126784, 80.58083333333331666 ) ) ;
#39059 = EDGE_LOOP ( 'NONE', ( #71397, #24231, #53539, #70063 ) ) ;
#39060 = CARTESIAN_POINT ( 'NONE',  ( -97.30629616937497417, -208.6684592857803011, 76.88989583420047325 ) ) ;
#39061 = ORIENTED_EDGE ( 'NONE', *, *, #49915, .T. ) ;
#39063 = EDGE_CURVE ( 'NONE', #22889, #67396, #14215, .T. ) ;
#39062 = CARTESIAN_POINT ( 'NONE',  ( 92.35000000045006630, 89.99996890530464100, 88.81037122970248276 ) ) ;
#39064 = DIRECTION ( 'NONE',  ( 0.000000000000000000, 0.7071067811865486830, -0.7071067811865463515 ) ) ;
#39065 = CARTESIAN_POINT ( 'NONE',  ( -92.34999999999999432, -209.9999999999999716, 76.34749999999999659 ) ) ;
#39066 = DIRECTION ( 'NONE',  ( -1.000000000000000000, 0.000000000000000000, 0.000000000000000000 ) ) ;
#39067 = AXIS2_PLACEMENT_3D ( 'NONE', #267, #11124, #56250 ) ;
#39068 = CARTESIAN_POINT ( 'NONE',  ( -97.65000000000001990, 90.00000000000004263, 81.10999999999999943 ) ) ;
#39069 = VECTOR ( 'NONE', #35545, 1000.000000000000227 ) ;
#39070 = CARTESIAN_POINT ( 'NONE',  ( -97.64999999999997726, 88.47002178664750716, 89.41791666666667027 ) ) ;
#39071 = CARTESIAN_POINT ( 'NONE',  ( 94.99999999999998579, 92.66308142843932671, 87.57906250086713840 ) ) ;
#39072 = CARTESIAN_POINT ( 'NONE',  ( -8.000000000000023093, -2.267179479189963121E-13, -20.20000000000037232 ) ) ;
#39073 = FACE_OUTER_BOUND ( 'NONE', #11406, .T. ) ;
#39074 = CARTESIAN_POINT ( 'NONE',  ( 97.64999999999992042, -208.4700217866473793, 86.56041666666668277 ) ) ;
#39075 = DIRECTION ( 'NONE',  ( -1.000000000000000000, 0.000000000000000000, -0.000000000000000000 ) ) ;
#39076 = CARTESIAN_POINT ( 'NONE',  ( 0.000000000000000000, -2.375000000000000444, -4.362804221962445569E-16 ) ) ;
#39077 = ADVANCED_FACE ( 'NONE', ( #54448 ), #8208, .F. ) ;
#39078 = PLANE ( 'NONE',  #3530 ) ;
#39079 = DIRECTION ( 'NONE',  ( 0.7950889364178798102, -0.6064928550163511956, 0.000000000000000000 ) ) ;
#39080 = ADVANCED_FACE ( 'NONE', ( #31875 ), #14966, .F. ) ;
#39081 = AXIS2_PLACEMENT_3D ( 'NONE', #15693, #72807, #44269 ) ;
#39082 = CYLINDRICAL_SURFACE ( 'NONE', #16401, 31.99999999999998579 ) ;
#39083 = EDGE_CURVE ( 'NONE', #53177, #22210, #44283, .T. ) ;
#39084 = CARTESIAN_POINT ( 'NONE',  ( 0.000000000000000000, 0.000000000000000000, 0.000000000000000000 ) ) ;
#39085 = CARTESIAN_POINT ( 'NONE',  ( -3.000000000000000000, 20.85821328998741109, 10.92862929874522315 ) ) ;
#39086 = DIRECTION ( 'NONE',  ( 0.000000000000000000, 0.000000000000000000, 1.000000000000000000 ) ) ;
#39087 = VECTOR ( 'NONE', #24605, 1000.000000000000114 ) ;
#39088 = CARTESIAN_POINT ( 'NONE',  ( 10.00000000000000000, 33.79645857604513992, -16.45098606841138178 ) ) ;
#39089 = CARTESIAN_POINT ( 'NONE',  ( -92.34999999999999432, -209.9999999999999716, 83.96750000000000114 ) ) ;
#39090 = CARTESIAN_POINT ( 'NONE',  ( 97.64999999999999147, 90.00000000000002842, 87.77749999999998920 ) ) ;
#39091 = AXIS2_PLACEMENT_3D ( 'NONE', #1371, #24262, #53942 ) ;
#39092 = CARTESIAN_POINT ( 'NONE',  ( 10.00000000000000000, 0.9569279952884607310, 2.500000000000015543 ) ) ;
#39093 = FACE_OUTER_BOUND ( 'NONE', #6341, .T. ) ;
#39094 = DIRECTION ( 'NONE',  ( -1.000000000000000000, -0.000000000000000000, -0.000000000000000000 ) ) ;
#39095 = CIRCLE ( 'NONE', #64324, 37.49900000000001654 ) ;
#39096 = CARTESIAN_POINT ( 'NONE',  ( 96.66077099052525057, -211.6002630214759961, 74.64190534806809296 ) ) ;
#39097 = ORIENTED_EDGE ( 'NONE', *, *, #19628, .T. ) ;
#39098 = ORIENTED_EDGE ( 'NONE', *, *, #62837, .T. ) ;
#39099 = PLANE ( 'NONE',  #30767 ) ;
#39100 = ORIENTED_EDGE ( 'NONE', *, *, #19170, .F. ) ;
#39101 = AXIS2_PLACEMENT_3D ( 'NONE', #3575, #65603, #48673 ) ;
#39102 = CARTESIAN_POINT ( 'NONE',  ( -93.67499999999998295, -207.7050326799711968, 79.70770833506762187 ) ) ;
#39103 = CIRCLE ( 'NONE', #67935, 77.49899999999999523 ) ;
#39104 = CARTESIAN_POINT ( 'NONE',  ( 92.69370383062501162, -211.3315407142195852, 76.99572916753380980 ) ) ;
#39105 = ORIENTED_EDGE ( 'NONE', *, *, #35492, .T. ) ;
#39106 = CIRCLE ( 'NONE', #65525, 77.49899999999999523 ) ;
#39107 = CARTESIAN_POINT ( 'NONE',  ( 92.69370383062501162, -211.3315407142195852, 81.59947916753381492 ) ) ;
#39108 = EDGE_CURVE ( 'NONE', #70987, #28395, #72827, .T. ) ;
#39109 = EDGE_LOOP ( 'NONE', ( #41991, #71617, #20338, #22369 ) ) ;
#39110 = LINE ( 'NONE', #60923, #63498 ) ;
#39111 = ORIENTED_EDGE ( 'NONE', *, *, #55414, .F. ) ;
#39112 = CARTESIAN_POINT ( 'NONE',  ( 10.00000000000000000, 14.67089635893713684, 73.72996012237443608 ) ) ;
#39113 = VECTOR ( 'NONE', #18196, 1000.000000000000000 ) ;
#39114 = ORIENTED_EDGE ( 'NONE', *, *, #7378, .T. ) ;
#39115 = FACE_OUTER_BOUND ( 'NONE', #10081, .T. ) ;
#39116 = ADVANCED_FACE ( 'NONE', ( #49542 ), #67212, .T. ) ;
#39117 = ORIENTED_EDGE ( 'NONE', *, *, #67415, .F. ) ;
#39118 = FACE_OUTER_BOUND ( 'NONE', #31356, .T. ) ;
#39119 = CARTESIAN_POINT ( 'NONE',  ( 11.99999999999999822, -73.73191006444561424, -14.66109333815538918 ) ) ;
#39120 = ADVANCED_FACE ( 'NONE', ( #4448 ), #74336, .T. ) ;
#39121 = VERTEX_POINT ( 'NONE', #22849 ) ;
#39122 = FACE_OUTER_BOUND ( 'NONE', #51939, .T. ) ;
#39123 = ORIENTED_EDGE ( 'NONE', *, *, #667, .T. ) ;
#39124 =( BOUNDED_CURVE ( )  B_SPLINE_CURVE ( 2, ( #51698, #23140, #6583, #29487, #43403, #14798, #71935 ),
 .UNSPECIFIED., .F., .F. ) 
 B_SPLINE_CURVE_WITH_KNOTS ( ( 3, 2, 2, 3 ),
 ( 0.3749999999999998335, 0.3819444444444441977, 0.3888888888888886730, 0.3958333333333330373 ),
 .UNSPECIFIED. ) 
 CURVE ( )  GEOMETRIC_REPRESENTATION_ITEM ( )  RATIONAL_B_SPLINE_CURVE ( ( 1.000000000000003109, 0.8660254037844354880, 1.000000000000000000, 0.8660254037844387076, 1.000000000000000000, 0.8660254037844440367, 0.9999999999999946709 ) ) 
 REPRESENTATION_ITEM ( '' )  );
#39125 = CARTESIAN_POINT ( 'NONE',  ( 11.99999999999999822, 0.000000000000000000, 0.000000000000000000 ) ) ;
#39126 = VERTEX_POINT ( 'NONE', #38649 ) ;
#39127 = EDGE_CURVE ( 'NONE', #40595, #68521, #68712, .T. ) ;
#39128 = EDGE_LOOP ( 'NONE', ( #28541, #71623, #47254, #37532 ) ) ;
#39129 = ORIENTED_EDGE ( 'NONE', *, *, #41254, .F. ) ;
#39130 = CARTESIAN_POINT ( 'NONE',  ( 96.15314808468750130, -211.9973110713294489, 75.88447916753381151 ) ) ;
#39131 = DIRECTION ( 'NONE',  ( 0.000000000000000000, 0.000000000000000000, -1.000000000000000000 ) ) ;
#39132 = VERTEX_POINT ( 'NONE', #11181 ) ;
#39133 = ORIENTED_EDGE ( 'NONE', *, *, #30702, .T. ) ;
#39134 = ORIENTED_EDGE ( 'NONE', *, *, #66536, .F. ) ;
#39135 = CYLINDRICAL_SURFACE ( 'NONE', #52897, 82.00000000000000000 ) ;
#39136 = FACE_OUTER_BOUND ( 'NONE', #69774, .T. ) ;
#39137 = CARTESIAN_POINT ( 'NONE',  ( -92.69370383062502583, 91.33154071421968467, 76.83697916753382628 ) ) ;
#39138 = ORIENTED_EDGE ( 'NONE', *, *, #40850, .T. ) ;
#39139 = ADVANCED_FACE ( 'NONE', ( #68337 ), #323, .T. ) ;
#39140 = CARTESIAN_POINT ( 'NONE',  ( 96.15314808468748708, 88.00268892867053694, 78.42447916753381776 ) ) ;
#39141 = ORIENTED_EDGE ( 'NONE', *, *, #21739, .F. ) ;
#39142 = CARTESIAN_POINT ( 'NONE',  ( 2.750000000000000000, 2.499999999999999112, 0.000000000000000000 ) ) ;
#39143 = CARTESIAN_POINT ( 'NONE',  ( -97.30629616937497417, -208.6684592857803011, 85.14489583420048291 ) ) ;
#39144 = ORIENTED_EDGE ( 'NONE', *, *, #55431, .T. ) ;
#39146 = ADVANCED_FACE ( 'NONE', ( #4828 ), #51396, .T. ) ;
#39145 = DIRECTION ( 'NONE',  ( -1.000000000000000000, 0.000000000000000000, 0.000000000000000000 ) ) ;
#39147 = DIRECTION ( 'NONE',  ( 1.000000000000000000, -0.000000000000000000, 0.000000000000000000 ) ) ;
#39148 = DIRECTION ( 'NONE',  ( -0.000000000000000000, -0.6691306063588670083, -0.7431448254773863615 ) ) ;
#39149 = CARTESIAN_POINT ( 'NONE',  ( -93.84685191531247028, -211.9973110713294489, 79.69447916753379957 ) ) ;
#39150 = CARTESIAN_POINT ( 'NONE',  ( 93.67499999999999716, 87.70503267997126784, 86.93083333333332519 ) ) ;
#39151 = CARTESIAN_POINT ( 'NONE',  ( 3.000000000000000000, 2.935248768560057897, -3.252606517456513302E-15 ) ) ;
#39152 = AXIS2_PLACEMENT_3D ( 'NONE', #17760, #64013, #52339 ) ;
#39153 = CARTESIAN_POINT ( 'NONE',  ( -96.32499999999996021, -207.7050326799711968, 84.17916666666666003 ) ) ;
#39154 = ORIENTED_EDGE ( 'NONE', *, *, #49246, .T. ) ;
#39155 = AXIS2_PLACEMENT_3D ( 'NONE', #73379, #67381, #38069 ) ;
#39156 = ORIENTED_EDGE ( 'NONE', *, *, #35882, .T. ) ;
#39157 = LINE ( 'NONE', #44057, #19230 ) ;
#39158 = VECTOR ( 'NONE', #56565, 1000.000000000000114 ) ;
#39159 = CARTESIAN_POINT ( 'NONE',  ( 97.64999999999997726, 91.52997821335253548, 84.65541666666669585 ) ) ;
#39160 = CARTESIAN_POINT ( 'NONE',  ( -3.000000000000000000, 18.84667830672579925, 18.68964196561269020 ) ) ;
#39161 = EDGE_CURVE ( 'NONE', #72303, #16639, #39017, .T. ) ;
#39162 = CARTESIAN_POINT ( 'NONE',  ( -96.15314808468752972, 91.99731107132950569, 83.18697916753382060 ) ) ;
#39163 = CARTESIAN_POINT ( 'NONE',  ( 0.000000000000000000, 0.000000000000000000, 0.000000000000000000 ) ) ;
#39164 = EDGE_CURVE ( 'NONE', #59815, #26527, #10817, .T. ) ;
#39165 = AXIS2_PLACEMENT_3D ( 'NONE', #19633, #2766, #42956 ) ;
#39166 = AXIS2_PLACEMENT_3D ( 'NONE', #19535, #20277, #53756 ) ;
#39167 = ORIENTED_EDGE ( 'NONE', *, *, #63814, .T. ) ;
#39168 = CARTESIAN_POINT ( 'NONE',  ( 0.000000000000000000, -50.23322058963298531, -64.81221759200398935 ) ) ;
#39169 = DIRECTION ( 'NONE',  ( -1.000000000000000000, 0.000000000000000000, -0.000000000000000000 ) ) ;
#39170 = CARTESIAN_POINT ( 'NONE',  ( 92.35000000000000853, -209.9999999999999716, 81.74500000000000455 ) ) ;
#39171 = CYLINDRICAL_SURFACE ( 'NONE', #32200, 16.00000000000000000 ) ;
#39172 = DIRECTION ( 'NONE',  ( 2.603472992746261562E-14, 2.546204323184492723E-14, -1.000000000000000000 ) ) ;
#39173 = AXIS2_PLACEMENT_3D ( 'NONE', #65090, #47417, #35748 ) ;
#39174 = CARTESIAN_POINT ( 'NONE',  ( -97.65000000000001990, 90.00000000000004263, 87.45999999999999375 ) ) ;
#39175 = CARTESIAN_POINT ( 'NONE',  ( -92.69370383062498320, -208.6684592857803011, 78.10697916753383652 ) ) ;
#39176 = CARTESIAN_POINT ( 'NONE',  ( 11.99999999999999822, -63.97538442413390669, -51.29473840253292138 ) ) ;
#39177 = ORIENTED_EDGE ( 'NONE', *, *, #38776, .T. ) ;
#39178 = DIRECTION ( 'NONE',  ( 1.000000000000000000, -0.000000000000000000, -0.000000000000000000 ) ) ;
#39179 = CARTESIAN_POINT ( 'NONE',  ( 22.30499999999999972, 3.061616997868384127E-16, -2.500000000000000888 ) ) ;
#39180 = CARTESIAN_POINT ( 'NONE',  ( -10.00000000000000000, 0.000000000000000000, 0.000000000000000000 ) ) ;
#39181 = VERTEX_POINT ( 'NONE', #27730 ) ;
#39182 = LINE ( 'NONE', #55354, #46188 ) ;
#39183 = DIRECTION ( 'NONE',  ( -0.000000000000000000, -0.000000000000000000, 1.000000000000000000 ) ) ;
#39184 = CLOSED_SHELL ( 'NONE', ( #62589, #43492, #40828, #33592, #66730, #26624, #64979, #46346, #71158, #61555 ) ) ;
#39185 = UNCERTAINTY_MEASURE_WITH_UNIT (LENGTH_MEASURE( 1.000000000000000082E-05 ), #30786, 'distance_accuracy_value', 'NONE');
#39186 = CARTESIAN_POINT ( 'NONE',  ( -15.70044424985398557, 0.001194404164747221980, -70.59999999999959641 ) ) ;
#39187 = ORIENTED_EDGE ( 'NONE', *, *, #62686, .T. ) ;
#39188 = DIRECTION ( 'NONE',  ( -1.000000000000000000, 0.000000000000000000, 0.000000000000000000 ) ) ;
#39189 = DIRECTION ( 'NONE',  ( 0.000000000000000000, 0.9135454576426005335, -0.4067366430758010409 ) ) ;
#39190 = ORIENTED_EDGE ( 'NONE', *, *, #13826, .F. ) ;
#39191 = CARTESIAN_POINT ( 'NONE',  ( 92.69370383062501162, -208.6684592857803295, 87.04989583420046984 ) ) ;
#39192 = CARTESIAN_POINT ( 'NONE',  ( 0.000000000000000000, 39.04073710021366139, -15.48615015657542315 ) ) ;
#39193 = AXIS2_PLACEMENT_3D ( 'NONE', #72959, #15460, #39524 ) ;
#39194 = ORIENTED_EDGE ( 'NONE', *, *, #24069, .F. ) ;
#39195 = EDGE_CURVE ( 'NONE', #25891, #54604, #24937, .T. ) ;
#39196 = CARTESIAN_POINT ( 'NONE',  ( 10.00000000000000000, 34.94270380257741948, -74.18225833017854143 ) ) ;
#39197 = ORIENTED_EDGE ( 'NONE', *, *, #33710, .T. ) ;
#39198 = CARTESIAN_POINT ( 'NONE',  ( 22.08297821871651934, -111.8242998470044540, 5.500000000000000000 ) ) ;
#39199 = ORIENTED_EDGE ( 'NONE', *, *, #10868, .T. ) ;
#39200 = PLANE ( 'NONE',  #57490 ) ;
#39201 = EDGE_CURVE ( 'NONE', #25433, #49534, #34081, .T. ) ;
#39202 = ORIENTED_EDGE ( 'NONE', *, *, #3344, .F. ) ;
#39203 = CIRCLE ( 'NONE', #65616, 31.99999999999999645 ) ;
#39204 = ORIENTED_EDGE ( 'NONE', *, *, #38709, .F. ) ;
#39205 = EDGE_CURVE ( 'NONE', #50648, #24697, #61580, .T. ) ;
#39206 = AXIS2_PLACEMENT_3D ( 'NONE', #31200, #49597, #54152 ) ;
#39207 = EDGE_CURVE ( 'NONE', #44003, #35321, #41733, .T. ) ;
#39208 = ORIENTED_EDGE ( 'NONE', *, *, #30223, .F. ) ;
#39209 = CYLINDRICAL_SURFACE ( 'NONE', #52771, 16.00000000000000000 ) ;
#39210 = ORIENTED_EDGE ( 'NONE', *, *, #46401, .T. ) ;
#39211 = AXIS2_PLACEMENT_3D ( 'NONE', #16589, #33129, #67731 ) ;
#39213 = EDGE_CURVE ( 'NONE', #53067, #16620, #51778, .T. ) ;
#39212 = ORIENTED_EDGE ( 'NONE', *, *, #51464, .F. ) ;
#39214 = CARTESIAN_POINT ( 'NONE',  ( 94.99999999999998579, 87.33691857156068750, 76.62531250086715318 ) ) ;
#39215 = CARTESIAN_POINT ( 'NONE',  ( 10.00000000000000000, 36.88895765772642932, -6.736453364083163642 ) ) ;
#39216 = CARTESIAN_POINT ( 'NONE',  ( 8.700667342345820288, -98.11853780484867116, 2.500000000000000000 ) ) ;
#39217 = ORIENTED_EDGE ( 'NONE', *, *, #26134, .T. ) ;
#39218 = EDGE_LOOP ( 'NONE', ( #70261, #14786 ) ) ;
#39219 = EDGE_CURVE ( 'NONE', #20422, #57250, #22469, .T. ) ;
#39220 = ORIENTED_EDGE ( 'NONE', *, *, #9761, .F. ) ;
#39221 = CARTESIAN_POINT ( 'NONE',  ( 94.99999999999998579, 87.33691857156068750, 89.16656250086712987 ) ) ;
#39222 = ORIENTED_EDGE ( 'NONE', *, *, #10589, .T. ) ;
#39223 = CARTESIAN_POINT ( 'NONE',  ( 97.30629616937498838, -209.9999999999999716, 84.24531250086714351 ) ) ;
#39224 = DIRECTION ( 'NONE',  ( 1.000000000000000000, 0.000000000000000000, 0.000000000000000000 ) ) ;
#39225 = DIRECTION ( 'NONE',  ( -1.000000000000000000, -0.000000000000000000, 0.000000000000000000 ) ) ;
#39226 = CIRCLE ( 'NONE', #3240, 15.99999999999999822 ) ;
#39227 = DIRECTION ( 'NONE',  ( -2.603472992746261562E-14, -2.546204323184492723E-14, 1.000000000000000000 ) ) ;
#39228 = CARTESIAN_POINT ( 'NONE',  ( 11.99999999999999822, 68.67312586194995561, 35.91791733033500122 ) ) ;
#39229 = CARTESIAN_POINT ( 'NONE',  ( 10.00000000000000000, -37.16516213103273714, -4.992566952385376844 ) ) ;
#39230 = DIRECTION ( 'NONE',  ( -1.000000000000000000, 0.000000000000000000, 0.000000000000000000 ) ) ;
#39231 = CARTESIAN_POINT ( 'NONE',  ( 92.34999999999999432, 88.47002178664752137, 85.05229166840096866 ) ) ;
#39232 = CARTESIAN_POINT ( 'NONE',  ( -94.99999999999997158, -212.6630814284392557, 86.62656250086715204 ) ) ;
#39233 = CARTESIAN_POINT ( 'NONE',  ( -92.69370383062502583, 88.66845928578038638, 84.98614583420047097 ) ) ;
#39234 = ORIENTED_EDGE ( 'NONE', *, *, #35492, .F. ) ;
#39236 = CARTESIAN_POINT ( 'NONE',  ( -95.00000000000002842, 92.66308142843932671, 85.67406250086715147 ) ) ;
#39235 = CARTESIAN_POINT ( 'NONE',  ( 96.15314808468748708, 91.99731107132950569, 89.43114583420047836 ) ) ;
#39237 = ORIENTED_EDGE ( 'NONE', *, *, #48324, .T. ) ;
#39238 = CARTESIAN_POINT ( 'NONE',  ( 97.30629616937498838, 91.33154071421968467, 74.93197916753381094 ) ) ;
#39240 = EDGE_CURVE ( 'NONE', #24844, #55952, #15713, .T. ) ;
#39239 = CARTESIAN_POINT ( 'NONE',  ( 3.000000000000000000, -1.467624384280027838, 2.542000000000001592 ) ) ;
#39241 = DIRECTION ( 'NONE',  ( 0.000000000000000000, -0.9969173337331287410, 0.07845909572783486829 ) ) ;
#39242 = CARTESIAN_POINT ( 'NONE',  ( 11.99999999999999822, 0.000000000000000000, 0.000000000000000000 ) ) ;
#39243 = CARTESIAN_POINT ( 'NONE',  ( -97.30629616937497417, -211.3315407142195852, 88.42572916753381662 ) ) ;
#39244 = FACE_OUTER_BOUND ( 'NONE', #70591, .T. ) ;
#39245 = CARTESIAN_POINT ( 'NONE',  ( 15.00000000000000000, -10.45096189432344502, -21.10159698893425784 ) ) ;
#39246 = DIRECTION ( 'NONE',  ( 0.000000000000000000, -0.8090169943749531134, 0.5877852522924653655 ) ) ;
#39247 = EDGE_CURVE ( 'NONE', #20797, #26436, #27347, .T. ) ;
#39248 = EDGE_CURVE ( 'NONE', #24726, #70, #39768, .T. ) ;
#39249 = DIRECTION ( 'NONE',  ( -0.000000000000000000, 0.5000000000000003331, -0.8660254037844384856 ) ) ;
#39250 = ORIENTED_EDGE ( 'NONE', *, *, #70760, .F. ) ;
#39251 = AXIS2_PLACEMENT_3D ( 'NONE', #67606, #60857, #26255 ) ;
#39252 = ORIENTED_EDGE ( 'NONE', *, *, #18019, .T. ) ;
#39253 = CARTESIAN_POINT ( 'NONE',  ( -97.65000000000001990, 88.47002178664754979, 81.16291666666666060 ) ) ;
#39254 = DIRECTION ( 'NONE',  ( -1.000000000000000000, -0.000000000000000000, -0.000000000000000000 ) ) ;
#39255 = EDGE_CURVE ( 'NONE', #15890, #12172, #57058, .T. ) ;
#39256 = DIRECTION ( 'NONE',  ( 1.000000000000000000, -0.000000000000000000, -0.000000000000000000 ) ) ;
#39257 = DIRECTION ( 'NONE',  ( 0.000000000000000000, 0.000000000000000000, -1.000000000000000000 ) ) ;
#39258 = DIRECTION ( 'NONE',  ( 0.000000000000000000, 0.000000000000000000, 1.000000000000000000 ) ) ;
#39259 = CARTESIAN_POINT ( 'NONE',  ( 0.000000000000000000, 0.000000000000000000, 21.00000000000000000 ) ) ;
#39260 = CARTESIAN_POINT ( 'NONE',  ( 0.000000000000000000, 0.000000000000000000, 0.000000000000000000 ) ) ;
#39261 = VERTEX_POINT ( 'NONE', #69797 ) ;
#39262 = CARTESIAN_POINT ( 'NONE',  ( -93.84685191531252713, 88.00268892867056536, 83.50447916753381605 ) ) ;
#39263 = AXIS2_PLACEMENT_3D ( 'NONE', #28649, #45605, #17744 ) ;
#39264 = FACE_OUTER_BOUND ( 'NONE', #54118, .T. ) ;
#39265 = CYLINDRICAL_SURFACE ( 'NONE', #48972, 2.649999999999985700 ) ;
#39266 = DIRECTION ( 'NONE',  ( 0.000000000000000000, 0.000000000000000000, 1.000000000000000000 ) ) ;
#39267 = VECTOR ( 'NONE', #61484, 1000.000000000000114 ) ;
#39268 = CYLINDRICAL_SURFACE ( 'NONE', #32107, 31.99999999999998579 ) ;
#39269 = CARTESIAN_POINT ( 'NONE',  ( 10.00000000000000000, 31.52238457039638320, -27.75498641678709788 ) ) ;
#39270 = CARTESIAN_POINT ( 'NONE',  ( -97.30629616937495996, -209.9999999999999716, 89.80156250086714920 ) ) ;
#39271 = VECTOR ( 'NONE', #58867, 1000.000000000000000 ) ;
#39272 =( NAMED_UNIT ( * ) SI_UNIT ( $, .STERADIAN. ) SOLID_ANGLE_UNIT ( ) );
#39273 =( BOUNDED_CURVE ( )  B_SPLINE_CURVE ( 2, ( #7976, #30892, #2384, #25277, #48201, #10188, #21843, #55688, #67339 ),
 .UNSPECIFIED., .F., .F. ) 
 B_SPLINE_CURVE_WITH_KNOTS ( ( 3, 2, 2, 2, 3 ),
 ( 0.7196881748034550386, 0.7267438507108833212, 0.7337996162517648191, 0.7408553817926464280, 0.7408554641864709689 ),
 .UNSPECIFIED. ) 
 CURVE ( )  GEOMETRIC_REPRESENTATION_ITEM ( )  RATIONAL_B_SPLINE_CURVE ( ( 0.9999965961303289852, 0.8660271057408951423, 1.000000000000000000, 0.8660254037844387076, 1.000000000000000000, 0.8660254037844387076, 1.000000000000000000, 0.9999984355093277655, 0.9999968710551943030 ) ) 
 REPRESENTATION_ITEM ( '' )  );
#39274 = AXIS2_PLACEMENT_3D ( 'NONE', #35282, #7076, #58577 ) ;
#39275 = CARTESIAN_POINT ( 'NONE',  ( 97.30629616937498838, 88.66845928578035796, 80.54114583420049200 ) ) ;
#39276 = CARTESIAN_POINT ( 'NONE',  ( -94.99999999999997158, -207.3369185715606307, 80.11781250086714579 ) ) ;
#39277 = DIRECTION ( 'NONE',  ( -0.000000000000000000, -0.000000000000000000, -1.000000000000000000 ) ) ;
#39278 = ORIENTED_EDGE ( 'NONE', *, *, #27692, .T. ) ;
#39279 = CARTESIAN_POINT ( 'NONE',  ( 92.34999999999999432, 90.00000000000002842, 88.09499999999999886 ) ) ;
#39280 = LINE ( 'NONE', #11791, #17842 ) ;
#39281 = CARTESIAN_POINT ( 'NONE',  ( 93.67499999999998295, 92.29496732002878900, 85.52854166840096184 ) ) ;
#39282 = AXIS2_PLACEMENT_3D ( 'NONE', #37819, #55093, #72378 ) ;
#39283 = CARTESIAN_POINT ( 'NONE',  ( -97.30629616937501680, 90.00000000000004263, 79.64156250086715261 ) ) ;
#39284 = CARTESIAN_POINT ( 'NONE',  ( 97.30629616937498838, -209.9999999999999716, 79.80031250086713612 ) ) ;
#39285 = EDGE_LOOP ( 'NONE', ( #32627, #18255, #61718, #23483 ) ) ;
#39286 = CIRCLE ( 'NONE', #74098, 82.00000000000000000 ) ;
#39287 = CARTESIAN_POINT ( 'NONE',  ( 11.99999999999999822, -46.11716303203136391, -67.80270845531939017 ) ) ;
#39288 = ORIENTED_EDGE ( 'NONE', *, *, #64674, .T. ) ;
#39289 = FACE_OUTER_BOUND ( 'NONE', #54888, .T. ) ;
#39290 = VERTEX_POINT ( 'NONE', #64180 ) ;
#39291 = EDGE_CURVE ( 'NONE', #44444, #65198, #30313, .T. ) ;
#39292 = DIRECTION ( 'NONE',  ( 0.000000000000000000, -0.000000000000000000, 1.000000000000000000 ) ) ;
#39293 = ADVANCED_FACE ( 'NONE', ( #41599 ), #18295, .F. ) ;
#39294 = ORIENTED_EDGE ( 'NONE', *, *, #23276, .T. ) ;
#39295 = ORIENTED_EDGE ( 'NONE', *, *, #17146, .F. ) ;
#39297 = EDGE_CURVE ( 'NONE', #41422, #6148, #13020, .T. ) ;
#39296 = ORIENTED_EDGE ( 'NONE', *, *, #10942, .T. ) ;
#39298 = EDGE_CURVE ( 'NONE', #57179, #10428, #18973, .T. ) ;
#39299 = CARTESIAN_POINT ( 'NONE',  ( 10.00000000000000000, 41.91543099594818500, 2.663952781846293139 ) ) ;
#39300 = VERTEX_POINT ( 'NONE', #35954 ) ;
#39301 =( REPRESENTATION_RELATIONSHIP ('NONE','NONE', #31117, #10045 ) REPRESENTATION_RELATIONSHIP_WITH_TRANSFORMATION ( #10543 )SHAPE_REPRESENTATION_RELATIONSHIP( ) );
#39302 = CARTESIAN_POINT ( 'NONE',  ( -30.50000000000000000, -120.0000000000000000, -5.500000000000000000 ) ) ;
#39303 = DIRECTION ( 'NONE',  ( -1.000000000000000000, 0.000000000000000000, 0.000000000000000000 ) ) ;
#39304 = CARTESIAN_POINT ( 'NONE',  ( 97.30629616937498838, 88.66845928578037217, 86.25614583420048120 ) ) ;
#39305 = CARTESIAN_POINT ( 'NONE',  ( 15.00000000000000000, -13.04903810567646971, 19.60159698893442481 ) ) ;
#39306 = CARTESIAN_POINT ( 'NONE',  ( 95.00000000000000000, -206.9400435732949575, 76.50624999999999432 ) ) ;
#39307 = AXIS2_PLACEMENT_3D ( 'NONE', #13511, #47722, #70265 ) ;
#39308 = ORIENTED_EDGE ( 'NONE', *, *, #11612, .T. ) ;
#39309 = ORIENTED_EDGE ( 'NONE', *, *, #27425, .T. ) ;
#39310 = VERTEX_POINT ( 'NONE', #12652 ) ;
#39311 = ORIENTED_EDGE ( 'NONE', *, *, #9692, .T. ) ;
#39312 = DIRECTION ( 'NONE',  ( 0.000000000000000000, 0.000000000000000000, 1.000000000000000000 ) ) ;
#39313 = SURFACE_SIDE_STYLE ('',( #73876 ) ) ;
#39314 = CARTESIAN_POINT ( 'NONE',  ( 12.00000000000000000, -23.29833615347109088, -3.418703333116486665 ) ) ;
#39315 = DIRECTION ( 'NONE',  ( -1.000000000000000000, 3.061616997868382648E-16, 0.000000000000000000 ) ) ;
#39316 = DIRECTION ( 'NONE',  ( 1.000000000000000000, 0.000000000000000000, 0.000000000000000000 ) ) ;
#39317 = CARTESIAN_POINT ( 'NONE',  ( -97.64999999998384794, -210.0000060634594661, 88.17456390440159453 ) ) ;
#39318 = EDGE_CURVE ( 'NONE', #55565, #52257, #69380, .T. ) ;
#39319 = CARTESIAN_POINT ( 'NONE',  ( 92.35000000049315361, 89.99996796133687837, 83.73041644179049570 ) ) ;
#39320 = ORIENTED_EDGE ( 'NONE', *, *, #47954, .F. ) ;
#39321 = CARTESIAN_POINT ( 'NONE',  ( -92.34999999999999432, -208.4700217866474645, 84.09979166840095388 ) ) ;
#39322 = ORIENTED_EDGE ( 'NONE', *, *, #49410, .F. ) ;
#39323 = CARTESIAN_POINT ( 'NONE',  ( 10.00000000000000000, 72.35160999960844208, -20.41045688087747223 ) ) ;
#39324 = ORIENTED_EDGE ( 'NONE', *, *, #46250, .F. ) ;
#39326 = CARTESIAN_POINT ( 'NONE',  ( -95.00000000000002842, 86.94004357329504273, 80.07812500173432113 ) ) ;
#39325 = CARTESIAN_POINT ( 'NONE',  ( 97.64999999999997726, 91.52997821335252127, 82.82979166840095786 ) ) ;
#39327 = ORIENTED_EDGE ( 'NONE', *, *, #1834, .F. ) ;
#39328 = CARTESIAN_POINT ( 'NONE',  ( 97.30629616937498838, 90.00000000000002842, 83.76906250086716454 ) ) ;
#39329 = LINE ( 'NONE', #21652, #8188 ) ;
#39330 = DIRECTION ( 'NONE',  ( -1.000000000000000000, 0.000000000000000000, 0.000000000000000000 ) ) ;
#39331 = CARTESIAN_POINT ( 'NONE',  ( 10.00000000000000000, 59.75363087400074846, 56.15606465354979804 ) ) ;
#39332 = CARTESIAN_POINT ( 'NONE',  ( 4.467624384280048488, 0.000000000000000000, 0.000000000000000000 ) ) ;
#39333 = CARTESIAN_POINT ( 'NONE',  ( 5.000000000000002665, -39.47590169984793818, -71.87247863392457248 ) ) ;
#39334 = ORIENTED_EDGE ( 'NONE', *, *, #8387, .F. ) ;
#39335 = DIRECTION ( 'NONE',  ( -0.000000000000000000, 0.000000000000000000, -1.000000000000000000 ) ) ;
#39336 = CARTESIAN_POINT ( 'NONE',  ( 15.00000000000000000, 20.85821328998756385, 10.92862929874494249 ) ) ;
#39337 = EDGE_CURVE ( 'NONE', #9704, #30416, #23571, .T. ) ;
#39338 = EDGE_CURVE ( 'NONE', #17434, #64362, #20144, .T. ) ;
#39339 = DIRECTION ( 'NONE',  ( 0.000000000000000000, 0.000000000000000000, 1.000000000000000000 ) ) ;
#39340 = ORIENTED_EDGE ( 'NONE', *, *, #39219, .T. ) ;
#39341 = VECTOR ( 'NONE', #71722, 1000.000000000000000 ) ;
#39342 = ORIENTED_EDGE ( 'NONE', *, *, #26552, .F. ) ;
#39343 = VECTOR ( 'NONE', #36064, 1000.000000000000000 ) ;
#39344 = CARTESIAN_POINT ( 'NONE',  ( 0.000000000000000000, 14.66109333815564852, -73.73191006444555740 ) ) ;
#39345 = DIRECTION ( 'NONE',  ( -1.000000000000000000, 0.000000000000000000, -0.000000000000000000 ) ) ;
#39346 = CARTESIAN_POINT ( 'NONE',  ( 10.00000000000000000, -81.96053171279902472, 2.543863470248087566 ) ) ;
#39347 = CARTESIAN_POINT ( 'NONE',  ( -93.84685191531248449, -208.0026889286704943, 80.69989583420047552 ) ) ;
#39348 = VERTEX_POINT ( 'NONE', #12283 ) ;
#39349 = CARTESIAN_POINT ( 'NONE',  ( -96.15314808468752972, 91.99731107132950569, 88.90197916753380980 ) ) ;
#39350 = ORIENTED_EDGE ( 'NONE', *, *, #4612, .F. ) ;
#39351 = CARTESIAN_POINT ( 'NONE',  ( 0.000000000000000000, 0.000000000000000000, -1.466666666666671670 ) ) ;
#39352 = CARTESIAN_POINT ( 'NONE',  ( 0.000000000000000000, -69.42325613327415113, -34.44570377933671779 ) ) ;
#39353 = LINE ( 'NONE', #39731, #8110 ) ;
#39354 = DIRECTION ( 'NONE',  ( -0.000000000000000000, -0.000000000000000000, 1.000000000000000000 ) ) ;
#39355 = DIRECTION ( 'NONE',  ( -0.000000000000000000, -0.000000000000000000, 1.000000000000000000 ) ) ;
#39356 = DIRECTION ( 'NONE',  ( 1.000000000000000000, 0.000000000000000000, 0.000000000000000000 ) ) ;
#39357 = CARTESIAN_POINT ( 'NONE',  ( 97.64999999999999147, 89.99999996655866141, 87.85687500050293863 ) ) ;
#39358 = LINE ( 'NONE', #67555, #1686 ) ;
#39359 = FACE_OUTER_BOUND ( 'NONE', #31833, .T. ) ;
#39360 = CARTESIAN_POINT ( 'NONE',  ( 6.000000000000000000, -79.10210256391383155, 21.60688246758558506 ) ) ;
#39361 =( BOUNDED_CURVE ( )  B_SPLINE_CURVE ( 2, ( #33975, #9928, #5060, #73449, #62953, #26847, #11055, #51260, #17065 ),
 .UNSPECIFIED., .F., .F. ) 
 B_SPLINE_CURVE_WITH_KNOTS ( ( 3, 2, 2, 2, 3 ),
 ( 0.8255245790604923695, 0.8325803338282082855, 0.8396360993691253105, 0.8466918649100423355, 0.8466920362409167122 ),
 .UNSPECIFIED. ) 
 CURVE ( )  GEOMETRIC_REPRESENTATION_ITEM ( )  RATIONAL_B_SPLINE_CURVE ( ( 1.000000000000000000, 0.8660254037844387076, 1.000000000000000000, 0.8660254037844387076, 1.000000000000000000, 0.8660254037844387076, 1.000000000000000000, 0.9999967467761544659, 0.9999934937103009958 ) ) 
 REPRESENTATION_ITEM ( '' )  );
#39362 = CARTESIAN_POINT ( 'NONE',  ( 0.000000000000000000, 0.000000000000000000, 0.000000000000000000 ) ) ;
#39363 = DIRECTION ( 'NONE',  ( 0.000000000000000000, 0.000000000000000000, 1.000000000000000000 ) ) ;
#39364 = MECHANICAL_DESIGN_GEOMETRIC_PRESENTATION_REPRESENTATION (  '', ( #10522 ), #68180 ) ;
#39365 = CARTESIAN_POINT ( 'NONE',  ( 15.00000000000000000, -3.948201729842355068, -23.21447184625292692 ) ) ;
#39366 = CARTESIAN_POINT ( 'NONE',  ( 11.99999999999999822, -20.40083707022829174, -72.35432306680507963 ) ) ;
#39367 = ORIENTED_EDGE ( 'NONE', *, *, #32306, .T. ) ;
#39368 = CARTESIAN_POINT ( 'NONE',  ( 10.00000000000000000, -62.50884508063395373, -41.76106447765554464 ) ) ;
#39369 = CARTESIAN_POINT ( 'NONE',  ( -92.69370383062504004, 90.00000000000004263, 78.53031250086714010 ) ) ;
#39370 = CIRCLE ( 'NONE', #36949, 77.49900000000000944 ) ;
#39371 = CARTESIAN_POINT ( 'NONE',  ( 96.15314808468750130, -211.9973110713294489, 89.21947916753380525 ) ) ;
#39372 = EDGE_LOOP ( 'NONE', ( #18283, #48021, #63118, #41445 ) ) ;
#39373 = LINE ( 'NONE', #28079, #67861 ) ;
#39374 = DIRECTION ( 'NONE',  ( 0.000000000000000000, -0.8090169943749531134, 0.5877852522924653655 ) ) ;
#39375 = CARTESIAN_POINT ( 'NONE',  ( 10.00000000000000000, -77.19088730480528682, 6.903761155837488062 ) ) ;
#39376 = PRODUCT_RELATED_PRODUCT_CATEGORY ( 'part', '', ( #9766 ) ) ;
#39377 = EDGE_CURVE ( 'NONE', #71829, #37544, #3387, .T. ) ;
#39378 = CARTESIAN_POINT ( 'NONE',  ( 92.35000000049298308, -210.0000320324309939, 85.63541623677062375 ) ) ;
#39379 = CARTESIAN_POINT ( 'NONE',  ( 95.00000000000000000, -207.3369185715606307, 75.03781250086714749 ) ) ;
#39380 = VECTOR ( 'NONE', #55847, 1000.000000000000000 ) ;
#39381 = EDGE_CURVE ( 'NONE', #56786, #1038, #64602, .T. ) ;
#39382 = CIRCLE ( 'NONE', #16564, 15.99999999999999822 ) ;
#39383 = VERTEX_POINT ( 'NONE', #70519 ) ;
#39384 = ORIENTED_EDGE ( 'NONE', *, *, #1253, .F. ) ;
#39385 = AXIS2_PLACEMENT_3D ( 'NONE', #63072, #73946, #45397 ) ;
#39386 = EDGE_CURVE ( 'NONE', #49355, #65052, #57409, .T. ) ;
#39387 = CARTESIAN_POINT ( 'NONE',  ( 10.00000000000000000, 0.000000000000000000, 0.000000000000000000 ) ) ;
#39388 = CARTESIAN_POINT ( 'NONE',  ( 0.000000000000000000, 0.000000000000000000, 0.000000000000000000 ) ) ;
#39389 = CIRCLE ( 'NONE', #6971, 42.00000000000000000 ) ;
#39390 = CARTESIAN_POINT ( 'NONE',  ( 0.000000000000000000, 0.000000000000000000, 0.000000000000000000 ) ) ;
#39391 = DIRECTION ( 'NONE',  ( 0.000000000000000000, 0.000000000000000000, 1.000000000000000000 ) ) ;
#39392 = ADVANCED_FACE ( 'NONE', ( #23949 ), #18660, .T. ) ;
#39393 = CARTESIAN_POINT ( 'NONE',  ( 0.000000000000000000, 0.000000000000000000, 20.00000000000000000 ) ) ;
#39394 = CARTESIAN_POINT ( 'NONE',  ( 92.35000000000002274, -211.5299782133524502, 87.51291666666666913 ) ) ;
#39395 = ORIENTED_EDGE ( 'NONE', *, *, #3082, .F. ) ;
#39396 = ORIENTED_EDGE ( 'NONE', *, *, #4591, .T. ) ;
#39397 = VERTEX_POINT ( 'NONE', #46504 ) ;
#39398 = CARTESIAN_POINT ( 'NONE',  ( 26.49955575015424358, 0.001194404164430948063, -49.00000000000068923 ) ) ;
#39399 = DIRECTION ( 'NONE',  ( 1.000000000000000000, 0.000000000000000000, 0.000000000000000000 ) ) ;
#39400 = VERTEX_POINT ( 'NONE', #7014 ) ;
#39401 = LINE ( 'NONE', #10446, #41387 ) ;
#39402 = CARTESIAN_POINT ( 'NONE',  ( 96.32499999999998863, -212.2949673200287179, 75.68604166840097491 ) ) ;
#39403 = CARTESIAN_POINT ( 'NONE',  ( 92.34999999999999432, 88.47002178664753558, 82.43291666666665662 ) ) ;
#39404 = EDGE_CURVE ( 'NONE', #24232, #50309, #4563, .T. ) ;
#39405 = VERTEX_POINT ( 'NONE', #41984 ) ;
#39406 = CARTESIAN_POINT ( 'NONE',  ( 92.35000000000000853, -208.4700217866474645, 75.42145833506764063 ) ) ;
#39407 = ORIENTED_EDGE ( 'NONE', *, *, #61992, .F. ) ;
#39408 = EDGE_CURVE ( 'NONE', #11928, #28623, #70584, .T. ) ;
#39409 = DIRECTION ( 'NONE',  ( -1.000000000000000000, 0.000000000000000000, -0.000000000000000000 ) ) ;
#39410 = VERTEX_POINT ( 'NONE', #17932 ) ;
#39411 = ORIENTED_EDGE ( 'NONE', *, *, #5650, .F. ) ;
#39412 = CARTESIAN_POINT ( 'NONE',  ( -92.69370383062504004, 90.00000000000004263, 84.40406250086715545 ) ) ;
#39413 = CARTESIAN_POINT ( 'NONE',  ( 97.30629616937498838, 90.00000000000002842, 78.53031250086714010 ) ) ;
#39414 = ORIENTED_EDGE ( 'NONE', *, *, #57625, .F. ) ;
#39415 = CARTESIAN_POINT ( 'NONE',  ( 11.99999999999999822, 0.8261519478431255115, 77.49459641780886443 ) ) ;
#39416 = AXIS2_PLACEMENT_3D ( 'NONE', #16701, #17439, #50904 ) ;
#39417 = VECTOR ( 'NONE', #68682, 1000.000000000000000 ) ;
#39418 = CARTESIAN_POINT ( 'NONE',  ( -13.05994868825747446, -139.5943292883446532, 5.500000000000000000 ) ) ;
#39419 = CARTESIAN_POINT ( 'NONE',  ( 10.00000000000000000, 14.67089635893819377, -73.72996012237423713 ) ) ;
#39420 = CYLINDRICAL_SURFACE ( 'NONE', #41938, 2.649999999999985700 ) ;
#39421 = EDGE_LOOP ( 'NONE', ( #56607, #57173, #40300, #40529 ) ) ;
#39422 = LINE ( 'NONE', #20998, #45324 ) ;
#39423 = EDGE_CURVE ( 'NONE', #65777, #65222, #45399, .T. ) ;
#39424 = CARTESIAN_POINT ( 'NONE',  ( -97.30629616937497417, -211.3315407142195852, 78.90072916753381094 ) ) ;
#39425 = VERTEX_POINT ( 'NONE', #41236 ) ;
#39426 = CIRCLE ( 'NONE', #72983, 15.99999999999999822 ) ;
#39427 = EDGE_LOOP ( 'NONE', ( #21921, #54559, #68218, #43502 ) ) ;
#39428 = VECTOR ( 'NONE', #55907, 1000.000000000000114 ) ;
#39429 = CARTESIAN_POINT ( 'NONE',  ( -92.35000000053402403, -209.9999467984910382, 78.96687695417375608 ) ) ;
#39430 = ORIENTED_EDGE ( 'NONE', *, *, #15289, .T. ) ;
#39431 = DIRECTION ( 'NONE',  ( 1.000000000000000000, 0.000000000000000000, 0.000000000000000000 ) ) ;
#39432 = CARTESIAN_POINT ( 'NONE',  ( 92.34999999999999432, 90.00000000000002842, 89.90078125043358170 ) ) ;
#39433 = ORIENTED_EDGE ( 'NONE', *, *, #70592, .F. ) ;
#39434 = CARTESIAN_POINT ( 'NONE',  ( -97.30629616937497417, -211.3315407142195852, 77.63072916753380071 ) ) ;
#39435 = ORIENTED_EDGE ( 'NONE', *, *, #48707, .F. ) ;
#39436 = CARTESIAN_POINT ( 'NONE',  ( 0.000000000000000000, 0.000000000000000000, 0.000000000000000000 ) ) ;
#39437 = DIRECTION ( 'NONE',  ( -1.000000000000000000, 0.000000000000000000, 0.000000000000000000 ) ) ;
#39438 = DIRECTION ( 'NONE',  ( 0.000000000000000000, -0.4067366430758009854, -0.9135454576426004225 ) ) ;
#39439 = CARTESIAN_POINT ( 'NONE',  ( 0.000000000000000000, 0.000000000000000000, 0.000000000000000000 ) ) ;
#39440 = AXIS2_PLACEMENT_3D ( 'NONE', #46035, #56194, #5818 ) ;
#39441 = LINE ( 'NONE', #21375, #665 ) ;
#39442 = CIRCLE ( 'NONE', #15422, 77.49900000000000944 ) ;
#39443 = DIRECTION ( 'NONE',  ( 0.000000000000000000, 0.000000000000000000, 1.000000000000000000 ) ) ;
#39445 = CIRCLE ( 'NONE', #58639, 3.000000000000000000 ) ;
#39444 = CARTESIAN_POINT ( 'NONE',  ( 92.69370383062498320, 88.66845928578035796, 85.25072916753379104 ) ) ;
#39446 = DIRECTION ( 'NONE',  ( -1.000000000000000000, 0.000000000000000000, -0.000000000000000000 ) ) ;
#39447 = DIRECTION ( 'NONE',  ( -1.000000000000000000, -0.000000000000000000, -0.000000000000000000 ) ) ;
#39448 = CARTESIAN_POINT ( 'NONE',  ( -2.500000000000015543, -73.00000000000001421, -255.0000000000000000 ) ) ;
#39449 = AXIS2_PLACEMENT_3D ( 'NONE', #51678, #18201, #226 ) ;
#39450 = DIRECTION ( 'NONE',  ( -0.4279312458752990711, -0.9038112904824846527, 0.000000000000000000 ) ) ;
#39451 = AXIS2_PLACEMENT_3D ( 'NONE', #27704, #8660, #5167 ) ;
#39452 = CARTESIAN_POINT ( 'NONE',  ( 94.99999999999998579, 86.94004357329502852, 86.42812500173430124 ) ) ;
#39453 = DIRECTION ( 'NONE',  ( 0.000000000000000000, 0.000000000000000000, 1.000000000000000000 ) ) ;
#39454 = PLANE ( 'NONE',  #3892 ) ;
#39455 = AXIS2_PLACEMENT_3D ( 'NONE', #18101, #41760, #63611 ) ;
#39456 = DIRECTION ( 'NONE',  ( -1.000000000000000000, 0.000000000000000000, 0.000000000000000000 ) ) ;
#39457 = LINE ( 'NONE', #62400, #70806 ) ;
#39458 = ADVANCED_FACE ( 'NONE', ( #29197 ), #46886, .T. ) ;
#39459 = DIRECTION ( 'NONE',  ( -1.000000000000000000, 0.000000000000000000, -0.000000000000000000 ) ) ;
#39460 = DIRECTION ( 'NONE',  ( -1.000000000000000000, 0.000000000000000000, 0.000000000000000000 ) ) ;
#39461 = CARTESIAN_POINT ( 'NONE',  ( -3.961125083139900749, -143.2122702051246677, -5.500000000000000000 ) ) ;
#39462 = CARTESIAN_POINT ( 'NONE',  ( -97.64999999999994884, -208.4700217866474645, 84.86708333333334053 ) ) ;
#39463 = EDGE_CURVE ( 'NONE', #12105, #1365, #59779, .T. ) ;
#39464 = EDGE_CURVE ( 'NONE', #16205, #37410, #32160, .T. ) ;
#39465 = DIRECTION ( 'NONE',  ( -0.8774505977381983346, -0.4796670183876294291, 0.000000000000000000 ) ) ;
#39466 = VECTOR ( 'NONE', #15180, 1000.000000000000000 ) ;
#39467 = CARTESIAN_POINT ( 'NONE',  ( 92.34999999999999432, 90.00000000000002842, 90.00000000000000000 ) ) ;
#39468 = CARTESIAN_POINT ( 'NONE',  ( 12.00000000000000000, 16.83928648764922542, -16.46020748918050458 ) ) ;
#39469 = DIRECTION ( 'NONE',  ( 0.000000000000000000, -0.3826834323650772363, -0.9238795325112919565 ) ) ;
#39470 = VECTOR ( 'NONE', #46757, 1000.000000000000000 ) ;
#39471 = EDGE_CURVE ( 'NONE', #11405, #21157, #22584, .T. ) ;
#39472 = CARTESIAN_POINT ( 'NONE',  ( 5.000000000000000000, 31.52238457039637609, -27.75498641678709788 ) ) ;
#39473 = CARTESIAN_POINT ( 'NONE',  ( 97.30629616937498838, -211.3315407142195852, 86.89114583420050053 ) ) ;
#39474 = AXIS2_PLACEMENT_3D ( 'NONE', #44061, #22238, #56078 ) ;
#39475 = AXIS2_PLACEMENT_3D ( 'NONE', #41397, #29362, #52307 ) ;
#39476 = VERTEX_POINT ( 'NONE', #66029 ) ;
#39477 = ORIENTED_EDGE ( 'NONE', *, *, #56665, .F. ) ;
#39478 = CARTESIAN_POINT ( 'NONE',  ( 15.69955575014744831, 0.001194404164628767254, -85.59999999999999432 ) ) ;
#39479 = ORIENTED_EDGE ( 'NONE', *, *, #47349, .F. ) ;
#39480 = CARTESIAN_POINT ( 'NONE',  ( 103.9230484541331947, -179.9999999999990337, -5.500000000000000000 ) ) ;
#39481 = CARTESIAN_POINT ( 'NONE',  ( 92.69370383062501162, -209.9999999999999716, 79.48281250086714067 ) ) ;
#39482 = EDGE_CURVE ( 'NONE', #6061, #47426, #9232, .T. ) ;
#39483 = ORIENTED_EDGE ( 'NONE', *, *, #6109, .T. ) ;
#39484 = CARTESIAN_POINT ( 'NONE',  ( 97.30629616937498838, -209.9999999999999716, 82.49906250086715431 ) ) ;
#39485 = VECTOR ( 'NONE', #63297, 1000.000000000000000 ) ;
#39486 = VECTOR ( 'NONE', #68831, 1000.000000000000114 ) ;
#39487 = EDGE_LOOP ( 'NONE', ( #60784, #25140, #29372, #63448 ) ) ;
#39488 = CYLINDRICAL_SURFACE ( 'NONE', #13075, 37.49900000000000233 ) ;
#39489 = VERTEX_POINT ( 'NONE', #65651 ) ;
#39490 = ORIENTED_EDGE ( 'NONE', *, *, #72396, .F. ) ;
#39491 = CARTESIAN_POINT ( 'NONE',  ( 15.00000000000000000, 16.83928648764922542, -16.46020748918050458 ) ) ;
#39492 = AXIS2_PLACEMENT_3D ( 'NONE', #65749, #21342, #31896 ) ;
#39493 = CARTESIAN_POINT ( 'NONE',  ( 11.99999999999999822, -44.88180994100419952, 63.18004540533013369 ) ) ;
#39494 = ORIENTED_EDGE ( 'NONE', *, *, #27227, .F. ) ;
#39495 = DIRECTION ( 'NONE',  ( 0.000000000000000000, -0.9876883405951394357, 0.1564344650402205716 ) ) ;
#39496 = CARTESIAN_POINT ( 'NONE',  ( 12.50000000000000000, -107.5000000000000000, 2.500000000000000000 ) ) ;
#39497 = AXIS2_PLACEMENT_3D ( 'NONE', #73370, #15875, #38803 ) ;
#39498 = EDGE_CURVE ( 'NONE', #14250, #10456, #64828, .T. ) ;
#39499 = ORIENTED_EDGE ( 'NONE', *, *, #25537, .T. ) ;
#39500 = FACE_OUTER_BOUND ( 'NONE', #1417, .T. ) ;
#39501 = EDGE_CURVE ( 'NONE', #15332, #9804, #49088, .T. ) ;
#39502 = VERTEX_POINT ( 'NONE', #3626 ) ;
#39503 = VECTOR ( 'NONE', #39662, 1000.000000000000000 ) ;
#39504 = CARTESIAN_POINT ( 'NONE',  ( 0.000000000000000000, 71.21200624218852226, -40.65526001592539984 ) ) ;
#39505 = EDGE_CURVE ( 'NONE', #72748, #8336, #1002, .T. ) ;
#39506 = ORIENTED_EDGE ( 'NONE', *, *, #73396, .T. ) ;
#39507 = VERTEX_POINT ( 'NONE', #49458 ) ;
#39508 = ORIENTED_EDGE ( 'NONE', *, *, #65216, .F. ) ;
#39509 = CARTESIAN_POINT ( 'NONE',  ( 97.30629616937498838, -211.3315407142195852, 75.93739583420047268 ) ) ;
#39510 = DIRECTION ( 'NONE',  ( -1.000000000000000000, -0.000000000000000000, -0.000000000000000000 ) ) ;
#39511 = EDGE_LOOP ( 'NONE', ( #18403, #7944, #55378, #66455 ) ) ;
#39512 = ORIENTED_EDGE ( 'NONE', *, *, #70463, .T. ) ;
#39513 = ORIENTED_EDGE ( 'NONE', *, *, #20287, .F. ) ;
#39514 = LINE ( 'NONE', #62457, #42123 ) ;
#39515 = CARTESIAN_POINT ( 'NONE',  ( 0.000000000000000000, 0.000000000000000000, 0.000000000000000000 ) ) ;
#39516 = CARTESIAN_POINT ( 'NONE',  ( -96.15314808468752972, 91.99731107132950569, 76.99572916753382401 ) ) ;
#39517 = VERTEX_POINT ( 'NONE', #60754 ) ;
#39518 = LINE ( 'NONE', #63565, #70688 ) ;
#39519 = ORIENTED_EDGE ( 'NONE', *, *, #42313, .T. ) ;
#39520 = CARTESIAN_POINT ( 'NONE',  ( 97.65000000000006253, 91.52997821335249284, 75.13041666666666174 ) ) ;
#39521 = CARTESIAN_POINT ( 'NONE',  ( -93.84685191531247028, -211.9973110713294489, 84.77447916753381207 ) ) ;
#39522 = ORIENTED_EDGE ( 'NONE', *, *, #70440, .T. ) ;
#39523 = CARTESIAN_POINT ( 'NONE',  ( 2.260257450329328233, -4.468542444510769762, -0.5197061503823295903 ) ) ;
#39524 = DIRECTION ( 'NONE',  ( 0.000000000000000000, 0.1564344650402242631, 0.9876883405951387696 ) ) ;
#39525 = FACE_OUTER_BOUND ( 'NONE', #6290, .T. ) ;
#39526 = CARTESIAN_POINT ( 'NONE',  ( -97.30629616937497417, -208.6684592857803295, 78.79489583420047438 ) ) ;
#39527 = CIRCLE ( 'NONE', #17885, 2.650000000000540812 ) ;
#39528 = DIRECTION ( 'NONE',  ( -0.000000000000000000, -0.000000000000000000, 1.000000000000000000 ) ) ;
#39529 = DIRECTION ( 'NONE',  ( 1.000000000000000000, -0.000000000000000000, -0.000000000000000000 ) ) ;
#39530 = DIRECTION ( 'NONE',  ( 0.000000000000000000, 0.000000000000000000, 1.000000000000000000 ) ) ;
#39531 = VECTOR ( 'NONE', #13094, 1000.000000000000000 ) ;
#39532 = DIRECTION ( 'NONE',  ( -1.000000000000000000, 0.000000000000000000, 0.000000000000000000 ) ) ;
#39533 = CARTESIAN_POINT ( 'NONE',  ( 92.34999999999999432, 90.00000000000002842, 79.83999999999998920 ) ) ;
#39534 = CARTESIAN_POINT ( 'NONE',  ( -95.00000000000002842, 92.66308142843932671, 83.13406250086714522 ) ) ;
#39535 = FACE_OUTER_BOUND ( 'NONE', #64436, .T. ) ;
#39536 = CARTESIAN_POINT ( 'NONE',  ( 0.000000000000000000, 32.34446384429971033, 26.79245525562726371 ) ) ;
#39537 = ORIENTED_EDGE ( 'NONE', *, *, #32557, .F. ) ;
#39538 = VECTOR ( 'NONE', #3677, 1000.000000000000000 ) ;
#39539 = EDGE_CURVE ( 'NONE', #1166, #66590, #70902, .T. ) ;
#39540 = DIRECTION ( 'NONE',  ( 0.000000000000000000, 0.4067366430758017626, -0.9135454576426003115 ) ) ;
#39542 = DIRECTION ( 'NONE',  ( 0.000000000000000000, 0.000000000000000000, -1.000000000000000000 ) ) ;
#39541 = VECTOR ( 'NONE', #65089, 1000.000000000000000 ) ;
#39543 = AXIS2_PLACEMENT_3D ( 'NONE', #21729, #6314, #73229 ) ;
#39544 = CARTESIAN_POINT ( 'NONE',  ( 11.99999999999999822, 36.72794159290241822, 65.59268652807223532 ) ) ;
#39545 = CARTESIAN_POINT ( 'NONE',  ( -0.3487148583350038744, 5.572172074566123179, -1.686035282245269995 ) ) ;
#39546 = DIRECTION ( 'NONE',  ( -1.000000000000000000, -0.000000000000000000, -0.000000000000000000 ) ) ;
#39547 = CARTESIAN_POINT ( 'NONE',  ( -97.30629616937497417, -211.3315407142195852, 80.32947916753381890 ) ) ;
#39548 = ADVANCED_FACE ( 'NONE', ( #37460 ), #54004, .F. ) ;
#39549 = CIRCLE ( 'NONE', #7127, 11.59999999999999787 ) ;
#39550 = EDGE_CURVE ( 'NONE', #17922, #28278, #42867, .T. ) ;
#39551 = LINE ( 'NONE', #5350, #45294 ) ;
#39552 = ORIENTED_EDGE ( 'NONE', *, *, #27780, .T. ) ;
#39553 = DIRECTION ( 'NONE',  ( -0.000000000000000000, -0.000000000000000000, 1.000000000000000000 ) ) ;
#39554 = CARTESIAN_POINT ( 'NONE',  ( 10.00000000000000000, -81.90746397400391743, 3.894527615417593847 ) ) ;
#39555 = DIRECTION ( 'NONE',  ( 2.603472992746261562E-14, 2.546204323184492723E-14, -1.000000000000000000 ) ) ;
#39556 = EDGE_CURVE ( 'NONE', #49804, #26693, #10546, .T. ) ;
#39557 = DIRECTION ( 'NONE',  ( 1.000000000000000000, -0.000000000000000000, -0.000000000000000000 ) ) ;
#39558 = CARTESIAN_POINT ( 'NONE',  ( 94.99999999999998579, 90.00000000000002842, 90.00000000000000000 ) ) ;
#39559 = CARTESIAN_POINT ( 'NONE',  ( 97.64999999999999147, 90.00000000000002842, 90.00000000000000000 ) ) ;
#39560 = ORIENTED_EDGE ( 'NONE', *, *, #61277, .F. ) ;
#39561 = DIRECTION ( 'NONE',  ( 0.000000000000000000, 0.4539904997395478037, -0.8910065241883673437 ) ) ;
#39562 = DIRECTION ( 'NONE',  ( 1.000000000000000000, -0.000000000000000000, 0.000000000000000000 ) ) ;
#39563 = ORIENTED_EDGE ( 'NONE', *, *, #35904, .F. ) ;
#39564 =( BOUNDED_CURVE ( )  B_SPLINE_CURVE ( 2, ( #38040, #21474, #49675, #44439, #21859, #72599, #38787 ),
 .UNSPECIFIED., .F., .F. ) 
 B_SPLINE_CURVE_WITH_KNOTS ( ( 3, 2, 2, 3 ),
 ( 0.06249999999999966693, 0.06944444444444407283, 0.07638888888888849260, 0.08333333333333288462 ),
 .UNSPECIFIED. ) 
 CURVE ( )  GEOMETRIC_REPRESENTATION_ITEM ( )  RATIONAL_B_SPLINE_CURVE ( ( 1.000000000000006439, 0.8660254037844322683, 1.000000000000000000, 0.8660254037844387076, 1.000000000000000000, 0.8660254037844472563, 0.9999999999999914513 ) ) 
 REPRESENTATION_ITEM ( '' )  );
#39565 = CARTESIAN_POINT ( 'NONE',  ( 97.30629616937498838, -208.6684592857803295, 88.10822916753380696 ) ) ;
#39566 = DIRECTION ( 'NONE',  ( 0.000000000000000000, 0.000000000000000000, 1.000000000000000000 ) ) ;
#39567 = EDGE_CURVE ( 'NONE', #42672, #1062, #31051, .T. ) ;
#39568 = ORIENTED_EDGE ( 'NONE', *, *, #52786, .F. ) ;
#39569 = VECTOR ( 'NONE', #19469, 1000.000000000000114 ) ;
#39570 = DIRECTION ( 'NONE',  ( 0.000000000000000000, 0.5877852522924689183, -0.8090169943749504489 ) ) ;
#39571 = CIRCLE ( 'NONE', #59985, 31.99999999999998579 ) ;
#39572 = ORIENTED_EDGE ( 'NONE', *, *, #22263, .F. ) ;
#39573 = ORIENTED_EDGE ( 'NONE', *, *, #58384, .F. ) ;
#39574 = CARTESIAN_POINT ( 'NONE',  ( -94.99999999999997158, -213.0599564267049857, 80.07812500173429271 ) ) ;
#39575 = ORIENTED_EDGE ( 'NONE', *, *, #16539, .T. ) ;
#39576 = EDGE_LOOP ( 'NONE', ( #36318, #21835, #24364, #66760 ) ) ;
#39577 = VECTOR ( 'NONE', #63427, 1000.000000000000000 ) ;
#39578 = ORIENTED_EDGE ( 'NONE', *, *, #6732, .T. ) ;
#39579 = FACE_OUTER_BOUND ( 'NONE', #28186, .T. ) ;
#39580 = ADVANCED_FACE ( 'NONE', ( #36698 ), #25428, .T. ) ;
#39581 = ORIENTED_EDGE ( 'NONE', *, *, #46269, .T. ) ;
#39582 = ADVANCED_FACE ( 'NONE', ( #59639 ), #48350, .T. ) ;
#39583 = EDGE_LOOP ( 'NONE', ( #60868, #34894, #28110, #30622 ) ) ;
#39584 = CARTESIAN_POINT ( 'NONE',  ( 96.32499999999997442, 92.29496732002878900, 88.51833333333333087 ) ) ;
#39585 = CARTESIAN_POINT ( 'NONE',  ( -95.00000000000002842, 90.00000000000004263, 90.00000000000000000 ) ) ;
#39586 = DIRECTION ( 'NONE',  ( -0.8660254037844382635, -0.5000000000000006661, 0.000000000000000000 ) ) ;
#39587 = VERTEX_POINT ( 'NONE', #60025 ) ;
#39589 = ORIENTED_EDGE ( 'NONE', *, *, #27391, .F. ) ;
#39588 = CIRCLE ( 'NONE', #26376, 16.00000000000000000 ) ;
#39590 = ORIENTED_EDGE ( 'NONE', *, *, #36589, .T. ) ;
#39591 = CARTESIAN_POINT ( 'NONE',  ( 97.30629616937498838, 90.00000000000002842, 86.78531250086714977 ) ) ;
#39592 = ORIENTED_EDGE ( 'NONE', *, *, #9583, .F. ) ;
#39593 = CARTESIAN_POINT ( 'NONE',  ( 92.69370383062501162, -208.6684592857803011, 85.14489583420048291 ) ) ;
#39594 = AXIS2_PLACEMENT_3D ( 'NONE', #43852, #55489, #66767 ) ;
#39595 = AXIS2_PLACEMENT_3D ( 'NONE', #68283, #45357, #57364 ) ;
#39596 = APPLICATION_PROTOCOL_DEFINITION ( 'draft international standard', 'automotive_design', 1998, #39750 ) ;
#39597 = DIRECTION ( 'NONE',  ( 0.000000000000000000, 0.000000000000000000, 1.000000000000000000 ) ) ;
#39598 = CARTESIAN_POINT ( 'NONE',  ( 95.00000000000000000, -209.9999999999999716, 90.00000000000000000 ) ) ;
#39599 = CARTESIAN_POINT ( 'NONE',  ( -25.50183398199384754, -112.6408924756582053, 5.500000000000000000 ) ) ;
#39600 = CYLINDRICAL_SURFACE ( 'NONE', #13958, 37.49900000000000233 ) ;
#39601 = DIRECTION ( 'NONE',  ( -2.628368902995175337E-16, -1.000000000000000000, 0.000000000000000000 ) ) ;
#39602 = CIRCLE ( 'NONE', #25156, 0.2999999999999999334 ) ;
#39603 = DIRECTION ( 'NONE',  ( 0.000000000000000000, 0.000000000000000000, 1.000000000000000000 ) ) ;
#39604 = CIRCLE ( 'NONE', #13186, 16.00000000000000355 ) ;
#39605 = CARTESIAN_POINT ( 'NONE',  ( -97.30629616937495996, -209.9999999999999716, 89.00781250086714635 ) ) ;
#39606 = CARTESIAN_POINT ( 'NONE',  ( -96.15314808468752972, 91.99731107132950569, 86.52072916753382970 ) ) ;
#39607 = ORIENTED_EDGE ( 'NONE', *, *, #30736, .F. ) ;
#39609 = CARTESIAN_POINT ( 'NONE',  ( -93.84685191531254134, 91.99731107132950569, 84.35114583420048007 ) ) ;
#39608 = CARTESIAN_POINT ( 'NONE',  ( 92.69370383062498320, 90.00000000000002842, 85.19781250086714408 ) ) ;
#39610 = ORIENTED_EDGE ( 'NONE', *, *, #18591, .F. ) ;
#39611 = DIRECTION ( 'NONE',  ( 0.000000000000000000, 0.000000000000000000, 1.000000000000000000 ) ) ;
#39612 = CARTESIAN_POINT ( 'NONE',  ( 10.00000000000000000, 59.75363087400152295, -56.15606465354897381 ) ) ;
#39613 = CARTESIAN_POINT ( 'NONE',  ( 10.00000000000000000, -40.98264845739743834, -9.188173127307738497 ) ) ;
#39614 = CARTESIAN_POINT ( 'NONE',  ( 96.32499999999997442, 92.29496732002878900, 87.24833333333333485 ) ) ;
#39615 = CARTESIAN_POINT ( 'NONE',  ( -94.99999999999997158, -212.6630814284392557, 89.16656250086712987 ) ) ;
#39616 = DIRECTION ( 'NONE',  ( -0.000000000000000000, -0.000000000000000000, 1.000000000000000000 ) ) ;
#39617 = DIRECTION ( 'NONE',  ( 1.000000000000000000, 0.000000000000000000, 0.000000000000000000 ) ) ;
#39618 = FACE_OUTER_BOUND ( 'NONE', #20433, .T. ) ;
#39619 = CARTESIAN_POINT ( 'NONE',  ( 10.00000000000000000, -8.830959090342926032, 74.65491531819115778 ) ) ;
#39620 = ORIENTED_EDGE ( 'NONE', *, *, #315, .F. ) ;
#39621 = VERTEX_POINT ( 'NONE', #9974 ) ;
#39622 = CARTESIAN_POINT ( 'NONE',  ( -95.00000000000002842, 86.94004357329504273, 78.72875000000001933 ) ) ;
#39623 = DIRECTION ( 'NONE',  ( -1.000000000000000000, 0.000000000000000000, 0.000000000000000000 ) ) ;
#39624 = CARTESIAN_POINT ( 'NONE',  ( -92.35000000000003695, 90.00000000000004263, 78.88750000000000284 ) ) ;
#39625 = FACE_OUTER_BOUND ( 'NONE', #40808, .T. ) ;
#39626 = DIRECTION ( 'NONE',  ( 0.000000000000000000, 0.000000000000000000, 1.000000000000000000 ) ) ;
#39627 = CARTESIAN_POINT ( 'NONE',  ( 94.99999999999998579, 93.05995642670504253, 87.38062500173430180 ) ) ;
#39628 = ADVANCED_FACE ( 'NONE', ( #41067 ), #10349, .F. ) ;
#39629 = DIRECTION ( 'NONE',  ( -1.000000000000000000, -0.000000000000000000, -0.000000000000000000 ) ) ;
#39630 = DIRECTION ( 'NONE',  ( 0.000000000000000000, 0.000000000000000000, -1.000000000000000000 ) ) ;
#39631 = AXIS2_PLACEMENT_3D ( 'NONE', #71255, #65644, #45599 ) ;
#39632 = ORIENTED_EDGE ( 'NONE', *, *, #32306, .F. ) ;
#39633 = CARTESIAN_POINT ( 'NONE',  ( -92.69370383062502583, 88.66845928578038638, 77.20739583420046870 ) ) ;
#39634 = VECTOR ( 'NONE', #35892, 1000.000000000000000 ) ;
#39635 = EDGE_CURVE ( 'NONE', #35752, #50947, #72939, .T. ) ;
#39637 = CARTESIAN_POINT ( 'NONE',  ( 11.99999999999999822, -74.74816331893454446, 33.71516098798715433 ) ) ;
#39636 = AXIS2_PLACEMENT_3D ( 'NONE', #34346, #16695, #68578 ) ;
#39638 = DIRECTION ( 'NONE',  ( 1.000000000000000000, 0.000000000000000000, 0.000000000000000000 ) ) ;
#39639 = EDGE_CURVE ( 'NONE', #52892, #21663, #40561, .T. ) ;
#39640 = CARTESIAN_POINT ( 'NONE',  ( 0.000000000000000000, -21.60688246758642705, 79.10210256391358996 ) ) ;
#39641 = DIRECTION ( 'NONE',  ( -0.6575728627325955200, 0.7533909544171996098, 1.230411769795008318E-16 ) ) ;
#39642 = AXIS2_PLACEMENT_3D ( 'NONE', #25554, #42857, #12788 ) ;
#39643 = CARTESIAN_POINT ( 'NONE',  ( -2.500000000000000000, 16.00000000000000000, -10.00000000000000178 ) ) ;
#39644 = CARTESIAN_POINT ( 'NONE',  ( -96.15314808468747287, -208.0026889286704943, 88.42572916753381662 ) ) ;
#39645 = EDGE_CURVE ( 'NONE', #26369, #28467, #14131, .T. ) ;
#39646 = CARTESIAN_POINT ( 'NONE',  ( 93.84685191531248449, 91.99731107132950569, 78.26572916753382003 ) ) ;
#39647 = CARTESIAN_POINT ( 'NONE',  ( -97.30629616937497417, -211.3315407142195852, 79.69447916753381378 ) ) ;
#39648 = CARTESIAN_POINT ( 'NONE',  ( -3.000000000000000000, -23.29833615347104825, -3.418703333116803744 ) ) ;
#39649 = AXIS2_PLACEMENT_3D ( 'NONE', #17972, #7436, #7796 ) ;
#39650 = ORIENTED_EDGE ( 'NONE', *, *, #48541, .T. ) ;
#39651 = ADVANCED_FACE ( 'NONE', ( #11098 ), #27642, .F. ) ;
#39652 = CARTESIAN_POINT ( 'NONE',  ( -92.35000000000003695, 90.00000000000004263, 87.22187500173430408 ) ) ;
#39653 = CARTESIAN_POINT ( 'NONE',  ( -95.84368202074679743, -214.6948328857849049, 74.84535815546854565 ) ) ;
#39654 = DIRECTION ( 'NONE',  ( 0.000000000000000000, 0.9723699203976756689, 0.2334453638559095268 ) ) ;
#39655 = CIRCLE ( 'NONE', #32432, 31.99999999999998579 ) ;
#39656 = AXIS2_PLACEMENT_3D ( 'NONE', #66347, #14820, #15933 ) ;
#39657 = CIRCLE ( 'NONE', #52857, 77.49899999999999523 ) ;
#39658 = VECTOR ( 'NONE', #51572, 1000.000000000000000 ) ;
#39659 = CARTESIAN_POINT ( 'NONE',  ( -95.00000000000002842, 87.33691857156074434, 77.26031250086714408 ) ) ;
#39660 = CARTESIAN_POINT ( 'NONE',  ( 92.69370383062501162, -209.9999999999999716, 78.84781250086714977 ) ) ;
#39661 = VERTEX_POINT ( 'NONE', #33650 ) ;
#39662 = DIRECTION ( 'NONE',  ( -1.000000000000000000, -0.000000000000000000, 0.000000000000000000 ) ) ;
#39663 = ADVANCED_FACE ( 'NONE', ( #73122 ), #45322, .F. ) ;
#39664 = EDGE_LOOP ( 'NONE', ( #2232, #4112, #4743 ) ) ;
#39665 = DIRECTION ( 'NONE',  ( 0.4796670183876317051, -0.8774505977381972244, 0.000000000000000000 ) ) ;
#39666 = EDGE_CURVE ( 'NONE', #53610, #38273, #68247, .T. ) ;
#39667 = ORIENTED_EDGE ( 'NONE', *, *, #64343, .F. ) ;
#39668 = AXIS2_PLACEMENT_3D ( 'NONE', #36026, #13462, #12352 ) ;
#39669 = CARTESIAN_POINT ( 'NONE',  ( 11.99999999999999822, 49.70050353004975818, -59.46389618801909904 ) ) ;
#39670 = ADVANCED_FACE ( 'NONE', ( #22003 ), #48967, .F. ) ;
#39671 = VERTEX_POINT ( 'NONE', #16362 ) ;
#39672 = ORIENTED_EDGE ( 'NONE', *, *, #52217, .T. ) ;
#39673 = ORIENTED_EDGE ( 'NONE', *, *, #9187, .T. ) ;
#39674 = CARTESIAN_POINT ( 'NONE',  ( 97.30629616937498838, -209.9999999999999716, 74.87906250086714977 ) ) ;
#39675 = EDGE_CURVE ( 'NONE', #40375, #22108, #50186, .T. ) ;
#39676 = ORIENTED_EDGE ( 'NONE', *, *, #61197, .T. ) ;
#39677 = CYLINDRICAL_SURFACE ( 'NONE', #5256, 31.99999999999999289 ) ;
#39678 = CYLINDRICAL_SURFACE ( 'NONE', #19642, 31.99999999999998579 ) ;
#39679 = CARTESIAN_POINT ( 'NONE',  ( 97.30629616937498838, 90.00000000000002842, 84.40406250086715545 ) ) ;
#39680 = DIRECTION ( 'NONE',  ( 1.000000000000000000, 0.000000000000000000, 0.000000000000000000 ) ) ;
#39681 = CARTESIAN_POINT ( 'NONE',  ( 92.35000000000000853, -209.9999999999999716, 79.20499999999999829 ) ) ;
#39682 = EDGE_LOOP ( 'NONE', ( #65182, #18470, #22379, #43599 ) ) ;
#39683 = EDGE_CURVE ( 'NONE', #30034, #71014, #50567, .T. ) ;
#39684 = ORIENTED_EDGE ( 'NONE', *, *, #35237, .T. ) ;
#39685 = CIRCLE ( 'NONE', #62502, 77.49900000000000944 ) ;
#39686 = VERTEX_POINT ( 'NONE', #16744 ) ;
#39687 = ORIENTED_EDGE ( 'NONE', *, *, #44035, .T. ) ;
#39688 = FILL_AREA_STYLE ('',( #9981 ) ) ;
#39689 = VECTOR ( 'NONE', #63050, 1000.000000000000000 ) ;
#39690 = SURFACE_STYLE_FILL_AREA ( #67879 ) ;
#39691 = CARTESIAN_POINT ( 'NONE',  ( 10.00000000000000000, -37.16516213103273714, -4.992566952385376844 ) ) ;
#39692 = LINE ( 'NONE', #56614, #11033 ) ;
#39693 = CIRCLE ( 'NONE', #16717, 77.49900000000000944 ) ;
#39694 = DIRECTION ( 'NONE',  ( -0.9730327541852497042, 0.2306669878475623159, 0.000000000000000000 ) ) ;
#39695 = DIRECTION ( 'NONE',  ( -1.000000000000000000, -0.000000000000000000, -0.000000000000000000 ) ) ;
#39696 = DIRECTION ( 'NONE',  ( 0.000000000000000000, -0.3090169943749349613, -0.9510565162951576390 ) ) ;
#39697 = EDGE_LOOP ( 'NONE', ( #48066, #60689, #1549, #21986 ) ) ;
#39698 = CARTESIAN_POINT ( 'NONE',  ( -97.64999999999994884, -208.4700217866474645, 81.13645833506764404 ) ) ;
#39699 = ORIENTED_EDGE ( 'NONE', *, *, #8159, .T. ) ;
#39700 = FACE_OUTER_BOUND ( 'NONE', #23146, .T. ) ;
#39701 = ORIENTED_EDGE ( 'NONE', *, *, #29611, .F. ) ;
#39703 = CARTESIAN_POINT ( 'NONE',  ( -92.35000000000005116, 88.47002178664754979, 80.81895833506764859 ) ) ;
#39702 = CARTESIAN_POINT ( 'NONE',  ( 94.99999999999998579, 86.94004357329500010, 80.07812500173432113 ) ) ;
#39704 = ORIENTED_EDGE ( 'NONE', *, *, #12166, .F. ) ;
#39705 = CARTESIAN_POINT ( 'NONE',  ( 92.69370383062498320, 88.66845928578037217, 84.77447916753381207 ) ) ;
#39706 = CYLINDRICAL_SURFACE ( 'NONE', #66192, 2.649999999999985700 ) ;
#39707 = LINE ( 'NONE', #34049, #51105 ) ;
#39708 = CARTESIAN_POINT ( 'NONE',  ( -10.00000000000000000, 0.000000000000000000, 0.000000000000000000 ) ) ;
#39709 = AXIS2_PLACEMENT_3D ( 'NONE', #37681, #4218, #62093 ) ;
#39710 = DIRECTION ( 'NONE',  ( -1.000000000000000000, 0.000000000000000000, -0.000000000000000000 ) ) ;
#39711 = VERTEX_POINT ( 'NONE', #6487 ) ;
#39712 = DIRECTION ( 'NONE',  ( -1.000000000000000000, -0.000000000000000000, 0.000000000000000000 ) ) ;
#39713 = CARTESIAN_POINT ( 'NONE',  ( -92.35000000002600018, 89.99998827382285072, 82.77687459617033028 ) ) ;
#39714 = AXIS2_PLACEMENT_3D ( 'NONE', #74076, #11297, #34231 ) ;
#39715 = ORIENTED_EDGE ( 'NONE', *, *, #46412, .T. ) ;
#39716 = AXIS2_PLACEMENT_3D ( 'NONE', #42472, #48835, #48105 ) ;
#39717 = VERTEX_POINT ( 'NONE', #52329 ) ;
#39718 = VECTOR ( 'NONE', #12908, 1000.000000000000000 ) ;
#39719 = CYLINDRICAL_SURFACE ( 'NONE', #41983, 17.50000000000000355 ) ;
#39720 = CARTESIAN_POINT ( 'NONE',  ( -92.35000000000177067, -209.9999969335172807, 75.79187510780353421 ) ) ;
#39721 = CARTESIAN_POINT ( 'NONE',  ( 0.000000000000000000, 0.000000000000000000, 0.000000000000000000 ) ) ;
#39722 = CARTESIAN_POINT ( 'NONE',  ( 10.00000000000000000, 0.000000000000000000, 0.000000000000000000 ) ) ;
#39723 = CARTESIAN_POINT ( 'NONE',  ( -92.69370383062498320, -208.6684592857803011, 82.55197916753382970 ) ) ;
#39724 = VERTEX_POINT ( 'NONE', #72742 ) ;
#39725 = CARTESIAN_POINT ( 'NONE',  ( -93.84685191531254134, 91.99731107132950569, 88.79614583420047325 ) ) ;
#39726 = VERTEX_POINT ( 'NONE', #33264 ) ;
#39727 = EDGE_CURVE ( 'NONE', #16833, #3451, #74248, .T. ) ;
#39728 = CARTESIAN_POINT ( 'NONE',  ( 95.00000000000000000, -209.9999999999999716, 90.00000000000000000 ) ) ;
#39729 = CARTESIAN_POINT ( 'NONE',  ( 0.000000000000000000, 0.000000000000000000, 40.00000000000000000 ) ) ;
#39730 = EDGE_CURVE ( 'NONE', #8961, #8129, #71163, .T. ) ;
#39731 = CARTESIAN_POINT ( 'NONE',  ( 5.000000000000002665, 68.55367621811205936, -44.99326035065983120 ) ) ;
#39732 = CARTESIAN_POINT ( 'NONE',  ( 10.00000000000000000, -68.27212725128298132, 31.46837873494953541 ) ) ;
#39733 = CARTESIAN_POINT ( 'NONE',  ( 10.00000000000000000, -21.53537804866058991, -30.80686688397033635 ) ) ;
#39734 = CARTESIAN_POINT ( 'NONE',  ( 15.00000000000000000, -11.95096189432312350, 23.69967320028773372 ) ) ;
#39735 = CARTESIAN_POINT ( 'NONE',  ( -92.34999999999999432, -209.9999999999999716, 78.88750000000000284 ) ) ;
#39736 = CARTESIAN_POINT ( 'NONE',  ( -3.000000000000000000, 0.000000000000000000, 0.000000000000000000 ) ) ;
#39737 = EDGE_CURVE ( 'NONE', #66290, #16867, #61496, .T. ) ;
#39739 = EDGE_CURVE ( 'NONE', #44128, #44780, #9415, .T. ) ;
#39738 = DIRECTION ( 'NONE',  ( -0.000000000000000000, -0.000000000000000000, -1.000000000000000000 ) ) ;
#39740 = DIRECTION ( 'NONE',  ( 0.000000000000000000, -0.8090169943749532244, 0.5877852522924652545 ) ) ;
#39741 = CARTESIAN_POINT ( 'NONE',  ( 97.30629616937498838, 90.00000000000002842, 87.57906250086715261 ) ) ;
#39742 = DIRECTION ( 'NONE',  ( -1.000000000000000000, 0.000000000000000000, -0.000000000000000000 ) ) ;
#39743 = DIRECTION ( 'NONE',  ( 0.000000000000000000, 0.000000000000000000, 1.000000000000000000 ) ) ;
#39744 = ORIENTED_EDGE ( 'NONE', *, *, #35572, .F. ) ;
#39745 = VECTOR ( 'NONE', #30280, 1000.000000000000000 ) ;
#39746 = DIRECTION ( 'NONE',  ( -1.000000000000000000, 0.000000000000000000, 0.000000000000000000 ) ) ;
#39747 = CARTESIAN_POINT ( 'NONE',  ( -93.84685191531252713, 88.00268892867056536, 80.32947916753380468 ) ) ;
#39748 = ADVANCED_FACE ( 'NONE', ( #65112 ), #7585, .F. ) ;
#39749 = DIRECTION ( 'NONE',  ( -0.000000000000000000, 0.000000000000000000, 1.000000000000000000 ) ) ;
#39750 = APPLICATION_CONTEXT ( 'automotive_design' ) ;
#39751 = ORIENTED_EDGE ( 'NONE', *, *, #13756, .F. ) ;
#39752 = CARTESIAN_POINT ( 'NONE',  ( 50.00005079999999680, 0.000000000000000000, 0.000000000000000000 ) ) ;
#39753 = CARTESIAN_POINT ( 'NONE',  ( 92.34999999999990905, 88.47002178664756400, 83.06791666666666174 ) ) ;
#39754 = DIRECTION ( 'NONE',  ( -1.000000000000000000, 0.000000000000000000, -0.000000000000000000 ) ) ;
#39755 = AXIS2_PLACEMENT_3D ( 'NONE', #28039, #32928, #21660 ) ;
#39756 = CARTESIAN_POINT ( 'NONE',  ( 93.67500000000001137, -212.2949673200287179, 85.74020833506763495 ) ) ;
#39757 = ADVANCED_FACE ( 'NONE', ( #64367 ), #70341, .T. ) ;
#39758 = EDGE_CURVE ( 'NONE', #53775, #44963, #25252, .T. ) ;
#39759 = LINE ( 'NONE', #62708, #40562 ) ;
#39760 = AXIS2_PLACEMENT_3D ( 'NONE', #47287, #70190, #18696 ) ;
#39761 = VERTEX_POINT ( 'NONE', #19958 ) ;
#39762 = CIRCLE ( 'NONE', #2555, 42.00000000000000000 ) ;
#39763 = ORIENTED_EDGE ( 'NONE', *, *, #74325, .F. ) ;
#39764 = CARTESIAN_POINT ( 'NONE',  ( 0.000000000000000000, -120.0000000000000000, 125.0000000000000000 ) ) ;
#39765 = DIRECTION ( 'NONE',  ( 0.000000000000000000, -0.6494480483301903195, 0.7604059656000251577 ) ) ;
#39766 = DIRECTION ( 'NONE',  ( 1.000000000000000000, 0.000000000000000000, 0.000000000000000000 ) ) ;
#39767 = DIRECTION ( 'NONE',  ( 0.000000000000000000, 0.000000000000000000, 1.000000000000000000 ) ) ;
#39768 = LINE ( 'NONE', #62715, #58586 ) ;
#39769 = CARTESIAN_POINT ( 'NONE',  ( 92.35000000000000853, -209.9999999999999716, 89.36499999999999488 ) ) ;
#39770 = ORIENTED_EDGE ( 'NONE', *, *, #4268, .F. ) ;
#39771 = EDGE_LOOP ( 'NONE', ( #8778, #44496, #65486, #34038 ) ) ;
#39772 = DIRECTION ( 'NONE',  ( 1.000000000000000000, -0.000000000000000000, -0.000000000000000000 ) ) ;
#39773 = ORIENTED_EDGE ( 'NONE', *, *, #67756, .F. ) ;
#39774 = ORIENTED_EDGE ( 'NONE', *, *, #33078, .T. ) ;
#39775 = DIRECTION ( 'NONE',  ( 0.000000000000000000, 0.7071067811865439090, 0.7071067811865512365 ) ) ;
#39776 =( NAMED_UNIT ( * ) SI_UNIT ( $, .STERADIAN. ) SOLID_ANGLE_UNIT ( ) );
#39777 = CARTESIAN_POINT ( 'NONE',  ( 4.180704885107411783, 3.359771601077109260, -5.801655677627843843 ) ) ;
#39778 = CARTESIAN_POINT ( 'NONE',  ( -7.499999999999969802, 73.00000000000001421, -204.9999999999999716 ) ) ;
#39779 = CARTESIAN_POINT ( 'NONE',  ( 92.35000000000000853, -209.9999999999999716, 76.10937500173430692 ) ) ;
#39780 = CARTESIAN_POINT ( 'NONE',  ( 94.99999999999998579, 93.05995642670504253, 80.95125000000000171 ) ) ;
#39781 = VERTEX_POINT ( 'NONE', #30501 ) ;
#39782 = CARTESIAN_POINT ( 'NONE',  ( 92.35000000000000853, -210.0000123297515984, 75.47437542817786493 ) ) ;
#39783 = VERTEX_POINT ( 'NONE', #7945 ) ;
#39784 = FACE_OUTER_BOUND ( 'NONE', #34569, .T. ) ;
#39785 = EDGE_LOOP ( 'NONE', ( #36884, #18645, #6577, #29914 ) ) ;
#39786 = CARTESIAN_POINT ( 'NONE',  ( 94.99999999999998579, 86.94004357329502852, 84.52312500173428589 ) ) ;
#39787 = CARTESIAN_POINT ( 'NONE',  ( -92.69370383062505425, 88.66845928578038638, 81.81114583420048803 ) ) ;
#39788 = CARTESIAN_POINT ( 'NONE',  ( 92.69370383062498320, 88.66845928578037217, 76.99572916753380980 ) ) ;
#39789 = ORIENTED_EDGE ( 'NONE', *, *, #69141, .F. ) ;
#39790 = DIRECTION ( 'NONE',  ( -0.6516173805718079581, 0.7585478161175704948, 0.000000000000000000 ) ) ;
#39791 = CARTESIAN_POINT ( 'NONE',  ( 11.99999999999999822, 62.50884508063487033, -41.76106447765422303 ) ) ;
#39792 = FACE_OUTER_BOUND ( 'NONE', #33502, .T. ) ;
#39793 = CIRCLE ( 'NONE', #45816, 32.50000000000000000 ) ;
#39794 = VERTEX_POINT ( 'NONE', #37278 ) ;
#39795 = DIRECTION ( 'NONE',  ( -1.000000000000000000, 0.000000000000000000, -0.000000000000000000 ) ) ;
#39796 = CARTESIAN_POINT ( 'NONE',  ( -97.30629616937495996, -209.9999999999999716, 76.30781250086714351 ) ) ;
#39797 = ORIENTED_EDGE ( 'NONE', *, *, #57378, .F. ) ;
#39798 = VECTOR ( 'NONE', #30543, 1000.000000000000000 ) ;
#39799 = EDGE_LOOP ( 'NONE', ( #60866, #11262, #27152, #14540 ) ) ;
#39800 = CARTESIAN_POINT ( 'NONE',  ( -11.68233973192911535, 0.000000000000000000, 0.000000000000000000 ) ) ;
#39801 = AXIS2_PLACEMENT_3D ( 'NONE', #60780, #20165, #25076 ) ;
#39802 = VERTEX_POINT ( 'NONE', #18487 ) ;
#39803 = DIRECTION ( 'NONE',  ( 0.000000000000000000, 0.000000000000000000, 1.000000000000000000 ) ) ;
#39804 = LINE ( 'NONE', #16120, #37689 ) ;
#39805 = ORIENTED_EDGE ( 'NONE', *, *, #63941, .F. ) ;
#39806 =( BOUNDED_CURVE ( )  B_SPLINE_CURVE ( 2, ( #70251, #12017, #2260, #58618, #24408, #7123, #30040 ),
 .UNSPECIFIED., .F., .F. ) 
 B_SPLINE_CURVE_WITH_KNOTS ( ( 3, 2, 2, 3 ),
 ( 0.3749999999999998335, 0.3819444444444441977, 0.3888888888888886730, 0.3958333333333330373 ),
 .UNSPECIFIED. ) 
 CURVE ( )  GEOMETRIC_REPRESENTATION_ITEM ( )  RATIONAL_B_SPLINE_CURVE ( ( 1.000000000000003109, 0.8660254037844354880, 1.000000000000000000, 0.8660254037844387076, 1.000000000000000000, 0.8660254037844440367, 0.9999999999999946709 ) ) 
 REPRESENTATION_ITEM ( '' )  );
#39807 = CARTESIAN_POINT ( 'NONE',  ( -94.99999999999997158, -212.6630814284392557, 76.46656250086712703 ) ) ;
#39808 = VERTEX_POINT ( 'NONE', #36514 ) ;
#39809 = CARTESIAN_POINT ( 'NONE',  ( -92.34999999999999432, -209.9999999999999716, 81.42749999999999488 ) ) ;
#39810 = CARTESIAN_POINT ( 'NONE',  ( 4.999999999999999112, 2.663952781846732343, -41.91543099594814947 ) ) ;
#39811 = DIRECTION ( 'NONE',  ( 0.000000000000000000, -0.9969173337331287410, 0.07845909572783495156 ) ) ;
#39812 = CARTESIAN_POINT ( 'NONE',  ( 10.00000000000000000, 0.8828120875900632436, 37.48860685352291000 ) ) ;
#39813 = EDGE_CURVE ( 'NONE', #7419, #42721, #24871, .T. ) ;
#39814 = CARTESIAN_POINT ( 'NONE',  ( 11.99999999999999822, 0.000000000000000000, 0.000000000000000000 ) ) ;
#39815 = VECTOR ( 'NONE', #18516, 1000.000000000000114 ) ;
#39816 = CIRCLE ( 'NONE', #5052, 5.000000000000004441 ) ;
#39817 = EDGE_CURVE ( 'NONE', #19352, #46404, #7003, .T. ) ;
#39818 = CARTESIAN_POINT ( 'NONE',  ( 96.32499999999998863, -207.7050326799711968, 86.05770833506763040 ) ) ;
#39819 = CARTESIAN_POINT ( 'NONE',  ( 92.69370383062498320, 88.66845928578035796, 86.52072916753381548 ) ) ;
#39820 = CARTESIAN_POINT ( 'NONE',  ( -92.34999999999999432, -209.9999999999999716, 75.07749999999998636 ) ) ;
#39821 = VECTOR ( 'NONE', #26504, 1000.000000000000000 ) ;
#39822 = DIRECTION ( 'NONE',  ( -1.000000000000000000, -0.000000000000000000, -0.000000000000000000 ) ) ;
#39823 = DIRECTION ( 'NONE',  ( 0.000000000000000000, 0.9969173337331276308, 0.07845909572784864894 ) ) ;
#39824 = CARTESIAN_POINT ( 'NONE',  ( 96.66734480923264528, -212.0887925413173321, 75.00000000000000000 ) ) ;
#39826 = EDGE_CURVE ( 'NONE', #65198, #58172, #4619, .T. ) ;
#39825 = CARTESIAN_POINT ( 'NONE',  ( 5.822613034544236399, -142.8165987265839476, -2.500000000000000000 ) ) ;
#39827 = CARTESIAN_POINT ( 'NONE',  ( 0.000000000000000000, 0.000000000000000000, -1.199999999999999956 ) ) ;
#39828 = CARTESIAN_POINT ( 'NONE',  ( 11.99999999999999822, -55.38113227695820484, 54.21277698773656084 ) ) ;
#39829 = VECTOR ( 'NONE', #26312, 1000.000000000000000 ) ;
#39830 = CARTESIAN_POINT ( 'NONE',  ( 11.99999999999999822, -65.58780272294100655, 36.73666225445870737 ) ) ;
#39831 = EDGE_CURVE ( 'NONE', #52760, #60509, #41426, .T. ) ;
#39832 = CARTESIAN_POINT ( 'NONE',  ( 5.000000000000000000, 31.52238457039637609, -27.75498641678709788 ) ) ;
#39833 = DIRECTION ( 'NONE',  ( -0.000000000000000000, -0.000000000000000000, 1.000000000000000000 ) ) ;
#39834 = CARTESIAN_POINT ( 'NONE',  ( 5.000000000000000000, -55.16347631942998220, -60.67117009219196433 ) ) ;
#39835 = CARTESIAN_POINT ( 'NONE',  ( -95.00000000002617639, -209.9999999999999432, -74.99999999999349143 ) ) ;
#39836 = CARTESIAN_POINT ( 'NONE',  ( -92.34999999999999432, -211.5299782133524502, 83.27958333333333485 ) ) ;
#39837 = ADVANCED_FACE ( 'NONE', ( #8321 ), #2357, .F. ) ;
#39838 = CARTESIAN_POINT ( 'NONE',  ( -95.00000000000002842, 86.94004357329504273, 79.99874999999998693 ) ) ;
#39839 = EDGE_CURVE ( 'NONE', #54928, #61657, #5848, .T. ) ;
#39840 = PRODUCT_DEFINITION_SHAPE ( 'NONE', 'NONE',  #74380 ) ;
#39841 = VERTEX_POINT ( 'NONE', #24151 ) ;
#39842 = CARTESIAN_POINT ( 'NONE',  ( 0.000000000000000000, 0.000000000000000000, -44.99999999999998579 ) ) ;
#39843 = LINE ( 'NONE', #33058, #9514 ) ;
#39844 = DIRECTION ( 'NONE',  ( 0.000000000000000000, 0.000000000000000000, 1.000000000000000000 ) ) ;
#39845 =( GEOMETRIC_REPRESENTATION_CONTEXT ( 3 ) GLOBAL_UNCERTAINTY_ASSIGNED_CONTEXT ( ( #67759 ) ) GLOBAL_UNIT_ASSIGNED_CONTEXT ( ( #52252, #30053, #59381 ) ) REPRESENTATION_CONTEXT ( 'NONE', 'WORKASPACE' ) );
#39846 = AXIS2_PLACEMENT_3D ( 'NONE', #26280, #66880, #15369 ) ;
#39847 = ADVANCED_FACE ( 'NONE', ( #35769 ), #53811, .F. ) ;
#39848 = EDGE_CURVE ( 'NONE', #17509, #7975, #52625, .T. ) ;
#39849 = CARTESIAN_POINT ( 'NONE',  ( 92.69370383062501162, -209.9999999999999716, 86.62656250086715204 ) ) ;
#39850 = AXIS2_PLACEMENT_3D ( 'NONE', #59415, #41744, #20286 ) ;
#39851 = ORIENTED_EDGE ( 'NONE', *, *, #1060, .F. ) ;
#39852 = EDGE_LOOP ( 'NONE', ( #50302, #16697, #48795, #5584 ) ) ;
#39853 = AXIS2_PLACEMENT_3D ( 'NONE', #48486, #59403, #58659 ) ;
#39854 = DIRECTION ( 'NONE',  ( 0.4796670183876317051, -0.8774505977381971134, 0.000000000000000000 ) ) ;
#39855 = EDGE_LOOP ( 'NONE', ( #24671, #44064, #6347, #25809 ) ) ;
#39856 = DIRECTION ( 'NONE',  ( -1.000000000000000000, 0.000000000000000000, -0.000000000000000000 ) ) ;
#39857 = AXIS2_PLACEMENT_3D ( 'NONE', #50195, #39315, #16373 ) ;
#39858 = CARTESIAN_POINT ( 'NONE',  ( 92.69370383062501162, -211.3315407142195852, 77.63072916753380071 ) ) ;
#39859 = ORIENTED_EDGE ( 'NONE', *, *, #31480, .F. ) ;
#39860 = CARTESIAN_POINT ( 'NONE',  ( 97.30629616937498838, -209.9999999999999716, 81.86406250086714920 ) ) ;
#39861 = ORIENTED_EDGE ( 'NONE', *, *, #58852, .F. ) ;
#39862 = DIRECTION ( 'NONE',  ( -1.000000000000000000, -0.000000000000000000, -0.000000000000000000 ) ) ;
#39863 = ORIENTED_EDGE ( 'NONE', *, *, #25300, .F. ) ;
#39864 = VECTOR ( 'NONE', #2391, 1000.000000000000000 ) ;
#39865 = VERTEX_POINT ( 'NONE', #42179 ) ;
#39866 = UNCERTAINTY_MEASURE_WITH_UNIT (LENGTH_MEASURE( 1.000000000000000082E-05 ), #7166, 'distance_accuracy_value', 'NONE');
#39867 = CIRCLE ( 'NONE', #49451, 16.00000000000000000 ) ;
#39868 = DIRECTION ( 'NONE',  ( -1.000000000000000000, -0.000000000000000000, -0.000000000000000000 ) ) ;
#39869 = VECTOR ( 'NONE', #74216, 1000.000000000000000 ) ;
#39870 = ORIENTED_EDGE ( 'NONE', *, *, #9579, .T. ) ;
#39871 = CARTESIAN_POINT ( 'NONE',  ( 93.67500000000001137, -212.2949673200287179, 76.85020833506763438 ) ) ;
#39872 = CARTESIAN_POINT ( 'NONE',  ( 93.67500000000001137, -212.2949673200287179, 87.64520833506762187 ) ) ;
#39873 = ORIENTED_EDGE ( 'NONE', *, *, #55685, .T. ) ;
#39874 = DIRECTION ( 'NONE',  ( 0.000000000000000000, 0.000000000000000000, 1.000000000000000000 ) ) ;
#39875 = VERTEX_POINT ( 'NONE', #13583 ) ;
#39876 = CARTESIAN_POINT ( 'NONE',  ( -97.30629616937501680, 91.33154071421968467, 89.74864583420048803 ) ) ;
#39877 = ORIENTED_EDGE ( 'NONE', *, *, #11530, .T. ) ;
#39878 = ORIENTED_EDGE ( 'NONE', *, *, #26144, .F. ) ;
#39879 = ORIENTED_EDGE ( 'NONE', *, *, #47117, .F. ) ;
#39880 = CARTESIAN_POINT ( 'NONE',  ( 10.00000000000000000, 25.88420570971438650, -27.13269053701069566 ) ) ;
#39881 = DIRECTION ( 'NONE',  ( -1.000000000000000000, -0.000000000000000000, -0.000000000000000000 ) ) ;
#39882 = EDGE_LOOP ( 'NONE', ( #38214, #29730, #64523, #7200 ) ) ;
#39883 = ORIENTED_EDGE ( 'NONE', *, *, #10595, .T. ) ;
#39885 = EDGE_CURVE ( 'NONE', #37783, #72369, #62247, .T. ) ;
#39884 = ORIENTED_EDGE ( 'NONE', *, *, #36241, .T. ) ;
#39886 = CARTESIAN_POINT ( 'NONE',  ( 10.00000000000000000, 0.000000000000000000, 0.000000000000000000 ) ) ;
#39887 = DIRECTION ( 'NONE',  ( -1.000000000000000000, 0.000000000000000000, 0.000000000000000000 ) ) ;
#39888 = EDGE_CURVE ( 'NONE', #55524, #11001, #7218, .T. ) ;
#39889 = CARTESIAN_POINT ( 'NONE',  ( -97.30629616937501680, 90.00000000000004263, 77.10156250086714635 ) ) ;
#39890 = ORIENTED_EDGE ( 'NONE', *, *, #43330, .F. ) ;
#39891 = CARTESIAN_POINT ( 'NONE',  ( 92.69370383062498320, 90.00000000000002842, 89.80156250086714920 ) ) ;
#39892 = ADVANCED_FACE ( 'NONE', ( #25605 ), #48543, .T. ) ;
#39893 = ORIENTED_EDGE ( 'NONE', *, *, #14231, .T. ) ;
#39894 = FACE_OUTER_BOUND ( 'NONE', #50446, .T. ) ;
#39895 = CARTESIAN_POINT ( 'NONE',  ( -92.69370383062498320, -209.9999999999999716, 86.15031250086714465 ) ) ;
#39896 = EDGE_LOOP ( 'NONE', ( #5019, #62516, #31078, #37570 ) ) ;
#39897 = CARTESIAN_POINT ( 'NONE',  ( -93.07557990970633455, 88.17815826261617929, 75.00000000000001421 ) ) ;
#39898 = CARTESIAN_POINT ( 'NONE',  ( 0.000000000000000000, 0.000000000000000000, 0.000000000000000000 ) ) ;
#39899 = CYLINDRICAL_SURFACE ( 'NONE', #32105, 37.49900000000000233 ) ;
#39900 = CARTESIAN_POINT ( 'NONE',  ( -97.30629616937497417, -211.3315407142195852, 75.09072916753380866 ) ) ;
#39901 = EDGE_CURVE ( 'NONE', #36077, #46616, #27394, .T. ) ;
#39902 = STYLED_ITEM ( 'NONE', ( #56701 ), #4129 ) ;
#39903 = CIRCLE ( 'NONE', #59054, 31.99999999999998934 ) ;
#39904 = CARTESIAN_POINT ( 'NONE',  ( 0.000000000000000000, 0.000000000000000000, -145.0000000000000000 ) ) ;
#39905 = DIRECTION ( 'NONE',  ( -0.4796670183876317051, 0.8774505977381971134, 0.000000000000000000 ) ) ;
#39906 = VECTOR ( 'NONE', #63874, 1000.000000000000000 ) ;
#39907 = EDGE_CURVE ( 'NONE', #68386, #15222, #67692, .T. ) ;
#39908 = CARTESIAN_POINT ( 'NONE',  ( 6.000000000000000000, -10.30890764327323161, -81.34940948281348483 ) ) ;
#39909 = LINE ( 'NONE', #23354, #49551 ) ;
#39910 = CARTESIAN_POINT ( 'NONE',  ( 92.34999999999999432, 88.47002178664752137, 79.97229166840095615 ) ) ;
#39911 = VECTOR ( 'NONE', #44333, 1000.000000000000000 ) ;
#39912 = CARTESIAN_POINT ( 'NONE',  ( -92.69370383062502583, 88.66845928578038638, 81.01739583420048518 ) ) ;
#39913 = CYLINDRICAL_SURFACE ( 'NONE', #69467, 37.49900000000000233 ) ;
#39914 = CYLINDRICAL_SURFACE ( 'NONE', #73417, 16.00000000000000000 ) ;
#39915 = AXIS2_PLACEMENT_3D ( 'NONE', #41629, #42380, #64949 ) ;
#39916 = ADVANCED_FACE ( 'NONE', ( #66584 ), #27077, .T. ) ;
#39917 = ORIENTED_EDGE ( 'NONE', *, *, #53796, .T. ) ;
#39918 = DIRECTION ( 'NONE',  ( -1.000000000000000000, 0.000000000000000000, 0.000000000000000000 ) ) ;
#39919 = CIRCLE ( 'NONE', #31470, 42.00000000000000000 ) ;
#39920 = DIRECTION ( 'NONE',  ( 0.000000000000000000, 0.000000000000000000, 1.000000000000000000 ) ) ;
#39921 = CARTESIAN_POINT ( 'NONE',  ( -8.637688417678550223, 13.69818742750669749, -64.01812422950393966 ) ) ;
#39922 = LINE ( 'NONE', #6803, #50237 ) ;
#39923 = CARTESIAN_POINT ( 'NONE',  ( 0.000000000000000000, 73.73191006444551476, 14.66109333815590254 ) ) ;
#39924 = CARTESIAN_POINT ( 'NONE',  ( -96.32500000000001705, 92.29496732002878900, 85.52854166840096184 ) ) ;
#39925 = CARTESIAN_POINT ( 'NONE',  ( -94.99999999999997158, -207.3369185715606307, 80.75281250086715090 ) ) ;
#39926 = ADVANCED_FACE ( 'NONE', ( #27451 ), #26708, .F. ) ;
#39927 = DIRECTION ( 'NONE',  ( -1.000000000000000000, 0.000000000000000000, 0.000000000000000000 ) ) ;
#39928 = ADVANCED_FACE ( 'NONE', ( #60936 ), #8696, .F. ) ;
#39929 = VERTEX_POINT ( 'NONE', #72204 ) ;
#39930 = DIRECTION ( 'NONE',  ( -1.000000000000000000, 0.000000000000000000, 0.000000000000000000 ) ) ;
#39931 = CARTESIAN_POINT ( 'NONE',  ( -3.000000000000000000, -25.60904388321925396, 6.976881207771172377 ) ) ;
#39932 = CARTESIAN_POINT ( 'NONE',  ( 10.00000000000000000, 4.992566952385523393, -37.16516213103272293 ) ) ;
#39933 = CARTESIAN_POINT ( 'NONE',  ( 0.000000000000000000, 0.000000000000000000, -20.00000000000000000 ) ) ;
#39934 = CARTESIAN_POINT ( 'NONE',  ( 0.000000000000000000, 36.73666225445894185, 65.58780272294090707 ) ) ;
#39935 = ORIENTED_EDGE ( 'NONE', *, *, #13761, .T. ) ;
#39936 = FACE_OUTER_BOUND ( 'NONE', #12286, .T. ) ;
#39937 = CARTESIAN_POINT ( 'NONE',  ( -24.50849501662245800, -109.8101191361138831, 5.500000000000000000 ) ) ;
#39938 = ORIENTED_EDGE ( 'NONE', *, *, #19583, .T. ) ;
#39939 = CARTESIAN_POINT ( 'NONE',  ( 97.30629616937498838, -209.9999999999999716, 88.05531250086713158 ) ) ;
#39940 = DIRECTION ( 'NONE',  ( 0.000000000000000000, -0.9510565162951566398, 0.3090169943749381809 ) ) ;
#39941 = ORIENTED_EDGE ( 'NONE', *, *, #44736, .T. ) ;
#39942 = CARTESIAN_POINT ( 'NONE',  ( 97.65000000000000568, -211.5299782133524502, 89.62958333333334338 ) ) ;
#39943 = VERTEX_POINT ( 'NONE', #72566 ) ;
#39944 = DIRECTION ( 'NONE',  ( -1.000000000000000000, -0.000000000000000000, 0.000000000000000000 ) ) ;
#39945 = VERTEX_POINT ( 'NONE', #31609 ) ;
#39946 = CARTESIAN_POINT ( 'NONE',  ( -92.34999999999999432, -211.5299782133524218, 80.18395833506764347 ) ) ;
#39947 = VECTOR ( 'NONE', #40799, 1000.000000000000227 ) ;
#39948 = ORIENTED_EDGE ( 'NONE', *, *, #60609, .F. ) ;
#39949 = DIRECTION ( 'NONE',  ( -1.000000000000000000, -0.000000000000000000, 0.000000000000000000 ) ) ;
#39950 = ORIENTED_EDGE ( 'NONE', *, *, #2151, .F. ) ;
#39951 = ORIENTED_EDGE ( 'NONE', *, *, #64526, .T. ) ;
#39952 = CARTESIAN_POINT ( 'NONE',  ( 11.99999999999999822, -58.39081064771713869, -50.95692526931392052 ) ) ;
#39953 = EDGE_CURVE ( 'NONE', #50675, #6695, #16180, .T. ) ;
#39954 = ORIENTED_EDGE ( 'NONE', *, *, #42180, .T. ) ;
#39955 = AXIS2_PLACEMENT_3D ( 'NONE', #64912, #29192, #70152 ) ;
#39956 = ORIENTED_EDGE ( 'NONE', *, *, #35091, .F. ) ;
#39957 = CARTESIAN_POINT ( 'NONE',  ( 10.00000000000000000, 68.27212725128275395, 31.46837873495001503 ) ) ;
#39958 = DIRECTION ( 'NONE',  ( -0.000000000000000000, -0.3090169943749450088, 0.9510565162951543083 ) ) ;
#39959 = ORIENTED_EDGE ( 'NONE', *, *, #8576, .F. ) ;
#39960 = EDGE_LOOP ( 'NONE', ( #36404, #39311, #69479, #31169 ) ) ;
#39961 = CARTESIAN_POINT ( 'NONE',  ( 92.69370383062498320, 91.33154071421968467, 86.41489583420047893 ) ) ;
#39962 = VECTOR ( 'NONE', #36463, 1000.000000000000000 ) ;
#39963 = VERTEX_POINT ( 'NONE', #10168 ) ;
#39964 = CARTESIAN_POINT ( 'NONE',  ( 93.84685191531249870, -208.0026889286704943, 83.82197916753381151 ) ) ;
#39965 = CIRCLE ( 'NONE', #7548, 31.99999999999999289 ) ;
#39966 = PRODUCT_CONTEXT ( 'NONE', #56557, 'mechanical' ) ;
#39967 = CARTESIAN_POINT ( 'NONE',  ( 0.000000000000000000, 0.000000000000000000, 0.000000000000000000 ) ) ;
#39968 = CARTESIAN_POINT ( 'NONE',  ( -11.99999999999999645, 0.000000000000000000, 0.000000000000000000 ) ) ;
#39969 = LINE ( 'NONE', #62924, #71335 ) ;
#39970 = EDGE_CURVE ( 'NONE', #52585, #65473, #1044, .T. ) ;
#39971 = CARTESIAN_POINT ( 'NONE',  ( 1.560000000000000053, -0.8660254037844384856, -1.500000000000000000 ) ) ;
#39972 = FACE_OUTER_BOUND ( 'NONE', #5471, .T. ) ;
#39973 = CARTESIAN_POINT ( 'NONE',  ( -96.15314808468747287, -208.0026889286704943, 88.26697916753380468 ) ) ;
#39974 = EDGE_CURVE ( 'NONE', #43515, #40791, #43299, .T. ) ;
#39975 = CARTESIAN_POINT ( 'NONE',  ( -97.30629616937501680, 90.00000000000004263, 86.62656250086715204 ) ) ;
#39976 = ORIENTED_EDGE ( 'NONE', *, *, #27993, .T. ) ;
#39978 = CARTESIAN_POINT ( 'NONE',  ( -95.00000000000002842, 92.66308142843932671, 83.76906250086713612 ) ) ;
#39977 = CARTESIAN_POINT ( 'NONE',  ( 96.15314808468748708, 88.00268892867053694, 85.40947916753380298 ) ) ;
#39979 = EDGE_LOOP ( 'NONE', ( #72695, #2899, #44098, #53362 ) ) ;
#39980 = CARTESIAN_POINT ( 'NONE',  ( -95.00000000000002842, 93.05995642670504253, 87.93624999999998693 ) ) ;
#39981 = CARTESIAN_POINT ( 'NONE',  ( 0.000000000000000000, 0.000000000000000000, 0.000000000000000000 ) ) ;
#39982 = CARTESIAN_POINT ( 'NONE',  ( 0.000000000000000000, 0.000000000000000000, 0.000000000000000000 ) ) ;
#39983 = LINE ( 'NONE', #58372, #47621 ) ;
#39984 = CARTESIAN_POINT ( 'NONE',  ( -94.99999999999997158, -212.6630814284392557, 84.72156250086713669 ) ) ;
#39985 = FACE_OUTER_BOUND ( 'NONE', #33590, .T. ) ;
#39986 = EDGE_CURVE ( 'NONE', #71349, #46909, #71819, .T. ) ;
#39987 = EDGE_CURVE ( 'NONE', #58109, #73300, #39442, .T. ) ;
#39988 = FACE_OUTER_BOUND ( 'NONE', #22427, .T. ) ;
#39989 = DIRECTION ( 'NONE',  ( -1.000000000000000000, 0.000000000000000000, 0.000000000000000000 ) ) ;
#39990 = CARTESIAN_POINT ( 'NONE',  ( -3.000000000000000000, 9.615535125379096826, -24.73947219025905042 ) ) ;
#39991 = VERTEX_POINT ( 'NONE', #49278 ) ;
#39992 = ORIENTED_EDGE ( 'NONE', *, *, #26706, .T. ) ;
#39993 = CARTESIAN_POINT ( 'NONE',  ( -92.35000000000003695, 90.00000000000004263, 78.25249999999999773 ) ) ;
#39994 = LINE ( 'NONE', #50890, #6692 ) ;
#39995 = DIRECTION ( 'NONE',  ( 0.000000000000000000, 0.000000000000000000, 1.000000000000000000 ) ) ;
#39996 = FACE_OUTER_BOUND ( 'NONE', #29508, .T. ) ;
#39997 = DIRECTION ( 'NONE',  ( 0.000000000000000000, 0.000000000000000000, 1.000000000000000000 ) ) ;
#39998 = CARTESIAN_POINT ( 'NONE',  ( 0.000000000000000000, 36.13751322684449008, -21.40280677340332716 ) ) ;
#39999 = DIRECTION ( 'NONE',  ( -1.000000000000000000, -0.000000000000000000, -0.000000000000000000 ) ) ;
#40000 = EDGE_CURVE ( 'NONE', #37989, #36437, #25038, .T. ) ;
#40001 = ORIENTED_EDGE ( 'NONE', *, *, #65710, .F. ) ;
#40002 = CARTESIAN_POINT ( 'NONE',  ( -93.84685191531254134, 91.99731107132950569, 79.90614583420047268 ) ) ;
#40003 = AXIS2_PLACEMENT_3D ( 'NONE', #26449, #49379, #13319 ) ;
#40004 = LINE ( 'NONE', #35100, #60789 ) ;
#40005 = DIRECTION ( 'NONE',  ( 0.000000000000000000, -0.3090169943749349613, -0.9510565162951576390 ) ) ;
#40006 = AXIS2_PLACEMENT_3D ( 'NONE', #65552, #25687, #32788 ) ;
#40007 = CARTESIAN_POINT ( 'NONE',  ( -3.000000000000000000, -23.29833615347104825, -3.418703333116803744 ) ) ;
#40008 = DIRECTION ( 'NONE',  ( 1.000000000000000000, 0.000000000000000000, 0.000000000000000000 ) ) ;
#40009 = CARTESIAN_POINT ( 'NONE',  ( 10.00000000000000000, 37.22597642581158084, 10.79786254984347593 ) ) ;
#40010 = DIRECTION ( 'NONE',  ( 0.000000000000000000, -0.7431448254773954654, 0.6691306063588569053 ) ) ;
#40011 = EDGE_CURVE ( 'NONE', #30579, #54289, #15063, .T. ) ;
#40012 = VECTOR ( 'NONE', #22761, 1000.000000000000000 ) ;
#40013 =( BOUNDED_CURVE ( )  B_SPLINE_CURVE ( 2, ( #22342, #28338, #33233, #32498, #10315, #33613, #67835 ),
 .UNSPECIFIED., .F., .F. ) 
 B_SPLINE_CURVE_WITH_KNOTS ( ( 3, 2, 2, 3 ),
 ( 0.5000000000000000000, 0.5069444444444444198, 0.5138888888888887285, 0.5208333333333332593 ),
 .UNSPECIFIED. ) 
 CURVE ( )  GEOMETRIC_REPRESENTATION_ITEM ( )  RATIONAL_B_SPLINE_CURVE ( ( 1.000000000000000000, 0.8660254037844387076, 1.000000000000000000, 0.8660254037844387076, 1.000000000000000000, 0.8660254037844408170, 0.9999999999999978906 ) ) 
 REPRESENTATION_ITEM ( '' )  );
#40014 = EDGE_CURVE ( 'NONE', #71829, #27433, #50192, .T. ) ;
#40015 = VECTOR ( 'NONE', #9112, 1000.000000000000000 ) ;
#40016 = CARTESIAN_POINT ( 'NONE',  ( 97.30629616937498838, 90.00000000000002842, 76.14906250086716000 ) ) ;
#40017 = CARTESIAN_POINT ( 'NONE',  ( -96.15314808468747287, -208.0026889286704943, 79.53572916753381605 ) ) ;
#40018 = ORIENTED_EDGE ( 'NONE', *, *, #32899, .T. ) ;
#40019 = DIRECTION ( 'NONE',  ( 0.000000000000000000, 0.000000000000000000, -1.000000000000000000 ) ) ;
#40020 = DIRECTION ( 'NONE',  ( 0.000000000000000000, 0.000000000000000000, 1.000000000000000000 ) ) ;
#40021 = DIRECTION ( 'NONE',  ( -0.000000000000000000, -0.000000000000000000, 1.000000000000000000 ) ) ;
#40022 = CIRCLE ( 'NONE', #13591, 82.00000000000000000 ) ;
#40023 = AXIS2_PLACEMENT_3D ( 'NONE', #9470, #66982, #33136 ) ;
#40024 = CIRCLE ( 'NONE', #3972, 31.99999999999999645 ) ;
#40025 = CARTESIAN_POINT ( 'NONE',  ( 0.000000000000000000, 36.73666225445894185, 65.58780272294090707 ) ) ;
#40026 = CARTESIAN_POINT ( 'NONE',  ( 93.84685191531251292, -211.9973110713294489, 80.22364583420046813 ) ) ;
#40027 = ORIENTED_EDGE ( 'NONE', *, *, #29706, .F. ) ;
#40028 = LINE ( 'NONE', #62218, #39503 ) ;
#40029 = ORIENTED_EDGE ( 'NONE', *, *, #33093, .F. ) ;
#40030 = DIRECTION ( 'NONE',  ( -1.000000000000000000, 0.000000000000000000, 0.000000000000000000 ) ) ;
#40031 = ORIENTED_EDGE ( 'NONE', *, *, #31482, .T. ) ;
#40032 = LINE ( 'NONE', #68233, #69423 ) ;
#40033 = ORIENTED_EDGE ( 'NONE', *, *, #49113, .F. ) ;
#40034 = ORIENTED_EDGE ( 'NONE', *, *, #64282, .T. ) ;
#40035 = ORIENTED_EDGE ( 'NONE', *, *, #61681, .F. ) ;
#40036 = CARTESIAN_POINT ( 'NONE',  ( 93.84685191531251292, -211.9973110713294489, 75.93739583420048689 ) ) ;
#40037 = VERTEX_POINT ( 'NONE', #60579 ) ;
#40038 = EDGE_LOOP ( 'NONE', ( #18043, #30352 ) ) ;
#40039 = CARTESIAN_POINT ( 'NONE',  ( 96.15314808468748708, 88.00268892867053694, 82.39322916753381776 ) ) ;
#40040 = CARTESIAN_POINT ( 'NONE',  ( 96.32499999999998863, -212.2949673200287179, 78.78166666666666629 ) ) ;
#40041 = VERTEX_POINT ( 'NONE', #44020 ) ;
#40042 = PRODUCT_DEFINITION_FORMATION_WITH_SPECIFIED_SOURCE ( 'ANY', '', #11005, .NOT_KNOWN. ) ;
#40043 = EDGE_LOOP ( 'NONE', ( #73699, #20417, #42358, #10223 ) ) ;
#40044 = ORIENTED_EDGE ( 'NONE', *, *, #48708, .T. ) ;
#40045 = ORIENTED_EDGE ( 'NONE', *, *, #15712, .T. ) ;
#40046 = LINE ( 'NONE', #45706, #58671 ) ;
#40047 = CIRCLE ( 'NONE', #44894, 31.99999999999998224 ) ;
#40048 = CARTESIAN_POINT ( 'NONE',  ( 0.000000000000000000, -20.41045688087772092, -72.35160999960838524 ) ) ;
#40049 = LINE ( 'NONE', #67882, #15860 ) ;
#40050 = DIRECTION ( 'NONE',  ( -1.000000000000000000, -0.000000000000000000, -0.000000000000000000 ) ) ;
#40051 = ADVANCED_FACE ( 'NONE', ( #9427 ), #38377, .T. ) ;
#40052 = CARTESIAN_POINT ( 'NONE',  ( -19.90058851926621131, -132.5883508287165853, 5.500000000000000000 ) ) ;
#40053 = DIRECTION ( 'NONE',  ( -1.000000000000000000, 0.000000000000000000, 0.000000000000000000 ) ) ;
#40054 = ORIENTED_EDGE ( 'NONE', *, *, #57956, .F. ) ;
#40055 = CARTESIAN_POINT ( 'NONE',  ( -92.34999999999999432, -211.5299782133524502, 82.72395833506762131 ) ) ;
#40056 = ORIENTED_EDGE ( 'NONE', *, *, #64317, .T. ) ;
#40057 = EDGE_CURVE ( 'NONE', #66589, #24429, #33401, .T. ) ;
#40058 = DIRECTION ( 'NONE',  ( 0.000000000000000000, 0.000000000000000000, 1.000000000000000000 ) ) ;
#40059 = ORIENTED_EDGE ( 'NONE', *, *, #71691, .T. ) ;
#40061 = CARTESIAN_POINT ( 'NONE',  ( -95.00000000000002842, 93.05995642670501411, 78.49062500173430124 ) ) ;
#40060 = CARTESIAN_POINT ( 'NONE',  ( 92.34999999999999432, 91.52997821335252127, 80.50145833506765314 ) ) ;
#40062 = AXIS2_PLACEMENT_3D ( 'NONE', #5295, #5661, #74053 ) ;
#40063 = ORIENTED_EDGE ( 'NONE', *, *, #71858, .F. ) ;
#40064 = CARTESIAN_POINT ( 'NONE',  ( 96.15314808468748708, 91.99731107132950569, 80.06489583420048461 ) ) ;
#40065 = AXIS2_PLACEMENT_3D ( 'NONE', #29173, #660, #7373 ) ;
#40066 = DIRECTION ( 'NONE',  ( -0.9827303690289279636, -0.1850432970638682117, 0.000000000000000000 ) ) ;
#40067 = CARTESIAN_POINT ( 'NONE',  ( 0.000000000000000000, 0.000000000000000000, 0.000000000000000000 ) ) ;
#40068 = FACE_OUTER_BOUND ( 'NONE', #34772, .T. ) ;
#40069 = DIRECTION ( 'NONE',  ( -1.000000000000000000, 0.000000000000000000, 0.000000000000000000 ) ) ;
#40070 = EDGE_CURVE ( 'NONE', #44983, #40423, #64653, .T. ) ;
#40071 = VERTEX_POINT ( 'NONE', #20337 ) ;
#40072 = CARTESIAN_POINT ( 'NONE',  ( 5.000000000000000000, 41.91543099594818500, 2.663952781846291362 ) ) ;
#40074 = CARTESIAN_POINT ( 'NONE',  ( 26.47460221209471598, -121.8961639463267090, 5.500000000000000000 ) ) ;
#40073 = AXIS2_PLACEMENT_3D ( 'NONE', #12978, #57759, #29903 ) ;
#40075 = VECTOR ( 'NONE', #70127, 1000.000000000000000 ) ;
#40076 = DIRECTION ( 'NONE',  ( -1.000000000000000000, 0.000000000000000000, 0.000000000000000000 ) ) ;
#40077 = VERTEX_POINT ( 'NONE', #66221 ) ;
#40078 = ORIENTED_EDGE ( 'NONE', *, *, #2702, .F. ) ;
#40079 = DIRECTION ( 'NONE',  ( -1.000000000000000000, -0.000000000000000000, -0.000000000000000000 ) ) ;
#40080 = EDGE_CURVE ( 'NONE', #55666, #5845, #55044, .T. ) ;
#40081 = CARTESIAN_POINT ( 'NONE',  ( -4.279208249584786294, -3.302900657080020341, -1.325189086772939895 ) ) ;
#40082 = CARTESIAN_POINT ( 'NONE',  ( 10.00000000000000000, -29.81001611430991360, -22.74946021919165418 ) ) ;
#40083 = CARTESIAN_POINT ( 'NONE',  ( -97.30629616937497417, -211.3315407142195852, 80.32947916753381890 ) ) ;
#40084 = ORIENTED_EDGE ( 'NONE', *, *, #38215, .T. ) ;
#40085 = EDGE_CURVE ( 'NONE', #25988, #23772, #11823, .T. ) ;
#40086 = ORIENTED_EDGE ( 'NONE', *, *, #52474, .T. ) ;
#40087 = EDGE_CURVE ( 'NONE', #37730, #68048, #34216, .T. ) ;
#40088 = CIRCLE ( 'NONE', #55696, 82.00000000000000000 ) ;
#40089 = FACE_OUTER_BOUND ( 'NONE', #51218, .T. ) ;
#40090 = ADVANCED_FACE ( 'NONE', ( #22573, #6399 ), #17666, .T. ) ;
#40091 = DIRECTION ( 'NONE',  ( 0.2306669878475623159, 0.9730327541852497042, -0.000000000000000000 ) ) ;
#40092 = DIRECTION ( 'NONE',  ( 0.000000000000000000, 0.3090169943749411230, 0.9510565162951555296 ) ) ;
#40093 = CARTESIAN_POINT ( 'NONE',  ( 92.69370383062498320, 88.66845928578035796, 75.72572916753381378 ) ) ;
#40094 = DIRECTION ( 'NONE',  ( -0.000000000000000000, -0.000000000000000000, -1.000000000000000000 ) ) ;
#40095 = DIRECTION ( 'NONE',  ( -1.000000000000000000, 0.000000000000000000, 0.000000000000000000 ) ) ;
#40096 = CARTESIAN_POINT ( 'NONE',  ( 5.000000000000000000, 21.40280677340421889, -36.13751322684397138 ) ) ;
#40097 = CARTESIAN_POINT ( 'NONE',  ( -92.34999999999999432, -208.4700217866474645, 76.47979166840096354 ) ) ;
#40098 = LINE ( 'NONE', #11512, #51998 ) ;
#40099 = CARTESIAN_POINT ( 'NONE',  ( 11.99999999999999822, 70.53064760720278059, 26.01480285779964774 ) ) ;
#40100 = ADVANCED_FACE ( 'NONE', ( #68813 ), #29300, .T. ) ;
#40101 = AXIS2_PLACEMENT_3D ( 'NONE', #38148, #21591, #43448 ) ;
#40102 = CARTESIAN_POINT ( 'NONE',  ( 96.15314808468748708, 91.99731107132950569, 88.31989583420048007 ) ) ;
#40103 = AXIS2_PLACEMENT_3D ( 'NONE', #36573, #8008, #30927 ) ;
#40104 = CARTESIAN_POINT ( 'NONE',  ( -96.15314808468747287, -208.0026889286704943, 88.42572916753381662 ) ) ;
#40105 = DIRECTION ( 'NONE',  ( 0.000000000000000000, 0.000000000000000000, 1.000000000000000000 ) ) ;
#40106 = ORIENTED_EDGE ( 'NONE', *, *, #36903, .F. ) ;
#40107 = FACE_OUTER_BOUND ( 'NONE', #11163, .T. ) ;
#40108 = CARTESIAN_POINT ( 'NONE',  ( -92.69370383062504004, 90.00000000000004263, 80.43531250086714124 ) ) ;
#40109 = AXIS2_PLACEMENT_3D ( 'NONE', #41788, #19223, #12837 ) ;
#40110 = CARTESIAN_POINT ( 'NONE',  ( 11.99999999999999822, -2.956366410620109519, -75.11725578898472122 ) ) ;
#40111 = ORIENTED_EDGE ( 'NONE', *, *, #10296, .F. ) ;
#40112 = AXIS2_PLACEMENT_3D ( 'NONE', #64273, #12748, #64633 ) ;
#40113 = CARTESIAN_POINT ( 'NONE',  ( 0.000000000000000000, 22.90783923731629201, 78.73519480814962890 ) ) ;
#40115 = DIRECTION ( 'NONE',  ( -1.000000000000000000, -0.000000000000000000, 0.000000000000000000 ) ) ;
#40114 = VECTOR ( 'NONE', #41858, 1000.000000000000000 ) ;
#40116 = DIRECTION ( 'NONE',  ( 0.000000000000000000, 0.000000000000000000, 1.000000000000000000 ) ) ;
#40117 = CIRCLE ( 'NONE', #50901, 16.00000000000000000 ) ;
#40118 = CARTESIAN_POINT ( 'NONE',  ( 95.00000000000000000, -213.0599564267049857, 85.79312500173431033 ) ) ;
#40119 = AXIS2_PLACEMENT_3D ( 'NONE', #26757, #38425, #21484 ) ;
#40120 = CARTESIAN_POINT ( 'NONE',  ( 92.69370383062501162, -209.9999999999999716, 75.83156250086716454 ) ) ;
#40121 = ORIENTED_EDGE ( 'NONE', *, *, #1744, .F. ) ;
#40122 = ORIENTED_EDGE ( 'NONE', *, *, #38464, .F. ) ;
#40123 = CARTESIAN_POINT ( 'NONE',  ( 92.69370383062501162, -209.9999999999999716, 85.35656250086715602 ) ) ;
#40124 = CARTESIAN_POINT ( 'NONE',  ( -94.99999999999997158, -206.9400435732949575, 81.66562500173431260 ) ) ;
#40125 = DIRECTION ( 'NONE',  ( 0.000000000000000000, -0.5224985647159559043, 0.8526401643540879594 ) ) ;
#40126 = DIRECTION ( 'NONE',  ( 0.000000000000000000, 0.000000000000000000, 1.000000000000000000 ) ) ;
#40127 = CARTESIAN_POINT ( 'NONE',  ( 5.000000000000000000, 27.75498641678742473, 31.52238457039609187 ) ) ;
#40128 = DIRECTION ( 'NONE',  ( -1.000000000000000000, 0.000000000000000000, 0.000000000000000000 ) ) ;
#40129 = CARTESIAN_POINT ( 'NONE',  ( 96.32499999999998863, -212.2949673200287179, 87.67166666666666686 ) ) ;
#40130 = VECTOR ( 'NONE', #3186, 1000.000000000000000 ) ;
#40131 = EDGE_CURVE ( 'NONE', #40171, #41715, #72997, .T. ) ;
#40132 = VERTEX_POINT ( 'NONE', #57901 ) ;
#40133 = ORIENTED_EDGE ( 'NONE', *, *, #26712, .T. ) ;
#40134 = ORIENTED_EDGE ( 'NONE', *, *, #58068, .T. ) ;
#40135 = ORIENTED_EDGE ( 'NONE', *, *, #20211, .T. ) ;
#40136 = ADVANCED_FACE ( 'NONE', ( #11639 ), #45138, .T. ) ;
#40137 = SURFACE_SIDE_STYLE ('',( #17206 ) ) ;
#40138 = CARTESIAN_POINT ( 'NONE',  ( 3.556264818047235821, 3.720292241887089624, -5.918341802876230240 ) ) ;
#40139 = ADVANCED_FACE ( 'NONE', ( #68060 ), #28561, .T. ) ;
#40140 = FACE_OUTER_BOUND ( 'NONE', #66120, .T. ) ;
#40141 = CARTESIAN_POINT ( 'NONE',  ( 92.35000000000000853, -209.9999999999999716, 77.37937500173428873 ) ) ;
#40142 = ADVANCED_FACE ( 'NONE', ( #39500 ), #62442, .T. ) ;
#40143 = CARTESIAN_POINT ( 'NONE',  ( 94.99999999999998579, 86.94004357329500010, 79.36374999999999602 ) ) ;
#40144 = ORIENTED_EDGE ( 'NONE', *, *, #25902, .F. ) ;
#40145 = DIRECTION ( 'NONE',  ( -1.000000000000000000, 0.000000000000000000, 0.000000000000000000 ) ) ;
#40146 = ORIENTED_EDGE ( 'NONE', *, *, #33424, .F. ) ;
#40147 = CARTESIAN_POINT ( 'NONE',  ( -94.99999999999997158, -206.9400435732949575, 82.93562500173430863 ) ) ;
#40148 = AXIS2_PLACEMENT_3D ( 'NONE', #28047, #74287, #11497 ) ;
#40149 = ORIENTED_EDGE ( 'NONE', *, *, #47806, .F. ) ;
#40150 = DIRECTION ( 'NONE',  ( 0.000000000000000000, -1.000000000000000000, 0.000000000000000000 ) ) ;
#40151 = EDGE_CURVE ( 'NONE', #20908, #31608, #68444, .T. ) ;
#40152 = CARTESIAN_POINT ( 'NONE',  ( -93.84685191531252713, 88.00268892867056536, 81.75822916753382685 ) ) ;
#40153 = CARTESIAN_POINT ( 'NONE',  ( 96.15314808468748708, 91.99731107132950569, 77.36614583420046642 ) ) ;
#40154 = ORIENTED_EDGE ( 'NONE', *, *, #60357, .F. ) ;
#40155 = CARTESIAN_POINT ( 'NONE',  ( 17.82587367876289974, -104.6869915565625320, 2.500000000000000000 ) ) ;
#40156 = FACE_OUTER_BOUND ( 'NONE', #67999, .T. ) ;
#40157 = CARTESIAN_POINT ( 'NONE',  ( 10.00000000000000000, 16.45098606841173705, -33.79645857604496229 ) ) ;
#40158 = EDGE_CURVE ( 'NONE', #1173, #12862, #34582, .T. ) ;
#40159 = CARTESIAN_POINT ( 'NONE',  ( 10.00000000000000000, 30.41916302227216562, -71.27951684757994144 ) ) ;
#40160 = ORIENTED_EDGE ( 'NONE', *, *, #71758, .F. ) ;
#40161 = CARTESIAN_POINT ( 'NONE',  ( 7.001685179585692254, -14.98378029539707512, 0.000000000000000000 ) ) ;
#40162 = CARTESIAN_POINT ( 'NONE',  ( -97.30629616937497417, -211.3315407142195852, 76.36072916753381890 ) ) ;
#40163 = VECTOR ( 'NONE', #3355, 999.9999999999998863 ) ;
#40164 = ORIENTED_EDGE ( 'NONE', *, *, #36812, .T. ) ;
#40165 = ORIENTED_EDGE ( 'NONE', *, *, #36380, .F. ) ;
#40166 = FACE_BOUND ( 'NONE', #24395, .T. ) ;
#40167 = ORIENTED_EDGE ( 'NONE', *, *, #20951, .T. ) ;
#40168 = CYLINDRICAL_SURFACE ( 'NONE', #44363, 2.649999999999985700 ) ;
#40169 = AXIS2_PLACEMENT_3D ( 'NONE', #13406, #69806, #36335 ) ;
#40170 = CYLINDRICAL_SURFACE ( 'NONE', #7730, 37.49900000000000233 ) ;
#40171 = VERTEX_POINT ( 'NONE', #28202 ) ;
#40172 = CARTESIAN_POINT ( 'NONE',  ( -92.69370383062498320, -211.3315407142195852, 76.57239583420046358 ) ) ;
#40173 = ORIENTED_EDGE ( 'NONE', *, *, #30825, .F. ) ;
#40174 = AXIS2_PLACEMENT_3D ( 'NONE', #3057, #8292, #42511 ) ;
#40175 = CARTESIAN_POINT ( 'NONE',  ( 0.000000000000000000, -17.28742895386137590, 75.54627589209937355 ) ) ;
#40176 = DIRECTION ( 'NONE',  ( 1.000000000000000000, -0.000000000000000000, 0.000000000000000000 ) ) ;
#40177 = CARTESIAN_POINT ( 'NONE',  ( 0.000000000000000000, 11.30684508768452368, -76.66974797899824523 ) ) ;
#40178 = EDGE_CURVE ( 'NONE', #52246, #72116, #51498, .T. ) ;
#40179 = DIRECTION ( 'NONE',  ( 1.000000000000000000, 0.000000000000000000, 0.000000000000000000 ) ) ;
#40180 = DIRECTION ( 'NONE',  ( 1.000000000000000000, 0.000000000000000000, 0.000000000000000000 ) ) ;
#40181 = AXIS2_PLACEMENT_3D ( 'NONE', #23368, #17713, #40655 ) ;
#40182 = EDGE_CURVE ( 'NONE', #56093, #5647, #57522, .T. ) ;
#40184 = EDGE_CURVE ( 'NONE', #11833, #65189, #67111, .T. ) ;
#40183 = AXIS2_PLACEMENT_3D ( 'NONE', #55453, #8853, #26869 ) ;
#40185 = DIRECTION ( 'NONE',  ( -1.000000000000000000, -0.000000000000000000, -0.000000000000000000 ) ) ;
#40186 = CARTESIAN_POINT ( 'NONE',  ( 97.30629616937498838, 88.66845928578035796, 84.82739583420048746 ) ) ;
#40187 = DIRECTION ( 'NONE',  ( 1.000000000000000000, 0.000000000000000000, 0.000000000000000000 ) ) ;
#40188 = DIRECTION ( 'NONE',  ( -1.000000000000000000, -0.000000000000000000, 0.000000000000000000 ) ) ;
#40189 = DIRECTION ( 'NONE',  ( 0.000000000000000000, -6.938893903907231533E-15, 1.000000000000000000 ) ) ;
#40190 = FACE_OUTER_BOUND ( 'NONE', #66109, .T. ) ;
#40191 = DIRECTION ( 'NONE',  ( -1.000000000000000000, 0.000000000000000000, 0.000000000000000000 ) ) ;
#40192 = CARTESIAN_POINT ( 'NONE',  ( 2.739742549670660665, 4.191711593333631747, -0.5197061503823161566 ) ) ;
#40193 = DIRECTION ( 'NONE',  ( -1.000000000000000000, 0.000000000000000000, 0.000000000000000000 ) ) ;
#40194 = EDGE_CURVE ( 'NONE', #16556, #54092, #53923, .T. ) ;
#40195 = AXIS2_PLACEMENT_3D ( 'NONE', #20218, #66114, #19849 ) ;
#40196 = LINE ( 'NONE', #28904, #41246 ) ;
#40197 = CIRCLE ( 'NONE', #3030, 82.00000000000000000 ) ;
#40198 = CARTESIAN_POINT ( 'NONE',  ( 6.000000000000000000, -8.966570791701288456, 81.50828551894223040 ) ) ;
#40199 = CARTESIAN_POINT ( 'NONE',  ( 0.000000000000000000, 58.39081064771823293, -50.95692526931266286 ) ) ;
#40200 = LINE ( 'NONE', #69145, #45552 ) ;
#40201 = DIRECTION ( 'NONE',  ( 0.000000000000000000, 0.9238795325112851842, 0.3826834323650938896 ) ) ;
#40202 = CARTESIAN_POINT ( 'NONE',  ( -10.00000000000000000, 0.000000000000000000, 0.000000000000000000 ) ) ;
#40203 = CARTESIAN_POINT ( 'NONE',  ( 97.64999999954044085, 90.00004935162768049, 87.22187670868791542 ) ) ;
#40204 = CARTESIAN_POINT ( 'NONE',  ( 95.00000000000000000, -209.9999999999999716, 90.00000000000000000 ) ) ;
#40205 = CARTESIAN_POINT ( 'NONE',  ( 10.00000000000000000, -65.58780272294100655, 36.73666225445870737 ) ) ;
#40206 = CARTESIAN_POINT ( 'NONE',  ( 0.000000000000000000, 0.000000000000000000, 0.000000000000000000 ) ) ;
#40207 = AXIS2_PLACEMENT_3D ( 'NONE', #41612, #12296, #41996 ) ;
#40208 = CARTESIAN_POINT ( 'NONE',  ( 93.84685191531249870, -208.0026889286704943, 83.98072916753382344 ) ) ;
#40209 = EDGE_LOOP ( 'NONE', ( #51056, #34792, #58351, #43638 ) ) ;
#40210 = ORIENTED_EDGE ( 'NONE', *, *, #70662, .F. ) ;
#40211 = CARTESIAN_POINT ( 'NONE',  ( 10.00000000000000000, 0.000000000000000000, 0.000000000000000000 ) ) ;
#40212 = ORIENTED_EDGE ( 'NONE', *, *, #66552, .F. ) ;
#40213 = DIRECTION ( 'NONE',  ( 0.000000000000000000, 0.000000000000000000, 1.000000000000000000 ) ) ;
#40214 = CARTESIAN_POINT ( 'NONE',  ( 95.00000000000000000, -207.3369185715606307, 79.95906250086713385 ) ) ;
#40215 = EDGE_LOOP ( 'NONE', ( #41420, #19584, #56099, #68142 ) ) ;
#40216 = CIRCLE ( 'NONE', #7802, 31.99999999999998579 ) ;
#40217 = CARTESIAN_POINT ( 'NONE',  ( 97.30629616937498838, -209.9999999999999716, 83.13406250086715943 ) ) ;
#40218 = ORIENTED_EDGE ( 'NONE', *, *, #883, .F. ) ;
#40219 = FACE_OUTER_BOUND ( 'NONE', #12740, .T. ) ;
#40220 = VERTEX_POINT ( 'NONE', #51882 ) ;
#40221 = VECTOR ( 'NONE', #41135, 1000.000000000000000 ) ;
#40222 = EDGE_LOOP ( 'NONE', ( #313, #35398, #63201, #3374 ) ) ;
#40223 = CARTESIAN_POINT ( 'NONE',  ( 10.00000000000000000, 37.58145647212453611, 0.6853352020791767529 ) ) ;
#40224 = EDGE_CURVE ( 'NONE', #49826, #73475, #1110, .T. ) ;
#40225 = CARTESIAN_POINT ( 'NONE',  ( 92.35000000000009379, -208.4700217866474361, 80.42208333333330472 ) ) ;
#40226 = CIRCLE ( 'NONE', #23595, 31.99999999999999645 ) ;
#40227 = ORIENTED_EDGE ( 'NONE', *, *, #11930, .T. ) ;
#40228 = CYLINDRICAL_SURFACE ( 'NONE', #36487, 16.00000000000000000 ) ;
#40229 = CARTESIAN_POINT ( 'NONE',  ( 92.35000000000000853, -209.9999999999999716, 88.17437500173430465 ) ) ;
#40230 = ADVANCED_FACE ( 'NONE', ( #39122 ), #421, .T. ) ;
#40231 = ORIENTED_EDGE ( 'NONE', *, *, #17511, .T. ) ;
#40232 = DIRECTION ( 'NONE',  ( -0.000000000000000000, -0.000000000000000000, -1.000000000000000000 ) ) ;
#40233 = ORIENTED_EDGE ( 'NONE', *, *, #29177, .F. ) ;
#40234 =( BOUNDED_CURVE ( )  B_SPLINE_CURVE ( 2, ( #71083, #19587, #60213, #48539, #31975, #36882, #44387, #59834, #71454 ),
 .UNSPECIFIED., .F., .F. ) 
 B_SPLINE_CURVE_WITH_KNOTS ( ( 3, 2, 2, 2, 3 ),
 ( 0.08466915177892317401, 0.08466918649058879920, 0.09172495203147107423, 0.09878071757235334927, 0.1058364832022827134 ),
 .UNSPECIFIED. ) 
 CURVE ( )  GEOMETRIC_REPRESENTATION_ITEM ( )  RATIONAL_B_SPLINE_CURVE ( ( 0.9999986817990250687, 0.9999993408962699615, 1.000000000000000000, 0.8660254037844387076, 1.000000000000000000, 0.8660254037844387076, 1.000000000000000000, 0.8660254037844387076, 1.000000000000000000 ) ) 
 REPRESENTATION_ITEM ( '' )  );
#40235 = CARTESIAN_POINT ( 'NONE',  ( 10.00000000000000000, -20.41045688087772092, -72.35160999960838524 ) ) ;
#40236 = VERTEX_POINT ( 'NONE', #36424 ) ;
#40237 = AXIS2_PLACEMENT_3D ( 'NONE', #31449, #37850, #38208 ) ;
#40238 = ORIENTED_EDGE ( 'NONE', *, *, #53073, .T. ) ;
#40239 = ORIENTED_EDGE ( 'NONE', *, *, #60813, .F. ) ;
#40240 = DIRECTION ( 'NONE',  ( 0.000000000000000000, 0.8090169943749486725, -0.5877852522924714718 ) ) ;
#40241 = CARTESIAN_POINT ( 'NONE',  ( -5.000000000000000000, -0.2835658343809315807, -0.5205273423269579647 ) ) ;
#40242 = ORIENTED_EDGE ( 'NONE', *, *, #49916, .T. ) ;
#40243 = ORIENTED_EDGE ( 'NONE', *, *, #48286, .F. ) ;
#40244 = VECTOR ( 'NONE', #25752, 1000.000000000000000 ) ;
#40245 = ORIENTED_EDGE ( 'NONE', *, *, #26808, .F. ) ;
#40246 = CARTESIAN_POINT ( 'NONE',  ( 92.35002740377129271, 91.52999403492727026, 79.86645724064027263 ) ) ;
#40247 = DIRECTION ( 'NONE',  ( -1.000000000000000000, 0.000000000000000000, 0.000000000000000000 ) ) ;
#40248 = EDGE_CURVE ( 'NONE', #13679, #51673, #58692, .T. ) ;
#40249 = CARTESIAN_POINT ( 'NONE',  ( -96.32500000000001705, 92.29496732002878900, 89.25916666666667254 ) ) ;
#40250 = EDGE_CURVE ( 'NONE', #21255, #29678, #61113, .T. ) ;
#40251 = ORIENTED_EDGE ( 'NONE', *, *, #8345, .F. ) ;
#40252 = DIRECTION ( 'NONE',  ( 1.000000000000000000, 0.000000000000000000, 0.000000000000000000 ) ) ;
#40253 = VERTEX_POINT ( 'NONE', #53721 ) ;
#40254 = DIRECTION ( 'NONE',  ( -0.000000000000000000, -0.000000000000000000, 1.000000000000000000 ) ) ;
#40255 = CARTESIAN_POINT ( 'NONE',  ( -97.30629616937497417, -211.3315407142195852, 86.52072916753381548 ) ) ;
#40256 = ORIENTED_EDGE ( 'NONE', *, *, #30538, .T. ) ;
#40257 = DIRECTION ( 'NONE',  ( 0.000000000000000000, 0.8910065241883690090, -0.4539904997395446395 ) ) ;
#40258 = CARTESIAN_POINT ( 'NONE',  ( 15.00000000000000000, 16.61724383029390140, 20.69703378468902955 ) ) ;
#40259 = CARTESIAN_POINT ( 'NONE',  ( 10.00000000000000000, 16.00000000000000000, 2.500000000000000000 ) ) ;
#40260 = CARTESIAN_POINT ( 'NONE',  ( -94.99999999999997158, -212.6630814284392557, 75.19656250086714522 ) ) ;
#40261 = CARTESIAN_POINT ( 'NONE',  ( 95.00000000002596323, -209.9999999999999147, -74.99999999999349143 ) ) ;
#40262 = CYLINDRICAL_SURFACE ( 'NONE', #51173, 12.49999999999999645 ) ;
#40263 = EDGE_CURVE ( 'NONE', #3810, #11463, #70626, .T. ) ;
#40264 = EDGE_CURVE ( 'NONE', #74142, #28208, #63539, .T. ) ;
#40265 = AXIS2_PLACEMENT_3D ( 'NONE', #59568, #30975, #54659 ) ;
#40266 = CARTESIAN_POINT ( 'NONE',  ( -97.65000000000001990, 90.00000000000004263, 84.99937500173429328 ) ) ;
#40267 = CARTESIAN_POINT ( 'NONE',  ( 92.35000000000000853, -209.9999999999999716, 81.10999999999999943 ) ) ;
#40268 = LINE ( 'NONE', #41018, #66794 ) ;
#40269 = CARTESIAN_POINT ( 'NONE',  ( -97.30629616937501680, 88.66845928578038638, 78.90072916753381094 ) ) ;
#40270 = CARTESIAN_POINT ( 'NONE',  ( 11.99999999999999822, 12.93880638057426502, -76.41127070299258150 ) ) ;
#40271 = DIRECTION ( 'NONE',  ( 0.000000000000000000, 0.000000000000000000, -1.000000000000000000 ) ) ;
#40272 = AXIS2_PLACEMENT_3D ( 'NONE', #52131, #63803, #12273 ) ;
#40273 = VERTEX_POINT ( 'NONE', #59006 ) ;
#40274 = CIRCLE ( 'NONE', #61912, 31.99999999999998934 ) ;
#40275 = CARTESIAN_POINT ( 'NONE',  ( 0.000000000000000000, 66.50666863322000211, 39.78640506895629159 ) ) ;
#40277 = LINE ( 'NONE', #74109, #20895 ) ;
#40276 = AXIS2_PLACEMENT_3D ( 'NONE', #39558, #33907, #56850 ) ;
#40278 = FACE_OUTER_BOUND ( 'NONE', #54447, .T. ) ;
#40279 = CARTESIAN_POINT ( 'NONE',  ( 10.00000000000000000, 37.16516213103277977, 4.992566952385115719 ) ) ;
#40280 = DIRECTION ( 'NONE',  ( 0.000000000000000000, 0.000000000000000000, 1.000000000000000000 ) ) ;
#40281 = CARTESIAN_POINT ( 'NONE',  ( 0.000000000000000000, 26.50000000000000711, 1.500000000000000000 ) ) ;
#40282 = CARTESIAN_POINT ( 'NONE',  ( -92.69370383062498320, -208.6684592857803011, 76.20197916753382117 ) ) ;
#40283 = AXIS2_PLACEMENT_3D ( 'NONE', #11146, #57015, #44627 ) ;
#40284 = DIRECTION ( 'NONE',  ( -1.000000000000000000, -0.000000000000000000, 0.000000000000000000 ) ) ;
#40285 = APPLICATION_CONTEXT ( 'automotive_design' ) ;
#40286 = VERTEX_POINT ( 'NONE', #13501 ) ;
#40287 = DIRECTION ( 'NONE',  ( 1.000000000000000000, 0.000000000000000000, 0.000000000000000000 ) ) ;
#40288 = CIRCLE ( 'NONE', #34268, 82.00000000000000000 ) ;
#40289 = CARTESIAN_POINT ( 'NONE',  ( -92.35000000000003695, 90.00000000000004263, 88.41249999999999432 ) ) ;
#40290 = DIRECTION ( 'NONE',  ( 0.6575728627325957421, -0.7533909544171994987, 0.000000000000000000 ) ) ;
#40291 = FACE_OUTER_BOUND ( 'NONE', #64459, .T. ) ;
#40292 = VECTOR ( 'NONE', #15884, 1000.000000000000114 ) ;
#40293 = CARTESIAN_POINT ( 'NONE',  ( 0.000000000000000000, -8.840884882374576037, -74.65374052328658649 ) ) ;
#40294 = ORIENTED_EDGE ( 'NONE', *, *, #58049, .F. ) ;
#40295 = FACE_OUTER_BOUND ( 'NONE', #46318, .T. ) ;
#40296 = CYLINDRICAL_SURFACE ( 'NONE', #64344, 77.49899999999999523 ) ;
#40297 = ORIENTED_EDGE ( 'NONE', *, *, #8897, .T. ) ;
#40298 = DIRECTION ( 'NONE',  ( -0.000000000000000000, -0.9135454576426059736, 0.4067366430757887730 ) ) ;
#40299 = FACE_OUTER_BOUND ( 'NONE', #16354, .T. ) ;
#40300 = ORIENTED_EDGE ( 'NONE', *, *, #34047, .F. ) ;
#40301 = PRODUCT_DEFINITION ( 'UNKNOWN', '', #6406, #54422 ) ;
#40302 = EDGE_CURVE ( 'NONE', #21993, #38841, #21424, .T. ) ;
#40303 = CARTESIAN_POINT ( 'NONE',  ( -23.50044424985617653, 0.001194404164806279773, -48.99999999999938893 ) ) ;
#40304 = VERTEX_POINT ( 'NONE', #64640 ) ;
#40305 = CARTESIAN_POINT ( 'NONE',  ( -7.001685179585692254, -14.98378029539707512, -1.199999999999999956 ) ) ;
#40306 = VERTEX_POINT ( 'NONE', #7860 ) ;
#40307 = CARTESIAN_POINT ( 'NONE',  ( -3.000000000000000000, -20.55727247249748046, 16.78983467731285018 ) ) ;
#40308 = ORIENTED_EDGE ( 'NONE', *, *, #26485, .F. ) ;
#40309 = EDGE_CURVE ( 'NONE', #50450, #18578, #10664, .T. ) ;
#40310 = LINE ( 'NONE', #57616, #34544 ) ;
#40311 = ORIENTED_EDGE ( 'NONE', *, *, #46443, .T. ) ;
#40312 = ORIENTED_EDGE ( 'NONE', *, *, #67019, .F. ) ;
#40313 = LINE ( 'NONE', #40691, #74065 ) ;
#40314 = ADVANCED_FACE ( 'NONE', ( #29662 ), #30409, .T. ) ;
#40315 = ORIENTED_EDGE ( 'NONE', *, *, #45772, .F. ) ;
#40316 = ORIENTED_EDGE ( 'NONE', *, *, #15418, .F. ) ;
#40317 = DIRECTION ( 'NONE',  ( -1.000000000000000000, -0.000000000000000000, 0.000000000000000000 ) ) ;
#40318 = ADVANCED_FACE ( 'NONE', ( #71001 ), #52993, .T. ) ;
#40319 = AXIS2_PLACEMENT_3D ( 'NONE', #14444, #71579, #37399 ) ;
#40320 = VERTEX_POINT ( 'NONE', #24412 ) ;
#40321 = ORIENTED_EDGE ( 'NONE', *, *, #34135, .T. ) ;
#40322 = CARTESIAN_POINT ( 'NONE',  ( 97.30629616937498838, 88.66845928578037217, 84.82739583420045903 ) ) ;
#40323 = VERTEX_POINT ( 'NONE', #18039 ) ;
#40324 = CIRCLE ( 'NONE', #33121, 82.00000000000000000 ) ;
#40325 = CARTESIAN_POINT ( 'NONE',  ( 93.84685191531251292, -211.9973110713294489, 83.39864583420047950 ) ) ;
#40326 = SHAPE_DEFINITION_REPRESENTATION ( #8545, #49787 ) ;
#40327 = CARTESIAN_POINT ( 'NONE',  ( -94.99999999999997158, -206.9400435732949575, 76.50624999999999432 ) ) ;
#40328 = DIRECTION ( 'NONE',  ( 1.000000000000000000, 0.000000000000000000, 0.000000000000000000 ) ) ;
#40329 = AXIS2_PLACEMENT_3D ( 'NONE', #18825, #64710, #13193 ) ;
#40330 = CARTESIAN_POINT ( 'NONE',  ( 93.67500000000001137, -207.7050326799711968, 79.09916666666666174 ) ) ;
#40331 = DIRECTION ( 'NONE',  ( 0.000000000000000000, -0.2079116908177641998, -0.9781476007338046896 ) ) ;
#40332 = CIRCLE ( 'NONE', #7915, 77.49900000000000944 ) ;
#40333 = DIRECTION ( 'NONE',  ( -1.000000000000000000, 0.000000000000000000, 0.000000000000000000 ) ) ;
#40334 = DIRECTION ( 'NONE',  ( -1.000000000000000000, 0.000000000000000000, 0.000000000000000000 ) ) ;
#40335 = CARTESIAN_POINT ( 'NONE',  ( -92.69370383062498320, -209.9999999999999716, 84.88031250086713442 ) ) ;
#40336 = EDGE_CURVE ( 'NONE', #40700, #41879, #32272, .T. ) ;
#40337 = CARTESIAN_POINT ( 'NONE',  ( -92.69370383062502583, 88.66845928578038638, 81.81114583420048803 ) ) ;
#40338 = EDGE_CURVE ( 'NONE', #23224, #47350, #45511, .T. ) ;
#40339 = ORIENTED_EDGE ( 'NONE', *, *, #2957, .T. ) ;
#40341 = CARTESIAN_POINT ( 'NONE',  ( -95.00000000000002842, 87.33691857156074434, 84.08656250086713158 ) ) ;
#40340 = CARTESIAN_POINT ( 'NONE',  ( 92.69370383062498320, 91.33154071421968467, 84.50989583420046358 ) ) ;
#40342 = VECTOR ( 'NONE', #19625, 1000.000000000000000 ) ;
#40343 = VERTEX_POINT ( 'NONE', #53354 ) ;
#40344 = LINE ( 'NONE', #5775, #33533 ) ;
#40345 = DIRECTION ( 'NONE',  ( 1.000000000000000000, -3.061616997868382648E-16, -0.000000000000000000 ) ) ;
#40346 = CARTESIAN_POINT ( 'NONE',  ( 24.95699195200416654, -110.9640411295978595, 5.500000000000000000 ) ) ;
#40347 = FACE_OUTER_BOUND ( 'NONE', #21072, .T. ) ;
#40348 = CARTESIAN_POINT ( 'NONE',  ( -92.69370383062498320, -208.6684592857803295, 86.20322916753380582 ) ) ;
#40349 = CARTESIAN_POINT ( 'NONE',  ( 97.64999999999999147, -209.9999999999999716, 82.06250000000000000 ) ) ;
#40350 = CARTESIAN_POINT ( 'NONE',  ( 10.00000000000000000, -71.91182617369207719, 28.89263327155721228 ) ) ;
#40351 = DIRECTION ( 'NONE',  ( 0.000000000000000000, 0.9969173337331281859, -0.07845909572784168229 ) ) ;
#40352 = DIRECTION ( 'NONE',  ( -1.000000000000000000, 0.000000000000000000, 0.000000000000000000 ) ) ;
#40353 = ORIENTED_EDGE ( 'NONE', *, *, #33361, .F. ) ;
#40354 = VECTOR ( 'NONE', #52313, 1000.000000000000000 ) ;
#40355 = ORIENTED_EDGE ( 'NONE', *, *, #49960, .F. ) ;
#40356 = CARTESIAN_POINT ( 'NONE',  ( -97.65000000000001990, 88.47002178664754979, 77.98791666666664923 ) ) ;
#40357 = DIRECTION ( 'NONE',  ( -1.000000000000000000, -0.000000000000000000, 0.000000000000000000 ) ) ;
#40358 = CYLINDRICAL_SURFACE ( 'NONE', #47774, 37.49900000000000233 ) ;
#40359 = CARTESIAN_POINT ( 'NONE',  ( 97.64999999999999147, 90.00000000000002842, 76.34749999999999659 ) ) ;
#40360 = LINE ( 'NONE', #13536, #11147 ) ;
#40361 = DIRECTION ( 'NONE',  ( 0.000000000000000000, -0.7071067811865536790, 0.7071067811865413555 ) ) ;
#40362 = LINE ( 'NONE', #58389, #51649 ) ;
#40363 = ORIENTED_EDGE ( 'NONE', *, *, #10467, .F. ) ;
#40364 = CARTESIAN_POINT ( 'NONE',  ( -95.00000000000002842, 92.66308142843932671, 78.05406250086714692 ) ) ;
#40365 = LINE ( 'NONE', #28709, #65562 ) ;
#40366 = CARTESIAN_POINT ( 'NONE',  ( 10.00000000000000000, 14.66109333815564852, -73.73191006444555740 ) ) ;
#40367 = CARTESIAN_POINT ( 'NONE',  ( 10.00000000000000000, 0.000000000000000000, 0.000000000000000000 ) ) ;
#40368 = CARTESIAN_POINT ( 'NONE',  ( -3.000000000000000000, 0.000000000000000000, 0.000000000000000000 ) ) ;
#40369 = CARTESIAN_POINT ( 'NONE',  ( -97.64998576286728849, 88.47001356683513507, 75.52729223699087413 ) ) ;
#40370 = CARTESIAN_POINT ( 'NONE',  ( -92.69370383062498320, -208.6684592857803011, 88.26697916753381890 ) ) ;
#40371 = VECTOR ( 'NONE', #54224, 1000.000000000000000 ) ;
#40372 = CARTESIAN_POINT ( 'NONE',  ( 94.99999999999998579, 87.33691857156068750, 77.26031250086714408 ) ) ;
#40373 = ADVANCED_FACE ( 'NONE', ( #1895 ), #35332, .T. ) ;
#40374 = CARTESIAN_POINT ( 'NONE',  ( -93.84685191531248449, -208.0026889286704943, 78.15989583420049769 ) ) ;
#40375 = VERTEX_POINT ( 'NONE', #2639 ) ;
#40376 = DIRECTION ( 'NONE',  ( 0.000000000000000000, 0.000000000000000000, 1.000000000000000000 ) ) ;
#40377 = CARTESIAN_POINT ( 'NONE',  ( -4.653126046682595884, -146.1313684676804314, -5.500000000000000000 ) ) ;
#40378 = CARTESIAN_POINT ( 'NONE',  ( 97.65000000000000568, -211.5299782133524218, 78.91395833506763324 ) ) ;
#40379 = CIRCLE ( 'NONE', #19972, 82.00000000000000000 ) ;
#40380 = EDGE_CURVE ( 'NONE', #28623, #26543, #20254, .T. ) ;
#40381 = AXIS2_PLACEMENT_3D ( 'NONE', #20902, #26164, #37837 ) ;
#40382 = CARTESIAN_POINT ( 'NONE',  ( -93.84685191531252713, 88.00268892867056536, 76.04322916753382344 ) ) ;
#40383 = CARTESIAN_POINT ( 'NONE',  ( 92.69370383062501162, -209.9999999999999716, 75.67281250086713840 ) ) ;
#40384 = ORIENTED_EDGE ( 'NONE', *, *, #30953, .F. ) ;
#40385 = EDGE_CURVE ( 'NONE', #5496, #25706, #17847, .T. ) ;
#40386 = CIRCLE ( 'NONE', #39165, 77.49900000000000944 ) ;
#40387 = DIRECTION ( 'NONE',  ( 0.000000000000000000, 0.000000000000000000, 1.000000000000000000 ) ) ;
#40388 = ORIENTED_EDGE ( 'NONE', *, *, #72538, .T. ) ;
#40389 = CIRCLE ( 'NONE', #7973, 31.99999999999999645 ) ;
#40390 = CARTESIAN_POINT ( 'NONE',  ( -92.34999999999999432, -208.4700217866474645, 87.90979166840097037 ) ) ;
#40391 = ORIENTED_EDGE ( 'NONE', *, *, #53289, .F. ) ;
#40392 = EDGE_CURVE ( 'NONE', #48178, #60576, #50988, .T. ) ;
#40393 = FACE_OUTER_BOUND ( 'NONE', #36588, .T. ) ;
#40394 = VECTOR ( 'NONE', #37537, 1000.000000000000114 ) ;
#40395 = ORIENTED_EDGE ( 'NONE', *, *, #20030, .T. ) ;
#40396 = EDGE_LOOP ( 'NONE', ( #67330, #58273, #10367, #62996 ) ) ;
#40397 = ORIENTED_EDGE ( 'NONE', *, *, #50465, .F. ) ;
#40398 = CARTESIAN_POINT ( 'NONE',  ( -15.44521549751111422, -137.7748507232956001, 5.500000000000000000 ) ) ;
#40399 = VERTEX_POINT ( 'NONE', #72117 ) ;
#40400 = VERTEX_POINT ( 'NONE', #26991 ) ;
#40401 = CARTESIAN_POINT ( 'NONE',  ( 92.69370383062498320, 90.00000000000002842, 84.08656250086716000 ) ) ;
#40402 = EDGE_CURVE ( 'NONE', #37124, #44604, #54834, .T. ) ;
#40403 = CARTESIAN_POINT ( 'NONE',  ( 97.64999999999999147, -209.9999999999999716, 76.34749999999999659 ) ) ;
#40404 = VERTEX_POINT ( 'NONE', #43580 ) ;
#40405 = VERTEX_POINT ( 'NONE', #71365 ) ;
#40406 = VERTEX_POINT ( 'NONE', #55947 ) ;
#40407 = ORIENTED_EDGE ( 'NONE', *, *, #9569, .T. ) ;
#40408 = CARTESIAN_POINT ( 'NONE',  ( 11.99999999999999822, -39.78640506895651896, 66.50666863321988842 ) ) ;
#40409 = CLOSED_SHELL ( 'NONE', ( #55999, #57791, #52458, #10892, #67933, #37099, #40564, #53920, #56864, #29122, #35212, #15882, #2442, #72050, #33064, #4207, #7043, #47278, #68101, #36479, #21796, #27895, #8485, #52426, #1416, #41606, #38514, #2994, #38388, #40090, #24218, #62046, #11845, #48489, #11125, #63910 ) ) ;
#40410 =( NAMED_UNIT ( * ) SI_UNIT ( $, .STERADIAN. ) SOLID_ANGLE_UNIT ( ) );
#40411 = DIRECTION ( 'NONE',  ( 1.000000000000000000, 0.000000000000000000, 0.000000000000000000 ) ) ;
#40412 = DIRECTION ( 'NONE',  ( 0.000000000000000000, 0.000000000000000000, -1.000000000000000000 ) ) ;
#40413 = DIRECTION ( 'NONE',  ( 1.000000000000000000, 0.000000000000000000, 0.000000000000000000 ) ) ;
#40414 = FACE_BOUND ( 'NONE', #15797, .T. ) ;
#40415 = CARTESIAN_POINT ( 'NONE',  ( -7.500000000000016875, -80.00000000000001421, -269.9999999999999432 ) ) ;
#40416 = CARTESIAN_POINT ( 'NONE',  ( 0.000000000000000000, -41.19522573413687638, -65.64334221924953283 ) ) ;
#40417 = ORIENTED_EDGE ( 'NONE', *, *, #67264, .F. ) ;
#40418 = CARTESIAN_POINT ( 'NONE',  ( -97.64999999999994884, -208.4700217866474645, 79.86645833506761960 ) ) ;
#40420 = ORIENTED_EDGE ( 'NONE', *, *, #33617, .F. ) ;
#40419 = EDGE_CURVE ( 'NONE', #3158, #21881, #8972, .T. ) ;
#40421 = DIRECTION ( 'NONE',  ( 1.000000000000000000, 0.000000000000000000, 0.000000000000000000 ) ) ;
#40422 = ADVANCED_FACE ( 'NONE', ( #15342 ), #49925, .T. ) ;
#40423 = VERTEX_POINT ( 'NONE', #19871 ) ;
#40425 = CARTESIAN_POINT ( 'NONE',  ( -93.67500000000003979, 87.70503267997129626, 80.76604166840097321 ) ) ;
#40424 = CARTESIAN_POINT ( 'NONE',  ( 96.32499999999997442, 92.29496732002878900, 78.43770833506764006 ) ) ;
#40427 = EDGE_CURVE ( 'NONE', #42621, #26528, #74314, .T. ) ;
#40426 = ORIENTED_EDGE ( 'NONE', *, *, #48564, .F. ) ;
#40428 = CARTESIAN_POINT ( 'NONE',  ( 97.30629616937498838, 88.66845928578037217, 79.27114583420048177 ) ) ;
#40429 = CIRCLE ( 'NONE', #51204, 20.64000000000000057 ) ;
#40430 = DIRECTION ( 'NONE',  ( 0.000000000000000000, -1.000000000000000000, 0.000000000000000000 ) ) ;
#40431 = DIRECTION ( 'NONE',  ( 0.000000000000000000, 0.000000000000000000, 1.000000000000000000 ) ) ;
#40432 = CARTESIAN_POINT ( 'NONE',  ( 95.00000000000000000, -213.0599564267049857, 79.44312500173430180 ) ) ;
#40433 = CARTESIAN_POINT ( 'NONE',  ( 97.64999999999999147, 90.00000000000002842, 90.00000000000000000 ) ) ;
#40434 = ORIENTED_EDGE ( 'NONE', *, *, #1133, .F. ) ;
#40435 = CYLINDRICAL_SURFACE ( 'NONE', #54386, 2.649999999999985700 ) ;
#40436 = LINE ( 'NONE', #41185, #38516 ) ;
#40437 = LINE ( 'NONE', #45737, #58802 ) ;
#40438 = VERTEX_POINT ( 'NONE', #54461 ) ;
#40439 = AXIS2_PLACEMENT_3D ( 'NONE', #48205, #36542, #71488 ) ;
#40440 = ORIENTED_EDGE ( 'NONE', *, *, #13986, .F. ) ;
#40441 = AXIS2_PLACEMENT_3D ( 'NONE', #50619, #73546, #45752 ) ;
#40442 = PRODUCT_DEFINITION_SHAPE ( 'NONE', 'NONE',  #74369 ) ;
#40443 = CARTESIAN_POINT ( 'NONE',  ( 11.99999999999999822, 75.11764819372149304, 29.05362095685338275 ) ) ;
#40444 = VECTOR ( 'NONE', #40551, 1000.000000000000000 ) ;
#40445 = CARTESIAN_POINT ( 'NONE',  ( -23.49999999999781863, -119.9999999999996021, -49.00000000000058265 ) ) ;
#40446 = FACE_OUTER_BOUND ( 'NONE', #3476, .T. ) ;
#40447 =( BOUNDED_CURVE ( )  B_SPLINE_CURVE ( 2, ( #39820, #33405, #28149 ),
 .UNSPECIFIED., .F., .T. ) 
 B_SPLINE_CURVE_WITH_KNOTS ( ( 3, 3 ),
 ( 0.9791666666666669627, 0.9841647806526082620 ),
 .UNSPECIFIED. ) 
 CURVE ( )  GEOMETRIC_REPRESENTATION_ITEM ( )  RATIONAL_B_SPLINE_CURVE ( ( 0.9999999999999935607, 0.9035746763527574554, 0.9459494432169380795 ) ) 
 REPRESENTATION_ITEM ( '' )  );
#40448 = CARTESIAN_POINT ( 'NONE',  ( -97.30629616937497417, -211.3315407142195852, 78.42447916753380355 ) ) ;
#40449 = ORIENTED_EDGE ( 'NONE', *, *, #13670, .T. ) ;
#40450 = CIRCLE ( 'NONE', #36847, 31.99999999999999289 ) ;
#40451 = LINE ( 'NONE', #70118, #63120 ) ;
#40452 = LINE ( 'NONE', #22812, #39069 ) ;
#40453 = VECTOR ( 'NONE', #34107, 1000.000000000000000 ) ;
#40454 = LINE ( 'NONE', #46104, #30917 ) ;
#40455 = CARTESIAN_POINT ( 'NONE',  ( 93.84685191531248449, 91.99731107132950569, 76.20197916753380696 ) ) ;
#40456 = CYLINDRICAL_SURFACE ( 'NONE', #16130, 2.649999999999985700 ) ;
#40457 = DIRECTION ( 'NONE',  ( 0.000000000000000000, 0.000000000000000000, 1.000000000000000000 ) ) ;
#40458 = DIRECTION ( 'NONE',  ( 0.2867529058022035837, -0.9580045777625452175, 0.000000000000000000 ) ) ;
#40459 = CARTESIAN_POINT ( 'NONE',  ( 2.500000000000034639, 90.00000000000000000, -310.0000000000000000 ) ) ;
#40460 = CARTESIAN_POINT ( 'NONE',  ( 15.00000000000000000, 26.49999999999999645, 1.499999999999995781 ) ) ;
#40461 = AXIS2_PLACEMENT_3D ( 'NONE', #46801, #29115, #6575 ) ;
#40462 = CARTESIAN_POINT ( 'NONE',  ( 0.1915406271734537980, -118.5122795329289858, 2.500000000000000000 ) ) ;
#40463 = CARTESIAN_POINT ( 'NONE',  ( 92.69370383062498320, 88.66845928578035796, 86.04447916753382231 ) ) ;
#40464 = CARTESIAN_POINT ( 'NONE',  ( 15.00000000000000000, 16.61724383029361718, -20.69703378468926402 ) ) ;
#40465 = CARTESIAN_POINT ( 'NONE',  ( 96.32499999999998863, 87.70503267997126784, 82.59166666666665435 ) ) ;
#40467 = EDGE_CURVE ( 'NONE', #58013, #11414, #25888, .T. ) ;
#40466 = ORIENTED_EDGE ( 'NONE', *, *, #36856, .F. ) ;
#40468 = DIRECTION ( 'NONE',  ( 1.000000000000000000, 0.000000000000000000, -0.000000000000000000 ) ) ;
#40469 = CARTESIAN_POINT ( 'NONE',  ( -95.00000000000002842, 92.66308142843932671, 78.68906250086713783 ) ) ;
#40470 = ADVANCED_FACE ( 'NONE', ( #2996 ), #55207, .T. ) ;
#40471 = LINE ( 'NONE', #63065, #5074 ) ;
#40472 = ADVANCED_FACE ( 'NONE', ( #9332 ), #14979, .T. ) ;
#40473 = ORIENTED_EDGE ( 'NONE', *, *, #18401, .T. ) ;
#40474 = CARTESIAN_POINT ( 'NONE',  ( 0.000000000000000000, -51.02545421589363883, 55.20638768913742922 ) ) ;
#40475 = DIRECTION ( 'NONE',  ( 1.000000000000000000, 0.000000000000000000, 0.000000000000000000 ) ) ;
#40476 = AXIS2_PLACEMENT_3D ( 'NONE', #16126, #72511, #68004 ) ;
#40477 = DIRECTION ( 'NONE',  ( 0.000000000000000000, 0.000000000000000000, 1.000000000000000000 ) ) ;
#40478 = AXIS2_PLACEMENT_3D ( 'NONE', #55661, #26347, #54919 ) ;
#40479 = EDGE_CURVE ( 'NONE', #69052, #59737, #50259, .T. ) ;
#40480 = LINE ( 'NONE', #23938, #62200 ) ;
#40481 = CARTESIAN_POINT ( 'NONE',  ( 97.30629616937498838, -208.6684592857803011, 75.56697916753383026 ) ) ;
#40482 = DIRECTION ( 'NONE',  ( -0.000000000000000000, -1.000000000000000000, -0.000000000000000000 ) ) ;
#40483 = VECTOR ( 'NONE', #6430, 1000.000000000000000 ) ;
#40484 = ORIENTED_EDGE ( 'NONE', *, *, #54773, .F. ) ;
#40485 = AXIS2_PLACEMENT_3D ( 'NONE', #16328, #33232, #40008 ) ;
#40486 = VERTEX_POINT ( 'NONE', #71736 ) ;
#40487 = CARTESIAN_POINT ( 'NONE',  ( 92.69370383062501162, -209.9999999999999716, 82.81656250086714977 ) ) ;
#40488 = DIRECTION ( 'NONE',  ( -1.000000000000000000, 0.000000000000000000, 0.000000000000000000 ) ) ;
#40489 = VECTOR ( 'NONE', #40284, 1000.000000000000000 ) ;
#40490 = CARTESIAN_POINT ( 'NONE',  ( 0.000000000000000000, 0.000000000000000000, 0.000000000000000000 ) ) ;
#40491 = CYLINDRICAL_SURFACE ( 'NONE', #31662, 31.99999999999998579 ) ;
#40492 = CARTESIAN_POINT ( 'NONE',  ( 5.822613034544236399, -142.8165987265839760, 2.500000000000000000 ) ) ;
#40493 = EDGE_CURVE ( 'NONE', #73031, #73482, #59891, .T. ) ;
#40494 = CARTESIAN_POINT ( 'NONE',  ( 0.000000000000000000, -16.45098606841149902, 33.79645857604508308 ) ) ;
#40495 = CARTESIAN_POINT ( 'NONE',  ( 92.35000000000002274, -211.5299782133524502, 84.97291666666666288 ) ) ;
#40496 = ORIENTED_EDGE ( 'NONE', *, *, #13754, .T. ) ;
#40497 = ORIENTED_EDGE ( 'NONE', *, *, #24116, .F. ) ;
#40498 = VERTEX_POINT ( 'NONE', #20239 ) ;
#40499 = ORIENTED_EDGE ( 'NONE', *, *, #50909, .T. ) ;
#40500 = DIRECTION ( 'NONE',  ( 0.000000000000000000, 0.9781476007338044676, 0.2079116908177653100 ) ) ;
#40501 = VECTOR ( 'NONE', #16081, 1000.000000000000000 ) ;
#40502 = CARTESIAN_POINT ( 'NONE',  ( -97.30629616937501680, 90.00000000000004263, 85.99156250086716113 ) ) ;
#40503 = DIRECTION ( 'NONE',  ( -1.000000000000000000, -0.000000000000000000, -0.000000000000000000 ) ) ;
#40504 = DIRECTION ( 'NONE',  ( 1.000000000000000000, 0.000000000000000000, 0.000000000000000000 ) ) ;
#40505 = CARTESIAN_POINT ( 'NONE',  ( 92.35000000000002274, -208.4700217866474645, 75.42145833506764063 ) ) ;
#40506 = CARTESIAN_POINT ( 'NONE',  ( 93.67499999999998295, 92.29496732002878900, 77.82916666666665151 ) ) ;
#40507 = AXIS2_PLACEMENT_3D ( 'NONE', #66672, #8042, #61778 ) ;
#40508 = ORIENTED_EDGE ( 'NONE', *, *, #12954, .F. ) ;
#40509 = LINE ( 'NONE', #16852, #1156 ) ;
#40510 = ORIENTED_EDGE ( 'NONE', *, *, #32845, .F. ) ;
#40511 = EDGE_CURVE ( 'NONE', #47167, #40375, #26626, .T. ) ;
#40512 = CARTESIAN_POINT ( 'NONE',  ( -97.64999999999996305, -209.9999999999999716, 83.09437500173430635 ) ) ;
#40513 = EDGE_CURVE ( 'NONE', #28422, #68067, #33452, .T. ) ;
#40514 = ORIENTED_EDGE ( 'NONE', *, *, #6046, .F. ) ;
#40515 = CARTESIAN_POINT ( 'NONE',  ( -92.35000000000003695, 90.00000000000004263, 88.49187500173430010 ) ) ;
#40516 = CARTESIAN_POINT ( 'NONE',  ( -96.15314808468752972, 91.99731107132950569, 81.44072916753381719 ) ) ;
#40517 = CARTESIAN_POINT ( 'NONE',  ( 94.99999999999998579, 87.33691857156068750, 88.69031250086716511 ) ) ;
#40518 = ORIENTED_EDGE ( 'NONE', *, *, #24759, .T. ) ;
#40519 = CARTESIAN_POINT ( 'NONE',  ( 0.000000000000000000, 16.83928648764923253, 16.46020748918050458 ) ) ;
#40520 = DIRECTION ( 'NONE',  ( -1.000000000000000000, -0.000000000000000000, 0.000000000000000000 ) ) ;
#40521 = CARTESIAN_POINT ( 'NONE',  ( 97.64997490602121388, 88.47000729863215440, 89.07395733288670669 ) ) ;
#40522 = CARTESIAN_POINT ( 'NONE',  ( 3.000000000000000000, 2.935248768560057897, -3.252606517456513302E-15 ) ) ;
#40523 = ORIENTED_EDGE ( 'NONE', *, *, #51009, .F. ) ;
#40524 = CARTESIAN_POINT ( 'NONE',  ( 11.99999999999999822, 73.72996012237440766, 14.67089635893739619 ) ) ;
#40525 = CARTESIAN_POINT ( 'NONE',  ( -97.30629616937495996, -209.9999999999999716, 78.84781250086714977 ) ) ;
#40526 = EDGE_LOOP ( 'NONE', ( #11429, #67579, #5494, #6760 ) ) ;
#40527 = EDGE_LOOP ( 'NONE', ( #13067, #14779, #19517, #50771 ) ) ;
#40528 = DIRECTION ( 'NONE',  ( -1.000000000000000000, 0.000000000000000000, -0.000000000000000000 ) ) ;
#40529 = ORIENTED_EDGE ( 'NONE', *, *, #73303, .F. ) ;
#40530 = CARTESIAN_POINT ( 'NONE',  ( 11.99999999999999822, -29.01471420065506379, -76.69515212746047439 ) ) ;
#40531 = CARTESIAN_POINT ( 'NONE',  ( 97.64999999999999147, 90.00000000000002842, 80.79249999999998977 ) ) ;
#40532 = ORIENTED_EDGE ( 'NONE', *, *, #17302, .F. ) ;
#40533 = CARTESIAN_POINT ( 'NONE',  ( -92.69370383062498320, -209.9999999999999716, 75.99031250086714806 ) ) ;
#40534 = EDGE_LOOP ( 'NONE', ( #49371, #51514, #30049, #73397 ) ) ;
#40535 = CARTESIAN_POINT ( 'NONE',  ( 10.00000000000000000, 33.17418723428333749, -17.67226234102790272 ) ) ;
#40536 = COLOUR_RGB ( '', 0.40784314, 0.44705882, 0.49803922) ;
#40537 = FACE_OUTER_BOUND ( 'NONE', #50098, .T. ) ;
#40538 = LINE ( 'NONE', #63485, #3898 ) ;
#40539 = VERTEX_POINT ( 'NONE', #72484 ) ;
#40540 = AXIS2_PLACEMENT_3D ( 'NONE', #22053, #16417, #11504 ) ;
#40541 = VERTEX_POINT ( 'NONE', #37559 ) ;
#40542 = CARTESIAN_POINT ( 'NONE',  ( 0.000000000000000000, 20.41045688087824317, 72.35160999960824313 ) ) ;
#40543 = CIRCLE ( 'NONE', #54969, 77.49899999999999523 ) ;
#40544 = FACE_OUTER_BOUND ( 'NONE', #31648, .T. ) ;
#40545 = CARTESIAN_POINT ( 'NONE',  ( 97.30629616937498838, 91.33154071421968467, 84.93322916753379559 ) ) ;
#40546 = CONICAL_SURFACE ( 'NONE', #4548, 15.39727592608509177, 1.361356816555577609 ) ;
#40547 = CARTESIAN_POINT ( 'NONE',  ( 0.000000000000000000, 12.42422080174638310, 35.38097989696515810 ) ) ;
#40548 = CARTESIAN_POINT ( 'NONE',  ( -92.34999999999995168, 88.47002178664756400, 75.65958333333333030 ) ) ;
#40549 = CARTESIAN_POINT ( 'NONE',  ( 11.99999999999999822, -68.27212725128298132, 31.46837873494953541 ) ) ;
#40550 = CARTESIAN_POINT ( 'NONE',  ( 97.64999999999999147, -209.9999999999999716, 88.41249999999999432 ) ) ;
#40551 = DIRECTION ( 'NONE',  ( -1.000000000000000000, 0.000000000000000000, 0.000000000000000000 ) ) ;
#40552 = CARTESIAN_POINT ( 'NONE',  ( 3.667169054266697703, 3.656261651251516032, -0.8603634151101352545 ) ) ;
#40553 = DIRECTION ( 'NONE',  ( 0.000000000000000000, 0.000000000000000000, -1.000000000000000000 ) ) ;
#40554 = ADVANCED_FACE ( 'NONE', ( #20987 ), #67231, .F. ) ;
#40555 = CARTESIAN_POINT ( 'NONE',  ( 92.35000000000005116, 88.47002178664747873, 78.62291666666668277 ) ) ;
#40556 = EDGE_CURVE ( 'NONE', #1655, #65945, #31147, .T. ) ;
#40557 = LINE ( 'NONE', #384, #20536 ) ;
#40558 = FACE_OUTER_BOUND ( 'NONE', #5594, .T. ) ;
#40559 = DIRECTION ( 'NONE',  ( 0.000000000000000000, 0.000000000000000000, 1.000000000000000000 ) ) ;
#40560 = EDGE_CURVE ( 'NONE', #62877, #52333, #33510, .T. ) ;
#40561 = CIRCLE ( 'NONE', #46572, 16.00000000000000000 ) ;
#40562 = VECTOR ( 'NONE', #57408, 1000.000000000000000 ) ;
#40563 = B_SPLINE_CURVE_WITH_KNOTS ( 'NONE', 1,
 ( #60435, #36368 ),
 .UNSPECIFIED., .F., .F.,
 ( 2, 2 ),
 ( 0.000000000000000000, 1.000000000000000000 ),
 .UNSPECIFIED. ) ;
#40564 = ADVANCED_FACE ( 'NONE', ( #37187 ), #8610, .F. ) ;
#40565 = CIRCLE ( 'NONE', #50151, 16.00000000000000000 ) ;
#40566 = VECTOR ( 'NONE', #55713, 1000.000000000000000 ) ;
#40567 = ORIENTED_EDGE ( 'NONE', *, *, #60062, .F. ) ;
#40568 = AXIS2_PLACEMENT_3D ( 'NONE', #56097, #16243, #28255 ) ;
#40569 = DIRECTION ( 'NONE',  ( -1.000000000000000000, 0.000000000000000000, 0.000000000000000000 ) ) ;
#40570 = CYLINDRICAL_SURFACE ( 'NONE', #5946, 16.00000000000000000 ) ;
#40571 = SURFACE_STYLE_FILL_AREA ( #2527 ) ;
#40572 = DIRECTION ( 'NONE',  ( -1.000000000000000000, -0.000000000000000000, 0.000000000000000000 ) ) ;
#40573 = ADVANCED_FACE ( 'NONE', ( #73971 ), #46158, .T. ) ;
#40574 = DIRECTION ( 'NONE',  ( -1.000000000000000000, 0.000000000000000000, 0.000000000000000000 ) ) ;
#40575 = CARTESIAN_POINT ( 'NONE',  ( 95.00000000000000000, -212.6630814284392557, 84.24531250086715772 ) ) ;
#40576 = ORIENTED_EDGE ( 'NONE', *, *, #72713, .F. ) ;
#40577 = ORIENTED_EDGE ( 'NONE', *, *, #18607, .F. ) ;
#40578 = DIRECTION ( 'NONE',  ( 0.000000000000000000, 0.1564344650402311743, -0.9876883405951377704 ) ) ;
#40579 = ORIENTED_EDGE ( 'NONE', *, *, #15510, .T. ) ;
#40580 = ADVANCED_FACE ( 'NONE', ( #56709 ), #50296, .T. ) ;
#40581 = CARTESIAN_POINT ( 'NONE',  ( -97.64997259622820991, -208.4700059650725450, 79.86645724064025842 ) ) ;
#40582 = CARTESIAN_POINT ( 'NONE',  ( 97.30629616937498838, -208.6684592857803295, 76.04322916753380923 ) ) ;
#40583 = VECTOR ( 'NONE', #56320, 1000.000000000000000 ) ;
#40585 = ORIENTED_EDGE ( 'NONE', *, *, #61102, .T. ) ;
#40584 = EDGE_CURVE ( 'NONE', #26097, #23361, #44685, .T. ) ;
#40586 = EDGE_CURVE ( 'NONE', #23763, #68521, #17911, .T. ) ;
#40587 = CARTESIAN_POINT ( 'NONE',  ( 97.30629616937498838, -208.6684592857803011, 81.91697916753381037 ) ) ;
#40588 = VECTOR ( 'NONE', #19730, 1000.000000000000000 ) ;
#40589 = CIRCLE ( 'NONE', #33379, 37.49900000000001654 ) ;
#40590 = ORIENTED_EDGE ( 'NONE', *, *, #25407, .F. ) ;
#40591 = CARTESIAN_POINT ( 'NONE',  ( 18.80329974962065265, -105.8248132807389084, 5.500000000000000000 ) ) ;
#40592 = ORIENTED_EDGE ( 'NONE', *, *, #35560, .F. ) ;
#40593 = EDGE_CURVE ( 'NONE', #14702, #44780, #62352, .T. ) ;
#40594 = EDGE_CURVE ( 'NONE', #56929, #45497, #6846, .T. ) ;
#40595 = VERTEX_POINT ( 'NONE', #22868 ) ;
#40596 = DIRECTION ( 'NONE',  ( -1.000000000000000000, -0.000000000000000000, -0.000000000000000000 ) ) ;
#40597 = CIRCLE ( 'NONE', #8172, 37.49900000000001654 ) ;
#40598 = CARTESIAN_POINT ( 'NONE',  ( 97.64999999999999147, -209.9999999999999716, 90.00000000000000000 ) ) ;
#40599 = VECTOR ( 'NONE', #38435, 1000.000000000000114 ) ;
#40600 = ORIENTED_EDGE ( 'NONE', *, *, #47858, .T. ) ;
#40601 = CARTESIAN_POINT ( 'NONE',  ( -3.000000000000000000, -19.89357724625003598, 12.59942793731059574 ) ) ;
#40602 = CARTESIAN_POINT ( 'NONE',  ( 97.64999999999999147, -209.9999999999999716, 85.95187500173430806 ) ) ;
#40603 = ORIENTED_EDGE ( 'NONE', *, *, #3502, .F. ) ;
#40604 = CARTESIAN_POINT ( 'NONE',  ( 0.000000000000000000, 41.76106447765580043, -62.50884508063379741 ) ) ;
#40605 = EDGE_CURVE ( 'NONE', #32327, #14220, #51557, .T. ) ;
#40606 = ORIENTED_EDGE ( 'NONE', *, *, #6039, .T. ) ;
#40607 = CARTESIAN_POINT ( 'NONE',  ( 5.000000000000000000, -1.472375319565264684, -0.9369361380397587258 ) ) ;
#40608 = ORIENTED_EDGE ( 'NONE', *, *, #67495, .T. ) ;
#40609 = EDGE_CURVE ( 'NONE', #34470, #58261, #41963, .T. ) ;
#40610 = ORIENTED_EDGE ( 'NONE', *, *, #28020, .F. ) ;
#40611 = VERTEX_POINT ( 'NONE', #57435 ) ;
#40612 = DIRECTION ( 'NONE',  ( 0.000000000000000000, 0.000000000000000000, 1.000000000000000000 ) ) ;
#40613 = DIRECTION ( 'NONE',  ( 0.000000000000000000, 0.000000000000000000, 1.000000000000000000 ) ) ;
#40614 = ORIENTED_EDGE ( 'NONE', *, *, #27583, .T. ) ;
#40615 = AXIS2_PLACEMENT_3D ( 'NONE', #49636, #61680, #14695 ) ;
#40616 = ORIENTED_EDGE ( 'NONE', *, *, #56784, .F. ) ;
#40617 = VECTOR ( 'NONE', #45728, 999.9999999999998863 ) ;
#40618 = ORIENTED_EDGE ( 'NONE', *, *, #59641, .T. ) ;
#40619 = CARTESIAN_POINT ( 'NONE',  ( 97.65000000000004832, -211.5299782133523934, 76.29458333333333542 ) ) ;
#40620 = FACE_OUTER_BOUND ( 'NONE', #7144, .T. ) ;
#40621 = VECTOR ( 'NONE', #65930, 1000.000000000000000 ) ;
#40622 = AXIS2_PLACEMENT_3D ( 'NONE', #10790, #33713, #39363 ) ;
#40623 = CARTESIAN_POINT ( 'NONE',  ( -92.35000000000005116, 91.52997821335253548, 87.83041666666666458 ) ) ;
#40624 = ORIENTED_EDGE ( 'NONE', *, *, #61188, .T. ) ;
#40625 = CARTESIAN_POINT ( 'NONE',  ( 96.66078690017486963, 88.39975348990186887, 74.64190636928353229 ) ) ;
#40626 = MECHANICAL_DESIGN_GEOMETRIC_PRESENTATION_REPRESENTATION (  '', ( #56244 ), #7011 ) ;
#40627 = VERTEX_POINT ( 'NONE', #51791 ) ;
#40628 = DIRECTION ( 'NONE',  ( -0.000000000000000000, -0.000000000000000000, 1.000000000000000000 ) ) ;
#40629 = CARTESIAN_POINT ( 'NONE',  ( -96.15314808468747287, -208.0026889286704943, 86.99697916753380866 ) ) ;
#40630 = ORIENTED_EDGE ( 'NONE', *, *, #27426, .F. ) ;
#40631 = CARTESIAN_POINT ( 'NONE',  ( -97.64999999999996305, -211.5299782133524218, 79.33729166840096525 ) ) ;
#40632 = FACE_OUTER_BOUND ( 'NONE', #12333, .T. ) ;
#40633 = DIRECTION ( 'NONE',  ( -0.000000000000000000, -0.000000000000000000, 1.000000000000000000 ) ) ;
#40634 = CARTESIAN_POINT ( 'NONE',  ( -97.30629616937495996, -209.9999999999999716, 77.57781250086713953 ) ) ;
#40635 = CARTESIAN_POINT ( 'NONE',  ( 97.64999999999999147, 90.00000000000002842, 90.00000000000000000 ) ) ;
#40636 = DIRECTION ( 'NONE',  ( -0.000000000000000000, -0.000000000000000000, -1.000000000000000000 ) ) ;
#40637 = CARTESIAN_POINT ( 'NONE',  ( 0.000000000000000000, 0.000000000000000000, -44.99999999999998579 ) ) ;
#40638 = DIRECTION ( 'NONE',  ( -1.000000000000000000, 0.000000000000000000, 0.000000000000000000 ) ) ;
#40639 = CYLINDRICAL_SURFACE ( 'NONE', #2003, 31.99999999999999289 ) ;
#40640 = CARTESIAN_POINT ( 'NONE',  ( -92.69370383062502583, 91.33154071421968467, 77.94822916753381037 ) ) ;
#40641 = DIRECTION ( 'NONE',  ( 0.000000000000000000, -0.5000000000000046629, 0.8660254037844359321 ) ) ;
#40642 = DIRECTION ( 'NONE',  ( 1.000000000000000000, 0.000000000000000000, 0.000000000000000000 ) ) ;
#40643 = CIRCLE ( 'NONE', #52590, 0.5999999999999928724 ) ;
#40644 = ORIENTED_EDGE ( 'NONE', *, *, #21695, .F. ) ;
#40645 = FACE_OUTER_BOUND ( 'NONE', #32423, .T. ) ;
#40646 = CIRCLE ( 'NONE', #31020, 12.49999999999999645 ) ;
#40647 = CIRCLE ( 'NONE', #8211, 82.00000000000000000 ) ;
#40648 = EDGE_CURVE ( 'NONE', #72033, #51387, #69091, .T. ) ;
#40649 = CARTESIAN_POINT ( 'NONE',  ( 93.67500000000001137, -207.7050326799711968, 89.33854166840096411 ) ) ;
#40650 = LINE ( 'NONE', #63599, #61066 ) ;
#40652 = AXIS2_PLACEMENT_3D ( 'NONE', #66978, #54960, #67355 ) ;
#40651 = DIRECTION ( 'NONE',  ( -2.603472992746261562E-14, -2.546204323184492723E-14, 1.000000000000000000 ) ) ;
#40653 = EDGE_CURVE ( 'NONE', #56198, #43284, #40509, .T. ) ;
#40654 = DIRECTION ( 'NONE',  ( -1.000000000000000000, -0.000000000000000000, -0.000000000000000000 ) ) ;
#40655 = DIRECTION ( 'NONE',  ( 0.000000000000000000, -1.156482317317870936E-15, -1.000000000000000000 ) ) ;
#40656 = CARTESIAN_POINT ( 'NONE',  ( -92.69370383062498320, -211.3315407142195852, 76.73114583420048973 ) ) ;
#40657 = AXIS2_PLACEMENT_3D ( 'NONE', #8388, #60277, #22257 ) ;
#40658 = EDGE_CURVE ( 'NONE', #48987, #16386, #11929, .T. ) ;
#40659 = ADVANCED_FACE ( 'NONE', ( #17212 ), #62731, .F. ) ;
#40660 = DIRECTION ( 'NONE',  ( 0.000000000000000000, 0.000000000000000000, -1.000000000000000000 ) ) ;
#40661 = ORIENTED_EDGE ( 'NONE', *, *, #47490, .T. ) ;
#40662 = DIRECTION ( 'NONE',  ( -1.000000000000000000, -0.000000000000000000, -0.000000000000000000 ) ) ;
#40663 = DIRECTION ( 'NONE',  ( 0.000000000000000000, 0.000000000000000000, -1.000000000000000000 ) ) ;
#40664 = DIRECTION ( 'NONE',  ( 0.000000000000000000, 0.9781476007338043566, -0.2079116908177651712 ) ) ;
#40665 = DIRECTION ( 'NONE',  ( 0.000000000000000000, 0.000000000000000000, 1.000000000000000000 ) ) ;
#40666 = CIRCLE ( 'NONE', #37062, 3.000000000000000000 ) ;
#40667 = ADVANCED_FACE ( 'NONE', ( #10452 ), #57073, .T. ) ;
#40669 = CARTESIAN_POINT ( 'NONE',  ( 10.00000000000000000, -27.75498641678764855, 31.52238457039589647 ) ) ;
#40668 = AXIS2_PLACEMENT_3D ( 'NONE', #37266, #3071, #60569 ) ;
#40670 = EDGE_CURVE ( 'NONE', #66432, #33851, #22109, .T. ) ;
#40671 = ORIENTED_EDGE ( 'NONE', *, *, #1905, .F. ) ;
#40672 = AXIS2_PLACEMENT_3D ( 'NONE', #57594, #40662, #63233 ) ;
#40673 = DIRECTION ( 'NONE',  ( 1.000000000000000000, 0.000000000000000000, 0.000000000000000000 ) ) ;
#40674 = CYLINDRICAL_SURFACE ( 'NONE', #9111, 31.99999999999998579 ) ;
#40675 = ORIENTED_EDGE ( 'NONE', *, *, #54012, .T. ) ;
#40676 = AXIS2_PLACEMENT_3D ( 'NONE', #46403, #17819, #29097 ) ;
#40677 =( BOUNDED_CURVE ( )  B_SPLINE_CURVE ( 2, ( #64681, #48496, #60531, #48855, #18799, #3038, #3396 ),
 .UNSPECIFIED., .F., .F. ) 
 B_SPLINE_CURVE_WITH_KNOTS ( ( 3, 2, 2, 3 ),
 ( 0.1693384224428226559, 0.1763941385229248482, 0.1834499040638421785, 0.1905056698846566698 ),
 .UNSPECIFIED. ) 
 CURVE ( )  GEOMETRIC_REPRESENTATION_ITEM ( )  RATIONAL_B_SPLINE_CURVE ( ( 0.9999981216931748129, 0.8660263429444348127, 1.000000000000000000, 0.8660254037844387076, 1.000000000000000000, 0.8660254037844387076, 1.000000000000000000 ) ) 
 REPRESENTATION_ITEM ( '' )  );
#40678 = CARTESIAN_POINT ( 'NONE',  ( 95.00000000000000000, -207.3369185715606307, 85.03906250086714635 ) ) ;
#40679 = DIRECTION ( 'NONE',  ( -1.000000000000000000, 0.000000000000000000, 0.000000000000000000 ) ) ;
#40680 = VERTEX_POINT ( 'NONE', #73598 ) ;
#40681 = CARTESIAN_POINT ( 'NONE',  ( 10.00000000000000000, -22.74946021919153694, 29.81001611431000597 ) ) ;
#40682 = ORIENTED_EDGE ( 'NONE', *, *, #71955, .F. ) ;
#40683 = DIRECTION ( 'NONE',  ( -1.000000000000000000, -0.000000000000000000, 0.000000000000000000 ) ) ;
#40684 = ORIENTED_EDGE ( 'NONE', *, *, #63071, .T. ) ;
#40685 = EDGE_CURVE ( 'NONE', #5670, #30842, #55368, .T. ) ;
#40686 = EDGE_CURVE ( 'NONE', #10365, #8213, #47628, .T. ) ;
#40687 = CARTESIAN_POINT ( 'NONE',  ( -96.15314808468751551, 88.00268892867056536, 81.65239583420049030 ) ) ;
#40688 = ORIENTED_EDGE ( 'NONE', *, *, #67758, .F. ) ;
#40689 = ORIENTED_EDGE ( 'NONE', *, *, #35169, .F. ) ;
#40690 = EDGE_LOOP ( 'NONE', ( #46480, #26877, #42199, #72638 ) ) ;
#40691 = CARTESIAN_POINT ( 'NONE',  ( 5.000000000000000000, -27.74655509720617275, -77.16300072079690153 ) ) ;
#40692 = CIRCLE ( 'NONE', #4702, 37.49900000000000944 ) ;
#40693 = EDGE_LOOP ( 'NONE', ( #15794, #4624, #41408, #20351 ) ) ;
#40694 = EDGE_LOOP ( 'NONE', ( #27737, #20230, #30577, #43134 ) ) ;
#40695 = LINE ( 'NONE', #17387, #10829 ) ;
#40696 = VECTOR ( 'NONE', #41159, 1000.000000000000000 ) ;
#40697 = AXIS2_PLACEMENT_3D ( 'NONE', #35401, #58330, #23389 ) ;
#40698 = ORIENTED_EDGE ( 'NONE', *, *, #68139, .T. ) ;
#40699 = VECTOR ( 'NONE', #41749, 1000.000000000000114 ) ;
#40700 = VERTEX_POINT ( 'NONE', #70537 ) ;
#40701 = CARTESIAN_POINT ( 'NONE',  ( 92.69370383062498320, 88.66845928578037217, 85.25072916753379104 ) ) ;
#40702 = ORIENTED_EDGE ( 'NONE', *, *, #40586, .T. ) ;
#40703 = CARTESIAN_POINT ( 'NONE',  ( 96.15314808468750130, -211.9973110713294489, 83.50447916753381605 ) ) ;
#40704 = CARTESIAN_POINT ( 'NONE',  ( 10.00000000000000000, 25.88420570971438650, -27.13269053701069566 ) ) ;
#40705 = AXIS2_PLACEMENT_3D ( 'NONE', #67645, #43976, #54873 ) ;
#40706 = DIRECTION ( 'NONE',  ( 0.000000000000000000, 0.000000000000000000, -1.000000000000000000 ) ) ;
#40707 = DIRECTION ( 'NONE',  ( -0.000000000000000000, -0.000000000000000000, -1.000000000000000000 ) ) ;
#40708 = CONICAL_SURFACE ( 'NONE', #47887, 12.85999999999999943, 0.7853981633974482790 ) ;
#40709 = DIRECTION ( 'NONE',  ( 1.000000000000000000, 0.000000000000000000, 0.000000000000000000 ) ) ;
#40710 = CARTESIAN_POINT ( 'NONE',  ( 0.000000000000000000, 0.000000000000000000, 0.000000000000000000 ) ) ;
#40711 = CARTESIAN_POINT ( 'NONE',  ( 10.00000000000000000, 3.894527615417895383, 81.90746397400390322 ) ) ;
#40712 = CARTESIAN_POINT ( 'NONE',  ( -97.30629616937497417, -211.3315407142195852, 82.71072916753379900 ) ) ;
#40713 = CARTESIAN_POINT ( 'NONE',  ( -93.84685191531252713, 88.00268892867056536, 81.12322916753382174 ) ) ;
#40714 = ORIENTED_EDGE ( 'NONE', *, *, #64795, .T. ) ;
#40715 = CARTESIAN_POINT ( 'NONE',  ( 94.99999999999998579, 87.33691857156068750, 84.08656250086713158 ) ) ;
#40716 = ORIENTED_EDGE ( 'NONE', *, *, #14459, .T. ) ;
#40717 = CARTESIAN_POINT ( 'NONE',  ( 7.400000000000021672, 2.574426074635176821E-13, 22.90000000000042490 ) ) ;
#40718 = CARTESIAN_POINT ( 'NONE',  ( 11.99999999999999822, -66.50666863322028632, 39.78640506895582973 ) ) ;
#40719 = DIRECTION ( 'NONE',  ( 1.000000000000000000, 0.000000000000000000, 0.000000000000000000 ) ) ;
#40720 = DIRECTION ( 'NONE',  ( 1.000000000000000000, 1.427937372958405461E-15, 7.962523111839130290E-16 ) ) ;
#40721 = AXIS2_PLACEMENT_3D ( 'NONE', #14728, #3475, #9458 ) ;
#40722 = CARTESIAN_POINT ( 'NONE',  ( -96.15314808468747287, -208.0026889286704943, 85.72697916753379843 ) ) ;
#40723 = DIRECTION ( 'NONE',  ( 0.000000000000000000, -0.5224985647159380298, -0.8526401643540988395 ) ) ;
#40724 = CARTESIAN_POINT ( 'NONE',  ( 10.00000000000000000, 35.47612816024556537, -22.48208911017461631 ) ) ;
#40725 = LINE ( 'NONE', #30531, #48705 ) ;
#40726 = CARTESIAN_POINT ( 'NONE',  ( 10.00000000000000000, 27.05870788708231700, 26.08949754953034272 ) ) ;
#40727 = ORIENTED_EDGE ( 'NONE', *, *, #30915, .T. ) ;
#40728 = AXIS2_PLACEMENT_3D ( 'NONE', #49256, #60558, #72180 ) ;
#40729 = AXIS2_PLACEMENT_3D ( 'NONE', #36710, #42366, #46903 ) ;
#40730 = ORIENTED_EDGE ( 'NONE', *, *, #24363, .F. ) ;
#40731 = AXIS2_PLACEMENT_3D ( 'NONE', #49910, #20614, #61956 ) ;
#40732 = AXIS2_PLACEMENT_3D ( 'NONE', #63148, #16909, #68785 ) ;
#40733 = CARTESIAN_POINT ( 'NONE',  ( -92.35000000000005116, 91.52997821335253548, 78.30541666666668732 ) ) ;
#40734 = DIRECTION ( 'NONE',  ( 0.000000000000000000, 0.000000000000000000, 1.000000000000000000 ) ) ;
#40735 = DIRECTION ( 'NONE',  ( -0.000000000000000000, -0.000000000000000000, -1.000000000000000000 ) ) ;
#40736 = CARTESIAN_POINT ( 'NONE',  ( -92.35000000000005116, 91.52997821335253548, 79.65479166840096070 ) ) ;
#40737 = APPLICATION_CONTEXT ( 'automotive_design' ) ;
#40738 = FACE_BOUND ( 'NONE', #24259, .T. ) ;
#40739 = DIRECTION ( 'NONE',  ( 0.000000000000000000, 0.000000000000000000, 1.000000000000000000 ) ) ;
#40740 = AXIS2_PLACEMENT_3D ( 'NONE', #17101, #11087, #73854 ) ;
#40741 = ORIENTED_EDGE ( 'NONE', *, *, #19427, .T. ) ;
#40742 = CARTESIAN_POINT ( 'NONE',  ( -92.69370383062504004, 90.00000000000004263, 77.89531250086714920 ) ) ;
#40743 = ADVANCED_FACE ( 'NONE', ( #23967 ), #29956, .T. ) ;
#40744 = CARTESIAN_POINT ( 'NONE',  ( 11.99999999999999822, 16.65972982744933972, 80.28980883073764119 ) ) ;
#40745 = ADVANCED_FACE ( 'NONE', ( #19048 ), #53640, .T. ) ;
#40746 = CARTESIAN_POINT ( 'NONE',  ( 10.00000000000000000, 60.67117009219215618, -55.16347631942976193 ) ) ;
#40747 = CARTESIAN_POINT ( 'NONE',  ( 11.99999999999999822, 28.89263327155849126, -71.91182617369157981 ) ) ;
#40748 = ADVANCED_FACE ( 'NONE', ( #52906 ), #25065, .F. ) ;
#40749 = CARTESIAN_POINT ( 'NONE',  ( 10.00000000000000000, 0.000000000000000000, 0.000000000000000000 ) ) ;
#40750 = DIRECTION ( 'NONE',  ( -0.000000000000000000, -0.000000000000000000, -1.000000000000000000 ) ) ;
#40751 = CARTESIAN_POINT ( 'NONE',  ( -92.69370383062498320, -208.6684592857803011, 86.36197916753383197 ) ) ;
#40752 = EDGE_CURVE ( 'NONE', #70258, #5237, #7031, .T. ) ;
#40753 = DIRECTION ( 'NONE',  ( -1.000000000000000000, 0.000000000000000000, 0.000000000000000000 ) ) ;
#40754 = ADVANCED_FACE ( 'NONE', ( #42000 ), #61085, .F. ) ;
#40755 = CARTESIAN_POINT ( 'NONE',  ( 94.99999999999998579, 92.66308142843932671, 75.67281250086715261 ) ) ;
#40756 = VECTOR ( 'NONE', #16265, 1000.000000000000000 ) ;
#40757 = AXIS2_PLACEMENT_3D ( 'NONE', #8939, #14569, #54796 ) ;
#40758 = CARTESIAN_POINT ( 'NONE',  ( -94.99999999999997158, -212.6630814284392557, 77.26031250086714408 ) ) ;
#40759 = DIRECTION ( 'NONE',  ( 0.000000000000000000, 0.9876883405951383255, -0.1564344650402276216 ) ) ;
#40760 = ORIENTED_EDGE ( 'NONE', *, *, #9400, .F. ) ;
#40761 = CARTESIAN_POINT ( 'NONE',  ( -93.67500000000003979, 92.29496732002878900, 82.88270833506763324 ) ) ;
#40762 = CARTESIAN_POINT ( 'NONE',  ( -10.00000000000000000, 0.000000000000000000, 0.000000000000000000 ) ) ;
#40763 = AXIS2_PLACEMENT_3D ( 'NONE', #27475, #20734, #54581 ) ;
#40764 = CARTESIAN_POINT ( 'NONE',  ( -95.00000000000002842, 90.00000000000004263, 75.00000000000000000 ) ) ;
#40765 = AXIS2_PLACEMENT_3D ( 'NONE', #43178, #31494, #8195 ) ;
#40766 = FACE_BOUND ( 'NONE', #67427, .T. ) ;
#40768 = EDGE_CURVE ( 'NONE', #33637, #16056, #53654, .T. ) ;
#40767 = CARTESIAN_POINT ( 'NONE',  ( 96.15314808468748708, -208.0026889286704943, 78.63614583420047666 ) ) ;
#40769 = ORIENTED_EDGE ( 'NONE', *, *, #40825, .T. ) ;
#40770 = EDGE_CURVE ( 'NONE', #35029, #14025, #1092, .T. ) ;
#40771 = CARTESIAN_POINT ( 'NONE',  ( 10.00000000000000178, 0.000000000000000000, 12.50000000000000000 ) ) ;
#40772 = ORIENTED_EDGE ( 'NONE', *, *, #54841, .F. ) ;
#40773 = DIRECTION ( 'NONE',  ( 0.000000000000000000, -0.7604059656000369261, 0.6494480483301766638 ) ) ;
#40774 = VERTEX_POINT ( 'NONE', #29590 ) ;
#40775 = CIRCLE ( 'NONE', #3542, 82.00000000000000000 ) ;
#40776 = FACE_OUTER_BOUND ( 'NONE', #4281, .T. ) ;
#40777 = CIRCLE ( 'NONE', #57581, 12.75000000000000000 ) ;
#40778 = EDGE_CURVE ( 'NONE', #11638, #72505, #2195, .T. ) ;
#40779 = EDGE_CURVE ( 'NONE', #12946, #41342, #13050, .T. ) ;
#40780 = VECTOR ( 'NONE', #13706, 1000.000000000000000 ) ;
#40781 = VERTEX_POINT ( 'NONE', #19800 ) ;
#40782 = VERTEX_POINT ( 'NONE', #53286 ) ;
#40783 = CIRCLE ( 'NONE', #62421, 31.99999999999998934 ) ;
#40784 = VERTEX_POINT ( 'NONE', #23985 ) ;
#40785 = AXIS2_PLACEMENT_3D ( 'NONE', #11991, #34932, #57865 ) ;
#40786 = CARTESIAN_POINT ( 'NONE',  ( -93.67499999999998295, -212.2949673200287179, 77.51166666666665606 ) ) ;
#40787 = ORIENTED_EDGE ( 'NONE', *, *, #45187, .F. ) ;
#40788 = ORIENTED_EDGE ( 'NONE', *, *, #2853, .T. ) ;
#40789 = CARTESIAN_POINT ( 'NONE',  ( 96.15314808468748708, 91.99731107132950569, 84.50989583420049200 ) ) ;
#40790 = CYLINDRICAL_SURFACE ( 'NONE', #44059, 23.50000000000000355 ) ;
#40791 = VERTEX_POINT ( 'NONE', #70931 ) ;
#40792 = VERTEX_POINT ( 'NONE', #47284 ) ;
#40793 = EDGE_LOOP ( 'NONE', ( #27679, #38398, #17681, #49852 ) ) ;
#40794 = VERTEX_POINT ( 'NONE', #13787 ) ;
#40795 = LINE ( 'NONE', #11104, #56311 ) ;
#40796 = ORIENTED_EDGE ( 'NONE', *, *, #903, .T. ) ;
#40797 = CARTESIAN_POINT ( 'NONE',  ( -1.578739900520546858E-13, -3.039576855223386628E-13, -72.00000000000001421 ) ) ;
#40798 = CARTESIAN_POINT ( 'NONE',  ( 10.00000000000000000, 0.000000000000000000, 0.000000000000000000 ) ) ;
#40799 = DIRECTION ( 'NONE',  ( 0.000000000000000000, 0.3090169943749580539, -0.9510565162951500895 ) ) ;
#40800 = DIRECTION ( 'NONE',  ( 0.000000000000000000, -0.4539904997395540764, 0.8910065241883642351 ) ) ;
#40801 = CARTESIAN_POINT ( 'NONE',  ( 10.00000000000000000, 0.000000000000000000, 0.000000000000000000 ) ) ;
#40802 = DIRECTION ( 'NONE',  ( 1.000000000000000000, 0.000000000000000000, -0.000000000000000000 ) ) ;
#40803 = DIRECTION ( 'NONE',  ( 0.8541291221503265474, -0.5200609990133007177, 0.000000000000000000 ) ) ;
#40804 = ORIENTED_EDGE ( 'NONE', *, *, #65548, .T. ) ;
#40805 = CARTESIAN_POINT ( 'NONE',  ( -94.99999999999997158, -206.9400435732949575, 79.12562500173429214 ) ) ;
#40806 = EDGE_LOOP ( 'NONE', ( #63126, #34287, #48298, #29130 ) ) ;
#40807 = FACE_BOUND ( 'NONE', #33755, .T. ) ;
#40808 = EDGE_LOOP ( 'NONE', ( #67874, #48882, #18130, #51438 ) ) ;
#40810 = CARTESIAN_POINT ( 'NONE',  ( -96.32500000000001705, 92.29496732002878900, 78.54354166840096241 ) ) ;
#40809 = CARTESIAN_POINT ( 'NONE',  ( 92.34999999999999432, 88.47002178664753558, 78.70229166840096013 ) ) ;
#40811 = ORIENTED_EDGE ( 'NONE', *, *, #42973, .T. ) ;
#40812 = CARTESIAN_POINT ( 'NONE',  ( 93.84685191531248449, 88.00268892867053694, 81.01739583420049939 ) ) ;
#40813 = CARTESIAN_POINT ( 'NONE',  ( -10.90093335751250692, 1.782551537117168429E-15, 13.71399988598171049 ) ) ;
#40814 = DIRECTION ( 'NONE',  ( -1.000000000000000000, 0.000000000000000000, 0.000000000000000000 ) ) ;
#40815 = CIRCLE ( 'NONE', #32356, 37.49900000000000944 ) ;
#40816 = CARTESIAN_POINT ( 'NONE',  ( -95.00000000000002842, 93.05995642670504253, 86.74562500173429669 ) ) ;
#40817 = CARTESIAN_POINT ( 'NONE',  ( -3.000000000000000000, -22.67460108101774807, -6.353146135318215038 ) ) ;
#40818 = AXIS2_PLACEMENT_3D ( 'NONE', #53858, #13629, #67642 ) ;
#40819 = ORIENTED_EDGE ( 'NONE', *, *, #30822, .F. ) ;
#40820 = CARTESIAN_POINT ( 'NONE',  ( 97.64999999999999147, -209.9999999999999716, 76.98250000000000171 ) ) ;
#40821 = DIRECTION ( 'NONE',  ( 0.000000000000000000, 0.3090169943749479509, -0.9510565162951534202 ) ) ;
#40822 = ORIENTED_EDGE ( 'NONE', *, *, #29498, .F. ) ;
#40823 = ORIENTED_EDGE ( 'NONE', *, *, #49901, .T. ) ;
#40824 = AXIS2_PLACEMENT_3D ( 'NONE', #70799, #47873, #2436 ) ;
#40825 = EDGE_CURVE ( 'NONE', #7101, #41677, #29891, .T. ) ;
#40826 = EDGE_CURVE ( 'NONE', #58064, #9787, #58549, .T. ) ;
#40827 = LINE ( 'NONE', #65152, #9639 ) ;
#40828 = ADVANCED_FACE ( 'NONE', ( #13429, #59672 ), #31082, .F. ) ;
#40829 = CARTESIAN_POINT ( 'NONE',  ( 11.99999999999999822, -65.58780272294100655, 36.73666225445870737 ) ) ;
#40830 = DIRECTION ( 'NONE',  ( -0.000000000000000000, -0.7431448254773870277, -0.6691306063588662312 ) ) ;
#40831 = CARTESIAN_POINT ( 'NONE',  ( -92.69370383062498320, -208.6684592857803011, 79.37697916753381833 ) ) ;
#40832 = ORIENTED_EDGE ( 'NONE', *, *, #34809, .T. ) ;
#40833 = PRODUCT_DEFINITION ( 'UNKNOWN', '', #7630, #59607 ) ;
#40834 = EDGE_CURVE ( 'NONE', #25604, #6768, #48382, .T. ) ;
#40835 = FACE_OUTER_BOUND ( 'NONE', #21055, .T. ) ;
#40836 = VECTOR ( 'NONE', #22064, 1000.000000000000000 ) ;
#40837 = CIRCLE ( 'NONE', #49237, 82.00000000000000000 ) ;
#40838 = AXIS2_PLACEMENT_3D ( 'NONE', #29510, #30621, #24267 ) ;
#40839 = CARTESIAN_POINT ( 'NONE',  ( 0.000000000000000000, 16.65560815589411092, 38.55633173627015253 ) ) ;
#40840 = DIRECTION ( 'NONE',  ( 0.000000000000000000, 0.000000000000000000, 1.000000000000000000 ) ) ;
#40841 = EDGE_CURVE ( 'NONE', #57048, #16540, #53983, .T. ) ;
#40842 = DIRECTION ( 'NONE',  ( -0.000000000000000000, -0.000000000000000000, 1.000000000000000000 ) ) ;
#40843 = DIRECTION ( 'NONE',  ( -1.000000000000000000, 0.000000000000000000, 0.000000000000000000 ) ) ;
#40844 = CARTESIAN_POINT ( 'NONE',  ( 10.00000000000000000, -51.02545421589363883, 55.20638768913742922 ) ) ;
#40845 = DIRECTION ( 'NONE',  ( 0.6516173805718058487, -0.7585478161175724932, 0.000000000000000000 ) ) ;
#40846 = AXIS2_PLACEMENT_3D ( 'NONE', #38004, #48179, #20339 ) ;
#40847 = CARTESIAN_POINT ( 'NONE',  ( -97.64999999999996305, -211.5299782133524218, 85.05229166840096866 ) ) ;
#40848 = FACE_OUTER_BOUND ( 'NONE', #4482, .T. ) ;
#40849 = CARTESIAN_POINT ( 'NONE',  ( -2.499999999999997780, 8.494897427831771708, -19.01812422950394676 ) ) ;
#40850 = EDGE_CURVE ( 'NONE', #36873, #45393, #66431, .T. ) ;
#40851 = CARTESIAN_POINT ( 'NONE',  ( 92.69370383062498320, 88.66845928578035796, 88.58447916753382856 ) ) ;
#40852 = CYLINDRICAL_SURFACE ( 'NONE', #11810, 77.49899999999999523 ) ;
#40853 = DIRECTION ( 'NONE',  ( 0.000000000000000000, 0.9945218953682732899, -0.1045284632676548031 ) ) ;
#40854 = VERTEX_POINT ( 'NONE', #31819 ) ;
#40855 = DIRECTION ( 'NONE',  ( 0.000000000000000000, -0.5877852522924803536, 0.8090169943749422332 ) ) ;
#40856 = CARTESIAN_POINT ( 'NONE',  ( -95.00000000000002842, 92.66308142843932671, 75.51406250086714067 ) ) ;
#40858 = EDGE_CURVE ( 'NONE', #57250, #62567, #26182, .T. ) ;
#40857 = CARTESIAN_POINT ( 'NONE',  ( 93.84685191531249870, -208.0026889286704943, 87.63197916753379957 ) ) ;
#40859 = ADVANCED_FACE ( 'NONE', ( #67159 ), #44233, .T. ) ;
#40860 = ORIENTED_EDGE ( 'NONE', *, *, #948, .F. ) ;
#40861 = DIRECTION ( 'NONE',  ( -5.778480238264233142E-17, 1.000000000000000000, 0.000000000000000000 ) ) ;
#40862 = ORIENTED_EDGE ( 'NONE', *, *, #21755, .T. ) ;
#40863 = AXIS2_PLACEMENT_3D ( 'NONE', #31655, #13993, #21773 ) ;
#40864 = ADVANCED_BREP_SHAPE_REPRESENTATION ( '', ( #37525, #43395 ), #56652 ) ;
#40866 = CIRCLE ( 'NONE', #8455, 16.00000000000000000 ) ;
#40865 = DIRECTION ( 'NONE',  ( 0.000000000000000000, 0.000000000000000000, -1.000000000000000000 ) ) ;
#40867 = DIRECTION ( 'NONE',  ( 0.000000000000000000, -0.1045284632676436454, -0.9945218953682744001 ) ) ;
#40868 = AXIS2_PLACEMENT_3D ( 'NONE', #36832, #47746, #60165 ) ;
#40869 = ORIENTED_EDGE ( 'NONE', *, *, #20979, .F. ) ;
#40870 = EDGE_LOOP ( 'NONE', ( #12919, #21992, #31974, #57424, #1871 ) ) ;
#40871 = CARTESIAN_POINT ( 'NONE',  ( 97.30629616937498838, -208.6684592857803295, 83.18697916753382060 ) ) ;
#40872 = DIRECTION ( 'NONE',  ( -1.000000000000000000, -0.000000000000000000, 0.000000000000000000 ) ) ;
#40873 = LINE ( 'NONE', #52885, #12409 ) ;
#40874 = CARTESIAN_POINT ( 'NONE',  ( 5.000000000000000000, 1.101175676120959901, -0.7375066809288793879 ) ) ;
#40875 = LINE ( 'NONE', #40127, #71122 ) ;
#40876 = DIRECTION ( 'NONE',  ( 0.000000000000000000, 0.000000000000000000, -1.000000000000000000 ) ) ;
#40877 = CARTESIAN_POINT ( 'NONE',  ( 97.64999999999997726, -208.4700217866474645, 84.02041666666667652 ) ) ;
#40878 = VECTOR ( 'NONE', #16783, 1000.000000000000000 ) ;
#40879 = ORIENTED_EDGE ( 'NONE', *, *, #11630, .F. ) ;
#40880 = EDGE_LOOP ( 'NONE', ( #54850, #1040, #49179, #16868 ) ) ;
#40881 = ORIENTED_EDGE ( 'NONE', *, *, #62775, .F. ) ;
#40882 = EDGE_LOOP ( 'NONE', ( #23114, #61661, #47061, #13764 ) ) ;
#40883 = CYLINDRICAL_SURFACE ( 'NONE', #34624, 16.00000000000000000 ) ;
#40884 = CARTESIAN_POINT ( 'NONE',  ( -96.15314808468751551, 88.00268892867056536, 86.73239583420048859 ) ) ;
#40885 = DIRECTION ( 'NONE',  ( 0.000000000000000000, 0.000000000000000000, 1.000000000000000000 ) ) ;
#40886 = CIRCLE ( 'NONE', #4903, 31.99999999999999645 ) ;
#40887 = DIRECTION ( 'NONE',  ( -0.7273375899149793211, 0.6862798483830554463, 0.000000000000000000 ) ) ;
#40888 = CARTESIAN_POINT ( 'NONE',  ( 97.64999999999997726, -211.5299782133524502, 77.64395833506762301 ) ) ;
#40889 = CARTESIAN_POINT ( 'NONE',  ( 97.64999999999999147, 90.00000000000002842, 78.88750000000000284 ) ) ;
#40890 = VERTEX_POINT ( 'NONE', #55511 ) ;
#40891 = CARTESIAN_POINT ( 'NONE',  ( -93.67499999999998295, -212.2949673200287179, 88.38604166840097776 ) ) ;
#40892 = EDGE_CURVE ( 'NONE', #11760, #9413, #27506, .T. ) ;
#40893 = VERTEX_POINT ( 'NONE', #55881 ) ;
#40894 = CARTESIAN_POINT ( 'NONE',  ( 10.00000000000000000, 37.58145647212453611, 0.6853352020791767529 ) ) ;
#40895 = ORIENTED_EDGE ( 'NONE', *, *, #19374, .F. ) ;
#40896 = CARTESIAN_POINT ( 'NONE',  ( -96.32500000000001705, 92.29496732002878900, 88.70354166840097321 ) ) ;
#40897 =( BOUNDED_CURVE ( )  B_SPLINE_CURVE ( 2, ( #47565, #22897, #35536 ),
 .UNSPECIFIED., .F., .F. ) 
 B_SPLINE_CURVE_WITH_KNOTS ( ( 3, 3 ),
 ( 0.000000000000000000, 2.334341054553106638E-05 ),
 .UNSPECIFIED. ) 
 CURVE ( )  GEOMETRIC_REPRESENTATION_ITEM ( )  RATIONAL_B_SPLINE_CURVE ( ( 0.9459494467533928752, 0.9464399322879002430, 0.9469490141588231547 ) ) 
 REPRESENTATION_ITEM ( '' )  );
#40898 = CARTESIAN_POINT ( 'NONE',  ( -97.30629616937501680, 90.00000000000004263, 82.81656250086714977 ) ) ;
#40899 = CARTESIAN_POINT ( 'NONE',  ( 97.30629616937498838, 91.33154071421968467, 75.40822916753381833 ) ) ;
#40900 = ORIENTED_EDGE ( 'NONE', *, *, #57563, .F. ) ;
#40901 = FACE_OUTER_BOUND ( 'NONE', #35238, .T. ) ;
#40902 = DIRECTION ( 'NONE',  ( 0.000000000000000000, -1.000000000000000000, 0.000000000000000000 ) ) ;
#40903 = CARTESIAN_POINT ( 'NONE',  ( 95.00000000000000000, -209.9999999999999716, 90.00000000000000000 ) ) ;
#40904 = CARTESIAN_POINT ( 'NONE',  ( -93.67499999999998295, -207.7050326799711968, 86.05770833506763040 ) ) ;
#40905 = EDGE_LOOP ( 'NONE', ( #50218, #55973, #47534, #55884 ) ) ;
#40906 = DIRECTION ( 'NONE',  ( 1.000000000000000000, 0.000000000000000000, -0.000000000000000000 ) ) ;
#40907 = CARTESIAN_POINT ( 'NONE',  ( -92.69370383062498320, -211.3315407142195852, 77.20739583420046870 ) ) ;
#40908 = ORIENTED_EDGE ( 'NONE', *, *, #33505, .F. ) ;
#40909 = ORIENTED_EDGE ( 'NONE', *, *, #42973, .F. ) ;
#40910 = EDGE_CURVE ( 'NONE', #1244, #57811, #15663, .T. ) ;
#40911 = DIRECTION ( 'NONE',  ( 0.000000000000000000, -0.000000000000000000, -1.000000000000000000 ) ) ;
#40912 = ADVANCED_FACE ( 'NONE', ( #60786 ), #26558, .F. ) ;
#40913 = ORIENTED_EDGE ( 'NONE', *, *, #44292, .F. ) ;
#40914 = DIRECTION ( 'NONE',  ( -1.000000000000000000, -0.000000000000000000, 0.000000000000000000 ) ) ;
#40915 = LINE ( 'NONE', #7797, #30520 ) ;
#40916 = ORIENTED_EDGE ( 'NONE', *, *, #5448, .F. ) ;
#40917 = CARTESIAN_POINT ( 'NONE',  ( -93.84685191531247028, -211.9973110713294489, 89.37822916753381719 ) ) ;
#40918 = VERTEX_POINT ( 'NONE', #37855 ) ;
#40919 = CARTESIAN_POINT ( 'NONE',  ( -94.99999999999997158, -206.9400435732949575, 81.58624999999999261 ) ) ;
#40920 = CARTESIAN_POINT ( 'NONE',  ( -16.06301359042743115, -102.7814171781257357, -5.500000000000000000 ) ) ;
#40921 = ORIENTED_EDGE ( 'NONE', *, *, #791, .F. ) ;
#40922 = ADVANCED_FACE ( 'NONE', ( #20557 ), #38212, .F. ) ;
#40923 = EDGE_CURVE ( 'NONE', #11059, #69197, #7117, .T. ) ;
#40924 = EDGE_LOOP ( 'NONE', ( #13500, #24771, #170, #32519 ) ) ;
#40925 = AXIS2_PLACEMENT_3D ( 'NONE', #14931, #43157, #55901 ) ;
#40926 = DIRECTION ( 'NONE',  ( 0.6516173805718078471, -0.7585478161175706058, 0.000000000000000000 ) ) ;
#40927 = VECTOR ( 'NONE', #52756, 1000.000000000000000 ) ;
#40928 = DIRECTION ( 'NONE',  ( 0.000000000000000000, 0.000000000000000000, 1.000000000000000000 ) ) ;
#40929 = CARTESIAN_POINT ( 'NONE',  ( 92.69370383062498320, 88.66845928578035796, 85.88572916753381037 ) ) ;
#40930 = DIRECTION ( 'NONE',  ( -1.000000000000000000, -0.000000000000000000, -0.000000000000000000 ) ) ;
#40931 = DIRECTION ( 'NONE',  ( -1.000000000000000000, -0.000000000000000000, -0.000000000000000000 ) ) ;
#40932 = FACE_OUTER_BOUND ( 'NONE', #47786, .T. ) ;
#40933 = CARTESIAN_POINT ( 'NONE',  ( 12.00000000000000000, 23.49999999999999645, 1.499999999999995337 ) ) ;
#40934 = CARTESIAN_POINT ( 'NONE',  ( 4.999999999999999112, 10.41901085202135491, -40.68715046381917944 ) ) ;
#40935 = CARTESIAN_POINT ( 'NONE',  ( 10.00000000000000000, -12.42422080174614862, -35.38097989696524337 ) ) ;
#40936 = DIRECTION ( 'NONE',  ( -1.000000000000000000, -0.000000000000000000, -0.000000000000000000 ) ) ;
#40937 = EDGE_CURVE ( 'NONE', #18134, #46588, #20920, .T. ) ;
#40938 = DIRECTION ( 'NONE',  ( 0.000000000000000000, -0.1564344650402170744, -0.9876883405951398798 ) ) ;
#40939 = AXIS2_PLACEMENT_3D ( 'NONE', #23353, #6074, #51164 ) ;
#40940 = CARTESIAN_POINT ( 'NONE',  ( -3.000000000000000000, 3.673940397442059868E-16, -25.03750572909317285 ) ) ;
#40941 = CARTESIAN_POINT ( 'NONE',  ( -97.30629616937501680, 88.66845928578038638, 89.06072916753382174 ) ) ;
#40942 = VECTOR ( 'NONE', #58462, 1000.000000000000000 ) ;
#40943 = CARTESIAN_POINT ( 'NONE',  ( 0.000000000000000000, 0.000000000000000000, 0.000000000000000000 ) ) ;
#40944 = AXIS2_PLACEMENT_3D ( 'NONE', #50774, #50021, #55682 ) ;
#40945 = AXIS2_PLACEMENT_3D ( 'NONE', #25305, #66273, #48952 ) ;
#40947 = ADVANCED_FACE ( 'NONE', ( #32563 ), #66785, .T. ) ;
#40946 = CYLINDRICAL_SURFACE ( 'NONE', #27631, 31.99999999999998579 ) ;
#40948 = EDGE_CURVE ( 'NONE', #58541, #53812, #55132, .T. ) ;
#40949 = ORIENTED_EDGE ( 'NONE', *, *, #34014, .T. ) ;
#40950 = CARTESIAN_POINT ( 'NONE',  ( 15.00000000000000000, -3.948201729842355068, -23.21447184625292692 ) ) ;
#40951 = EDGE_CURVE ( 'NONE', #1255, #45686, #22751, .T. ) ;
#40952 = DIRECTION ( 'NONE',  ( -0.000000000000000000, -0.000000000000000000, 1.000000000000000000 ) ) ;
#40953 = CARTESIAN_POINT ( 'NONE',  ( 92.35000000046504454, -210.0000309987310061, 83.09538598081256566 ) ) ;
#40954 = FACE_OUTER_BOUND ( 'NONE', #70543, .T. ) ;
#40955 = CARTESIAN_POINT ( 'NONE',  ( -95.00000000000002842, 86.94004357329504273, 77.53812500173428646 ) ) ;
#40956 = DIRECTION ( 'NONE',  ( 1.000000000000000000, 1.427937372958405461E-15, 7.962523111839130290E-16 ) ) ;
#40957 = CARTESIAN_POINT ( 'NONE',  ( 97.30629616937498838, -209.9999999999999716, 85.03906250086714635 ) ) ;
#40958 = ORIENTED_EDGE ( 'NONE', *, *, #52699, .T. ) ;
#40959 = ORIENTED_EDGE ( 'NONE', *, *, #50479, .F. ) ;
#40960 = CYLINDRICAL_SURFACE ( 'NONE', #71621, 31.99999999999997868 ) ;
#40961 = VERTEX_POINT ( 'NONE', #72419 ) ;
#40962 = CARTESIAN_POINT ( 'NONE',  ( -3.000000000000000000, -11.95096189432345390, 23.69967320028757385 ) ) ;
#40963 = CARTESIAN_POINT ( 'NONE',  ( 97.30629616937498838, -211.3315407142195852, 76.57239583420046358 ) ) ;
#40964 = VERTEX_POINT ( 'NONE', #60064 ) ;
#40965 = CARTESIAN_POINT ( 'NONE',  ( 92.69370383062501162, -211.3315407142195852, 79.05947916753382287 ) ) ;
#40966 = AXIS2_PLACEMENT_3D ( 'NONE', #41180, #40430, #29503 ) ;
#40967 = ORIENTED_EDGE ( 'NONE', *, *, #45099, .F. ) ;
#40968 = CYLINDRICAL_SURFACE ( 'NONE', #20315, 77.49899999999999523 ) ;
#40969 = ORIENTED_EDGE ( 'NONE', *, *, #47541, .F. ) ;
#40970 = AXIS2_PLACEMENT_3D ( 'NONE', #31103, #24006, #70208 ) ;
#40971 = ORIENTED_EDGE ( 'NONE', *, *, #22571, .T. ) ;
#40972 = CARTESIAN_POINT ( 'NONE',  ( 92.35000000003287823, -209.9999916080746516, 86.90410584365268676 ) ) ;
#40973 = PRESENTATION_STYLE_ASSIGNMENT (( #48081 ) ) ;
#40974 = CYLINDRICAL_SURFACE ( 'NONE', #73739, 82.00000000000000000 ) ;
#40975 = ORIENTED_EDGE ( 'NONE', *, *, #26965, .T. ) ;
#40976 = DIRECTION ( 'NONE',  ( 0.000000000000000000, -0.8090169943749508930, 0.5877852522924683631 ) ) ;
#40977 = CARTESIAN_POINT ( 'NONE',  ( 92.35000000000000853, -209.9999999999999716, 85.63437500173431260 ) ) ;
#40978 = CARTESIAN_POINT ( 'NONE',  ( 94.26574316504957096, 85.91408486779583598, 74.64692065633562379 ) ) ;
#40979 = ORIENTED_EDGE ( 'NONE', *, *, #723, .F. ) ;
#40980 = DIRECTION ( 'NONE',  ( 0.000000000000000000, -0.4539904997395350361, -0.8910065241883738940 ) ) ;
#40981 = EDGE_CURVE ( 'NONE', #5747, #8743, #43869, .T. ) ;
#40982 = VERTEX_POINT ( 'NONE', #8541 ) ;
#40983 = ORIENTED_EDGE ( 'NONE', *, *, #17233, .F. ) ;
#40984 = CARTESIAN_POINT ( 'NONE',  ( 5.000000000000000000, -1.349638343847295419, -0.8687551798607463516 ) ) ;
#40985 = ORIENTED_EDGE ( 'NONE', *, *, #41310, .T. ) ;
#40986 = CARTESIAN_POINT ( 'NONE',  ( 93.67499999999998295, 92.29496732002878900, 84.89354166840095672 ) ) ;
#40987 = ORIENTED_EDGE ( 'NONE', *, *, #55670, .T. ) ;
#40988 =( NAMED_UNIT ( * ) SI_UNIT ( $, .STERADIAN. ) SOLID_ANGLE_UNIT ( ) );
#40989 = EDGE_LOOP ( 'NONE', ( #43106, #60075, #2346, #1150, #59349 ) ) ;
#40990 = CARTESIAN_POINT ( 'NONE',  ( 0.000000000000000000, -73.72996012237429397, -14.67089635893794508 ) ) ;
#40991 = AXIS2_PLACEMENT_3D ( 'NONE', #12871, #65144, #13978 ) ;
#40992 = DIRECTION ( 'NONE',  ( 0.000000000000000000, 0.5224985647159500202, -0.8526401643540915121 ) ) ;
#40994 = ADVANCED_FACE ( 'NONE', ( #31455 ), #48749, .T. ) ;
#40993 = ORIENTED_EDGE ( 'NONE', *, *, #6807, .T. ) ;
#40995 = ORIENTED_EDGE ( 'NONE', *, *, #5456, .T. ) ;
#40996 = ORIENTED_EDGE ( 'NONE', *, *, #43136, .T. ) ;
#40997 = DIRECTION ( 'NONE',  ( 0.000000000000000000, 0.9876883405951383255, -0.1564344650402277048 ) ) ;
#40998 = AXIS2_PLACEMENT_3D ( 'NONE', #39366, #74309, #39743 ) ;
#40999 = EDGE_CURVE ( 'NONE', #63075, #61291, #20379, .T. ) ;
#41000 = CARTESIAN_POINT ( 'NONE',  ( 0.000000000000000000, 0.000000000000000000, 0.000000000000000000 ) ) ;
#41001 = CARTESIAN_POINT ( 'NONE',  ( -95.00000000000002842, 86.94004357329504273, 88.25374999999999659 ) ) ;
#41002 = ORIENTED_EDGE ( 'NONE', *, *, #56090, .T. ) ;
#41003 = FACE_OUTER_BOUND ( 'NONE', #27068, .T. ) ;
#41004 = ORIENTED_EDGE ( 'NONE', *, *, #40594, .T. ) ;
#41005 = DIRECTION ( 'NONE',  ( -0.000000000000000000, -0.000000000000000000, 1.000000000000000000 ) ) ;
#41006 = CARTESIAN_POINT ( 'NONE',  ( -92.69370383062498320, -209.9999999999999716, 81.70531250086713726 ) ) ;
#41007 = VERTEX_POINT ( 'NONE', #33299 ) ;
#41008 = CARTESIAN_POINT ( 'NONE',  ( 11.99999999999999822, -33.71516098798685590, -74.74816331893465815 ) ) ;
#41009 = CARTESIAN_POINT ( 'NONE',  ( 10.00000000000000000, 0.000000000000000000, 0.000000000000000000 ) ) ;
#41010 = CARTESIAN_POINT ( 'NONE',  ( 97.65000000000000568, -208.4700217866474645, 87.83041666666669300 ) ) ;
#41011 = CARTESIAN_POINT ( 'NONE',  ( -93.84685191531247028, -211.9973110713294489, 77.78947916753381264 ) ) ;
#41012 = EDGE_CURVE ( 'NONE', #72033, #48661, #16778, .T. ) ;
#41013 = DIRECTION ( 'NONE',  ( -0.000000000000000000, -0.000000000000000000, 1.000000000000000000 ) ) ;
#41014 = DIRECTION ( 'NONE',  ( 0.000000000000000000, 0.000000000000000000, -1.000000000000000000 ) ) ;
#41015 = DIRECTION ( 'NONE',  ( 0.000000000000000000, 0.000000000000000000, -1.000000000000000000 ) ) ;
#41016 = CARTESIAN_POINT ( 'NONE',  ( 95.00000000000000000, -209.9999999999999716, 90.00000000000000000 ) ) ;
#41017 = CARTESIAN_POINT ( 'NONE',  ( -3.000000000000000000, 3.673940397442059868E-16, 0.000000000000000000 ) ) ;
#41018 = CARTESIAN_POINT ( 'NONE',  ( 10.00000000000000000, 58.39081064771751528, 50.95692526931350841 ) ) ;
#41019 = CARTESIAN_POINT ( 'NONE',  ( -93.84685191531254134, 91.99731107132950569, 78.00114583420048575 ) ) ;
#41020 = DIRECTION ( 'NONE',  ( 0.000000000000000000, 0.8660254037844359321, 0.5000000000000046629 ) ) ;
#41021 = CARTESIAN_POINT ( 'NONE',  ( 10.00000000000000000, 74.65491531819118620, 23.16904090965733332 ) ) ;
#41022 = EDGE_CURVE ( 'NONE', #28741, #64000, #52088, .T. ) ;
#41023 = VERTEX_POINT ( 'NONE', #29147 ) ;
#41024 = ADVANCED_FACE ( 'NONE', ( #69023 ), #67222, .T. ) ;
#41025 = CARTESIAN_POINT ( 'NONE',  ( 10.00000000000000000, 10.41901085202135668, -40.68715046381917944 ) ) ;
#41026 = COLOUR_RGB ( '', 0.72549020, 0.75294118, 0.79215686) ;
#41027 = AXIS2_PLACEMENT_3D ( 'NONE', #26734, #26372, #16580 ) ;
#41028 = VECTOR ( 'NONE', #25838, 1000.000000000000000 ) ;
#41029 = EDGE_CURVE ( 'NONE', #71661, #22641, #44615, .T. ) ;
#41030 = CARTESIAN_POINT ( 'NONE',  ( 10.00000000000000000, -35.53030884539077050, -12.26510123303296851 ) ) ;
#41031 = PLANE ( 'NONE',  #5811 ) ;
#41032 = FACE_OUTER_BOUND ( 'NONE', #47551, .T. ) ;
#41033 = DIRECTION ( 'NONE',  ( 1.000000000000000000, 0.000000000000000000, 0.000000000000000000 ) ) ;
#41034 = VECTOR ( 'NONE', #29709, 1000.000000000000000 ) ;
#41035 = DIRECTION ( 'NONE',  ( -1.000000000000000000, -0.000000000000000000, -0.000000000000000000 ) ) ;
#41036 = CARTESIAN_POINT ( 'NONE',  ( -94.99999999999997158, -207.3369185715606307, 76.30781250086715772 ) ) ;
#41037 = VECTOR ( 'NONE', #62651, 1000.000000000000000 ) ;
#41038 = DIRECTION ( 'NONE',  ( -1.000000000000000000, 0.000000000000000000, -0.000000000000000000 ) ) ;
#41039 = EDGE_CURVE ( 'NONE', #24232, #35666, #62418, .T. ) ;
#41040 = ORIENTED_EDGE ( 'NONE', *, *, #43558, .F. ) ;
#41041 = CARTESIAN_POINT ( 'NONE',  ( 90.00000000000001421, -204.9999999999999716, 90.00000000000000000 ) ) ;
#41042 = CARTESIAN_POINT ( 'NONE',  ( 10.00000000000000000, -27.13269053701114331, 25.88420570971391754 ) ) ;
#41043 = CARTESIAN_POINT ( 'NONE',  ( 0.000000000000000000, -0.8261519478436571973, 77.49459641780886443 ) ) ;
#41044 = CARTESIAN_POINT ( 'NONE',  ( 11.99999999999999822, -63.18004540533059554, 44.88180994100355292 ) ) ;
#41045 = CIRCLE ( 'NONE', #23078, 77.49900000000000944 ) ;
#41046 = DIRECTION ( 'NONE',  ( 1.000000000000000000, 0.000000000000000000, -0.000000000000000000 ) ) ;
#41047 = ORIENTED_EDGE ( 'NONE', *, *, #65305, .F. ) ;
#41048 = CARTESIAN_POINT ( 'NONE',  ( 0.000000000000000000, -77.19088730480527261, 6.903761155837504049 ) ) ;
#41049 = DIRECTION ( 'NONE',  ( -1.000000000000000000, 0.000000000000000000, -0.000000000000000000 ) ) ;
#41050 = ORIENTED_EDGE ( 'NONE', *, *, #47043, .T. ) ;
#41051 = CARTESIAN_POINT ( 'NONE',  ( 92.69370383062501162, -211.3315407142195852, 84.61572916753380014 ) ) ;
#41052 = CYLINDRICAL_SURFACE ( 'NONE', #44350, 42.00000000000000000 ) ;
#41053 = ORIENTED_EDGE ( 'NONE', *, *, #50984, .T. ) ;
#41054 = CARTESIAN_POINT ( 'NONE',  ( 0.000000000000000000, -26.08949754953005495, -27.05870788708258701 ) ) ;
#41055 = VERTEX_POINT ( 'NONE', #73901 ) ;
#41056 = CARTESIAN_POINT ( 'NONE',  ( 0.000000000000000000, -12.93880638057369659, 76.41127070299266677 ) ) ;
#41057 = ORIENTED_EDGE ( 'NONE', *, *, #27490, .F. ) ;
#41058 = CARTESIAN_POINT ( 'NONE',  ( -97.30629616937501680, 90.00000000000004263, 79.00656250086716170 ) ) ;
#41059 = EDGE_LOOP ( 'NONE', ( #69090, #12763, #47899, #9646 ) ) ;
#41060 = ORIENTED_EDGE ( 'NONE', *, *, #12449, .F. ) ;
#41061 = DIRECTION ( 'NONE',  ( -1.000000000000000000, 0.000000000000000000, 0.000000000000000000 ) ) ;
#41062 = ORIENTED_EDGE ( 'NONE', *, *, #1387, .T. ) ;
#41063 = LINE ( 'NONE', #28375, #10097 ) ;
#41064 = CARTESIAN_POINT ( 'NONE',  ( -11.69999999999999929, 0.000000000000000000, 0.000000000000000000 ) ) ;
#41065 = ORIENTED_EDGE ( 'NONE', *, *, #61962, .F. ) ;
#41067 = FACE_OUTER_BOUND ( 'NONE', #46889, .T. ) ;
#41066 = PRODUCT_DEFINITION_SHAPE ( 'NONE', 'NONE',  #74358 ) ;
#41068 = ORIENTED_EDGE ( 'NONE', *, *, #60288, .T. ) ;
#41069 = CARTESIAN_POINT ( 'NONE',  ( 92.35000000000000853, -209.9999999999999716, 80.55437500173430010 ) ) ;
#41070 = VERTEX_POINT ( 'NONE', #67907 ) ;
#41071 = EDGE_CURVE ( 'NONE', #48479, #27645, #50601, .T. ) ;
#41072 = VECTOR ( 'NONE', #30075, 1000.000000000000000 ) ;
#41073 = EDGE_CURVE ( 'NONE', #3179, #12067, #48019, .T. ) ;
#41074 = ORIENTED_EDGE ( 'NONE', *, *, #17986, .T. ) ;
#41075 = ORIENTED_EDGE ( 'NONE', *, *, #5186, .F. ) ;
#41076 = CARTESIAN_POINT ( 'NONE',  ( 97.30629616937498838, -209.9999999999999716, 81.07031250086714635 ) ) ;
#41077 = SHAPE_DEFINITION_REPRESENTATION ( #3170, #54059 ) ;
#41078 = CARTESIAN_POINT ( 'NONE',  ( -97.65000000000003411, -208.4700217866475214, 76.61208333333333087 ) ) ;
#41079 = EDGE_CURVE ( 'NONE', #20786, #17939, #69588, .T. ) ;
#41081 = CARTESIAN_POINT ( 'NONE',  ( 0.000000000000000000, -62.50884508063453637, 41.76106447765467777 ) ) ;
#41080 = CIRCLE ( 'NONE', #8662, 16.00000000000000000 ) ;
#41082 = DIRECTION ( 'NONE',  ( 0.000000000000000000, 0.8526401643540897357, 0.5224985647159527957 ) ) ;
#41083 = CARTESIAN_POINT ( 'NONE',  ( 0.000000000000000000, 62.20884554314085335, -46.21855187248562657 ) ) ;
#41084 = CARTESIAN_POINT ( 'NONE',  ( 0.000000000000000000, 0.000000000000000000, 0.000000000000000000 ) ) ;
#41085 = EDGE_CURVE ( 'NONE', #19782, #63727, #35988, .T. ) ;
#41086 = CARTESIAN_POINT ( 'NONE',  ( 97.64999999999999147, -209.9999999999999716, 76.34749999999999659 ) ) ;
#41087 = CARTESIAN_POINT ( 'NONE',  ( -97.30629616937497417, -208.6684592857803011, 83.87489583420047268 ) ) ;
#41088 = CARTESIAN_POINT ( 'NONE',  ( -97.30629616937501680, 91.33154071421968467, 81.49364583420047836 ) ) ;
#41089 = VERTEX_POINT ( 'NONE', #22799 ) ;
#41090 = CARTESIAN_POINT ( 'NONE',  ( 92.69370383062498320, 91.33154071421968467, 85.14489583420048291 ) ) ;
#41091 = VECTOR ( 'NONE', #24249, 1000.000000000000000 ) ;
#41092 = EDGE_CURVE ( 'NONE', #41316, #44409, #37179, .T. ) ;
#41093 = VERTEX_POINT ( 'NONE', #28788 ) ;
#41094 = DIRECTION ( 'NONE',  ( 0.000000000000000000, 0.8090169943749433434, -0.5877852522924786882 ) ) ;
#41095 = CARTESIAN_POINT ( 'NONE',  ( 0.000000000000000000, 0.000000000000000000, -44.99999999999998579 ) ) ;
#41096 = LINE ( 'NONE', #17773, #60247 ) ;
#41097 = DIRECTION ( 'NONE',  ( 0.000000000000000000, 0.000000000000000000, -1.000000000000000000 ) ) ;
#41098 = DIRECTION ( 'NONE',  ( -1.000000000000000000, 0.000000000000000000, 0.000000000000000000 ) ) ;
#41099 = CARTESIAN_POINT ( 'NONE',  ( -97.30629616937497417, -208.6684592857803295, 85.14489583420045449 ) ) ;
#41100 = CARTESIAN_POINT ( 'NONE',  ( 30.50000000000000000, -120.0000000000000000, 2.500000000000000000 ) ) ;
#41101 = CARTESIAN_POINT ( 'NONE',  ( -3.000000000000000000, 23.59884966291521380, 12.14883922797262805 ) ) ;
#41102 = DIRECTION ( 'NONE',  ( -1.000000000000000000, 0.000000000000000000, -0.000000000000000000 ) ) ;
#41103 = VECTOR ( 'NONE', #1747, 1000.000000000000000 ) ;
#41104 = CARTESIAN_POINT ( 'NONE',  ( 11.59999999999999787, 1.420590287010929336E-15, 52.00000000000002132 ) ) ;
#41105 = ORIENTED_EDGE ( 'NONE', *, *, #28414, .T. ) ;
#41106 = ORIENTED_EDGE ( 'NONE', *, *, #42762, .T. ) ;
#41107 = CARTESIAN_POINT ( 'NONE',  ( -93.67500000000003979, 92.29496732002878900, 78.35833333333333428 ) ) ;
#41108 = DIRECTION ( 'NONE',  ( 0.000000000000000000, -1.000000000000000000, 0.000000000000000000 ) ) ;
#41109 = CARTESIAN_POINT ( 'NONE',  ( -95.00000000000002842, 92.66308142843932671, 86.94406250086714749 ) ) ;
#41110 = CARTESIAN_POINT ( 'NONE',  ( 92.34999999999993747, -208.4700217866474929, 81.05708333333332405 ) ) ;
#41111 = CYLINDRICAL_SURFACE ( 'NONE', #62611, 42.00000000000000000 ) ;
#41112 = LINE ( 'NONE', #36197, #40927 ) ;
#41113 = DIRECTION ( 'NONE',  ( -0.000000000000000000, -0.5000000000000003331, -0.8660254037844384856 ) ) ;
#41114 = EDGE_LOOP ( 'NONE', ( #14400, #32278, #37257, #19121 ) ) ;
#41115 = CARTESIAN_POINT ( 'NONE',  ( -93.84685191531254134, 91.99731107132950569, 79.27114583420046756 ) ) ;
#41116 = CARTESIAN_POINT ( 'NONE',  ( 6.250000000000005329, 0.000000000000000000, 0.000000000000000000 ) ) ;
#41117 = EDGE_CURVE ( 'NONE', #4950, #73972, #16792, .T. ) ;
#41118 = ADVANCED_FACE ( 'NONE', ( #46090 ), #17507, .T. ) ;
#41119 = DIRECTION ( 'NONE',  ( -1.000000000000000000, -0.000000000000000000, -0.000000000000000000 ) ) ;
#41120 = CARTESIAN_POINT ( 'NONE',  ( 10.00000000000000000, 21.53537804866126137, -30.80686688396986028 ) ) ;
#41121 = DIRECTION ( 'NONE',  ( 1.000000000000000000, -0.000000000000000000, -0.000000000000000000 ) ) ;
#41122 = CARTESIAN_POINT ( 'NONE',  ( -92.35000000000005116, 88.47002178664754979, 75.73895833506765030 ) ) ;
#41123 = CARTESIAN_POINT ( 'NONE',  ( -92.69370383062498320, -208.6684592857803011, 87.63197916753382799 ) ) ;
#41124 =( NAMED_UNIT ( * ) PLANE_ANGLE_UNIT ( ) SI_UNIT ( $, .RADIAN. ) );
#41125 = CARTESIAN_POINT ( 'NONE',  ( 15.00000000000000000, 14.60985201121729737, 18.46759930825687235 ) ) ;
#41126 = EDGE_CURVE ( 'NONE', #33969, #60251, #40437, .T. ) ;
#41127 =( BOUNDED_SURFACE ( )  B_SPLINE_SURFACE ( 1, 2, ( 
 ( #39270, #62587, #15955, #56572, #73832, #17077, #5072, #27971, #4328, #21589, #68955, #57298, #5809, #68591, #16330, #28339, #4701, #28716, #51657, #23096, #38895, #50907, #68210, #17443, #16704, #27218, #39644, #50150, #51275, #40370, #11781, #21966, #34730, #10316, #27607, #73460, #41849, #13637, #65166, #18542, #12162, #41123, #70396, #47853, #18179, #1310, #563, #64421, #58032, #41480, #19282, #57678, #53134, #12896, #13276, #18904, #64058, #42236, #7637, #47133, #23456, #35825, #64793, #12532, #2039, #40751, #7277, #36206, #47496, #30556, #30191, #6182, #24202, #29080, #52383, #35469, #59147, #70038, #1672, #24561, #58779, #6538, #53505, #46386, #35105, #24925, #70779, #69313, #17799, #69683, #52013, #63693, #29441, #933, #23820, #46760, #58399, #6897, #29815, #52767, #36570, #26403, #49688, #8752, #32402, #14003, #72614, #60633, #72259, #9113, #31667, #30925, #15117, #71515, #20402, #25307, #20013, #54612, #49332, #42971, #65907, #59521, #53868, #3867, #43713, #20759, #54972, #48602, #43355, #36948, #38056, #9478, #55345, #48235, #14385, #37333, #3496, #60271, #8006, #3136, #2415, #14747, #66636, #26028, #54254, #60985, #71143, #26761, #48954, #21122, #66990, #44070, #71884, #65533, #66275, #19647, #42593, #37701, #32032, #59896, #8381, #31299, #2779, #25667, #45940, #10972, #22251, #45571, #51183, #21875, #51561, #39925, #4981, #55717, #73735, #74114, #44818, #34263, #72986, #39547, #22625, #5349, #62873, #62494, #112, #33514, #61369, #10220, #67744, #28246, #27884, #33900, #56841, #45194, #15870, #68494, #4233, #44450, #16986, #11331, #27126, #50058, #27510, #73366, #38799, #21490, #10587, #15490, #23004, #57211, #33143, #67366, #38429, #56476, #61738, #68113, #5716, #56088, #28619, #9854, #32769, #39175, #4608, #62106, #50444, #50806, #16234, #16604, #11690, #57948, #6449, #30463, #12440, #35383, #57587, #13184, #41391, #69951, #52668, #472, #1220, #23726, #844, #53412, #46662, #58683, #53046, #40656, #52298, #69593, #18094, #23369, #46298, #30098, #1950, #41036, #63603, #40282, #6806, #36116, #29355, #69228, #63969, #35732, #58312, #68864, #35016, #6091, #29719, #64330, #41752, #24114, #47040, #34635, #59060, #24834, #47405, #7553, #51927, #17349, #18450, #7183, #12806, #1583, #64696, #24470, #70308 ),
 ( #63230, #28993, #18812, #17714, #12076, #55258, #8665, #2319, #31211, #60543, #37968, #8284, #65807, #65076, #54522, #48144, #31576, #9387, #3777, #43265, #3049, #3409, #9023, #54162, #32313, #72168, #37242, #13550, #25940, #31945, #2693, #66549, #30832, #71790, #54885, #37612, #20674, #20301, #47761, #14292, #19193, #42503, #25576, #26310, #60183, #66183, #14659, #48872, #71056, #49242, #36478, #60903, #43627, #42880, #71420, #15026, #19558, #70679, #25217, #42144, #59424, #7914, #53773, #19922, #48508, #65446, #13908, #36853, #59801, #49973, #55631, #16517, #33812, #44356, #44735, #57125, #72892, #50723, #27415, #21397, #67283, #51100, #73651, #73281, #22165, #5266, #15395, #33052, #45105, #55996, #27798, #38715, #62023, #43985, #15777, #4519, #26675, #39462, #4902, #10888, #72530, #68028, #50354, #62408, #21784, #21035, #16150, #74025, #27039, #66906, #61648, #10133, #62788, #67658, #39089, #38339, #45482, #56761, #28167, #10501, #32680, #33425, #56386, #22540, #11252, #68410, #16903, #39836, #34183, #49604, #61278, #9764, #4146, #35566, #42331, #65632, #58881, #1407, #52481, #19007, #25405, #70136, #58496, #18636, #47965, #24658, #5632, #47226, #69777, #53235, #2138, #53979, #12995, #70493, #46865, #48331, #14103, #59620, #71240, #64153, #37053, #35933, #19381, #41576, #64517, #2523, #7374, #8103, #1771, #29916, #41959, #42694, #30291, #31026, #47589, #28529, #65264, #23925, #18278, #12628, #30653, #13737, #70881, #19745, #53599, #1032, #64896, #41215, #24299, #13372, #36674, #36303, #25022, #6992, #59246, #52868, #7738, #48695, #14483, #21220, #15599, #71619, #25766, #71991, #43457, #8852, #20116, #55076, #60000, #67473, #67097, #3238, #43077, #44553, #26507, #66009, #66735, #3969, #26128, #38535, #37437, #61094, #60368, #31766, #32873, #31400, #15224, #4335, #61473, #8484, #49794, #73095, #32131, #55822, #54709, #21599, #9591, #44173, #32510, #3608, #54349, #9951, #20504, #43818, #49064, #66375, #49437, #72715, #14856, #37802, #2873, #60734, #27229, #50162, #15964, #26868, #9212, #38155, #72364, #20861, #55452, #34744, #27617, #73840, #45301, #57308, #16715, #61841, #5453, #10324, #17087, #51664, #56945, #56581, #28725, #33241, #57687, #68220, #23105, #69321, #46394, #74219, #67846, #22352, #211, #29087, #39653 ) ),
 .UNSPECIFIED., .F., .F., .F. ) 
 B_SPLINE_SURFACE_WITH_KNOTS ( ( 2, 2 ),
 ( 3, 2, 2, 2, 2, 2, 2, 2, 2, 2, 2, 2, 2, 2, 2, 2, 2, 2, 2, 2, 2, 2, 2, 2, 2, 2, 2, 2, 2, 2, 2, 2, 2, 2, 2, 2, 2, 2, 2, 2, 2, 2, 2, 2, 2, 2, 2, 2, 2, 2, 2, 2, 2, 2, 2, 2, 2, 2, 2, 2, 2, 2, 2, 2, 2, 2, 2, 2, 2, 2, 2, 2, 2, 2, 2, 2, 2, 2, 2, 2, 2, 2, 2, 2, 2, 2, 2, 2, 2, 2, 2, 2, 2, 2, 2, 2, 2, 2, 2, 2, 2, 2, 2, 2, 2, 2, 2, 2, 2, 2, 2, 2, 2, 2, 2, 2, 2, 2, 2, 2, 2, 2, 2, 2, 2, 2, 2, 2, 2, 2, 2, 2, 2, 2, 2, 2, 2, 2, 2, 2, 2, 2, 2, 3 ),
 ( 0.000000000000000000, 1.000000000000000000 ),
 ( 0.000000000000000000, 0.006944444444444444059, 0.01388888888888888812, 0.02083333333333333218, 0.02777777777777777624, 0.03472222222222222376, 0.04166666666666666435, 0.04861111111111111188, 0.05555555555555555247, 0.06250000000000000000, 0.06944444444444444753, 0.07638888888888889506, 0.08333333333333332871, 0.09027777777777777624, 0.09722222222222222376, 0.1041666666666666713, 0.1111111111111111049, 0.1180555555555555525, 0.1250000000000000000, 0.1319444444444444475, 0.1388888888888888951, 0.1458333333333333426, 0.1527777777777777901, 0.1597222222222222099, 0.1666666666666666574, 0.1736111111111111049, 0.1805555555555555525, 0.1875000000000000000, 0.1944444444444444475, 0.2013888888888888951, 0.2083333333333333426, 0.2152777777777777901, 0.2222222222222222099, 0.2291666666666666574, 0.2361111111111111049, 0.2430555555555555525, 0.2500000000000000000, 0.2569444444444444198, 0.2638888888888888951, 0.2708333333333333148, 0.2777777777777777901, 0.2847222222222222099, 0.2916666666666666852, 0.2986111111111111049, 0.3055555555555555802, 0.3125000000000000000, 0.3194444444444444198, 0.3263888888888888951, 0.3333333333333333148, 0.3402777777777777901, 0.3472222222222222099, 0.3541666666666666852, 0.3611111111111111049, 0.3680555555555555802, 0.3750000000000000000, 0.3819444444444444198, 0.3888888888888888951, 0.3958333333333333148, 0.4027777777777777901, 0.4097222222222222099, 0.4166666666666666852, 0.4236111111111111049, 0.4305555555555555802, 0.4375000000000000000, 0.4444444444444444198, 0.4513888888888888951, 0.4583333333333333148, 0.4652777777777777901, 0.4722222222222222099, 0.4791666666666666852, 0.4861111111111111049, 0.4930555555555555802, 0.5000000000000000000, 0.5069444444444444198, 0.5138888888888888395, 0.5208333333333333703, 0.5277777777777777901, 0.5347222222222222099, 0.5416666666666666297, 0.5486111111111111605, 0.5555555555555555802, 0.5625000000000000000, 0.5694444444444444198, 0.5763888888888888395, 0.5833333333333333703, 0.5902777777777777901, 0.5972222222222222099, 0.6041666666666666297, 0.6111111111111111605, 0.6180555555555555802, 0.6250000000000000000, 0.6319444444444444198, 0.6388888888888888395, 0.6458333333333333703, 0.6527777777777777901, 0.6597222222222222099, 0.6666666666666666297, 0.6736111111111111605, 0.6805555555555555802, 0.6875000000000000000, 0.6944444444444444198, 0.7013888888888888395, 0.7083333333333333703, 0.7152777777777777901, 0.7222222222222222099, 0.7291666666666666297, 0.7361111111111111605, 0.7430555555555555802, 0.7500000000000000000, 0.7569444444444444198, 0.7638888888888888395, 0.7708333333333333703, 0.7777777777777777901, 0.7847222222222222099, 0.7916666666666666297, 0.7986111111111111605, 0.8055555555555555802, 0.8125000000000000000, 0.8194444444444444198, 0.8263888888888888395, 0.8333333333333333703, 0.8402777777777777901, 0.8472222222222222099, 0.8541666666666666297, 0.8611111111111111605, 0.8680555555555555802, 0.8750000000000000000, 0.8819444444444444198, 0.8888888888888888395, 0.8958333333333333703, 0.9027777777777777901, 0.9097222222222222099, 0.9166666666666666297, 0.9236111111111111605, 0.9305555555555555802, 0.9375000000000000000, 0.9444444444444444198, 0.9513888888888888395, 0.9583333333333333703, 0.9652777777777777901, 0.9722222222222222099, 0.9791666666666666297, 0.9842226772312641092, 0.9940649040035767214 ),
 .UNSPECIFIED. ) 
 GEOMETRIC_REPRESENTATION_ITEM ( )  RATIONAL_B_SPLINE_SURFACE ( (
 ( 1.000000000000000000, 0.8660254037844387076, 1.000000000000000000, 0.8660254037844387076, 1.000000000000000000, 0.8660254037844387076, 1.000000000000000000, 0.8660254037844387076, 1.000000000000000000, 0.8660254037844387076, 1.000000000000000000, 0.8660254037844387076, 1.000000000000000000, 0.8660254037844387076, 1.000000000000000000, 0.8660254037844387076, 1.000000000000000000, 0.8660254037844387076, 1.000000000000000000, 0.8660254037844387076, 1.000000000000000000, 0.8660254037844387076, 1.000000000000000000, 0.8660254037844387076, 1.000000000000000000, 0.8660254037844387076, 1.000000000000000000, 0.8660254037844387076, 1.000000000000000000, 0.8660254037844387076, 1.000000000000000000, 0.8660254037844387076, 1.000000000000000000, 0.8660254037844387076, 1.000000000000000000, 0.8660254037844387076, 1.000000000000000000, 0.8660254037844387076, 1.000000000000000000, 0.8660254037844387076, 1.000000000000000000, 0.8660254037844387076, 1.000000000000000000, 0.8660254037844387076, 1.000000000000000000, 0.8660254037844387076, 1.000000000000000000, 0.8660254037844387076, 1.000000000000000000, 0.8660254037844387076, 1.000000000000000000, 0.8660254037844387076, 1.000000000000000000, 0.8660254037844387076, 1.000000000000000000, 0.8660254037844387076, 1.000000000000000000, 0.8660254037844387076, 1.000000000000000000, 0.8660254037844387076, 1.000000000000000000, 0.8660254037844387076, 1.000000000000000000, 0.8660254037844387076, 1.000000000000000000, 0.8660254037844387076, 1.000000000000000000, 0.8660254037844387076, 1.000000000000000000, 0.8660254037844387076, 1.000000000000000000, 0.8660254037844387076, 1.000000000000000000, 0.8660254037844387076, 1.000000000000000000, 0.8660254037844387076, 1.000000000000000000, 0.8660254037844387076, 1.000000000000000000, 0.8660254037844387076, 1.000000000000000000, 0.8660254037844387076, 1.000000000000000000, 0.8660254037844387076, 1.000000000000000000, 0.8660254037844387076, 1.000000000000000000, 0.8660254037844387076, 1.000000000000000000, 0.8660254037844387076, 1.000000000000000000, 0.8660254037844387076, 1.000000000000000000, 0.8660254037844387076, 1.000000000000000000, 0.8660254037844387076, 1.000000000000000000, 0.8660254037844387076, 1.000000000000000000, 0.8660254037844387076, 1.000000000000000000, 0.8660254037844387076, 1.000000000000000000, 0.8660254037844387076, 1.000000000000000000, 0.8660254037844387076, 1.000000000000000000, 0.8660254037844387076, 1.000000000000000000, 0.8660254037844387076, 1.000000000000000000, 0.8660254037844387076, 1.000000000000000000, 0.8660254037844387076, 1.000000000000000000, 0.8660254037844387076, 1.000000000000000000, 0.8660254037844387076, 1.000000000000000000, 0.8660254037844387076, 1.000000000000000000, 0.8660254037844387076, 1.000000000000000000, 0.8660254037844387076, 1.000000000000000000, 0.8660254037844387076, 1.000000000000000000, 0.8660254037844387076, 1.000000000000000000, 0.8660254037844387076, 1.000000000000000000, 0.8660254037844387076, 1.000000000000000000, 0.8660254037844387076, 1.000000000000000000, 0.8660254037844387076, 1.000000000000000000, 0.8660254037844387076, 1.000000000000000000, 0.8660254037844387076, 1.000000000000000000, 0.8660254037844387076, 1.000000000000000000, 0.8660254037844387076, 1.000000000000000000, 0.8660254037844387076, 1.000000000000000000, 0.8660254037844387076, 1.000000000000000000, 0.8660254037844387076, 1.000000000000000000, 0.8660254037844387076, 1.000000000000000000, 0.8660254037844387076, 1.000000000000000000, 0.8660254037844387076, 1.000000000000000000, 0.8660254037844387076, 1.000000000000000000, 0.8660254037844387076, 1.000000000000000000, 0.8660254037844387076, 1.000000000000000000, 0.8660254037844387076, 1.000000000000000000, 0.8660254037844387076, 1.000000000000000000, 0.8660254037844387076, 1.000000000000000000, 0.8660254037844387076, 1.000000000000000000, 0.8660254037844387076, 1.000000000000000000, 0.8660254037844387076, 1.000000000000000000, 0.8660254037844387076, 1.000000000000000000, 0.8660254037844387076, 1.000000000000000000, 0.8660254037844387076, 1.000000000000000000, 0.8660254037844387076, 1.000000000000000000, 0.8660254037844387076, 1.000000000000000000, 0.8660254037844387076, 1.000000000000000000, 0.8660254037844387076, 1.000000000000000000, 0.8660254037844387076, 1.000000000000000000, 0.8660254037844387076, 1.000000000000000000, 0.8660254037844387076, 1.000000000000000000, 0.8660254037844387076, 1.000000000000000000, 0.8660254037844387076, 1.000000000000000000, 0.8660254037844387076, 1.000000000000000000, 0.8660254037844387076, 1.000000000000000000, 0.8660254037844387076, 1.000000000000000000, 0.8660254037844387076, 1.000000000000000000, 0.8660254037844387076, 1.000000000000000000, 0.8660254037844387076, 1.000000000000000000, 0.8660254037844387076, 1.000000000000000000, 0.8660254037844387076, 1.000000000000000000, 0.8660254037844387076, 1.000000000000000000, 0.8660254037844387076, 1.000000000000000000, 0.8660254037844387076, 1.000000000000000000, 0.8660254037844387076, 1.000000000000000000, 0.8660254037844387076, 1.000000000000000000, 0.8660254037844387076, 1.000000000000000000, 0.8660254037844387076, 1.000000000000000000, 0.8660254037844387076, 1.000000000000000000, 0.8660254037844387076, 1.000000000000000000, 0.8660254037844387076, 1.000000000000000000, 0.8660254037844387076, 1.000000000000000000, 0.8660254037844387076, 1.000000000000000000, 0.8660254037844387076, 1.000000000000000000, 0.8660254037844387076, 1.000000000000000000, 0.8660254037844387076, 1.000000000000000000, 0.8660254037844387076, 1.000000000000000000, 0.8660254037844387076, 1.000000000000000000, 0.8660254037844387076, 1.000000000000000000, 0.8660254037844387076, 1.000000000000000000, 0.8660254037844387076, 1.000000000000000000, 0.8660254037844387076, 1.000000000000000000, 0.8660254037844387076, 1.000000000000000000, 0.8660254037844387076, 1.000000000000000000, 0.8660254037844387076, 1.000000000000000000, 0.8660254037844387076, 1.000000000000000000, 0.8660254037844387076, 1.000000000000000000, 0.8660254037844387076, 1.000000000000000000, 0.8660254037844387076, 1.000000000000000000, 0.8660254037844387076, 1.000000000000000000, 0.8660254037844387076, 1.000000000000000000, 0.8660254037844387076, 1.000000000000000000, 0.8660254037844387076, 1.000000000000000000, 0.8660254037844387076, 1.000000000000000000, 0.8660254037844387076, 1.000000000000000000, 0.9024577157650887083, 0.9469497795711399046, 0.9469497795711399046, 0.9469497795711399046),
 ( 1.000000000000000000, 0.8660254037844387076, 1.000000000000000000, 0.8660254037844387076, 1.000000000000000000, 0.8660254037844387076, 1.000000000000000000, 0.8660254037844387076, 1.000000000000000000, 0.8660254037844387076, 1.000000000000000000, 0.8660254037844387076, 1.000000000000000000, 0.8660254037844387076, 1.000000000000000000, 0.8660254037844387076, 1.000000000000000000, 0.8660254037844387076, 1.000000000000000000, 0.8660254037844387076, 1.000000000000000000, 0.8660254037844387076, 1.000000000000000000, 0.8660254037844387076, 1.000000000000000000, 0.8660254037844387076, 1.000000000000000000, 0.8660254037844387076, 1.000000000000000000, 0.8660254037844387076, 1.000000000000000000, 0.8660254037844387076, 1.000000000000000000, 0.8660254037844387076, 1.000000000000000000, 0.8660254037844387076, 1.000000000000000000, 0.8660254037844387076, 1.000000000000000000, 0.8660254037844387076, 1.000000000000000000, 0.8660254037844387076, 1.000000000000000000, 0.8660254037844387076, 1.000000000000000000, 0.8660254037844387076, 1.000000000000000000, 0.8660254037844387076, 1.000000000000000000, 0.8660254037844387076, 1.000000000000000000, 0.8660254037844387076, 1.000000000000000000, 0.8660254037844387076, 1.000000000000000000, 0.8660254037844387076, 1.000000000000000000, 0.8660254037844387076, 1.000000000000000000, 0.8660254037844387076, 1.000000000000000000, 0.8660254037844387076, 1.000000000000000000, 0.8660254037844387076, 1.000000000000000000, 0.8660254037844387076, 1.000000000000000000, 0.8660254037844387076, 1.000000000000000000, 0.8660254037844387076, 1.000000000000000000, 0.8660254037844387076, 1.000000000000000000, 0.8660254037844387076, 1.000000000000000000, 0.8660254037844387076, 1.000000000000000000, 0.8660254037844387076, 1.000000000000000000, 0.8660254037844387076, 1.000000000000000000, 0.8660254037844387076, 1.000000000000000000, 0.8660254037844387076, 1.000000000000000000, 0.8660254037844387076, 1.000000000000000000, 0.8660254037844387076, 1.000000000000000000, 0.8660254037844387076, 1.000000000000000000, 0.8660254037844387076, 1.000000000000000000, 0.8660254037844387076, 1.000000000000000000, 0.8660254037844387076, 1.000000000000000000, 0.8660254037844387076, 1.000000000000000000, 0.8660254037844387076, 1.000000000000000000, 0.8660254037844387076, 1.000000000000000000, 0.8660254037844387076, 1.000000000000000000, 0.8660254037844387076, 1.000000000000000000, 0.8660254037844387076, 1.000000000000000000, 0.8660254037844387076, 1.000000000000000000, 0.8660254037844387076, 1.000000000000000000, 0.8660254037844387076, 1.000000000000000000, 0.8660254037844387076, 1.000000000000000000, 0.8660254037844387076, 1.000000000000000000, 0.8660254037844387076, 1.000000000000000000, 0.8660254037844387076, 1.000000000000000000, 0.8660254037844387076, 1.000000000000000000, 0.8660254037844387076, 1.000000000000000000, 0.8660254037844387076, 1.000000000000000000, 0.8660254037844387076, 1.000000000000000000, 0.8660254037844387076, 1.000000000000000000, 0.8660254037844387076, 1.000000000000000000, 0.8660254037844387076, 1.000000000000000000, 0.8660254037844387076, 1.000000000000000000, 0.8660254037844387076, 1.000000000000000000, 0.8660254037844387076, 1.000000000000000000, 0.8660254037844387076, 1.000000000000000000, 0.8660254037844387076, 1.000000000000000000, 0.8660254037844387076, 1.000000000000000000, 0.8660254037844387076, 1.000000000000000000, 0.8660254037844387076, 1.000000000000000000, 0.8660254037844387076, 1.000000000000000000, 0.8660254037844387076, 1.000000000000000000, 0.8660254037844387076, 1.000000000000000000, 0.8660254037844387076, 1.000000000000000000, 0.8660254037844387076, 1.000000000000000000, 0.8660254037844387076, 1.000000000000000000, 0.8660254037844387076, 1.000000000000000000, 0.8660254037844387076, 1.000000000000000000, 0.8660254037844387076, 1.000000000000000000, 0.8660254037844387076, 1.000000000000000000, 0.8660254037844387076, 1.000000000000000000, 0.8660254037844387076, 1.000000000000000000, 0.8660254037844387076, 1.000000000000000000, 0.8660254037844387076, 1.000000000000000000, 0.8660254037844387076, 1.000000000000000000, 0.8660254037844387076, 1.000000000000000000, 0.8660254037844387076, 1.000000000000000000, 0.8660254037844387076, 1.000000000000000000, 0.8660254037844387076, 1.000000000000000000, 0.8660254037844387076, 1.000000000000000000, 0.8660254037844387076, 1.000000000000000000, 0.8660254037844387076, 1.000000000000000000, 0.8660254037844387076, 1.000000000000000000, 0.8660254037844387076, 1.000000000000000000, 0.8660254037844387076, 1.000000000000000000, 0.8660254037844387076, 1.000000000000000000, 0.8660254037844387076, 1.000000000000000000, 0.8660254037844387076, 1.000000000000000000, 0.8660254037844387076, 1.000000000000000000, 0.8660254037844387076, 1.000000000000000000, 0.8660254037844387076, 1.000000000000000000, 0.8660254037844387076, 1.000000000000000000, 0.8660254037844387076, 1.000000000000000000, 0.8660254037844387076, 1.000000000000000000, 0.8660254037844387076, 1.000000000000000000, 0.8660254037844387076, 1.000000000000000000, 0.8660254037844387076, 1.000000000000000000, 0.8660254037844387076, 1.000000000000000000, 0.8660254037844387076, 1.000000000000000000, 0.8660254037844387076, 1.000000000000000000, 0.8660254037844387076, 1.000000000000000000, 0.8660254037844387076, 1.000000000000000000, 0.8660254037844387076, 1.000000000000000000, 0.8660254037844387076, 1.000000000000000000, 0.8660254037844387076, 1.000000000000000000, 0.8660254037844387076, 1.000000000000000000, 0.8660254037844387076, 1.000000000000000000, 0.8660254037844387076, 1.000000000000000000, 0.8660254037844387076, 1.000000000000000000, 0.8660254037844387076, 1.000000000000000000, 0.8660254037844387076, 1.000000000000000000, 0.8660254037844387076, 1.000000000000000000, 0.8660254037844387076, 1.000000000000000000, 0.8660254037844387076, 1.000000000000000000, 0.8660254037844387076, 1.000000000000000000, 0.8660254037844387076, 1.000000000000000000, 0.8660254037844387076, 1.000000000000000000, 0.8660254037844387076, 1.000000000000000000, 0.8660254037844387076, 1.000000000000000000, 0.8660254037844387076, 1.000000000000000000, 0.8660254037844387076, 1.000000000000000000, 0.8660254037844387076, 1.000000000000000000, 0.8660254037844387076, 1.000000000000000000, 0.8660254037844387076, 1.000000000000000000, 0.8660254037844387076, 1.000000000000000000, 0.9024577157650887083, 0.9469497795711399046, 0.9469497795711399046, 0.9469497795711399046) ) ) 
 REPRESENTATION_ITEM ( '' )  SURFACE ( )  );
#41128 = CARTESIAN_POINT ( 'NONE',  ( 92.69370383062498320, 88.66845928578035796, 78.42447916753380355 ) ) ;
#41129 = CARTESIAN_POINT ( 'NONE',  ( -97.30629616937495996, -209.9999999999999716, 75.19656250086714522 ) ) ;
#41130 = DIRECTION ( 'NONE',  ( -1.000000000000000000, -0.000000000000000000, -0.000000000000000000 ) ) ;
#41131 = VERTEX_POINT ( 'NONE', #38966 ) ;
#41132 =( GEOMETRIC_REPRESENTATION_CONTEXT ( 3 ) GLOBAL_UNCERTAINTY_ASSIGNED_CONTEXT ( ( #10867 ) ) GLOBAL_UNIT_ASSIGNED_CONTEXT ( ( #72476, #60121, #8603 ) ) REPRESENTATION_CONTEXT ( 'NONE', 'WORKASPACE' ) );
#41133 = DIRECTION ( 'NONE',  ( -0.000000000000000000, -0.000000000000000000, -1.000000000000000000 ) ) ;
#41134 = DIRECTION ( 'NONE',  ( 0.000000000000000000, -0.9238795325112906243, 0.3826834323650804004 ) ) ;
#41135 = DIRECTION ( 'NONE',  ( 1.000000000000000000, -0.000000000000000000, -0.000000000000000000 ) ) ;
#41136 = CARTESIAN_POINT ( 'NONE',  ( -97.30629616937501680, 88.66845928578038638, 75.24947916753383481 ) ) ;
#41137 = CARTESIAN_POINT ( 'NONE',  ( 93.84685191531249870, -208.0026889286704943, 77.47197916753380298 ) ) ;
#41138 = ORIENTED_EDGE ( 'NONE', *, *, #31884, .T. ) ;
#41139 = AXIS2_PLACEMENT_3D ( 'NONE', #21194, #10672, #39626 ) ;
#41140 = ORIENTED_EDGE ( 'NONE', *, *, #31555, .T. ) ;
#41141 = CIRCLE ( 'NONE', #68733, 32.00000000000000000 ) ;
#41142 = DIRECTION ( 'NONE',  ( 0.000000000000000000, 0.000000000000000000, 1.000000000000000000 ) ) ;
#41143 = ORIENTED_EDGE ( 'NONE', *, *, #44257, .T. ) ;
#41144 = LINE ( 'NONE', #23846, #45404 ) ;
#41145 = VECTOR ( 'NONE', #48128, 1000.000000000000000 ) ;
#41146 = VERTEX_POINT ( 'NONE', #61900 ) ;
#41147 = ORIENTED_EDGE ( 'NONE', *, *, #26838, .F. ) ;
#41148 = ORIENTED_EDGE ( 'NONE', *, *, #12033, .T. ) ;
#41149 = DIRECTION ( 'NONE',  ( -1.000000000000000000, -0.000000000000000000, -0.000000000000000000 ) ) ;
#41150 = ORIENTED_EDGE ( 'NONE', *, *, #54751, .T. ) ;
#41151 = EDGE_LOOP ( 'NONE', ( #30158, #12019, #23476, #24952 ) ) ;
#41152 = CARTESIAN_POINT ( 'NONE',  ( 96.15314808468748708, 91.99731107132950569, 82.60489583420049087 ) ) ;
#41153 = CYLINDRICAL_SURFACE ( 'NONE', #49185, 42.00000000000000000 ) ;
#41154 = CARTESIAN_POINT ( 'NONE',  ( 95.00000000000000000, -206.9400435732949575, 75.87125000000000341 ) ) ;
#41155 = ORIENTED_EDGE ( 'NONE', *, *, #47985, .F. ) ;
#41156 = ORIENTED_EDGE ( 'NONE', *, *, #27490, .T. ) ;
#41157 = ORIENTED_EDGE ( 'NONE', *, *, #63324, .T. ) ;
#41158 = EDGE_LOOP ( 'NONE', ( #58536, #7304, #11114, #8698 ) ) ;
#41159 = DIRECTION ( 'NONE',  ( -0.000000000000000000, -0.000000000000000000, -1.000000000000000000 ) ) ;
#41160 = ORIENTED_EDGE ( 'NONE', *, *, #68411, .F. ) ;
#41161 = CARTESIAN_POINT ( 'NONE',  ( 0.000000000000000000, 0.000000000000000000, -90.00000000000001421 ) ) ;
#41162 = CARTESIAN_POINT ( 'NONE',  ( -97.64999999994212487, -210.0000112241608292, 75.47473230080855444 ) ) ;
#41163 = EDGE_CURVE ( 'NONE', #41422, #45134, #16397, .T. ) ;
#41164 = CARTESIAN_POINT ( 'NONE',  ( 92.35000000000007958, 88.47002178664747873, 83.70291666666668107 ) ) ;
#41165 = DIRECTION ( 'NONE',  ( -0.000000000000000000, -0.000000000000000000, -1.000000000000000000 ) ) ;
#41166 = CARTESIAN_POINT ( 'NONE',  ( 0.000000000000000000, -22.48208911017525580, 35.47612816024516036 ) ) ;
#41167 = CARTESIAN_POINT ( 'NONE',  ( -97.65000000000001990, 90.00000000000004263, 90.00000000000000000 ) ) ;
#41168 = CARTESIAN_POINT ( 'NONE',  ( 92.34999999999999432, 90.00000000000002842, 77.93499999999998806 ) ) ;
#41169 = ADVANCED_FACE ( 'NONE', ( #73528 ), #68657, .F. ) ;
#41170 = CARTESIAN_POINT ( 'NONE',  ( -93.67499999999998295, -207.7050326799711968, 80.34270833506762699 ) ) ;
#41171 = EDGE_LOOP ( 'NONE', ( #49374, #18113, #66783, #72686 ) ) ;
#41172 = DIRECTION ( 'NONE',  ( -0.000000000000000000, -0.000000000000000000, 1.000000000000000000 ) ) ;
#41173 = APPLICATION_CONTEXT ( 'automotive_design' ) ;
#41174 = ORIENTED_EDGE ( 'NONE', *, *, #3942, .F. ) ;
#41176 = CARTESIAN_POINT ( 'NONE',  ( -96.32500000000001705, 92.29496732002878900, 77.27354166840096639 ) ) ;
#41175 = CARTESIAN_POINT ( 'NONE',  ( 92.34999999999999432, 90.00000000000002842, 78.01437500173430806 ) ) ;
#41177 = EDGE_CURVE ( 'NONE', #26852, #24224, #63647, .T. ) ;
#41178 = ORIENTED_EDGE ( 'NONE', *, *, #59831, .F. ) ;
#41179 = CARTESIAN_POINT ( 'NONE',  ( 92.69370383062498320, 88.66845928578037217, 80.32947916753381890 ) ) ;
#41180 = CARTESIAN_POINT ( 'NONE',  ( -2.500000000000020428, -90.00000000000000000, -310.0000000000000000 ) ) ;
#41181 = DIRECTION ( 'NONE',  ( -1.000000000000000000, -0.000000000000000000, 0.000000000000000000 ) ) ;
#41182 = DIRECTION ( 'NONE',  ( 1.000000000000000000, -0.000000000000000000, 0.000000000000000000 ) ) ;
#41183 =( GEOMETRIC_REPRESENTATION_CONTEXT ( 3 ) GLOBAL_UNCERTAINTY_ASSIGNED_CONTEXT ( ( #65621 ) ) GLOBAL_UNIT_ASSIGNED_CONTEXT ( ( #38188, #8519, #48726 ) ) REPRESENTATION_CONTEXT ( 'NONE', 'WORKASPACE' ) );
#41184 = ORIENTED_EDGE ( 'NONE', *, *, #64279, .T. ) ;
#41185 = CARTESIAN_POINT ( 'NONE',  ( 0.000000000000000000, -25.60904388321925396, 6.976881207771172377 ) ) ;
#41186 = DIRECTION ( 'NONE',  ( -1.000000000000000000, -0.000000000000000000, -0.000000000000000000 ) ) ;
#41187 = EDGE_LOOP ( 'NONE', ( #54244, #48329, #36604, #9525 ) ) ;
#41188 = CIRCLE ( 'NONE', #31554, 77.49899999999999523 ) ;
#41189 = ORIENTED_EDGE ( 'NONE', *, *, #68620, .F. ) ;
#41190 = EDGE_CURVE ( 'NONE', #14148, #23851, #9594, .T. ) ;
#41191 = EDGE_CURVE ( 'NONE', #34939, #57170, #58463, .T. ) ;
#41192 = DIRECTION ( 'NONE',  ( -0.8774505977381978905, -0.4796670183876304283, 0.000000000000000000 ) ) ;
#41193 = DIRECTION ( 'NONE',  ( 0.000000000000000000, 0.000000000000000000, 1.000000000000000000 ) ) ;
#41194 = AXIS2_PLACEMENT_3D ( 'NONE', #27145, #16254, #4999 ) ;
#41195 = CARTESIAN_POINT ( 'NONE',  ( -96.15314808468747287, -208.0026889286704943, 76.36072916753381890 ) ) ;
#41196 = VERTEX_POINT ( 'NONE', #630 ) ;
#41197 = CARTESIAN_POINT ( 'NONE',  ( -92.35000000000400178, 89.99999541993113894, 76.42687486206344261 ) ) ;
#41198 = EDGE_CURVE ( 'NONE', #33146, #26720, #63662, .T. ) ;
#41200 = EDGE_CURVE ( 'NONE', #14031, #44982, #13180, .T. ) ;
#41199 = AXIS2_PLACEMENT_3D ( 'NONE', #48404, #71317, #31479 ) ;
#41201 = CARTESIAN_POINT ( 'NONE',  ( 10.00000000000000000, -81.34940948281328588, -10.30890764327469711 ) ) ;
#41202 = DIRECTION ( 'NONE',  ( -1.000000000000000000, -0.000000000000000000, -0.000000000000000000 ) ) ;
#41203 = DIRECTION ( 'NONE',  ( -1.000000000000000000, 0.000000000000000000, 0.000000000000000000 ) ) ;
#41204 = DIRECTION ( 'NONE',  ( -1.000000000000000000, 0.000000000000000000, 0.000000000000000000 ) ) ;
#41205 = FACE_OUTER_BOUND ( 'NONE', #40793, .T. ) ;
#41206 = CARTESIAN_POINT ( 'NONE',  ( 0.000000000000000000, 77.32052557432841411, 5.256550761633138613 ) ) ;
#41207 = CARTESIAN_POINT ( 'NONE',  ( 94.99999999999998579, 93.05995642670504253, 86.11062500173430578 ) ) ;
#41208 = DIRECTION ( 'NONE',  ( 1.000000000000000000, 0.000000000000000000, -0.000000000000000000 ) ) ;
#41209 = CARTESIAN_POINT ( 'NONE',  ( 10.00000000000000000, -6.736453364083817341, 36.88895765772630142 ) ) ;
#41210 = CARTESIAN_POINT ( 'NONE',  ( 96.15314808468748708, 91.99731107132950569, 86.41489583420049314 ) ) ;
#41211 = CARTESIAN_POINT ( 'NONE',  ( -92.69370383062498320, -211.3315407142195852, 87.52614583420049144 ) ) ;
#41212 = CYLINDRICAL_SURFACE ( 'NONE', #20592, 31.99999999999999289 ) ;
#41213 = ORIENTED_EDGE ( 'NONE', *, *, #27463, .F. ) ;
#41214 = CARTESIAN_POINT ( 'NONE',  ( 0.000000000000000000, 51.02545421589402252, -55.20638768913705263 ) ) ;
#41215 = CARTESIAN_POINT ( 'NONE',  ( -92.34999999999999432, -211.5299782133524502, 80.10458333333332348 ) ) ;
#41216 = CARTESIAN_POINT ( 'NONE',  ( -93.51319757292682766, 91.80467564693685745, 74.81083481226639265 ) ) ;
#41217 = CARTESIAN_POINT ( 'NONE',  ( 96.15314808468748708, -208.0026889286704943, 86.89114583420047211 ) ) ;
#41218 = ORIENTED_EDGE ( 'NONE', *, *, #32987, .F. ) ;
#41219 = AXIS2_PLACEMENT_3D ( 'NONE', #73925, #46856, #28814 ) ;
#41220 = ORIENTED_EDGE ( 'NONE', *, *, #48239, .F. ) ;
#41221 = ORIENTED_EDGE ( 'NONE', *, *, #61385, .F. ) ;
#41222 = CARTESIAN_POINT ( 'NONE',  ( 16.84844760790522145, -103.5491698323862124, -2.500000000000000000 ) ) ;
#41223 = CARTESIAN_POINT ( 'NONE',  ( 0.000000000000000000, -120.0000000000000000, 2.500000000000000000 ) ) ;
#41224 = CIRCLE ( 'NONE', #5184, 2.650000000000540812 ) ;
#41225 = ORIENTED_EDGE ( 'NONE', *, *, #34961, .F. ) ;
#41226 = ORIENTED_EDGE ( 'NONE', *, *, #74284, .F. ) ;
#41227 = EDGE_CURVE ( 'NONE', #51481, #6686, #30260, .T. ) ;
#41228 = CARTESIAN_POINT ( 'NONE',  ( 97.30629616937498838, -208.6684592857803295, 82.55197916753380127 ) ) ;
#41229 = DIRECTION ( 'NONE',  ( 1.000000000000000000, 0.000000000000000000, 0.000000000000000000 ) ) ;
#41230 = LINE ( 'NONE', #63439, #62791 ) ;
#41231 = EDGE_CURVE ( 'NONE', #12484, #60926, #59586, .T. ) ;
#41232 = VECTOR ( 'NONE', #63809, 1000.000000000000000 ) ;
#41233 = CARTESIAN_POINT ( 'NONE',  ( -92.35000000000306386, -210.0000040461925437, 77.06187486178056645 ) ) ;
#41234 = CYLINDRICAL_SURFACE ( 'NONE', #355, 0.5000000000000004441 ) ;
#41235 = AXIS2_PLACEMENT_3D ( 'NONE', #31575, #1949, #31210 ) ;
#41236 = CARTESIAN_POINT ( 'NONE',  ( 10.00000000000000000, 81.96053171279901051, 2.543863470248666658 ) ) ;
#41237 = CARTESIAN_POINT ( 'NONE',  ( 96.32499999999998863, -212.2949673200287179, 85.13166666666666060 ) ) ;
#41238 = PRODUCT_RELATED_PRODUCT_CATEGORY ( 'part', '', ( #31948 ) ) ;
#41239 = EDGE_CURVE ( 'NONE', #17937, #12034, #8363, .T. ) ;
#41240 = EDGE_LOOP ( 'NONE', ( #37284, #10309, #9806, #66577 ) ) ;
#41241 = EDGE_LOOP ( 'NONE', ( #71811, #46411, #48643, #31589 ) ) ;
#41242 = ORIENTED_EDGE ( 'NONE', *, *, #20726, .F. ) ;
#41243 = AXIS2_PLACEMENT_3D ( 'NONE', #70124, #52104, #46470 ) ;
#41244 = ORIENTED_EDGE ( 'NONE', *, *, #15339, .F. ) ;
#41246 = VECTOR ( 'NONE', #10882, 1000.000000000000000 ) ;
#41245 = CARTESIAN_POINT ( 'NONE',  ( 12.50000000000000000, -132.5000000000000000, -40.00000000000000000 ) ) ;
#41247 = CIRCLE ( 'NONE', #58046, 31.99999999999998934 ) ;
#41248 = CARTESIAN_POINT ( 'NONE',  ( -97.30629616937501680, 88.66845928578038638, 86.04447916753382231 ) ) ;
#41249 = EDGE_CURVE ( 'NONE', #55642, #47807, #60003, .T. ) ;
#41250 = FACE_OUTER_BOUND ( 'NONE', #15979, .T. ) ;
#41251 = CARTESIAN_POINT ( 'NONE',  ( -97.65000000000001990, 90.00000000000004263, 90.00000000000000000 ) ) ;
#41252 = CARTESIAN_POINT ( 'NONE',  ( 95.00000000000000000, -212.6630814284392557, 88.53156250086713897 ) ) ;
#41253 = CARTESIAN_POINT ( 'NONE',  ( 96.32499999999997442, 92.29496732002878900, 78.99333333333332519 ) ) ;
#41255 = ORIENTED_EDGE ( 'NONE', *, *, #62860, .F. ) ;
#41254 = EDGE_CURVE ( 'NONE', #65774, #33146, #10630, .T. ) ;
#41256 = CARTESIAN_POINT ( 'NONE',  ( -93.67499999999998295, -212.2949673200287179, 89.02104166840096866 ) ) ;
#41257 = ORIENTED_EDGE ( 'NONE', *, *, #42306, .T. ) ;
#41258 = FACE_OUTER_BOUND ( 'NONE', #69366, .T. ) ;
#41259 = ORIENTED_EDGE ( 'NONE', *, *, #14582, .F. ) ;
#41260 = DIRECTION ( 'NONE',  ( 0.000000000000000000, 1.000000000000000000, 3.469446951953614189E-15 ) ) ;
#41261 = EDGE_CURVE ( 'NONE', #29988, #59210, #2108, .T. ) ;
#41262 = CARTESIAN_POINT ( 'NONE',  ( 94.99999999999998579, 92.66308142843935514, 76.14906250086716000 ) ) ;
#41263 = ORIENTED_EDGE ( 'NONE', *, *, #25325, .T. ) ;
#41264 = DIRECTION ( 'NONE',  ( 0.000000000000000000, 0.000000000000000000, 1.000000000000000000 ) ) ;
#41265 = AXIS2_PLACEMENT_3D ( 'NONE', #73609, #15737, #11567 ) ;
#41266 = CARTESIAN_POINT ( 'NONE',  ( 10.00000000000000000, -22.48208911017474065, -35.47612816024548721 ) ) ;
#41267 = LINE ( 'NONE', #54030, #22161 ) ;
#41268 = DIRECTION ( 'NONE',  ( 0.000000000000000000, 1.078060571631605650E-14, 1.000000000000000000 ) ) ;
#41269 = VERTEX_POINT ( 'NONE', #41922 ) ;
#41270 = DIRECTION ( 'NONE',  ( -1.000000000000000000, -0.000000000000000000, -0.000000000000000000 ) ) ;
#41271 = CARTESIAN_POINT ( 'NONE',  ( -96.15314808468747287, -208.0026889286704943, 75.56697916753381605 ) ) ;
#41272 = ORIENTED_EDGE ( 'NONE', *, *, #72617, .T. ) ;
#41273 = ORIENTED_EDGE ( 'NONE', *, *, #42346, .T. ) ;
#41274 = CARTESIAN_POINT ( 'NONE',  ( 10.00000000000000000, -46.53671651293991118, 59.03961581697383565 ) ) ;
#41275 = ADVANCED_FACE ( 'NONE', ( #18609 ), #69378, .T. ) ;
#41276 = ADVANCED_FACE ( 'NONE', ( #46452 ), #58848, .T. ) ;
#41277 = CARTESIAN_POINT ( 'NONE',  ( 0.000000000000000000, 0.000000000000000000, -56.19999999999998863 ) ) ;
#41278 = AXIS2_PLACEMENT_3D ( 'NONE', #70730, #19235, #12849 ) ;
#41279 = DIRECTION ( 'NONE',  ( 0.9038112904824842087, -0.4279312458753000703, 0.000000000000000000 ) ) ;
#41280 = ORIENTED_EDGE ( 'NONE', *, *, #32237, .F. ) ;
#41281 = CARTESIAN_POINT ( 'NONE',  ( -93.84685191531247028, -211.9973110713294489, 88.74322916753382628 ) ) ;
#41282 = ORIENTED_EDGE ( 'NONE', *, *, #21968, .T. ) ;
#41283 = LINE ( 'NONE', #54408, #69343 ) ;
#41284 = ORIENTED_EDGE ( 'NONE', *, *, #70581, .F. ) ;
#41285 = CIRCLE ( 'NONE', #7676, 15.99999999999999822 ) ;
#41286 = CARTESIAN_POINT ( 'NONE',  ( 97.30629616937498838, 88.66845928578037217, 77.20739583420046870 ) ) ;
#41287 = VERTEX_POINT ( 'NONE', #23894 ) ;
#41288 = DIRECTION ( 'NONE',  ( 0.000000000000000000, -0.8090169943749403458, -0.5877852522924830181 ) ) ;
#41289 = FACE_OUTER_BOUND ( 'NONE', #33996, .T. ) ;
#41290 = CARTESIAN_POINT ( 'NONE',  ( 93.84685191531248449, 88.00268892867053694, 82.12864583420046927 ) ) ;
#41291 = DIRECTION ( 'NONE',  ( -1.000000000000000000, 0.000000000000000000, -0.000000000000000000 ) ) ;
#41292 = DIRECTION ( 'NONE',  ( 0.000000000000000000, 0.7604059656000277112, 0.6494480483301875440 ) ) ;
#41293 = CARTESIAN_POINT ( 'NONE',  ( -97.65000000000001990, 90.00000000000004263, 81.10999999999999943 ) ) ;
#41294 = DIRECTION ( 'NONE',  ( 0.000000000000000000, 0.000000000000000000, 1.000000000000000000 ) ) ;
#41295 = DIRECTION ( 'NONE',  ( -1.000000000000000000, 0.000000000000000000, -0.000000000000000000 ) ) ;
#41296 = CARTESIAN_POINT ( 'NONE',  ( -10.00000000000000000, 0.000000000000000000, 0.000000000000000000 ) ) ;
#41297 = CARTESIAN_POINT ( 'NONE',  ( -6.880223345695647197, -142.5202692415819854, 5.500000000000000000 ) ) ;
#41298 = CIRCLE ( 'NONE', #23275, 77.49900000000000944 ) ;
#41299 = AXIS2_PLACEMENT_3D ( 'NONE', #25021, #70880, #55450 ) ;
#41300 = CARTESIAN_POINT ( 'NONE',  ( 92.35000000000000853, -209.9999999999999716, 85.63437500173431260 ) ) ;
#41301 = CARTESIAN_POINT ( 'NONE',  ( 14.09999999999999964, 0.000000000000000000, -1.199999999999999956 ) ) ;
#41302 = CARTESIAN_POINT ( 'NONE',  ( -95.00000000000002842, 87.33691857156074434, 85.35656250086714181 ) ) ;
#41303 = AXIS2_PLACEMENT_3D ( 'NONE', #54880, #61274, #26305 ) ;
#41304 = CARTESIAN_POINT ( 'NONE',  ( 12.00000000000000000, 8.688484142253932063, -21.88630264137371384 ) ) ;
#41305 = DIRECTION ( 'NONE',  ( 2.603472992746261562E-14, 2.546204323184492723E-14, -1.000000000000000000 ) ) ;
#41306 = ORIENTED_EDGE ( 'NONE', *, *, #19104, .T. ) ;
#41307 = FACE_OUTER_BOUND ( 'NONE', #26731, .T. ) ;
#41308 = CARTESIAN_POINT ( 'NONE',  ( 92.35000000006147047, -209.9999881782113107, 76.10900611559200968 ) ) ;
#41309 = LINE ( 'NONE', #70595, #39531 ) ;
#41310 = EDGE_CURVE ( 'NONE', #49532, #24421, #17875, .T. ) ;
#41311 = CIRCLE ( 'NONE', #11312, 0.5999999999999998668 ) ;
#41312 = CARTESIAN_POINT ( 'NONE',  ( 6.000000000000000000, 80.28980883073758434, 16.65972982744962749 ) ) ;
#41313 = CARTESIAN_POINT ( 'NONE',  ( 95.00000000000000000, -207.3369185715606307, 82.65781250086715204 ) ) ;
#41314 = VERTEX_POINT ( 'NONE', #23520 ) ;
#41315 = ADVANCED_FACE ( 'NONE', ( #36640 ), #12959, .T. ) ;
#41316 = VERTEX_POINT ( 'NONE', #47562 ) ;
#41317 = EDGE_CURVE ( 'NONE', #73338, #5282, #35898, .T. ) ;
#41318 = DIRECTION ( 'NONE',  ( -1.000000000000000000, 0.000000000000000000, 0.000000000000000000 ) ) ;
#41319 = VERTEX_POINT ( 'NONE', #18971 ) ;
#41320 = CIRCLE ( 'NONE', #18505, 31.99999999999998934 ) ;
#41321 = PLANE ( 'NONE',  #36574 ) ;
#41322 =( BOUNDED_CURVE ( )  B_SPLINE_CURVE ( 2, ( #3320, #4806, #72443, #44644, #48777, #49152, #43539 ),
 .UNSPECIFIED., .F., .F. ) 
 B_SPLINE_CURVE_WITH_KNOTS ( ( 3, 2, 2, 3 ),
 ( 0.04166666666666644231, 0.04861111111111085514, 0.05555555555555525410, 0.06249999999999966693 ),
 .UNSPECIFIED. ) 
 CURVE ( )  GEOMETRIC_REPRESENTATION_ITEM ( )  RATIONAL_B_SPLINE_CURVE ( ( 1.000000000000004219, 0.8660254037844343777, 1.000000000000000000, 0.8660254037844387076, 1.000000000000000000, 0.8660254037844451469, 0.9999999999999935607 ) ) 
 REPRESENTATION_ITEM ( '' )  );
#41323 = DIRECTION ( 'NONE',  ( 1.000000000000000000, -0.000000000000000000, -0.000000000000000000 ) ) ;
#41324 = ORIENTED_EDGE ( 'NONE', *, *, #50351, .T. ) ;
#41325 = CARTESIAN_POINT ( 'NONE',  ( 96.15314808468748708, -208.0026889286704943, 78.15989583420049769 ) ) ;
#41326 = EDGE_CURVE ( 'NONE', #49856, #60856, #64862, .T. ) ;
#41327 = VERTEX_POINT ( 'NONE', #37016 ) ;
#41328 = FACE_OUTER_BOUND ( 'NONE', #31536, .T. ) ;
#41329 = ORIENTED_EDGE ( 'NONE', *, *, #37251, .T. ) ;
#41330 = ORIENTED_EDGE ( 'NONE', *, *, #22162, .T. ) ;
#41331 = DIRECTION ( 'NONE',  ( 0.000000000000000000, 0.000000000000000000, 1.000000000000000000 ) ) ;
#41332 = AXIS2_PLACEMENT_3D ( 'NONE', #27073, #31606, #66218 ) ;
#41333 = FACE_OUTER_BOUND ( 'NONE', #39855, .T. ) ;
#41334 = EDGE_LOOP ( 'NONE', ( #19524, #50485, #8675, #38595 ) ) ;
#41335 = CYLINDRICAL_SURFACE ( 'NONE', #56917, 3.299999999999983391 ) ;
#41336 = CARTESIAN_POINT ( 'NONE',  ( 93.67500000000001137, -207.7050326799711968, 86.16354166840096696 ) ) ;
#41337 = CARTESIAN_POINT ( 'NONE',  ( 97.64999999999999147, 90.00000000000002842, 89.68250000000000455 ) ) ;
#41338 = ORIENTED_EDGE ( 'NONE', *, *, #52432, .F. ) ;
#41339 = CARTESIAN_POINT ( 'NONE',  ( 94.99999999999998579, 93.05995642670504253, 84.84062500173429555 ) ) ;
#41340 = PLANE ( 'NONE',  #21279 ) ;
#41341 = VECTOR ( 'NONE', #1526, 1000.000000000000000 ) ;
#41342 = VERTEX_POINT ( 'NONE', #37768 ) ;
#41343 = ORIENTED_EDGE ( 'NONE', *, *, #37262, .T. ) ;
#41344 = CYLINDRICAL_SURFACE ( 'NONE', #61335, 31.99999999999999289 ) ;
#41345 = EDGE_CURVE ( 'NONE', #47069, #51767, #23984, .T. ) ;
#41346 = ORIENTED_EDGE ( 'NONE', *, *, #60199, .T. ) ;
#41347 = CARTESIAN_POINT ( 'NONE',  ( 97.64999999999997726, 91.52997821335252127, 84.73479166840097321 ) ) ;
#41348 = ORIENTED_EDGE ( 'NONE', *, *, #6161, .T. ) ;
#41349 = AXIS2_PLACEMENT_3D ( 'NONE', #5715, #843, #23003 ) ;
#41350 = EDGE_LOOP ( 'NONE', ( #45151, #15440, #73170, #45058 ) ) ;
#41351 = CARTESIAN_POINT ( 'NONE',  ( -18.24502636017238899, -100.7225776329765665, 5.500000000000000000 ) ) ;
#41352 = AXIS2_PLACEMENT_3D ( 'NONE', #34746, #21600, #46036 ) ;
#41353 = DIRECTION ( 'NONE',  ( -1.000000000000000000, 0.000000000000000000, 0.000000000000000000 ) ) ;
#41354 = ORIENTED_EDGE ( 'NONE', *, *, #48450, .T. ) ;
#41355 = VERTEX_POINT ( 'NONE', #15567 ) ;
#41356 = ORIENTED_EDGE ( 'NONE', *, *, #7460, .T. ) ;
#41357 = PLANE ( 'NONE',  #21702 ) ;
#41359 = CIRCLE ( 'NONE', #14947, 82.00000000000000000 ) ;
#41358 = CARTESIAN_POINT ( 'NONE',  ( 8.000000000000007105, 1.142349898368116708E-14, 6.370018489481387452E-15 ) ) ;
#41360 = CARTESIAN_POINT ( 'NONE',  ( -95.00000000000002842, 93.05995642670501411, 89.20624999999999716 ) ) ;
#41361 = ADVANCED_FACE ( 'NONE', ( #54679 ), #2488, .F. ) ;
#41362 = ORIENTED_EDGE ( 'NONE', *, *, #8199, .T. ) ;
#41363 = EDGE_CURVE ( 'NONE', #2959, #5973, #66012, .T. ) ;
#41364 = CARTESIAN_POINT ( 'NONE',  ( 5.000000000000002665, -15.33399622253423722, -80.55351364060604169 ) ) ;
#41365 = DIRECTION ( 'NONE',  ( -0.1850432970638656582, 0.9827303690289285187, 0.000000000000000000 ) ) ;
#41366 = ORIENTED_EDGE ( 'NONE', *, *, #11949, .T. ) ;
#41367 = CARTESIAN_POINT ( 'NONE',  ( 96.32499999999998863, -212.2949673200287179, 85.13166666666666060 ) ) ;
#41368 = CARTESIAN_POINT ( 'NONE',  ( -92.69370383062498320, -208.6684592857803011, 84.29822916753380468 ) ) ;
#41369 = ORIENTED_EDGE ( 'NONE', *, *, #57836, .F. ) ;
#41370 = EDGE_CURVE ( 'NONE', #20120, #45152, #49183, .T. ) ;
#41371 = CARTESIAN_POINT ( 'NONE',  ( -93.08359813425042262, 88.16968857444109631, 74.99954695036826990 ) ) ;
#41372 = DIRECTION ( 'NONE',  ( -1.000000000000000000, -0.000000000000000000, -0.000000000000000000 ) ) ;
#41373 = DIRECTION ( 'NONE',  ( 1.000000000000000000, -0.000000000000000000, -0.000000000000000000 ) ) ;
#41374 = CARTESIAN_POINT ( 'NONE',  ( -92.69370383062498320, -211.3315407142195852, 77.20739583420046870 ) ) ;
#41375 = VECTOR ( 'NONE', #8709, 1000.000000000000000 ) ;
#41376 = FACE_OUTER_BOUND ( 'NONE', #14597, .T. ) ;
#41377 = SURFACE_STYLE_USAGE ( .BOTH. , #24096 ) ;
#41378 = CARTESIAN_POINT ( 'NONE',  ( 0.000000000000000000, 17.28742895386084655, 75.54627589209950145 ) ) ;
#41379 = CARTESIAN_POINT ( 'NONE',  ( -6.782329983125267248, 10.49999999999999645, -125.0000000000000000 ) ) ;
#41380 = CARTESIAN_POINT ( 'NONE',  ( 96.32499999999998863, 87.70503267997126784, 88.30666666666665776 ) ) ;
#41381 = CARTESIAN_POINT ( 'NONE',  ( -97.30629616937501680, 88.66845928578038638, 79.53572916753380184 ) ) ;
#41382 = CARTESIAN_POINT ( 'NONE',  ( 10.00000000000000000, 37.22597642581150268, 5.202137450157037435 ) ) ;
#41383 = FACE_OUTER_BOUND ( 'NONE', #38249, .T. ) ;
#41384 = CARTESIAN_POINT ( 'NONE',  ( 11.99999999999999822, 74.65374052328660071, -8.840884882374309583 ) ) ;
#41385 = FACE_OUTER_BOUND ( 'NONE', #14329, .T. ) ;
#41386 = DIRECTION ( 'NONE',  ( -1.000000000000000000, -0.000000000000000000, -0.000000000000000000 ) ) ;
#41387 = VECTOR ( 'NONE', #73967, 1000.000000000000000 ) ;
#41388 = CARTESIAN_POINT ( 'NONE',  ( 97.64999999999999147, 90.00000000000002842, 87.14249999999999829 ) ) ;
#41389 = CARTESIAN_POINT ( 'NONE',  ( 95.73180504966251192, -212.6374485842880233, 75.02735117824599342 ) ) ;
#41390 = LINE ( 'NONE', #1219, #4018 ) ;
#41391 = CARTESIAN_POINT ( 'NONE',  ( -93.84685191531247028, -211.9973110713294489, 77.31322916753381946 ) ) ;
#41392 = PLANE ( 'NONE',  #54876 ) ;
#41393 = EDGE_LOOP ( 'NONE', ( #4760, #45805, #61030, #36522 ) ) ;
#41394 = AXIS2_PLACEMENT_3D ( 'NONE', #17640, #40572, #57133 ) ;
#41395 = CARTESIAN_POINT ( 'NONE',  ( 14.59956846177685996, -138.4757300459248484, 5.500000000000000000 ) ) ;
#41396 = AXIS2_PLACEMENT_3D ( 'NONE', #32816, #5026, #22298 ) ;
#41397 = CARTESIAN_POINT ( 'NONE',  ( -10.00000000000000000, 0.000000000000000000, 0.000000000000000000 ) ) ;
#41398 = DIRECTION ( 'NONE',  ( -1.000000000000000000, 0.000000000000000000, 0.000000000000000000 ) ) ;
#41399 = CARTESIAN_POINT ( 'NONE',  ( 89.17737905728634473, -39.70432723693593857, -5.500000000000000000 ) ) ;
#41400 = EDGE_CURVE ( 'NONE', #12406, #60338, #67062, .T. ) ;
#41401 = VECTOR ( 'NONE', #39183, 1000.000000000000000 ) ;
#41402 = EDGE_CURVE ( 'NONE', #13032, #4950, #1216, .T. ) ;
#41403 = DIRECTION ( 'NONE',  ( 0.000000000000000000, 0.000000000000000000, -1.000000000000000000 ) ) ;
#41404 = ORIENTED_EDGE ( 'NONE', *, *, #12235, .F. ) ;
#41406 = ADVANCED_FACE ( 'NONE', ( #31366 ), #20832, .T. ) ;
#41405 = CARTESIAN_POINT ( 'NONE',  ( 21.85433023846371370, -135.0628101570779620, -5.500000000000000000 ) ) ;
#41407 = SURFACE_STYLE_FILL_AREA ( #13562 ) ;
#41408 = ORIENTED_EDGE ( 'NONE', *, *, #27484, .F. ) ;
#41409 = CARTESIAN_POINT ( 'NONE',  ( 93.84685191531249870, -208.0026889286704943, 85.09197916753380753 ) ) ;
#41410 = CARTESIAN_POINT ( 'NONE',  ( 95.00000000000000000, -207.3369185715606307, 87.73781250086715033 ) ) ;
#41411 = VERTEX_POINT ( 'NONE', #54316 ) ;
#41412 = AXIS2_PLACEMENT_3D ( 'NONE', #18968, #12599, #58843 ) ;
#41413 = CARTESIAN_POINT ( 'NONE',  ( 92.69370383062501162, -209.9999999999999716, 89.80156250086714920 ) ) ;
#41414 = EDGE_CURVE ( 'NONE', #36301, #31828, #72683, .T. ) ;
#41415 = ORIENTED_EDGE ( 'NONE', *, *, #69328, .F. ) ;
#41416 = CARTESIAN_POINT ( 'NONE',  ( 0.000000000000000000, 0.000000000000000000, 0.000000000000000000 ) ) ;
#41417 = ORIENTED_EDGE ( 'NONE', *, *, #55919, .F. ) ;
#41418 = CARTESIAN_POINT ( 'NONE',  ( -97.30629616937501680, 91.33154071421968467, 80.85864583420048746 ) ) ;
#41419 = ORIENTED_EDGE ( 'NONE', *, *, #36729, .T. ) ;
#41420 = ORIENTED_EDGE ( 'NONE', *, *, #54477, .F. ) ;
#41421 = LINE ( 'NONE', #42532, #35216 ) ;
#41422 = VERTEX_POINT ( 'NONE', #3938 ) ;
#41423 = CARTESIAN_POINT ( 'NONE',  ( 97.64999999999999147, -210.0000001167898631, 84.68187499741277691 ) ) ;
#41424 = CYLINDRICAL_SURFACE ( 'NONE', #4433, 82.00000000000000000 ) ;
#41425 = EDGE_LOOP ( 'NONE', ( #13267, #5316, #18704, #54443 ) ) ;
#41426 = LINE ( 'NONE', #12840, #65832 ) ;
#41427 = EDGE_CURVE ( 'NONE', #17454, #45219, #3571, .T. ) ;
#41428 = ORIENTED_EDGE ( 'NONE', *, *, #73767, .T. ) ;
#41429 = CARTESIAN_POINT ( 'NONE',  ( 10.00000000000000000, 75.11725578898472122, -2.956366410619845730 ) ) ;
#41430 = EDGE_CURVE ( 'NONE', #55748, #35036, #51489, .T. ) ;
#41431 = ORIENTED_EDGE ( 'NONE', *, *, #53659, .F. ) ;
#41432 = ORIENTED_EDGE ( 'NONE', *, *, #8133, .T. ) ;
#41433 = ORIENTED_EDGE ( 'NONE', *, *, #2897, .F. ) ;
#41434 = CARTESIAN_POINT ( 'NONE',  ( 97.30629616937498838, -209.9999999999999716, 80.43531250086714124 ) ) ;
#41435 = CIRCLE ( 'NONE', #42620, 32.00000000000000000 ) ;
#41436 = DIRECTION ( 'NONE',  ( -1.000000000000000000, 0.000000000000000000, 0.000000000000000000 ) ) ;
#41437 = DIRECTION ( 'NONE',  ( 0.000000000000000000, 0.000000000000000000, 1.000000000000000000 ) ) ;
#41438 = DIRECTION ( 'NONE',  ( -1.000000000000000000, 0.000000000000000000, 0.000000000000000000 ) ) ;
#41439 = DIRECTION ( 'NONE',  ( -0.000000000000000000, -0.000000000000000000, 1.000000000000000000 ) ) ;
#41440 = DIRECTION ( 'NONE',  ( 0.000000000000000000, 0.000000000000000000, 1.000000000000000000 ) ) ;
#41441 = CARTESIAN_POINT ( 'NONE',  ( 92.35000000000000853, -209.9999999999999716, 76.66499999999999204 ) ) ;
#41442 = CARTESIAN_POINT ( 'NONE',  ( -97.30629616937497417, -208.6684592857803011, 85.77989583420048803 ) ) ;
#41443 = CARTESIAN_POINT ( 'NONE',  ( -97.30629616937501680, 88.66845928578038638, 81.59947916753381492 ) ) ;
#41444 = ADVANCED_FACE ( 'NONE', ( #48670, #61439 ), #32103, .T. ) ;
#41445 = ORIENTED_EDGE ( 'NONE', *, *, #70782, .F. ) ;
#41446 = EDGE_CURVE ( 'NONE', #50481, #49570, #71877, .T. ) ;
#41447 = CARTESIAN_POINT ( 'NONE',  ( 97.30629616937498838, 91.33154071421968467, 80.48822916753383083 ) ) ;
#41448 = ORIENTED_EDGE ( 'NONE', *, *, #45583, .F. ) ;
#41449 = CARTESIAN_POINT ( 'NONE',  ( -97.65000000000001990, 88.47002178664754979, 78.70229166840096013 ) ) ;
#41451 = AXIS2_PLACEMENT_3D ( 'NONE', #40829, #12968, #68661 ) ;
#41450 = FACE_OUTER_BOUND ( 'NONE', #62379, .T. ) ;
#41452 = CARTESIAN_POINT ( 'NONE',  ( 93.67500000000001137, -212.2949673200287179, 76.21520833506762926 ) ) ;
#41453 = AXIS2_PLACEMENT_3D ( 'NONE', #34973, #39881, #46254 ) ;
#41454 = CARTESIAN_POINT ( 'NONE',  ( -3.961125083139900749, -143.2122702051246677, 5.500000000000000000 ) ) ;
#41455 = DIRECTION ( 'NONE',  ( -0.000000000000000000, -0.000000000000000000, 1.000000000000000000 ) ) ;
#41456 = CARTESIAN_POINT ( 'NONE',  ( -94.99999999999997158, -207.3369185715606307, 85.03906250086714635 ) ) ;
#41457 = CARTESIAN_POINT ( 'NONE',  ( 0.000000000000000000, 68.55367621811205936, -44.99326035065983120 ) ) ;
#41458 = CARTESIAN_POINT ( 'NONE',  ( -96.32500000000001705, 87.70503267997129626, 88.91520833506763211 ) ) ;
#41459 = DIRECTION ( 'NONE',  ( 1.000000000000000000, -0.000000000000000000, -0.000000000000000000 ) ) ;
#41460 = CONICAL_SURFACE ( 'NONE', #715, 2.649999999999999467, 1.029744258676654312 ) ;
#41461 = DIRECTION ( 'NONE',  ( -1.000000000000000000, 0.000000000000000000, 0.000000000000000000 ) ) ;
#41462 = ORIENTED_EDGE ( 'NONE', *, *, #39195, .F. ) ;
#41463 = ORIENTED_EDGE ( 'NONE', *, *, #6312, .F. ) ;
#41464 = CIRCLE ( 'NONE', #69056, 82.00000000000000000 ) ;
#41465 = CARTESIAN_POINT ( 'NONE',  ( -93.67500000000003979, 87.70503267997129626, 75.60666666666665492 ) ) ;
#41466 = CYLINDRICAL_SURFACE ( 'NONE', #33133, 31.99999999999998579 ) ;
#41467 = CARTESIAN_POINT ( 'NONE',  ( -95.00000000000002842, 92.66308142843932671, 87.57906250086713840 ) ) ;
#41468 = DIRECTION ( 'NONE',  ( 0.000000000000000000, 0.000000000000000000, 1.000000000000000000 ) ) ;
#41469 = FACE_OUTER_BOUND ( 'NONE', #70175, .T. ) ;
#41470 = CARTESIAN_POINT ( 'NONE',  ( 96.32499999999998863, -207.7050326799711968, 77.80270833506763495 ) ) ;
#41471 = CARTESIAN_POINT ( 'NONE',  ( -92.35000000000010800, -208.4700217866473793, 78.30541666666667311 ) ) ;
#41472 = ORIENTED_EDGE ( 'NONE', *, *, #15971, .T. ) ;
#41473 = CARTESIAN_POINT ( 'NONE',  ( -12.75044424985852487, 0.001194404164724885897, 127.4927882439606464 ) ) ;
#41474 = CIRCLE ( 'NONE', #72680, 31.99999999999999289 ) ;
#41475 = CARTESIAN_POINT ( 'NONE',  ( 97.64999999999999147, -209.9999999999999716, 87.77749999999998920 ) ) ;
#41476 = CYLINDRICAL_SURFACE ( 'NONE', #53843, 77.49899999999999523 ) ;
#41477 = CYLINDRICAL_SURFACE ( 'NONE', #53738, 37.49900000000000233 ) ;
#41478 = VECTOR ( 'NONE', #35184, 1000.000000000000000 ) ;
#41479 = DIRECTION ( 'NONE',  ( -1.000000000000000000, 0.000000000000000000, 0.000000000000000000 ) ) ;
#41480 = CARTESIAN_POINT ( 'NONE',  ( -97.30629616937497417, -208.6684592857803011, 87.20864583420049598 ) ) ;
#41481 = DIRECTION ( 'NONE',  ( 0.000000000000000000, 0.9238795325112878487, -0.3826834323650874503 ) ) ;
#41482 = CARTESIAN_POINT ( 'NONE',  ( 92.69370383062498320, 88.66845928578035796, 75.24947916753383481 ) ) ;
#41483 = ADVANCED_FACE ( 'NONE', ( #61061 ), #65599, .T. ) ;
#41484 = CARTESIAN_POINT ( 'NONE',  ( -94.99999999999997158, -207.3369185715606307, 75.03781250086714749 ) ) ;
#41485 = DIRECTION ( 'NONE',  ( 0.000000000000000000, 0.000000000000000000, 1.000000000000000000 ) ) ;
#41486 = ORIENTED_EDGE ( 'NONE', *, *, #6809, .T. ) ;
#41487 = CARTESIAN_POINT ( 'NONE',  ( 93.67499999999999716, 87.70503267997126784, 87.64520833506762187 ) ) ;
#41488 = FACE_OUTER_BOUND ( 'NONE', #2562, .T. ) ;
#41489 = DIRECTION ( 'NONE',  ( -1.000000000000000000, -0.000000000000000000, 0.000000000000000000 ) ) ;
#41490 = CONICAL_SURFACE ( 'NONE', #34247, 3.000000000000000000, 0.9599310885968762586 ) ;
#41491 = ADVANCED_FACE ( 'NONE', ( #8816 ), #31736, .T. ) ;
#41492 = EDGE_CURVE ( 'NONE', #633, #60365, #64877, .T. ) ;
#41493 = EDGE_CURVE ( 'NONE', #28922, #52606, #16843, .T. ) ;
#41494 = CARTESIAN_POINT ( 'NONE',  ( -92.69370383062504004, 90.00000000000004263, 74.87906250086714977 ) ) ;
#41495 = CARTESIAN_POINT ( 'NONE',  ( 93.84685191531249870, -208.0026889286704943, 76.20197916753380696 ) ) ;
#41496 = ORIENTED_EDGE ( 'NONE', *, *, #60838, .F. ) ;
#41497 = EDGE_LOOP ( 'NONE', ( #69838, #33125, #43025 ) ) ;
#41498 = CARTESIAN_POINT ( 'NONE',  ( 0.000000000000000000, 31.52238457039637609, -27.75498641678709788 ) ) ;
#41499 = CIRCLE ( 'NONE', #69100, 31.99999999999998934 ) ;
#41500 = ORIENTED_EDGE ( 'NONE', *, *, #27260, .T. ) ;
#41501 = EDGE_CURVE ( 'NONE', #50412, #13574, #21947, .T. ) ;
#41502 = DIRECTION ( 'NONE',  ( -1.000000000000000000, -0.000000000000000000, 0.000000000000000000 ) ) ;
#41503 = AXIS2_PLACEMENT_3D ( 'NONE', #50955, #10736, #4368 ) ;
#41504 = ORIENTED_EDGE ( 'NONE', *, *, #32133, .F. ) ;
#41505 = CIRCLE ( 'NONE', #69156, 31.99999999999998579 ) ;
#41506 = ORIENTED_EDGE ( 'NONE', *, *, #24012, .T. ) ;
#41507 = CIRCLE ( 'NONE', #57094, 20.20000000000036522 ) ;
#41508 = VERTEX_POINT ( 'NONE', #56549 ) ;
#41509 = CARTESIAN_POINT ( 'NONE',  ( 0.000000000000000000, -80.28980883073769803, 16.65972982744905551 ) ) ;
#41510 = ORIENTED_EDGE ( 'NONE', *, *, #1266, .F. ) ;
#41511 = ADVANCED_FACE ( 'NONE', ( #17055 ), #5423, .T. ) ;
#41512 = CIRCLE ( 'NONE', #23484, 77.49899999999999523 ) ;
#41513 = VERTEX_POINT ( 'NONE', #51251 ) ;
#41514 = CARTESIAN_POINT ( 'NONE',  ( 97.30629616937498838, 91.33154071421968467, 78.74197916753382742 ) ) ;
#41515 = DIRECTION ( 'NONE',  ( -0.000000000000000000, -0.000000000000000000, -1.000000000000000000 ) ) ;
#41516 = EDGE_CURVE ( 'NONE', #72658, #31992, #4677, .T. ) ;
#41517 = CARTESIAN_POINT ( 'NONE',  ( 96.32499999999998863, -207.7050326799711968, 75.18333333333332291 ) ) ;
#41518 = ORIENTED_EDGE ( 'NONE', *, *, #7454, .F. ) ;
#41519 = ORIENTED_EDGE ( 'NONE', *, *, #50554, .T. ) ;
#41520 = ORIENTED_EDGE ( 'NONE', *, *, #45546, .T. ) ;
#41521 = LINE ( 'NONE', #18581, #1079 ) ;
#41523 = ORIENTED_EDGE ( 'NONE', *, *, #4241, .T. ) ;
#41522 = EDGE_CURVE ( 'NONE', #49623, #10745, #9471, .T. ) ;
#41524 = EDGE_CURVE ( 'NONE', #10838, #11647, #50424, .T. ) ;
#41525 = CARTESIAN_POINT ( 'NONE',  ( -95.00000000000002842, 86.94004357329504273, 87.61874999999999147 ) ) ;
#41526 = AXIS2_PLACEMENT_3D ( 'NONE', #45208, #17003, #33911 ) ;
#41527 = CYLINDRICAL_SURFACE ( 'NONE', #18259, 16.00000000000000000 ) ;
#41528 = CARTESIAN_POINT ( 'NONE',  ( 0.000000000000000000, 0.000000000000000000, 0.000000000000000000 ) ) ;
#41529 = CARTESIAN_POINT ( 'NONE',  ( 15.00000000000000000, -4.261787119644963262, 26.19803753235780164 ) ) ;
#41530 = CARTESIAN_POINT ( 'NONE',  ( 6.000000000000000000, -29.01471420065506379, -76.69515212746047439 ) ) ;
#41531 = DIRECTION ( 'NONE',  ( 1.000000000000000000, 0.000000000000000000, -0.000000000000000000 ) ) ;
#41532 = CARTESIAN_POINT ( 'NONE',  ( -93.67499999999998295, -207.7050326799711968, 79.70770833506762187 ) ) ;
#41533 = DIRECTION ( 'NONE',  ( 0.000000000000000000, -0.000000000000000000, -1.000000000000000000 ) ) ;
#41534 = EDGE_CURVE ( 'NONE', #62549, #63558, #33589, .T. ) ;
#41535 = ORIENTED_EDGE ( 'NONE', *, *, #42022, .F. ) ;
#41537 = CARTESIAN_POINT ( 'NONE',  ( -95.00000000000002842, 86.94004357329504273, 76.90312500173429555 ) ) ;
#41536 = CARTESIAN_POINT ( 'NONE',  ( 96.90829146052656995, 88.16127117233635602, 74.44346887015069569 ) ) ;
#41538 =( BOUNDED_CURVE ( )  B_SPLINE_CURVE ( 2, ( #13903, #60178, #3044, #65802, #25209, #24465, #47399 ),
 .UNSPECIFIED., .F., .F. ) 
 B_SPLINE_CURVE_WITH_KNOTS ( ( 3, 2, 2, 3 ),
 ( 0.3175094496522546383, 0.3245652148821828731, 0.3316209804230999536, 0.3386766260354857061 ),
 .UNSPECIFIED. ) 
 CURVE ( )  GEOMETRIC_REPRESENTATION_ITEM ( )  RATIONAL_B_SPLINE_CURVE ( ( 1.000000000000000000, 0.8660254037844387076, 1.000000000000000000, 0.8660254037844387076, 1.000000000000000000, 0.8660276809826341626, 0.9999954456810212777 ) ) 
 REPRESENTATION_ITEM ( '' )  );
#41539 = ORIENTED_EDGE ( 'NONE', *, *, #3087, .F. ) ;
#41540 = CARTESIAN_POINT ( 'NONE',  ( 93.84685191531248449, 91.99731107132950569, 78.90072916753382515 ) ) ;
#41541 = DIRECTION ( 'NONE',  ( 0.000000000000000000, 0.000000000000000000, 1.000000000000000000 ) ) ;
#41542 = DIRECTION ( 'NONE',  ( 0.02332147558787931590, 0.9997280174009348652, 0.000000000000000000 ) ) ;
#41543 = DIRECTION ( 'NONE',  ( 0.9227826878668540234, 0.3853207896976547087, 0.000000000000000000 ) ) ;
#41544 = EDGE_CURVE ( 'NONE', #73707, #39502, #52851, .T. ) ;
#41545 = DIRECTION ( 'NONE',  ( 0.000000000000000000, 0.000000000000000000, 1.000000000000000000 ) ) ;
#41546 = ORIENTED_EDGE ( 'NONE', *, *, #58384, .T. ) ;
#41547 = DIRECTION ( 'NONE',  ( 0.000000000000000000, 0.7071067811865486830, -0.7071067811865463515 ) ) ;
#41548 = DIRECTION ( 'NONE',  ( -1.000000000000000000, -0.000000000000000000, 0.000000000000000000 ) ) ;
#41549 = ORIENTED_EDGE ( 'NONE', *, *, #55414, .T. ) ;
#41550 = ORIENTED_EDGE ( 'NONE', *, *, #1567, .T. ) ;
#41551 = DIRECTION ( 'NONE',  ( 2.603472992745699578E-14, -2.546204323184531851E-14, 1.000000000000000000 ) ) ;
#41552 = LINE ( 'NONE', #46460, #43878 ) ;
#41553 = DIRECTION ( 'NONE',  ( 1.000000000000000000, -0.000000000000000000, -0.000000000000000000 ) ) ;
#41554 = CARTESIAN_POINT ( 'NONE',  ( -92.69370383062498320, -209.9999999999999716, 78.68906250086715204 ) ) ;
#41555 =( BOUNDED_CURVE ( )  B_SPLINE_CURVE ( 2, ( #45857, #62026, #27 ),
 .UNSPECIFIED., .F., .F. ) 
 B_SPLINE_CURVE_WITH_KNOTS ( ( 3, 3 ),
 ( 0.9791666666666669627, 0.9841647806526082620 ),
 .UNSPECIFIED. ) 
 CURVE ( )  GEOMETRIC_REPRESENTATION_ITEM ( )  RATIONAL_B_SPLINE_CURVE ( ( 0.9999999999999935607, 0.9035746763527574554, 0.9459494432169380795 ) ) 
 REPRESENTATION_ITEM ( '' )  );
#41556 = ORIENTED_EDGE ( 'NONE', *, *, #45247, .F. ) ;
#41557 = CARTESIAN_POINT ( 'NONE',  ( 10.00000000000000000, 72.35160999960844208, -20.41045688087747223 ) ) ;
#41558 = FACE_OUTER_BOUND ( 'NONE', #6032, .T. ) ;
#41559 = CYLINDRICAL_SURFACE ( 'NONE', #32199, 15.70000000000000284 ) ;
#41560 = VECTOR ( 'NONE', #41439, 1000.000000000000000 ) ;
#41561 = CARTESIAN_POINT ( 'NONE',  ( 21.07894319797337346, -103.8699611390234878, 2.500000000000000000 ) ) ;
#41562 = LINE ( 'NONE', #69040, #12424 ) ;
#41563 = CARTESIAN_POINT ( 'NONE',  ( 0.000000000000000000, 0.000000000000000000, 0.000000000000000000 ) ) ;
#41564 = AXIS2_PLACEMENT_3D ( 'NONE', #71597, #2121, #60347 ) ;
#41565 = DIRECTION ( 'NONE',  ( 0.000000000000000000, -0.2079116908177664480, -0.9781476007338041345 ) ) ;
#41566 = CARTESIAN_POINT ( 'NONE',  ( -97.64999999999996305, -209.9999999999999716, 84.99937500173429328 ) ) ;
#41567 = CARTESIAN_POINT ( 'NONE',  ( -97.64999999999996305, -209.9999999999999716, 78.57000000000000739 ) ) ;
#41568 = FACE_OUTER_BOUND ( 'NONE', #55170, .T. ) ;
#41569 = AXIS2_PLACEMENT_3D ( 'NONE', #31651, #54958, #3481 ) ;
#41570 = AXIS2_PLACEMENT_3D ( 'NONE', #72514, #21014, #43967 ) ;
#41571 = CARTESIAN_POINT ( 'NONE',  ( 94.99999999999998579, 92.66308142843932671, 83.29281250086715715 ) ) ;
#41572 = CARTESIAN_POINT ( 'NONE',  ( -92.69370383062498320, -211.3315407142195852, 88.16114583420048234 ) ) ;
#41573 = LINE ( 'NONE', #2135, #27786 ) ;
#41574 = EDGE_LOOP ( 'NONE', ( #402, #44765, #25257, #6121 ) ) ;
#41575 = CARTESIAN_POINT ( 'NONE',  ( 0.000000000000000000, 44.99326035066149387, -68.55367621811095091 ) ) ;
#41576 = CARTESIAN_POINT ( 'NONE',  ( -92.34999999999999432, -211.5299782133524502, 81.37458333333333371 ) ) ;
#41577 = EDGE_CURVE ( 'NONE', #17670, #5506, #26432, .T. ) ;
#41578 = CARTESIAN_POINT ( 'NONE',  ( -92.69370383062505425, 88.66845928578038638, 75.93739583420050110 ) ) ;
#41579 = EDGE_CURVE ( 'NONE', #45314, #36429, #68478, .T. ) ;
#41580 = AXIS2_PLACEMENT_3D ( 'NONE', #54900, #3793, #3423 ) ;
#41581 = EDGE_CURVE ( 'NONE', #11006, #47167, #50125, .T. ) ;
#41582 = EDGE_CURVE ( 'NONE', #19435, #13842, #16308, .T. ) ;
#41583 = CARTESIAN_POINT ( 'NONE',  ( 97.30629616937498838, -208.6684592857803011, 88.10822916753380696 ) ) ;
#41584 = EDGE_LOOP ( 'NONE', ( #31692, #36865, #42301, #24595, #45608 ) ) ;
#41585 = ORIENTED_EDGE ( 'NONE', *, *, #30735, .F. ) ;
#41586 = ORIENTED_EDGE ( 'NONE', *, *, #12214, .F. ) ;
#41587 = CARTESIAN_POINT ( 'NONE',  ( 92.34999999999995168, -211.5299782133524502, 75.44791666666667140 ) ) ;
#41589 = AXIS2_PLACEMENT_3D ( 'NONE', #10457, #15733, #55582 ) ;
#41588 = CARTESIAN_POINT ( 'NONE',  ( -7.500000000000015099, -73.00000000000001421, -204.9999999999999716 ) ) ;
#41590 = VERTEX_POINT ( 'NONE', #61812 ) ;
#41591 = ORIENTED_EDGE ( 'NONE', *, *, #53374, .F. ) ;
#41592 = EDGE_CURVE ( 'NONE', #66094, #38048, #21565, .T. ) ;
#41593 = CARTESIAN_POINT ( 'NONE',  ( 10.00000000000000000, 35.53030884539102630, -12.26510123303222599 ) ) ;
#41594 = CARTESIAN_POINT ( 'NONE',  ( 96.15314808468750130, -211.9973110713294489, 83.02822916753380866 ) ) ;
#41595 = DIRECTION ( 'NONE',  ( -0.000000000000000000, -0.000000000000000000, -1.000000000000000000 ) ) ;
#41596 = FACE_OUTER_BOUND ( 'NONE', #28269, .T. ) ;
#41597 = CARTESIAN_POINT ( 'NONE',  ( 97.65000000000000568, -211.5299782133524218, 76.92958333333332632 ) ) ;
#41598 = AXIS2_PLACEMENT_3D ( 'NONE', #33873, #45165, #50784 ) ;
#41599 = FACE_OUTER_BOUND ( 'NONE', #26512, .T. ) ;
#41600 = CARTESIAN_POINT ( 'NONE',  ( 97.64999999999997726, -208.4700217866474645, 83.38541666666667140 ) ) ;
#41601 = ORIENTED_EDGE ( 'NONE', *, *, #56644, .T. ) ;
#41602 = EDGE_LOOP ( 'NONE', ( #64108, #4831, #71254, #46256 ) ) ;
#41603 = ORIENTED_EDGE ( 'NONE', *, *, #6317, .F. ) ;
#41604 = ORIENTED_EDGE ( 'NONE', *, *, #20574, .F. ) ;
#41605 = CARTESIAN_POINT ( 'NONE',  ( 10.00000000000000000, -15.33399622253424965, -80.55351364060605590 ) ) ;
#41606 = ADVANCED_FACE ( 'NONE', ( #33967, #57277 ), #27586, .T. ) ;
#41607 = EDGE_CURVE ( 'NONE', #74237, #66421, #74031, .T. ) ;
#41608 = SHAPE_REPRESENTATION_RELATIONSHIP ( 'NONE' , 'NONE' ,  #23457, #55235 ) ;
#41609 = CARTESIAN_POINT ( 'NONE',  ( -96.15314808468752972, 91.99731107132950569, 87.79072916753381151 ) ) ;
#41610 = AXIS2_PLACEMENT_3D ( 'NONE', #31774, #26136, #49074 ) ;
#41611 = DIRECTION ( 'NONE',  ( 1.000000000000000000, -0.000000000000000000, -0.000000000000000000 ) ) ;
#41612 = CARTESIAN_POINT ( 'NONE',  ( 2.746650072473138780E-12, -120.0000000000000000, -70.59999999999999432 ) ) ;
#41613 = CARTESIAN_POINT ( 'NONE',  ( 97.30629616937498838, -209.9999999999999716, 88.05531250086713158 ) ) ;
#41614 = CARTESIAN_POINT ( 'NONE',  ( 94.99999999999998579, 93.05995642670504253, 79.04625000000000057 ) ) ;
#41615 = ORIENTED_EDGE ( 'NONE', *, *, #11965, .T. ) ;
#41616 = CARTESIAN_POINT ( 'NONE',  ( -10.00000000000000000, 0.000000000000000000, 0.000000000000000000 ) ) ;
#41617 = EDGE_LOOP ( 'NONE', ( #2916, #35412, #37522, #12395 ) ) ;
#41618 = CARTESIAN_POINT ( 'NONE',  ( -94.99999999999997158, -213.0599564267049857, 85.07875000000001364 ) ) ;
#41619 = VECTOR ( 'NONE', #28901, 1000.000000000000000 ) ;
#41620 = EDGE_LOOP ( 'NONE', ( #45013, #73017, #47362, #40995 ) ) ;
#41621 = CARTESIAN_POINT ( 'NONE',  ( -96.32500000000001705, 87.70503267997129626, 85.74020833506763495 ) ) ;
#41622 = CARTESIAN_POINT ( 'NONE',  ( 97.30629616937498838, 88.66845928578037217, 76.57239583420046358 ) ) ;
#41623 = ORIENTED_EDGE ( 'NONE', *, *, #6625, .T. ) ;
#41624 = FACE_OUTER_BOUND ( 'NONE', #7769, .T. ) ;
#41625 = FACE_OUTER_BOUND ( 'NONE', #24138, .T. ) ;
#41626 = CARTESIAN_POINT ( 'NONE',  ( 0.000000000000000000, 0.000000000000000000, 12.50000000000000000 ) ) ;
#41627 = CARTESIAN_POINT ( 'NONE',  ( 0.000000000000000000, 35.92658777277510040, 10.74501242461294659 ) ) ;
#41628 = EDGE_LOOP ( 'NONE', ( #19897, #69436, #53906, #26230 ) ) ;
#41629 = CARTESIAN_POINT ( 'NONE',  ( 0.000000000000000000, 0.000000000000000000, 40.80000000000001847 ) ) ;
#41630 = DIRECTION ( 'NONE',  ( 0.9580045777625458836, 0.2867529058022011412, -0.000000000000000000 ) ) ;
#41631 = ORIENTED_EDGE ( 'NONE', *, *, #22151, .T. ) ;
#41632 = ORIENTED_EDGE ( 'NONE', *, *, #26636, .F. ) ;
#41633 = CARTESIAN_POINT ( 'NONE',  ( 10.00000000000000000, 0.000000000000000000, 0.000000000000000000 ) ) ;
#41634 = CARTESIAN_POINT ( 'NONE',  ( 10.00000000000000000, 30.80686688397041451, -21.53537804866048688 ) ) ;
#41635 = DIRECTION ( 'NONE',  ( -1.000000000000000000, 0.000000000000000000, -0.000000000000000000 ) ) ;
#41636 = ORIENTED_EDGE ( 'NONE', *, *, #11386, .F. ) ;
#41637 = CARTESIAN_POINT ( 'NONE',  ( -97.30629616937497417, -208.6684592857803011, 88.47864583420047779 ) ) ;
#41638 = VERTEX_POINT ( 'NONE', #32840 ) ;
#41639 = CARTESIAN_POINT ( 'NONE',  ( -92.34999999999999432, -209.9999999999999716, 82.69749999999999091 ) ) ;
#41640 = ORIENTED_EDGE ( 'NONE', *, *, #22990, .T. ) ;
#41641 = ORIENTED_EDGE ( 'NONE', *, *, #27326, .F. ) ;
#41642 = CARTESIAN_POINT ( 'NONE',  ( 22.08297821871651934, -111.8242998470044540, -5.500000000000000000 ) ) ;
#41643 = VECTOR ( 'NONE', #73357, 1000.000000000000000 ) ;
#41644 = DIRECTION ( 'NONE',  ( 0.000000000000000000, 0.4539904997395477482, -0.8910065241883674547 ) ) ;
#41645 = CYLINDRICAL_SURFACE ( 'NONE', #3756, 32.00000000000000000 ) ;
#41646 = CARTESIAN_POINT ( 'NONE',  ( 97.30629616937498838, 88.66845928578035796, 82.28739583420048120 ) ) ;
#41647 = CYLINDRICAL_SURFACE ( 'NONE', #56824, 82.00000000000000000 ) ;
#41648 = CARTESIAN_POINT ( 'NONE',  ( -92.35000000000005116, 91.52997821335253548, 80.28979166840095161 ) ) ;
#41649 = CYLINDRICAL_SURFACE ( 'NONE', #14448, 31.99999999999998579 ) ;
#41650 = DIRECTION ( 'NONE',  ( -1.000000000000000000, -0.000000000000000000, -0.000000000000000000 ) ) ;
#41651 = DIRECTION ( 'NONE',  ( -1.000000000000000000, 0.000000000000000000, 0.000000000000000000 ) ) ;
#41652 = CARTESIAN_POINT ( 'NONE',  ( 4.279208249584789847, 3.302900657080011459, -1.325189086772932123 ) ) ;
#41653 = CARTESIAN_POINT ( 'NONE',  ( 95.00000000000000000, -209.9999999999999716, 90.00000000000000000 ) ) ;
#41654 = AXIS2_PLACEMENT_3D ( 'NONE', #69839, #39437, #5240 ) ;
#41655 = CARTESIAN_POINT ( 'NONE',  ( 11.99999999999999822, -31.47745569255189224, 68.26794271651249346 ) ) ;
#41656 = EDGE_CURVE ( 'NONE', #16746, #47938, #5787, .T. ) ;
#41657 = CIRCLE ( 'NONE', #861, 31.99999999999998579 ) ;
#41658 = CARTESIAN_POINT ( 'NONE',  ( 6.000000000000000000, -76.69515212746036070, 29.01471420065536932 ) ) ;
#41659 = CARTESIAN_POINT ( 'NONE',  ( -97.30629616937501680, 90.00000000000004263, 87.73781250086713612 ) ) ;
#41660 = CARTESIAN_POINT ( 'NONE',  ( 0.000000000000000000, -120.0000000000000000, 2.500000000000000000 ) ) ;
#41661 = VECTOR ( 'NONE', #47325, 1000.000000000000000 ) ;
#41662 = EDGE_CURVE ( 'NONE', #36881, #26809, #49076, .T. ) ;
#41663 = AXIS2_PLACEMENT_3D ( 'NONE', #35879, #59197, #6942 ) ;
#41664 =( BOUNDED_CURVE ( )  B_SPLINE_CURVE ( 2, ( #35984, #17591, #1088, #6681, #29587, #7428, #40904, #47281, #46534 ),
 .UNSPECIFIED., .F., .F. ) 
 B_SPLINE_CURVE_WITH_KNOTS ( ( 3, 2, 2, 2, 3 ),
 ( 0.2116728463017078510, 0.2116729662275106394, 0.2187287317684276922, 0.2257844973093446894, 0.2328402629031412763 ),
 .UNSPECIFIED. ) 
 CURVE ( )  GEOMETRIC_REPRESENTATION_ITEM ( )  RATIONAL_B_SPLINE_CURVE ( ( 0.9999954457846356171, 0.9999977228536134355, 1.000000000000000000, 0.8660254037844387076, 1.000000000000000000, 0.8660254037844387076, 1.000000000000000000, 0.8660254037844387076, 1.000000000000000000 ) ) 
 REPRESENTATION_ITEM ( '' )  );
#41665 = EDGE_CURVE ( 'NONE', #27978, #464, #36034, .T. ) ;
#41666 = LINE ( 'NONE', #46575, #28876 ) ;
#41667 = VECTOR ( 'NONE', #16606, 1000.000000000000000 ) ;
#41668 = EDGE_LOOP ( 'NONE', ( #44386, #66080, #23259, #36091 ) ) ;
#41669 = EDGE_CURVE ( 'NONE', #50389, #986, #58378, .T. ) ;
#41670 = DIRECTION ( 'NONE',  ( 0.000000000000000000, 0.000000000000000000, 1.000000000000000000 ) ) ;
#41671 = DIRECTION ( 'NONE',  ( -1.000000000000000000, 0.000000000000000000, -0.000000000000000000 ) ) ;
#41672 = VECTOR ( 'NONE', #52209, 1000.000000000000000 ) ;
#41673 = DIRECTION ( 'NONE',  ( 0.000000000000000000, 0.000000000000000000, 1.000000000000000000 ) ) ;
#41674 = DIRECTION ( 'NONE',  ( 0.000000000000000000, 0.000000000000000000, 1.000000000000000000 ) ) ;
#41675 = CARTESIAN_POINT ( 'NONE',  ( 95.00000000000000000, -212.6630814284392557, 81.07031250086716057 ) ) ;
#41676 = AXIS2_PLACEMENT_3D ( 'NONE', #73573, #39013, #45029 ) ;
#41677 = VERTEX_POINT ( 'NONE', #63671 ) ;
#41678 = ORIENTED_EDGE ( 'NONE', *, *, #70111, .F. ) ;
#41679 = EDGE_CURVE ( 'NONE', #24699, #54553, #64771, .T. ) ;
#41680 = EDGE_CURVE ( 'NONE', #63633, #47974, #4445, .T. ) ;
#41681 = CYLINDRICAL_SURFACE ( 'NONE', #35616, 12.50000000000000000 ) ;
#41682 = ORIENTED_EDGE ( 'NONE', *, *, #65799, .T. ) ;
#41683 = CARTESIAN_POINT ( 'NONE',  ( -12.75044424985254921, 0.001194404164626844313, -80.00000000000001421 ) ) ;
#41684 = CARTESIAN_POINT ( 'NONE',  ( -3.000000000000000000, 23.59884966291538078, -12.14883922797231541 ) ) ;
#41685 = ORIENTED_EDGE ( 'NONE', *, *, #2426, .F. ) ;
#41686 = CARTESIAN_POINT ( 'NONE',  ( 96.15314808468748708, -208.0026889286704943, 80.06489583420048461 ) ) ;
#41687 = ORIENTED_EDGE ( 'NONE', *, *, #21437, .T. ) ;
#41688 = LINE ( 'NONE', #54096, #56351 ) ;
#41689 = ORIENTED_EDGE ( 'NONE', *, *, #7295, .T. ) ;
#41690 = ORIENTED_EDGE ( 'NONE', *, *, #69548, .F. ) ;
#41691 = CARTESIAN_POINT ( 'NONE',  ( 2.746707903440850533E-12, -120.0000000000000000, -70.59999999999999432 ) ) ;
#41692 = EDGE_CURVE ( 'NONE', #41704, #15433, #30171, .T. ) ;
#41693 = ADVANCED_FACE ( 'NONE', ( #17781 ), #42213, .T. ) ;
#41694 = CARTESIAN_POINT ( 'NONE',  ( 6.509281303079589520, -14.89695620656361008, -1.199999999999999956 ) ) ;
#41695 = VERTEX_POINT ( 'NONE', #41825 ) ;
#41696 = DIRECTION ( 'NONE',  ( -0.000000000000000000, -0.000000000000000000, 1.000000000000000000 ) ) ;
#41697 = CARTESIAN_POINT ( 'NONE',  ( 92.35000000000002274, -208.4700217866474645, 82.40645833506762585 ) ) ;
#41698 = CARTESIAN_POINT ( 'NONE',  ( 97.64999999999999147, 90.00000000000002842, 89.04749999999999943 ) ) ;
#41699 = ORIENTED_EDGE ( 'NONE', *, *, #25951, .F. ) ;
#41700 = CARTESIAN_POINT ( 'NONE',  ( 93.67499999999998295, 92.29496732002878900, 84.89354166840095672 ) ) ;
#41701 = CYLINDRICAL_SURFACE ( 'NONE', #68147, 16.00000000000000000 ) ;
#41702 =( REPRESENTATION_RELATIONSHIP ('NONE','NONE', #31117, #23018 ) REPRESENTATION_RELATIONSHIP_WITH_TRANSFORMATION ( #29675 )SHAPE_REPRESENTATION_RELATIONSHIP( ) );
#41703 = EDGE_LOOP ( 'NONE', ( #13124, #14201, #2002, #23934 ) ) ;
#41704 = VERTEX_POINT ( 'NONE', #70016 ) ;
#41705 = CARTESIAN_POINT ( 'NONE',  ( -92.69370383062504004, 90.00000000000004263, 87.57906250086715261 ) ) ;
#41706 = AXIS2_PLACEMENT_3D ( 'NONE', #67543, #16034, #20567 ) ;
#41707 = ORIENTED_EDGE ( 'NONE', *, *, #37252, .F. ) ;
#41709 = CARTESIAN_POINT ( 'NONE',  ( 97.64999999999997726, 88.47002178664753558, 84.62895833506763665 ) ) ;
#41708 = AXIS2_PLACEMENT_3D ( 'NONE', #57909, #6410, #797 ) ;
#41710 = SURFACE_STYLE_FILL_AREA ( #53004 ) ;
#41711 = ORIENTED_EDGE ( 'NONE', *, *, #51159, .T. ) ;
#41712 = FACE_BOUND ( 'NONE', #42190, .T. ) ;
#41713 = CARTESIAN_POINT ( 'NONE',  ( 6.000000000000000000, -71.87247863392443037, 39.47590169984818687 ) ) ;
#41714 = VERTEX_POINT ( 'NONE', #29418 ) ;
#41715 = VERTEX_POINT ( 'NONE', #41104 ) ;
#41716 = ORIENTED_EDGE ( 'NONE', *, *, #27209, .T. ) ;
#41717 = CARTESIAN_POINT ( 'NONE',  ( -97.65000000000009095, 91.52997821335247863, 86.13708333333332234 ) ) ;
#41718 = CARTESIAN_POINT ( 'NONE',  ( 11.99999999999999822, -14.66109333815410487, -73.73191006444587003 ) ) ;
#41719 = CARTESIAN_POINT ( 'NONE',  ( -96.32500000000001705, 87.70503267997129626, 88.83583333333334053 ) ) ;
#41720 = ORIENTED_EDGE ( 'NONE', *, *, #56827, .F. ) ;
#41721 = CARTESIAN_POINT ( 'NONE',  ( 11.99999999999999822, 0.000000000000000000, 0.000000000000000000 ) ) ;
#41722 = CARTESIAN_POINT ( 'NONE',  ( 0.000000000000000000, -73.72996012237449293, 14.67089635893687571 ) ) ;
#41723 = ORIENTED_EDGE ( 'NONE', *, *, #45950, .F. ) ;
#41724 = DIRECTION ( 'NONE',  ( -1.000000000000000000, -0.000000000000000000, -0.000000000000000000 ) ) ;
#41725 = CARTESIAN_POINT ( 'NONE',  ( -94.99999999999997158, -207.3369185715606307, 81.86406250086714920 ) ) ;
#41726 = ORIENTED_EDGE ( 'NONE', *, *, #24111, .F. ) ;
#41727 = FACE_OUTER_BOUND ( 'NONE', #28215, .T. ) ;
#41728 = LINE ( 'NONE', #19899, #36824 ) ;
#41729 = DIRECTION ( 'NONE',  ( -1.000000000000000000, 0.000000000000000000, 0.000000000000000000 ) ) ;
#41730 = CARTESIAN_POINT ( 'NONE',  ( -97.64999999989197477, 90.00001510551047090, 78.64888723592453346 ) ) ;
#41731 = EDGE_CURVE ( 'NONE', #3104, #56774, #540, .T. ) ;
#41732 = CARTESIAN_POINT ( 'NONE',  ( 0.000000000000000000, 50.95692526931414790, -58.39081064771693974 ) ) ;
#41733 = CIRCLE ( 'NONE', #44096, 17.50000000000000355 ) ;
#41734 = DIRECTION ( 'NONE',  ( -1.000000000000000000, 0.000000000000000000, 0.000000000000000000 ) ) ;
#41735 = CARTESIAN_POINT ( 'NONE',  ( 10.00000000000000000, 5.256550761633969060, -77.32052557432835727 ) ) ;
#41736 = ADVANCED_FACE ( 'NONE', ( #58758 ), #35085, .F. ) ;
#41737 = DIRECTION ( 'NONE',  ( -1.000000000000000000, -0.000000000000000000, 0.000000000000000000 ) ) ;
#41738 = DIRECTION ( 'NONE',  ( -1.000000000000000000, -0.000000000000000000, 0.000000000000000000 ) ) ;
#41740 = ADVANCED_FACE ( 'NONE', ( #64036 ), #57656, .F. ) ;
#41739 = AXIS2_PLACEMENT_3D ( 'NONE', #42272, #14789, #37372 ) ;
#41741 = DIRECTION ( 'NONE',  ( -1.000000000000000000, -1.427937372958405461E-15, -7.962523111839130290E-16 ) ) ;
#41742 = CARTESIAN_POINT ( 'NONE',  ( -92.69370383062502583, 88.66845928578038638, 76.57239583420046358 ) ) ;
#41743 = DIRECTION ( 'NONE',  ( 0.000000000000000000, 0.000000000000000000, 1.000000000000000000 ) ) ;
#41744 = DIRECTION ( 'NONE',  ( -1.000000000000000000, -0.000000000000000000, -0.000000000000000000 ) ) ;
#41745 = DIRECTION ( 'NONE',  ( -1.000000000000000000, 0.000000000000000000, 0.000000000000000000 ) ) ;
#41746 = EDGE_CURVE ( 'NONE', #38802, #51749, #74307, .T. ) ;
#41747 = DIRECTION ( 'NONE',  ( 0.000000000000000000, 0.000000000000000000, 1.000000000000000000 ) ) ;
#41748 = DIRECTION ( 'NONE',  ( -1.000000000000000000, 0.000000000000000000, 0.000000000000000000 ) ) ;
#41749 = DIRECTION ( 'NONE',  ( 0.6575728627325955200, -0.7533909544171996098, -1.230411769795008318E-16 ) ) ;
#41750 = DIRECTION ( 'NONE',  ( 0.000000000000000000, -0.8910065241883722287, 0.4539904997395383113 ) ) ;
#41751 = CYLINDRICAL_SURFACE ( 'NONE', #5258, 82.00000000000000000 ) ;
#41752 = CARTESIAN_POINT ( 'NONE',  ( -92.69370383062498320, -209.9999999999999716, 75.51406250086715488 ) ) ;
#41753 = FACE_OUTER_BOUND ( 'NONE', #70719, .T. ) ;
#41754 =( BOUNDED_CURVE ( )  B_SPLINE_CURVE ( 2, ( #69568, #57927, #27857, #29330, #51906, #45914, #22604 ),
 .UNSPECIFIED., .F., .F. ) 
 B_SPLINE_CURVE_WITH_KNOTS ( ( 3, 2, 2, 3 ),
 ( 0.5624999999999997780, 0.5694444444444440867, 0.5763888888888885065, 0.5833333333333329263 ),
 .UNSPECIFIED. ) 
 CURVE ( )  GEOMETRIC_REPRESENTATION_ITEM ( )  RATIONAL_B_SPLINE_CURVE ( ( 1.000000000000004219, 0.8660254037844343777, 1.000000000000000000, 0.8660254037844387076, 1.000000000000000000, 0.8660254037844472563, 0.9999999999999914513 ) ) 
 REPRESENTATION_ITEM ( '' )  );
#41755 = EDGE_LOOP ( 'NONE', ( #71353, #30354, #64005, #17648 ) ) ;
#41756 = ADVANCED_FACE ( 'NONE', ( #19261 ), #35447, .F. ) ;
#41757 = VECTOR ( 'NONE', #26983, 1000.000000000000000 ) ;
#41758 = DIRECTION ( 'NONE',  ( -1.000000000000000000, 7.571543891232750625E-15, 2.563413034563919882E-14 ) ) ;
#41759 = DIRECTION ( 'NONE',  ( -1.000000000000000000, -0.000000000000000000, -0.000000000000000000 ) ) ;
#41760 = DIRECTION ( 'NONE',  ( 0.6064928550163511956, 0.7950889364178798102, -0.000000000000000000 ) ) ;
#41761 =( GEOMETRIC_REPRESENTATION_CONTEXT ( 3 ) GLOBAL_UNCERTAINTY_ASSIGNED_CONTEXT ( ( #45886 ) ) GLOBAL_UNIT_ASSIGNED_CONTEXT ( ( #24003, #69846, #65701 ) ) REPRESENTATION_CONTEXT ( 'NONE', 'WORKASPACE' ) );
#41762 = AXIS2_PLACEMENT_3D ( 'NONE', #71234, #52861, #46858 ) ;
#41763 = CARTESIAN_POINT ( 'NONE',  ( 5.000000000000000000, 64.81221759200343513, 50.23322058963371006 ) ) ;
#41764 = VECTOR ( 'NONE', #39438, 1000.000000000000114 ) ;
#41765 = DIRECTION ( 'NONE',  ( 1.000000000000000000, 0.000000000000000000, 0.000000000000000000 ) ) ;
#41766 = ORIENTED_EDGE ( 'NONE', *, *, #9582, .T. ) ;
#41767 = EDGE_CURVE ( 'NONE', #52143, #42621, #36185, .T. ) ;
#41768 = CARTESIAN_POINT ( 'NONE',  ( 10.00000000000000000, 36.88895765772633695, 6.736453364083687667 ) ) ;
#41769 = EDGE_CURVE ( 'NONE', #16195, #31341, #24180, .T. ) ;
#41770 = FILL_AREA_STYLE_COLOUR ( '', #61989 ) ;
#41771 = ORIENTED_EDGE ( 'NONE', *, *, #69511, .F. ) ;
#41772 = CARTESIAN_POINT ( 'NONE',  ( 92.69370383062501162, -209.9999999999999716, 83.92781250086714806 ) ) ;
#41773 = CARTESIAN_POINT ( 'NONE',  ( 96.15314808468748708, -208.0026889286704943, 87.04989583420048405 ) ) ;
#41774 = ADVANCED_FACE ( 'NONE', ( #46366 ), #47113, .T. ) ;
#41775 = EDGE_LOOP ( 'NONE', ( #3825, #3011 ) ) ;
#41776 = CARTESIAN_POINT ( 'NONE',  ( -97.65000000000000568, 91.52997821335254969, 79.78708333333331382 ) ) ;
#41777 = ORIENTED_EDGE ( 'NONE', *, *, #29611, .T. ) ;
#41778 = FACE_BOUND ( 'NONE', #22322, .T. ) ;
#41779 = VERTEX_POINT ( 'NONE', #35804 ) ;
#41780 = CARTESIAN_POINT ( 'NONE',  ( -96.15314808468752972, 91.99731107132950569, 80.17072916753382117 ) ) ;
#41781 = VECTOR ( 'NONE', #58905, 1000.000000000000114 ) ;
#41782 = ORIENTED_EDGE ( 'NONE', *, *, #13728, .T. ) ;
#41783 = ORIENTED_EDGE ( 'NONE', *, *, #26210, .F. ) ;
#41784 = CIRCLE ( 'NONE', #11779, 12.50000000000000000 ) ;
#41785 = LINE ( 'NONE', #2351, #22077 ) ;
#41786 = VECTOR ( 'NONE', #29105, 1000.000000000000000 ) ;
#41787 = ORIENTED_EDGE ( 'NONE', *, *, #70496, .F. ) ;
#41788 = CARTESIAN_POINT ( 'NONE',  ( 7.103376864691351012E-17, -120.0000000000000000, -85.59999999999999432 ) ) ;
#41789 =( NAMED_UNIT ( * ) SI_UNIT ( $, .STERADIAN. ) SOLID_ANGLE_UNIT ( ) );
#41790 = AXIS2_PLACEMENT_3D ( 'NONE', #41844, #36202, #59514 ) ;
#41791 = VERTEX_POINT ( 'NONE', #24537 ) ;
#41792 = CARTESIAN_POINT ( 'NONE',  ( 5.000000000000000000, 50.23322058963442061, -64.81221759200289512 ) ) ;
#41793 = EDGE_LOOP ( 'NONE', ( #52055, #52658, #60144, #32712 ) ) ;
#41794 = CIRCLE ( 'NONE', #36970, 42.00000000000000000 ) ;
#41795 = DIRECTION ( 'NONE',  ( -1.000000000000000000, -0.000000000000000000, 0.000000000000000000 ) ) ;
#41796 = ORIENTED_EDGE ( 'NONE', *, *, #39848, .T. ) ;
#41797 = ORIENTED_EDGE ( 'NONE', *, *, #4377, .T. ) ;
#41798 = VERTEX_POINT ( 'NONE', #18884 ) ;
#41799 = CARTESIAN_POINT ( 'NONE',  ( 93.84685191531251292, -211.9973110713294489, 82.12864583420046927 ) ) ;
#41800 = LINE ( 'NONE', #53820, #68918 ) ;
#41801 = CONTEXT_DEPENDENT_SHAPE_REPRESENTATION ( #3315, #51845 ) ;
#41802 = CARTESIAN_POINT ( 'NONE',  ( 97.64999999999999147, -209.9999999999999716, 90.00000000000000000 ) ) ;
#41803 = LINE ( 'NONE', #64378, #513 ) ;
#41804 = DIRECTION ( 'NONE',  ( 0.000000000000000000, 1.000000000000000000, 3.491481338843133750E-15 ) ) ;
#41805 = LINE ( 'NONE', #36904, #34367 ) ;
#41806 = CARTESIAN_POINT ( 'NONE',  ( -97.64999999999996305, -210.0000343786549308, 88.80937619077334944 ) ) ;
#41807 = CARTESIAN_POINT ( 'NONE',  ( -0.0004442498525516064278, 0.001194404164626844313, -85.59999999999999432 ) ) ;
#41808 = CARTESIAN_POINT ( 'NONE',  ( -94.99999999999997158, -207.3369185715606307, 85.03906250086714635 ) ) ;
#41809 = CARTESIAN_POINT ( 'NONE',  ( -96.15314808468752972, 91.99731107132950569, 82.07572916753382231 ) ) ;
#41810 = ORIENTED_EDGE ( 'NONE', *, *, #52828, .T. ) ;
#41811 = CARTESIAN_POINT ( 'NONE',  ( 92.69370383062498320, 91.33154071421968467, 81.96989583420048575 ) ) ;
#41812 = ORIENTED_EDGE ( 'NONE', *, *, #53240, .T. ) ;
#41813 = CARTESIAN_POINT ( 'NONE',  ( -92.35000000002618492, -210.0000000000000853, -74.99999999999342037 ) ) ;
#41814 = CARTESIAN_POINT ( 'NONE',  ( -3.000000000000000000, -20.55727247249748046, 16.78983467731285018 ) ) ;
#41815 = AXIS2_PLACEMENT_3D ( 'NONE', #44585, #3633, #39312 ) ;
#41816 = CARTESIAN_POINT ( 'NONE',  ( -94.99999999999997158, -213.0599564267049857, 83.25312500173430408 ) ) ;
#41817 = DIRECTION ( 'NONE',  ( -1.000000000000000000, -0.000000000000000000, -0.000000000000000000 ) ) ;
#41818 = DIRECTION ( 'NONE',  ( -1.000000000000000000, 0.000000000000000000, -0.000000000000000000 ) ) ;
#41819 = CARTESIAN_POINT ( 'NONE',  ( -97.30629616937495996, -209.9999999999999716, 82.02281250086714692 ) ) ;
#41820 = VECTOR ( 'NONE', #73828, 1000.000000000000000 ) ;
#41821 = AXIS2_PLACEMENT_3D ( 'NONE', #51558, #34632, #17711 ) ;
#41822 = DIRECTION ( 'NONE',  ( 1.000000000000000000, -3.061616997868382648E-16, -0.000000000000000000 ) ) ;
#41823 = LINE ( 'NONE', #64769, #14621 ) ;
#41824 = LINE ( 'NONE', #35803, #16297 ) ;
#41825 = CARTESIAN_POINT ( 'NONE',  ( 23.50000000000000355, -120.0000000000000000, -64.00000000000000000 ) ) ;
#41826 = VERTEX_POINT ( 'NONE', #37678 ) ;
#41827 = CIRCLE ( 'NONE', #35806, 42.00000000000000000 ) ;
#41828 = ORIENTED_EDGE ( 'NONE', *, *, #46082, .T. ) ;
#41829 = VECTOR ( 'NONE', #46478, 1000.000000000000000 ) ;
#41830 = EDGE_CURVE ( 'NONE', #66208, #46926, #65512, .T. ) ;
#41831 = CARTESIAN_POINT ( 'NONE',  ( -92.35000000000005116, 91.52997821335253548, 75.76541666666666686 ) ) ;
#41832 = EDGE_CURVE ( 'NONE', #45184, #38512, #20742, .T. ) ;
#41833 = CYLINDRICAL_SURFACE ( 'NONE', #11514, 16.00000000000000000 ) ;
#41834 = CARTESIAN_POINT ( 'NONE',  ( -95.00000000000002842, 92.66308142843932671, 88.84906250086713442 ) ) ;
#41835 = LINE ( 'NONE', #71872, #68234 ) ;
#41836 = DIRECTION ( 'NONE',  ( -1.000000000000000000, 3.061616997868382648E-16, 0.000000000000000000 ) ) ;
#41837 = FACE_OUTER_BOUND ( 'NONE', #12368, .T. ) ;
#41838 = DIRECTION ( 'NONE',  ( 0.000000000000000000, 0.6494480483301848794, -0.7604059656000299317 ) ) ;
#41839 = ORIENTED_EDGE ( 'NONE', *, *, #20005, .F. ) ;
#41840 = CARTESIAN_POINT ( 'NONE',  ( -97.30629616937501680, 91.33154071421968467, 75.61989583420047722 ) ) ;
#41841 = EDGE_CURVE ( 'NONE', #52067, #33176, #71493, .T. ) ;
#41842 = CIRCLE ( 'NONE', #9410, 16.00000000000000355 ) ;
#41843 = EDGE_CURVE ( 'NONE', #62834, #51153, #20427, .T. ) ;
#41844 = CARTESIAN_POINT ( 'NONE',  ( 11.99999999999999822, -72.35160999960801576, -20.41045688087902121 ) ) ;
#41845 = AXIS2_PLACEMENT_3D ( 'NONE', #30867, #31248, #29755 ) ;
#41846 = DIRECTION ( 'NONE',  ( 0.000000000000000000, 0.000000000000000000, -1.000000000000000000 ) ) ;
#41847 = DIRECTION ( 'NONE',  ( 0.000000000000000000, 0.8910065241883657894, 0.4539904997395509678 ) ) ;
#41848 = CARTESIAN_POINT ( 'NONE',  ( 95.00000000000000000, -213.0599564267049857, 82.53874999999999318 ) ) ;
#41849 = CARTESIAN_POINT ( 'NONE',  ( -97.30629616937495996, -209.9999999999999716, 87.89656250086714806 ) ) ;
#41850 = AXIS2_PLACEMENT_3D ( 'NONE', #54542, #8686, #65829 ) ;
#41851 = AXIS2_PLACEMENT_3D ( 'NONE', #30094, #30459, #53408 ) ;
#41852 = DIRECTION ( 'NONE',  ( -1.000000000000000000, 0.000000000000000000, 0.000000000000000000 ) ) ;
#41853 = EDGE_CURVE ( 'NONE', #32262, #27633, #30017, .T. ) ;
#41854 = FACE_OUTER_BOUND ( 'NONE', #2344, .T. ) ;
#41855 = CARTESIAN_POINT ( 'NONE',  ( -94.99999999999997158, -207.3369185715606307, 76.94281250086714863 ) ) ;
#41856 = CARTESIAN_POINT ( 'NONE',  ( -2.977765906491215642, 1.885622467823562354E-15, 15.39727592589476579 ) ) ;
#41857 = ORIENTED_EDGE ( 'NONE', *, *, #68613, .F. ) ;
#41858 = DIRECTION ( 'NONE',  ( -1.000000000000000000, -0.000000000000000000, 0.000000000000000000 ) ) ;
#41859 = FACE_OUTER_BOUND ( 'NONE', #57696, .T. ) ;
#41860 = DIRECTION ( 'NONE',  ( -1.000000000000000000, -0.000000000000000000, -0.000000000000000000 ) ) ;
#41861 = CARTESIAN_POINT ( 'NONE',  ( 94.99999999999998579, 90.00000000000002842, 90.00000000000000000 ) ) ;
#41862 = CARTESIAN_POINT ( 'NONE',  ( 93.84685191531251292, -211.9973110713294489, 77.04864583420047097 ) ) ;
#41863 = VERTEX_POINT ( 'NONE', #32013 ) ;
#41864 = AXIS2_PLACEMENT_3D ( 'NONE', #19697, #55027, #65585 ) ;
#41865 = ADVANCED_FACE ( 'NONE', ( #65883 ), #3116, .T. ) ;
#41866 = EDGE_CURVE ( 'NONE', #2618, #48989, #19992, .T. ) ;
#41867 = EDGE_CURVE ( 'NONE', #21615, #30533, #20246, .T. ) ;
#41868 = CARTESIAN_POINT ( 'NONE',  ( -3.000000000000000000, -18.13022148937263012, 15.02647892043544608 ) ) ;
#41869 = LINE ( 'NONE', #13658, #48710 ) ;
#41870 = ORIENTED_EDGE ( 'NONE', *, *, #26830, .T. ) ;
#41871 = VECTOR ( 'NONE', #2464, 1000.000000000000000 ) ;
#41872 = DIRECTION ( 'NONE',  ( -1.000000000000000000, -0.000000000000000000, -0.000000000000000000 ) ) ;
#41873 = EDGE_LOOP ( 'NONE', ( #11089, #62432, #19560, #9053 ) ) ;
#41874 = VECTOR ( 'NONE', #17368, 1000.000000000000000 ) ;
#41875 = CIRCLE ( 'NONE', #51476, 2.650000000000540812 ) ;
#41876 = LINE ( 'NONE', #12184, #41786 ) ;
#41877 = CIRCLE ( 'NONE', #51479, 77.49900000000000944 ) ;
#41878 = ORIENTED_EDGE ( 'NONE', *, *, #10250, .F. ) ;
#41879 = VERTEX_POINT ( 'NONE', #71861 ) ;
#41880 = AXIS2_PLACEMENT_3D ( 'NONE', #57595, #27888, #16610 ) ;
#41881 = ORIENTED_EDGE ( 'NONE', *, *, #5227, .T. ) ;
#41882 = DIRECTION ( 'NONE',  ( 0.000000000000000000, 1.000000000000000000, 3.491481338843133750E-15 ) ) ;
#41883 = ORIENTED_EDGE ( 'NONE', *, *, #33440, .T. ) ;
#41884 = EDGE_LOOP ( 'NONE', ( #53441, #61185, #29924, #53353 ) ) ;
#41885 = CARTESIAN_POINT ( 'NONE',  ( 96.15314808468748708, 91.99731107132950569, 81.33489583420049485 ) ) ;
#41886 = DIRECTION ( 'NONE',  ( -1.000000000000000000, -0.000000000000000000, -0.000000000000000000 ) ) ;
#41887 = CARTESIAN_POINT ( 'NONE',  ( 0.000000000000000000, 4.992566952385522505, -37.16516213103271582 ) ) ;
#41888 = AXIS2_PLACEMENT_3D ( 'NONE', #7617, #6162, #6516 ) ;
#41889 = EDGE_LOOP ( 'NONE', ( #33101, #66835, #49719, #27290 ) ) ;
#41891 = ORIENTED_EDGE ( 'NONE', *, *, #9683, .F. ) ;
#41890 = AXIS2_PLACEMENT_3D ( 'NONE', #26412, #32041, #71525 ) ;
#41892 = ORIENTED_EDGE ( 'NONE', *, *, #41092, .T. ) ;
#41893 = DIRECTION ( 'NONE',  ( 1.000000000000000000, 0.000000000000000000, 0.000000000000000000 ) ) ;
#41894 = ORIENTED_EDGE ( 'NONE', *, *, #33528, .F. ) ;
#41895 = AXIS2_PLACEMENT_3D ( 'NONE', #14517, #8884, #31801 ) ;
#41896 = AXIS2_PLACEMENT_3D ( 'NONE', #12020, #787, #57530 ) ;
#41897 = FILL_AREA_STYLE ('',( #35872 ) ) ;
#41898 = CARTESIAN_POINT ( 'NONE',  ( 10.00000000000000000, 0.000000000000000000, 0.000000000000000000 ) ) ;
#41899 = CARTESIAN_POINT ( 'NONE',  ( -94.22990255303845686, 92.23316662872736060, 74.81945665767621279 ) ) ;
#41900 = FACE_OUTER_BOUND ( 'NONE', #40526, .T. ) ;
#41901 = CARTESIAN_POINT ( 'NONE',  ( -97.64999999980585699, -210.0000198431789897, 84.36502761000342332 ) ) ;
#41902 = CARTESIAN_POINT ( 'NONE',  ( 4.999999999999999112, 10.41901085202078292, 40.68715046381932865 ) ) ;
#41903 = AXIS2_PLACEMENT_3D ( 'NONE', #14969, #49546, #4452 ) ;
#41904 = CARTESIAN_POINT ( 'NONE',  ( 0.000000000000000000, -80.55351364060599906, 15.33399622253457295 ) ) ;
#41905 = VECTOR ( 'NONE', #21496, 1000.000000000000000 ) ;
#41906 = CARTESIAN_POINT ( 'NONE',  ( -92.34999999999999432, -211.5299782133524502, 80.81895833506764859 ) ) ;
#41907 = CARTESIAN_POINT ( 'NONE',  ( 12.49999999999999822, -120.0000000000000000, 125.0000000000000000 ) ) ;
#41908 = EDGE_CURVE ( 'NONE', #31821, #4105, #34699, .T. ) ;
#41910 = CARTESIAN_POINT ( 'NONE',  ( -97.65000000000001990, 91.52997821335253548, 74.78645833506763552 ) ) ;
#41909 = CARTESIAN_POINT ( 'NONE',  ( 92.69370383062498320, 91.33154071421968467, 89.58989583420047609 ) ) ;
#41911 = AXIS2_PLACEMENT_3D ( 'NONE', #29275, #71245, #23648 ) ;
#41912 = ORIENTED_EDGE ( 'NONE', *, *, #53995, .T. ) ;
#41913 = CARTESIAN_POINT ( 'NONE',  ( 97.30629616937498838, 88.66845928578037217, 77.36614583420048064 ) ) ;
#41914 = DIRECTION ( 'NONE',  ( -0.000000000000000000, -0.000000000000000000, 1.000000000000000000 ) ) ;
#41915 = FACE_OUTER_BOUND ( 'NONE', #27441, .T. ) ;
#41916 = CARTESIAN_POINT ( 'NONE',  ( 95.00000000000000000, -206.9400435732949575, 77.22062500173429100 ) ) ;
#41917 = EDGE_CURVE ( 'NONE', #15716, #4389, #21483, .T. ) ;
#41918 = CARTESIAN_POINT ( 'NONE',  ( 97.64999999999999147, -209.9999998456624155, 79.60187500750917877 ) ) ;
#41919 = DIRECTION ( 'NONE',  ( -1.000000000000000000, 0.000000000000000000, 0.000000000000000000 ) ) ;
#41920 = VERTEX_POINT ( 'NONE', #59874 ) ;
#41921 = DIRECTION ( 'NONE',  ( -1.000000000000000000, -0.000000000000000000, 0.000000000000000000 ) ) ;
#41922 = CARTESIAN_POINT ( 'NONE',  ( 11.99999999999999822, -68.55367621811110723, -44.99326035066126650 ) ) ;
#41923 = ORIENTED_EDGE ( 'NONE', *, *, #57711, .T. ) ;
#41924 = ADVANCED_FACE ( 'NONE', ( #15095 ), #31646, .F. ) ;
#41925 = ORIENTED_EDGE ( 'NONE', *, *, #29684, .F. ) ;
#41926 = EDGE_CURVE ( 'NONE', #45726, #68048, #32382, .T. ) ;
#41927 = CIRCLE ( 'NONE', #37093, 42.00000000000000000 ) ;
#41928 = DIRECTION ( 'NONE',  ( -1.000000000000000000, 0.000000000000000000, 0.000000000000000000 ) ) ;
#41929 = DIRECTION ( 'NONE',  ( -1.000000000000000000, -0.000000000000000000, -0.000000000000000000 ) ) ;
#41930 = CARTESIAN_POINT ( 'NONE',  ( 23.49955575014872622, 0.001194404164656991856, -48.99999999999938893 ) ) ;
#41931 = CARTESIAN_POINT ( 'NONE',  ( -93.17363653571617021, -211.7597761561306129, 74.93163452119476631 ) ) ;
#41932 = CARTESIAN_POINT ( 'NONE',  ( -96.15314808468747287, -208.0026889286704943, 78.90072916753382515 ) ) ;
#41933 = AXIS2_PLACEMENT_3D ( 'NONE', #18146, #34695, #51244 ) ;
#41934 = EDGE_LOOP ( 'NONE', ( #57575, #55407, #9105, #56225 ) ) ;
#41935 = AXIS2_PLACEMENT_3D ( 'NONE', #69338, #11452, #52799 ) ;
#41936 = CIRCLE ( 'NONE', #19110, 15.99999999999999822 ) ;
#41937 = ADVANCED_FACE ( 'NONE', ( #42572 ), #26744, .T. ) ;
#41939 = CARTESIAN_POINT ( 'NONE',  ( -92.35000000002600018, 89.99998827382285072, 82.77687459617033028 ) ) ;
#41938 = AXIS2_PLACEMENT_3D ( 'NONE', #16107, #51060, #51804 ) ;
#41940 = DIRECTION ( 'NONE',  ( -0.9827303690289279636, -0.1850432970638682117, 0.000000000000000000 ) ) ;
#41941 = AXIS2_PLACEMENT_3D ( 'NONE', #58668, #18802, #53035 ) ;
#41942 = CARTESIAN_POINT ( 'NONE',  ( 10.00000000000000000, 0.000000000000000000, 0.000000000000000000 ) ) ;
#41943 = CARTESIAN_POINT ( 'NONE',  ( -3.000000000000000000, 23.59884966291538078, -12.14883922797231541 ) ) ;
#41944 = CIRCLE ( 'NONE', #26311, 3.299999999999997158 ) ;
#41945 = FACE_OUTER_BOUND ( 'NONE', #63187, .T. ) ;
#41946 = FACE_OUTER_BOUND ( 'NONE', #53799, .T. ) ;
#41947 = CARTESIAN_POINT ( 'NONE',  ( 11.99999999999999822, 77.32052557432841411, 5.256550761633121738 ) ) ;
#41948 = CARTESIAN_POINT ( 'NONE',  ( 15.00000000000000000, -10.45096189432344502, -21.10159698893425784 ) ) ;
#41949 = CARTESIAN_POINT ( 'NONE',  ( -94.99999999999997158, -206.9400435732949575, 77.85562500173431033 ) ) ;
#41950 = DIRECTION ( 'NONE',  ( -1.000000000000000000, 0.000000000000000000, -0.000000000000000000 ) ) ;
#41951 = EDGE_CURVE ( 'NONE', #8033, #54914, #49309, .T. ) ;
#41952 = EDGE_CURVE ( 'NONE', #47114, #24429, #30902, .T. ) ;
#41953 = CARTESIAN_POINT ( 'NONE',  ( 96.15314808468748708, 91.99731107132950569, 85.14489583420048291 ) ) ;
#41954 = CARTESIAN_POINT ( 'NONE',  ( -94.99999999999997158, -212.6630814284392557, 85.51531250086715374 ) ) ;
#41955 = DIRECTION ( 'NONE',  ( 1.000000000000000000, 0.000000000000000000, 0.000000000000000000 ) ) ;
#41956 = AXIS2_PLACEMENT_3D ( 'NONE', #13146, #7520, #59393 ) ;
#41957 = ORIENTED_EDGE ( 'NONE', *, *, #13046, .F. ) ;
#41958 = CARTESIAN_POINT ( 'NONE',  ( -3.000000000000000000, -22.67460108101783334, 6.353146135317912169 ) ) ;
#41959 = CARTESIAN_POINT ( 'NONE',  ( -96.32499999999996021, -207.7050326799711968, 81.00416666666666288 ) ) ;
#41960 = CARTESIAN_POINT ( 'NONE',  ( -95.00000000000002842, 87.33691857156074434, 77.10156250086711793 ) ) ;
#41961 = EDGE_CURVE ( 'NONE', #28563, #25004, #8290, .T. ) ;
#41962 = AXIS2_PLACEMENT_3D ( 'NONE', #12584, #24251, #58085 ) ;
#41963 = CIRCLE ( 'NONE', #47968, 42.00000000000000000 ) ;
#41964 = AXIS2_PLACEMENT_3D ( 'NONE', #62144, #44860, #27165 ) ;
#41965 = AXIS2_PLACEMENT_3D ( 'NONE', #24119, #48149, #30101 ) ;
#41966 = CARTESIAN_POINT ( 'NONE',  ( 97.30629616937498838, -209.9999999999999716, 88.05531250086713158 ) ) ;
#41967 = VERTEX_POINT ( 'NONE', #26380 ) ;
#41968 = EDGE_CURVE ( 'NONE', #66872, #31431, #31093, .T. ) ;
#41969 = EDGE_LOOP ( 'NONE', ( #54810, #30127, #5322, #24695 ) ) ;
#41970 = ORIENTED_EDGE ( 'NONE', *, *, #62515, .T. ) ;
#41971 = ADVANCED_FACE ( 'NONE', ( #31280 ), #54232, .F. ) ;
#41972 = CARTESIAN_POINT ( 'NONE',  ( -97.65000000000001990, 90.00000000000004263, 75.39499999999999602 ) ) ;
#41973 = CARTESIAN_POINT ( 'NONE',  ( 10.00000000000000000, 77.49459641780886443, 0.8261519478433866359 ) ) ;
#41974 = ORIENTED_EDGE ( 'NONE', *, *, #27922, .T. ) ;
#41975 = EDGE_LOOP ( 'NONE', ( #38833, #65376, #71865, #794, #56135, #43908, #66583, #26446, #44021, #38281, #69319, #60140, #21938, #73980, #48778, #48456, #358, #53244, #36062, #60594, #32564, #70161, #55133, #9033, #5127, #72918, #62535, #29292, #67336, #33367, #64374, #68141, #9689, #60506, #32881, #54642, #50660, #68819, #4056, #66748, #64199, #1978, #21552, #25686, #74145, #20363, #67691, #61191, #23653, #66625, #14525, #32465, #24305, #5123, #1414, #59251, #13937, #34291, #39884, #48531, #42463, #59121, #46413, #24222, #8426, #71198, #55030, #32359, #15145, #55948, #1071, #55, #30692, #233, #12931, #12290, #29733, #54182, #495, #30706, #51634, #20528, #22583, #72276, #55363, #43787, #67678, #43737, #57184, #846, #31882, #73124, #68251, #30574, #32931, #61707, #12452, #27011, #52587, #17611, #46784, #37838, #56697, #22180, #10977, #21234, #37994, #36614, #31957, #57835, #24425, #56227, #2569, #25622, #51066, #54591, #72200, #24626, #10704, #12464, #50027, #7572, #50316, #9132, #37941, #41002, #6928, #7515, #73155, #58192, #40496, #46494, #64447, #49616, #46093, #31965, #12775, #36985, #56214, #7506, #24684, #17656, #20331, #924, #1889, #21438, #46701, #22960, #22290, #51482, #35870, #26153, #65751, #25749, #40760, #61747, #5296, #59099, #33005, #42437, #35946, #8850, #25466, #60219, #40449 ) ) ;
#41976 = DIRECTION ( 'NONE',  ( -1.000000000000000000, 0.000000000000000000, 0.000000000000000000 ) ) ;
#41977 = CARTESIAN_POINT ( 'NONE',  ( 92.69370383062501162, -211.3315407142195852, 80.96447916753382401 ) ) ;
#41978 = CARTESIAN_POINT ( 'NONE',  ( 96.32499999999997442, 92.29496732002878900, 89.78833333333332689 ) ) ;
#41979 = CARTESIAN_POINT ( 'NONE',  ( 0.000000000000000000, -50.23322058963393744, 64.81221759200325039 ) ) ;
#41980 =( BOUNDED_CURVE ( )  B_SPLINE_CURVE ( 2, ( #58004, #29407, #23066, #52356, #28681, #1282, #69286, #41449, #24169, #58368, #11748 ),
 .UNSPECIFIED., .F., .F. ) 
 B_SPLINE_CURVE_WITH_KNOTS ( ( 3, 2, 2, 2, 2, 3 ),
 ( 0.6985206468843497829, 0.6985207885473544431, 0.7055765540882368292, 0.7126323196291192152, 0.7196880851700017123, 0.7196881748034551496 ),
 .UNSPECIFIED. ) 
 CURVE ( )  GEOMETRIC_REPRESENTATION_ITEM ( )  RATIONAL_B_SPLINE_CURVE ( ( 0.9999946203249847620, 0.9999973101084858040, 1.000000000000000000, 0.8660254037844387076, 1.000000000000000000, 0.8660254037844387076, 1.000000000000000000, 0.8660254037844387076, 1.000000000000000000, 0.9999982980435414559, 0.9999965961303247663 ) ) 
 REPRESENTATION_ITEM ( '' )  );
#41981 = CARTESIAN_POINT ( 'NONE',  ( 10.00000000000000000, 0.000000000000000000, 0.000000000000000000 ) ) ;
#41982 = DIRECTION ( 'NONE',  ( 1.000000000000000000, 0.000000000000000000, -0.000000000000000000 ) ) ;
#41983 = AXIS2_PLACEMENT_3D ( 'NONE', #11135, #34060, #31919 ) ;
#41984 = CARTESIAN_POINT ( 'NONE',  ( 10.00000000000000000, -17.80606268964516659, -33.00180498840066434 ) ) ;
#41985 = CARTESIAN_POINT ( 'NONE',  ( 97.64999999999997726, -211.5299782133524502, 83.27958333333333485 ) ) ;
#41986 = AXIS2_PLACEMENT_3D ( 'NONE', #31730, #49021, #54674 ) ;
#41987 = ORIENTED_EDGE ( 'NONE', *, *, #31308, .T. ) ;
#41988 = ORIENTED_EDGE ( 'NONE', *, *, #25204, .F. ) ;
#41989 = VECTOR ( 'NONE', #60604, 1000.000000000000000 ) ;
#41990 = ORIENTED_EDGE ( 'NONE', *, *, #38308, .T. ) ;
#41991 = ORIENTED_EDGE ( 'NONE', *, *, #42515, .F. ) ;
#41992 = CARTESIAN_POINT ( 'NONE',  ( 93.67500000000001137, -212.2949673200287179, 86.93083333333332519 ) ) ;
#41993 = CARTESIAN_POINT ( 'NONE',  ( -93.84685191531254134, 91.99731107132950569, 86.41489583420049314 ) ) ;
#41994 = DIRECTION ( 'NONE',  ( -0.000000000000000000, -0.000000000000000000, 1.000000000000000000 ) ) ;
#41995 = AXIS2_PLACEMENT_3D ( 'NONE', #41016, #56166, #69576 ) ;
#41996 = DIRECTION ( 'NONE',  ( -1.000000000000000000, 7.619177619974977057E-15, 2.612289469705706555E-14 ) ) ;
#41997 = CARTESIAN_POINT ( 'NONE',  ( 93.84685191531251292, -211.9973110713294489, 87.20864583420046756 ) ) ;
#41998 = CARTESIAN_POINT ( 'NONE',  ( 96.90829729882592858, 88.16127723152901297, 74.99909419456535886 ) ) ;
#41999 = ORIENTED_EDGE ( 'NONE', *, *, #74190, .F. ) ;
#42000 = FACE_OUTER_BOUND ( 'NONE', #6251, .T. ) ;
#42001 = ORIENTED_EDGE ( 'NONE', *, *, #39164, .T. ) ;
#42002 = DIRECTION ( 'NONE',  ( -1.000000000000000000, -0.000000000000000000, 0.000000000000000000 ) ) ;
#42003 = ORIENTED_EDGE ( 'NONE', *, *, #37391, .T. ) ;
#42004 = CARTESIAN_POINT ( 'NONE',  ( -92.35000000000005116, 91.52997821335253548, 86.00479166840096923 ) ) ;
#42005 = CARTESIAN_POINT ( 'NONE',  ( 97.30629616937498838, 89.06967028092473981, 74.68334033237941583 ) ) ;
#42006 = CARTESIAN_POINT ( 'NONE',  ( 0.000000000000000000, -29.81001611430991360, -22.74946021919165418 ) ) ;
#42007 = DIRECTION ( 'NONE',  ( -1.000000000000000000, 0.000000000000000000, 0.000000000000000000 ) ) ;
#42008 = VECTOR ( 'NONE', #55516, 1000.000000000000000 ) ;
#42009 = CARTESIAN_POINT ( 'NONE',  ( 0.000000000000000000, 73.44644590900061587, 24.73286445877730699 ) ) ;
#42010 = EDGE_CURVE ( 'NONE', #54593, #71746, #73577, .T. ) ;
#42011 = DIRECTION ( 'NONE',  ( -1.000000000000000000, 0.000000000000000000, 0.000000000000000000 ) ) ;
#42012 = EDGE_LOOP ( 'NONE', ( #53625, #28560, #27452, #57621 ) ) ;
#42013 = CARTESIAN_POINT ( 'NONE',  ( 1.653121499799246719, -4.819072548984012272, -5.948595712916168843 ) ) ;
#42014 = AXIS2_PLACEMENT_3D ( 'NONE', #62299, #15684, #12534 ) ;
#42016 = CARTESIAN_POINT ( 'NONE',  ( -92.35000000000005116, 91.52997821335253548, 81.55979166840097605 ) ) ;
#42015 = VECTOR ( 'NONE', #70467, 1000.000000000000000 ) ;
#42017 = ORIENTED_EDGE ( 'NONE', *, *, #28330, .T. ) ;
#42018 = EDGE_CURVE ( 'NONE', #73972, #50699, #59937, .T. ) ;
#42019 = ORIENTED_EDGE ( 'NONE', *, *, #24682, .T. ) ;
#42020 = DIRECTION ( 'NONE',  ( 0.000000000000000000, 0.000000000000000000, 1.000000000000000000 ) ) ;
#42021 = VECTOR ( 'NONE', #21530, 1000.000000000000000 ) ;
#42022 = EDGE_CURVE ( 'NONE', #7004, #9907, #37600, .T. ) ;
#42023 = VECTOR ( 'NONE', #70223, 1000.000000000000000 ) ;
#42024 = DIRECTION ( 'NONE',  ( -1.000000000000000000, -0.000000000000000000, -0.000000000000000000 ) ) ;
#42025 = DIRECTION ( 'NONE',  ( 0.000000000000000000, 0.000000000000000000, 1.000000000000000000 ) ) ;
#42026 = CARTESIAN_POINT ( 'NONE',  ( -93.84685191531248449, -208.0026889286704943, 86.41489583420049314 ) ) ;
#42027 = ORIENTED_EDGE ( 'NONE', *, *, #59169, .F. ) ;
#42028 = PRESENTATION_STYLE_ASSIGNMENT (( #48029 ) ) ;
#42029 = ORIENTED_EDGE ( 'NONE', *, *, #60922, .F. ) ;
#42030 = VERTEX_POINT ( 'NONE', #4585 ) ;
#42031 = DIRECTION ( 'NONE',  ( -1.000000000000000000, -0.000000000000000000, 0.000000000000000000 ) ) ;
#42032 = DIRECTION ( 'NONE',  ( 0.000000000000000000, 0.000000000000000000, 1.000000000000000000 ) ) ;
#42033 = DIRECTION ( 'NONE',  ( -1.000000000000000000, -0.000000000000000000, -0.000000000000000000 ) ) ;
#42034 = CARTESIAN_POINT ( 'NONE',  ( 93.84685191531248449, 88.00268892867053694, 81.49364583420047836 ) ) ;
#42035 = DIRECTION ( 'NONE',  ( -1.000000000000000000, 0.000000000000000000, 0.000000000000000000 ) ) ;
#42036 = CARTESIAN_POINT ( 'NONE',  ( 4.250000000000000000, -13.95926121303099343, -1.199999999999999956 ) ) ;
#42037 = CARTESIAN_POINT ( 'NONE',  ( -3.000000000000000000, -0.9646360437375307573, 23.52805723605590060 ) ) ;
#42038 = DIRECTION ( 'NONE',  ( 0.000000000000000000, 0.8910065241883657894, 0.4539904997395509678 ) ) ;
#42039 = EDGE_CURVE ( 'NONE', #28860, #64494, #27106, .T. ) ;
#42040 = CARTESIAN_POINT ( 'NONE',  ( 2.369999999999999662, 0.000000000000000000, 4.750000000000000000 ) ) ;
#42041 = CARTESIAN_POINT ( 'NONE',  ( 0.000000000000000000, -27.05870788708213226, -26.08949754953053102 ) ) ;
#42042 = CARTESIAN_POINT ( 'NONE',  ( 0.000000000000000000, -70.53064760720336324, 26.01480285779810231 ) ) ;
#42043 = CIRCLE ( 'NONE', #74283, 42.00000000000000000 ) ;
#42044 = DIRECTION ( 'NONE',  ( 1.000000000000000000, 0.000000000000000000, 0.000000000000000000 ) ) ;
#42045 = DIRECTION ( 'NONE',  ( 0.000000000000000000, 0.000000000000000000, 1.000000000000000000 ) ) ;
#42046 = ORIENTED_EDGE ( 'NONE', *, *, #9829, .F. ) ;
#42047 = CIRCLE ( 'NONE', #7203, 42.00000000000000000 ) ;
#42048 = CARTESIAN_POINT ( 'NONE',  ( -97.30629616937501680, 91.33154071421968467, 85.77989583420048803 ) ) ;
#42049 = EDGE_CURVE ( 'NONE', #46234, #23039, #4961, .T. ) ;
#42050 = EDGE_CURVE ( 'NONE', #52399, #3442, #56338, .T. ) ;
#42051 = FACE_OUTER_BOUND ( 'NONE', #27450, .T. ) ;
#42052 = CIRCLE ( 'NONE', #62455, 82.00000000000000000 ) ;
#42053 = DIRECTION ( 'NONE',  ( 0.8225049752423776450, 0.5687579148473765889, -0.000000000000000000 ) ) ;
#42054 = EDGE_CURVE ( 'NONE', #35660, #46991, #35927, .T. ) ;
#42055 = ORIENTED_EDGE ( 'NONE', *, *, #2409, .F. ) ;
#42056 = PLANE ( 'NONE',  #5467 ) ;
#42057 = CARTESIAN_POINT ( 'NONE',  ( 95.00000000000000000, -206.9400435732949575, 75.95062500173428077 ) ) ;
#42058 = DIRECTION ( 'NONE',  ( -1.000000000000000000, 0.000000000000000000, 0.000000000000000000 ) ) ;
#42059 = AXIS2_PLACEMENT_3D ( 'NONE', #44436, #4588, #72598 ) ;
#42060 = LINE ( 'NONE', #38544, #51212 ) ;
#42061 = AXIS2_PLACEMENT_3D ( 'NONE', #56666, #6900, #28064 ) ;
#42062 = CIRCLE ( 'NONE', #1264, 15.99999999999999822 ) ;
#42063 = CARTESIAN_POINT ( 'NONE',  ( 95.00000000000000000, -212.6630814284392557, 82.34031250086714238 ) ) ;
#42064 = ORIENTED_EDGE ( 'NONE', *, *, #36649, .F. ) ;
#42065 = CIRCLE ( 'NONE', #22861, 82.00000000000000000 ) ;
#42066 = ORIENTED_EDGE ( 'NONE', *, *, #66333, .F. ) ;
#42067 = VECTOR ( 'NONE', #36590, 999.9999999999998863 ) ;
#42068 = DIRECTION ( 'NONE',  ( 0.000000000000000000, 0.000000000000000000, 1.000000000000000000 ) ) ;
#42069 = EDGE_LOOP ( 'NONE', ( #21046, #7887, #54625, #36989 ) ) ;
#42070 = CARTESIAN_POINT ( 'NONE',  ( 15.00000000000000000, 24.81905959214260804, -9.408202855044828894 ) ) ;
#42071 = CARTESIAN_POINT ( 'NONE',  ( 96.15314808468748708, -208.0026889286704943, 76.09614583420047040 ) ) ;
#42072 = ORIENTED_EDGE ( 'NONE', *, *, #60922, .T. ) ;
#42073 = CARTESIAN_POINT ( 'NONE',  ( 95.00000000000000000, -212.6630814284392557, 79.16531250086715943 ) ) ;
#42074 = EDGE_LOOP ( 'NONE', ( #65420, #45144, #39632, #45225 ) ) ;
#42075 = DIRECTION ( 'NONE',  ( 0.000000000000000000, -0.9510565162951566398, 0.3090169943749381809 ) ) ;
#42076 = ORIENTED_EDGE ( 'NONE', *, *, #48192, .T. ) ;
#42077 = CIRCLE ( 'NONE', #36051, 37.49900000000000233 ) ;
#42078 = EDGE_LOOP ( 'NONE', ( #70979, #44673, #66225, #66586 ) ) ;
#42079 = CARTESIAN_POINT ( 'NONE',  ( -92.35000000000674447, -209.9999940177768565, 82.14187520865739600 ) ) ;
#42080 = CARTESIAN_POINT ( 'NONE',  ( -97.64999999999996305, 91.52997821335257811, 82.96208333333332519 ) ) ;
#42081 = VERTEX_POINT ( 'NONE', #45171 ) ;
#42082 = LINE ( 'NONE', #35676, #67790 ) ;
#42083 = CARTESIAN_POINT ( 'NONE',  ( 93.67500000000001137, -207.7050326799711968, 82.98854166840096980 ) ) ;
#42084 = CARTESIAN_POINT ( 'NONE',  ( 93.67499999999999716, 87.70503267997126784, 88.20083333333332121 ) ) ;
#42085 = ORIENTED_EDGE ( 'NONE', *, *, #8500, .F. ) ;
#42086 = DIRECTION ( 'NONE',  ( -1.000000000000000000, -0.000000000000000000, -0.000000000000000000 ) ) ;
#42087 = CARTESIAN_POINT ( 'NONE',  ( -10.00000000000000000, 0.000000000000000000, 0.000000000000000000 ) ) ;
#42088 = ORIENTED_EDGE ( 'NONE', *, *, #65115, .T. ) ;
#42089 = VERTEX_POINT ( 'NONE', #68095 ) ;
#42090 = CARTESIAN_POINT ( 'NONE',  ( -95.00000000000002842, 92.66308142843932671, 89.00781250086716057 ) ) ;
#42091 = CARTESIAN_POINT ( 'NONE',  ( 94.99999999999998579, 87.33691857156068750, 84.72156250086713669 ) ) ;
#42092 = ORIENTED_EDGE ( 'NONE', *, *, #17931, .T. ) ;
#42093 = CARTESIAN_POINT ( 'NONE',  ( 92.34999999999999432, 90.00000000000002842, 86.26937500173430351 ) ) ;
#42094 = CIRCLE ( 'NONE', #44458, 31.99999999999998934 ) ;
#42095 = ADVANCED_FACE ( 'NONE', ( #66969 ), #15467, .T. ) ;
#42096 = ORIENTED_EDGE ( 'NONE', *, *, #13890, .F. ) ;
#42097 = LINE ( 'NONE', #37569, #72871 ) ;
#42098 = AXIS2_PLACEMENT_3D ( 'NONE', #7363, #35188, #35551 ) ;
#42099 = CARTESIAN_POINT ( 'NONE',  ( -93.67500000000003979, 87.70503267997129626, 85.84604166840097150 ) ) ;
#42100 = ORIENTED_EDGE ( 'NONE', *, *, #2418, .F. ) ;
#42101 = EDGE_LOOP ( 'NONE', ( #51440, #32449, #38038, #8613 ) ) ;
#42102 = EDGE_CURVE ( 'NONE', #34388, #57700, #11662, .T. ) ;
#42103 = VECTOR ( 'NONE', #31816, 1000.000000000000000 ) ;
#42104 = ORIENTED_EDGE ( 'NONE', *, *, #56373, .F. ) ;
#42105 = DIRECTION ( 'NONE',  ( 2.603472992746261562E-14, 2.546204323184492723E-14, -1.000000000000000000 ) ) ;
#42106 = CARTESIAN_POINT ( 'NONE',  ( 94.99999999999998579, 93.05995642670504253, 75.31562500173430408 ) ) ;
#42107 = ADVANCED_FACE ( 'NONE', ( #9282 ), #26196, .T. ) ;
#42108 = CARTESIAN_POINT ( 'NONE',  ( -97.65000000000001990, 88.47002178664754979, 83.70291666666668107 ) ) ;
#42109 = ORIENTED_EDGE ( 'NONE', *, *, #57755, .F. ) ;
#42110 = LINE ( 'NONE', #24084, #67172 ) ;
#42111 = CARTESIAN_POINT ( 'NONE',  ( 6.000000000000000000, -80.55351364060599906, 15.33399622253457295 ) ) ;
#42112 = VERTEX_POINT ( 'NONE', #39352 ) ;
#42113 = CYLINDRICAL_SURFACE ( 'NONE', #71968, 2.649999999999999467 ) ;
#42114 = CARTESIAN_POINT ( 'NONE',  ( -92.69370383062498320, -208.6684592857803011, 81.12322916753382174 ) ) ;
#42116 = ORIENTED_EDGE ( 'NONE', *, *, #25857, .T. ) ;
#42115 = ADVANCED_FACE ( 'NONE', ( #20933 ), #26939, .T. ) ;
#42117 = DIRECTION ( 'NONE',  ( -2.628368902995175337E-16, -1.000000000000000000, 0.000000000000000000 ) ) ;
#42118 = CARTESIAN_POINT ( 'NONE',  ( 10.00000000000000000, -27.13269053701114331, 25.88420570971391754 ) ) ;
#42119 = CYLINDRICAL_SURFACE ( 'NONE', #59709, 31.99999999999999289 ) ;
#42120 = CARTESIAN_POINT ( 'NONE',  ( 10.00000000000000000, 5.202137450156389953, 37.22597642581160216 ) ) ;
#42121 = AXIS2_PLACEMENT_3D ( 'NONE', #29336, #456, #52281 ) ;
#42122 = CARTESIAN_POINT ( 'NONE',  ( 0.000000000000000000, 21.53537804866126137, -30.80686688396986028 ) ) ;
#42123 = VECTOR ( 'NONE', #56805, 1000.000000000000000 ) ;
#42124 = CARTESIAN_POINT ( 'NONE',  ( 0.000000000000000000, -17.28742895386139722, 75.54627589209937355 ) ) ;
#42125 = CARTESIAN_POINT ( 'NONE',  ( -10.00000000000000000, 0.000000000000000000, 0.000000000000000000 ) ) ;
#42126 = LINE ( 'NONE', #74198, #32748 ) ;
#42127 = CIRCLE ( 'NONE', #63706, 37.49900000000001654 ) ;
#42128 = SHAPE_REPRESENTATION ( 'taper roller bearing_iso_ISO 355-2 - 2BD25 - 22,SI,NC,22', ( #43395 ), #57869 ) ;
#42129 = DIRECTION ( 'NONE',  ( 0.000000000000000000, -0.1564344650402170744, -0.9876883405951399908 ) ) ;
#42130 = EDGE_CURVE ( 'NONE', #52827, #57700, #73175, .T. ) ;
#42131 = DIRECTION ( 'NONE',  ( 0.000000000000000000, 0.000000000000000000, -1.000000000000000000 ) ) ;
#42132 = EDGE_CURVE ( 'NONE', #19022, #9704, #4793, .T. ) ;
#42133 = CARTESIAN_POINT ( 'NONE',  ( -97.30629616937501680, 88.66845928578038638, 76.36072916753381890 ) ) ;
#42134 = CARTESIAN_POINT ( 'NONE',  ( 10.00000000000000000, 17.67226234102826510, 33.17418723428314564 ) ) ;
#42135 = CARTESIAN_POINT ( 'NONE',  ( 15.00000000000000000, -19.89357724624986545, 12.59942793731086219 ) ) ;
#42136 = DIRECTION ( 'NONE',  ( 1.000000000000000000, 0.000000000000000000, 0.000000000000000000 ) ) ;
#42137 = DIRECTION ( 'NONE',  ( -1.000000000000000000, -0.000000000000000000, 0.000000000000000000 ) ) ;
#42138 = DIRECTION ( 'NONE',  ( 0.000000000000000000, 0.000000000000000000, -1.000000000000000000 ) ) ;
#42139 = EDGE_CURVE ( 'NONE', #16487, #47350, #10399, .T. ) ;
#42140 = EDGE_CURVE ( 'NONE', #1858, #32827, #62288, .T. ) ;
#42141 = DIRECTION ( 'NONE',  ( 0.000000000000000000, 0.000000000000000000, 1.000000000000000000 ) ) ;
#42142 = DIRECTION ( 'NONE',  ( 0.000000000000000000, -0.000000000000000000, -1.000000000000000000 ) ) ;
#42143 = DIRECTION ( 'NONE',  ( 0.000000000000000000, 0.9945218953682744001, -0.1045284632676436454 ) ) ;
#42144 = CARTESIAN_POINT ( 'NONE',  ( -97.64999999999994884, -211.5299782133524502, 86.87791666666664980 ) ) ;
#42145 = DIRECTION ( 'NONE',  ( -1.000000000000000000, 0.000000000000000000, 0.000000000000000000 ) ) ;
#42146 = ORIENTED_EDGE ( 'NONE', *, *, #17184, .F. ) ;
#42147 = CARTESIAN_POINT ( 'NONE',  ( 12.00000000000000000, 9.615535125378768200, -24.73947219025917121 ) ) ;
#42148 = DIRECTION ( 'NONE',  ( -1.000000000000000000, 0.000000000000000000, 0.000000000000000000 ) ) ;
#42149 = CARTESIAN_POINT ( 'NONE',  ( 10.00000000000000000, 0.000000000000000000, 0.000000000000000000 ) ) ;
#42150 = DIRECTION ( 'NONE',  ( 1.000000000000000000, -3.061616997868382648E-16, -0.000000000000000000 ) ) ;
#42151 = AXIS2_PLACEMENT_3D ( 'NONE', #52469, #25011, #41565 ) ;
#42152 = VECTOR ( 'NONE', #48292, 1000.000000000000000 ) ;
#42153 = CIRCLE ( 'NONE', #66144, 31.99999999999999289 ) ;
#42154 = FACE_OUTER_BOUND ( 'NONE', #21139, .T. ) ;
#42155 = ORIENTED_EDGE ( 'NONE', *, *, #56364, .T. ) ;
#42156 = CARTESIAN_POINT ( 'NONE',  ( 97.64999999999999147, -210.0000000024471092, 75.15687493081163950 ) ) ;
#42157 = DIRECTION ( 'NONE',  ( 0.000000000000000000, 0.000000000000000000, 1.000000000000000000 ) ) ;
#42158 = EDGE_LOOP ( 'NONE', ( #30522, #14162 ) ) ;
#42159 = CARTESIAN_POINT ( 'NONE',  ( 96.15314808468748708, -208.0026889286704943, 84.35114583420048007 ) ) ;
#42160 = CARTESIAN_POINT ( 'NONE',  ( 96.15314808468750130, -211.9973110713294489, 88.74322916753382628 ) ) ;
#42161 = EDGE_LOOP ( 'NONE', ( #50180, #341, #15411, #51680 ) ) ;
#42162 = CARTESIAN_POINT ( 'NONE',  ( 96.15314808468748708, -208.0026889286704943, 88.95489583420049939 ) ) ;
#42163 = VECTOR ( 'NONE', #19817, 1000.000000000000000 ) ;
#42164 = VERTEX_POINT ( 'NONE', #32580 ) ;
#42165 = CARTESIAN_POINT ( 'NONE',  ( -92.35000000000007958, -211.5299782133525071, 80.73958333333335702 ) ) ;
#42166 = ORIENTED_EDGE ( 'NONE', *, *, #48056, .F. ) ;
#42167 = CIRCLE ( 'NONE', #66167, 82.00000000000000000 ) ;
#42168 = CARTESIAN_POINT ( 'NONE',  ( -93.84685191531252713, 88.00268892867056536, 81.75822916753382685 ) ) ;
#42169 = AXIS2_PLACEMENT_3D ( 'NONE', #59677, #66070, #14542 ) ;
#42170 = EDGE_LOOP ( 'NONE', ( #54936, #65755, #51507, #68452 ) ) ;
#42171 = VERTEX_POINT ( 'NONE', #26574 ) ;
#42172 = CARTESIAN_POINT ( 'NONE',  ( -97.64999999969889188, -209.9999754409357422, 87.53856274002470172 ) ) ;
#42173 = EDGE_CURVE ( 'NONE', #24493, #43739, #70685, .T. ) ;
#42174 = VECTOR ( 'NONE', #14745, 1000.000000000000227 ) ;
#42175 = ORIENTED_EDGE ( 'NONE', *, *, #19333, .F. ) ;
#42176 = CYLINDRICAL_SURFACE ( 'NONE', #4111, 82.00000000000000000 ) ;
#42177 = ADVANCED_FACE ( 'NONE', ( #4408, #43529, #67923, #61174, #66806, #55528, #27303, #38228, #21676, #66442, #67548, #27693, #10775, #14925, #16039, #37870, #49508 ), #50616, .F. ) ;
#42178 = ORIENTED_EDGE ( 'NONE', *, *, #1935, .F. ) ;
#42179 = CARTESIAN_POINT ( 'NONE',  ( -2.500000000000003997, -4.330127018922192761, -6.000000000000000000 ) ) ;
#42180 = EDGE_CURVE ( 'NONE', #54092, #54682, #60802, .T. ) ;
#42181 = ORIENTED_EDGE ( 'NONE', *, *, #3592, .F. ) ;
#42182 = CYLINDRICAL_SURFACE ( 'NONE', #67224, 82.00000000000000000 ) ;
#42183 = VERTEX_POINT ( 'NONE', #33311 ) ;
#42184 = EDGE_CURVE ( 'NONE', #73572, #43336, #68366, .T. ) ;
#42185 = VERTEX_POINT ( 'NONE', #52100 ) ;
#42186 = VERTEX_POINT ( 'NONE', #40839 ) ;
#42187 = CARTESIAN_POINT ( 'NONE',  ( 96.15314808468750130, -211.9973110713294489, 77.78947916753381264 ) ) ;
#42188 = DIRECTION ( 'NONE',  ( -1.000000000000000000, 0.000000000000000000, 0.000000000000000000 ) ) ;
#42189 = DIRECTION ( 'NONE',  ( 0.000000000000000000, 0.000000000000000000, -1.000000000000000000 ) ) ;
#42190 = EDGE_LOOP ( 'NONE', ( #72187, #1231, #50741, #50558 ) ) ;
#42191 = DIRECTION ( 'NONE',  ( 0.000000000000000000, -0.3090169943749551673, -0.9510565162951510887 ) ) ;
#42192 = DIRECTION ( 'NONE',  ( 0.000000000000000000, 0.000000000000000000, 1.000000000000000000 ) ) ;
#42193 = EDGE_CURVE ( 'NONE', #34217, #16870, #27502, .T. ) ;
#42194 = CARTESIAN_POINT ( 'NONE',  ( -92.34999999999988063, -211.5299782133523649, 75.65958333333333030 ) ) ;
#42195 = CARTESIAN_POINT ( 'NONE',  ( 11.99999999999999822, 55.19960302592066625, 51.03279382321107249 ) ) ;
#42196 = CARTESIAN_POINT ( 'NONE',  ( 97.64999999999993463, -208.4700217866474077, 76.40041666666667197 ) ) ;
#42197 = CARTESIAN_POINT ( 'NONE',  ( -93.84685191531247028, -211.9973110713294489, 82.23447916753380582 ) ) ;
#42198 = CARTESIAN_POINT ( 'NONE',  ( -95.00000000000002842, 92.66308142843932671, 78.21281250086717307 ) ) ;
#42199 = ORIENTED_EDGE ( 'NONE', *, *, #12450, .F. ) ;
#42200 = CARTESIAN_POINT ( 'NONE',  ( 96.15314808468748708, 91.99731107132950569, 80.54114583420046358 ) ) ;
#42201 = ORIENTED_EDGE ( 'NONE', *, *, #40479, .F. ) ;
#42202 = DIRECTION ( 'NONE',  ( 1.000000000000000000, 0.000000000000000000, 0.000000000000000000 ) ) ;
#42203 = DIRECTION ( 'NONE',  ( 1.000000000000000000, 0.000000000000000000, 0.000000000000000000 ) ) ;
#42204 = EDGE_CURVE ( 'NONE', #31960, #9134, #57380, .T. ) ;
#42205 = CARTESIAN_POINT ( 'NONE',  ( 96.32499999999998863, 87.70503267997126784, 77.59104166840097605 ) ) ;
#42206 = DIRECTION ( 'NONE',  ( -1.000000000000000000, 0.000000000000000000, 0.000000000000000000 ) ) ;
#42207 = CARTESIAN_POINT ( 'NONE',  ( 10.00000000000000000, -2.946379043145784582, -75.11764819372150725 ) ) ;
#42208 = CARTESIAN_POINT ( 'NONE',  ( -94.99999999999997158, -207.3369185715606307, 83.76906250086715033 ) ) ;
#42209 = CIRCLE ( 'NONE', #69822, 77.49899999999999523 ) ;
#42210 = CARTESIAN_POINT ( 'NONE',  ( -9.937067298023317008, 7.583184918921300977, -44.99999999999998579 ) ) ;
#42211 = FACE_OUTER_BOUND ( 'NONE', #63905, .T. ) ;
#42212 = AXIS2_PLACEMENT_3D ( 'NONE', #67272, #26662, #15765 ) ;
#42213 = CYLINDRICAL_SURFACE ( 'NONE', #13065, 16.00000000000000000 ) ;
#42214 = ORIENTED_EDGE ( 'NONE', *, *, #9019, .F. ) ;
#42215 = AXIS2_PLACEMENT_3D ( 'NONE', #36932, #7624, #71502 ) ;
#42216 = ORIENTED_EDGE ( 'NONE', *, *, #54992, .F. ) ;
#42217 = LINE ( 'NONE', #48217, #72089 ) ;
#42218 = CARTESIAN_POINT ( 'NONE',  ( 92.35000000049315361, 89.99996796133687837, 83.73041644179049570 ) ) ;
#42219 = EDGE_CURVE ( 'NONE', #64362, #63204, #643, .T. ) ;
#42220 = LINE ( 'NONE', #9098, #49977 ) ;
#42221 = AXIS2_PLACEMENT_3D ( 'NONE', #12677, #1455, #709 ) ;
#42222 = EDGE_CURVE ( 'NONE', #72132, #21615, #6260, .T. ) ;
#42223 = CARTESIAN_POINT ( 'NONE',  ( -95.00000000000002842, 87.33691857156074434, 84.08656250086713158 ) ) ;
#42224 = LINE ( 'NONE', #60258, #58614 ) ;
#42225 = DIRECTION ( 'NONE',  ( 1.000000000000000000, -0.000000000000000000, -0.000000000000000000 ) ) ;
#42226 = CARTESIAN_POINT ( 'NONE',  ( 0.000000000000000000, 0.000000000000000000, 0.000000000000000000 ) ) ;
#42227 = DIRECTION ( 'NONE',  ( -1.000000000000000000, 0.000000000000000000, 0.000000000000000000 ) ) ;
#42228 =( BOUNDED_CURVE ( )  B_SPLINE_CURVE ( 2, ( #1271, #7234, #40330, #35062, #58736, #69641, #12121 ),
 .UNSPECIFIED., .F., .F. ) 
 B_SPLINE_CURVE_WITH_KNOTS ( ( 3, 2, 2, 3 ),
 ( 0.7083333333333331483, 0.7152777777777775681, 0.7222222222222220989, 0.7291666666666665186 ),
 .UNSPECIFIED. ) 
 CURVE ( )  GEOMETRIC_REPRESENTATION_ITEM ( )  RATIONAL_B_SPLINE_CURVE ( ( 1.000000000000004219, 0.8660254037844343777, 1.000000000000000000, 0.8660254037844387076, 1.000000000000000000, 0.8660254037844408170, 0.9999999999999978906 ) ) 
 REPRESENTATION_ITEM ( '' )  );
#42229 = ORIENTED_EDGE ( 'NONE', *, *, #48892, .F. ) ;
#42230 = CARTESIAN_POINT ( 'NONE',  ( -92.69370383062502583, 91.33154071421968467, 75.40822916753381833 ) ) ;
#42231 = DIRECTION ( 'NONE',  ( 0.000000000000000000, 0.000000000000000000, 1.000000000000000000 ) ) ;
#42232 = AXIS2_PLACEMENT_3D ( 'NONE', #56623, #46072, #33285 ) ;
#42233 = LINE ( 'NONE', #36204, #5890 ) ;
#42234 = CARTESIAN_POINT ( 'NONE',  ( 15.00000000000000000, 8.688484142254226938, 21.88630264137359305 ) ) ;
#42235 = CARTESIAN_POINT ( 'NONE',  ( -96.32499999999996021, -207.7050326799711968, 79.17854166840096752 ) ) ;
#42236 = CARTESIAN_POINT ( 'NONE',  ( -94.99999999999997158, -212.6630814284392557, 86.78531250086716398 ) ) ;
#42237 = AXIS2_PLACEMENT_3D ( 'NONE', #60451, #43900, #61558 ) ;
#42238 = CARTESIAN_POINT ( 'NONE',  ( 0.000000000000000000, 38.55633173627034438, -16.65560815589369881 ) ) ;
#42239 = DIRECTION ( 'NONE',  ( -1.000000000000000000, -0.000000000000000000, -0.000000000000000000 ) ) ;
#42240 = CARTESIAN_POINT ( 'NONE',  ( -97.30629616937495996, -209.9999999999999716, 76.46656250086715545 ) ) ;
#42241 = DIRECTION ( 'NONE',  ( -0.000000000000000000, 0.9781476007338042455, 0.2079116908177664758 ) ) ;
#42242 = ORIENTED_EDGE ( 'NONE', *, *, #9312, .F. ) ;
#42243 = CARTESIAN_POINT ( 'NONE',  ( 92.34999999999999432, 90.00000000000002842, 87.45999999999999375 ) ) ;
#42244 = LINE ( 'NONE', #30203, #63487 ) ;
#42245 = DIRECTION ( 'NONE',  ( -0.000000000000000000, -0.000000000000000000, -1.000000000000000000 ) ) ;
#42246 = DIRECTION ( 'NONE',  ( 0.000000000000000000, 0.000000000000000000, 1.000000000000000000 ) ) ;
#42247 = CARTESIAN_POINT ( 'NONE',  ( 92.69370383062501162, -208.6684592857803011, 87.20864583420049598 ) ) ;
#42248 = ORIENTED_EDGE ( 'NONE', *, *, #64890, .T. ) ;
#42249 = ADVANCED_FACE ( 'NONE', ( #23533 ), #29160, .F. ) ;
#42250 = CARTESIAN_POINT ( 'NONE',  ( 96.32499999999998863, 87.70503267997126784, 87.11604166840096752 ) ) ;
#42251 = DIRECTION ( 'NONE',  ( -1.000000000000000000, 0.000000000000000000, -0.000000000000000000 ) ) ;
#42252 = DIRECTION ( 'NONE',  ( -1.000000000000000000, 0.000000000000000000, -0.000000000000000000 ) ) ;
#42253 = ORIENTED_EDGE ( 'NONE', *, *, #41961, .T. ) ;
#42254 = CARTESIAN_POINT ( 'NONE',  ( 0.000000000000000000, -50.95692526931372157, 58.39081064771733054 ) ) ;
#42255 = ORIENTED_EDGE ( 'NONE', *, *, #11631, .T. ) ;
#42256 =( GEOMETRIC_REPRESENTATION_CONTEXT ( 3 ) GLOBAL_UNCERTAINTY_ASSIGNED_CONTEXT ( ( #9168 ) ) GLOBAL_UNIT_ASSIGNED_CONTEXT ( ( #64422, #35826, #64794 ) ) REPRESENTATION_CONTEXT ( 'NONE', 'WORKASPACE' ) );
#42257 = AXIS2_PLACEMENT_3D ( 'NONE', #52643, #69201, #28972 ) ;
#42258 = FACE_OUTER_BOUND ( 'NONE', #72821, .T. ) ;
#42259 = AXIS2_PLACEMENT_3D ( 'NONE', #16974, #1573, #29344 ) ;
#42260 = ORIENTED_EDGE ( 'NONE', *, *, #5539, .F. ) ;
#42261 = ORIENTED_EDGE ( 'NONE', *, *, #26477, .T. ) ;
#42262 = EDGE_CURVE ( 'NONE', #66486, #54478, #23918, .T. ) ;
#42263 = VERTEX_POINT ( 'NONE', #41201 ) ;
#42264 = DIRECTION ( 'NONE',  ( -0.000000000000000000, -0.000000000000000000, 1.000000000000000000 ) ) ;
#42265 = ADVANCED_FACE ( 'NONE', ( #45750 ), #63398, .F. ) ;
#42266 = CIRCLE ( 'NONE', #6270, 31.99999999999999645 ) ;
#42267 = ORIENTED_EDGE ( 'NONE', *, *, #4001, .T. ) ;
#42268 = CONICAL_SURFACE ( 'NONE', #53051, 13.71319123046128752, 0.2094395102393127317 ) ;
#42269 = EDGE_LOOP ( 'NONE', ( #36072, #37562, #5151, #49361 ) ) ;
#42270 = CARTESIAN_POINT ( 'NONE',  ( 96.15314808468748708, 91.99731107132950569, 79.42989583420049371 ) ) ;
#42271 = DIRECTION ( 'NONE',  ( -1.000000000000000000, 0.000000000000000000, 0.000000000000000000 ) ) ;
#42272 = CARTESIAN_POINT ( 'NONE',  ( 10.00000000000000000, 0.000000000000000000, 0.000000000000000000 ) ) ;
#42273 = ORIENTED_EDGE ( 'NONE', *, *, #57833, .F. ) ;
#42274 = EDGE_CURVE ( 'NONE', #25489, #72033, #40452, .T. ) ;
#42275 = ORIENTED_EDGE ( 'NONE', *, *, #52044, .F. ) ;
#42276 = ADVANCED_FACE ( 'NONE', ( #17887 ), #23176, .F. ) ;
#42277 = ORIENTED_EDGE ( 'NONE', *, *, #26585, .T. ) ;
#42278 = CARTESIAN_POINT ( 'NONE',  ( 11.99999999999999822, 73.73191006444551476, 14.66109333815590254 ) ) ;
#42279 = AXIS2_PLACEMENT_3D ( 'NONE', #23350, #51160, #46275 ) ;
#42280 = VERTEX_POINT ( 'NONE', #46846 ) ;
#42281 = TOROIDAL_SURFACE ( 'NONE', #60316, 13.10000000000000142, 0.5999999999999998668 ) ;
#42282 = DIRECTION ( 'NONE',  ( 0.9927274188295609481, 0.1203838523390816373, -2.034265265314174749E-17 ) ) ;
#42283 = CARTESIAN_POINT ( 'NONE',  ( 0.000000000000000000, 0.000000000000000000, 0.000000000000000000 ) ) ;
#42284 = CYLINDRICAL_SURFACE ( 'NONE', #56760, 31.99999999999998579 ) ;
#42285 = CARTESIAN_POINT ( 'NONE',  ( -95.00000000000002842, 90.00000000000004263, 90.00000000000000000 ) ) ;
#42286 = DIRECTION ( 'NONE',  ( -1.000000000000000000, 0.000000000000000000, 0.000000000000000000 ) ) ;
#42287 = CARTESIAN_POINT ( 'NONE',  ( 0.000000000000000000, -72.35432306680498016, 20.40083707022857951 ) ) ;
#42288 = CARTESIAN_POINT ( 'NONE',  ( -14.87942725330654348, -141.9795960975983178, 2.500000000000000000 ) ) ;
#42289 = CARTESIAN_POINT ( 'NONE',  ( -93.67499999999998295, -212.2949673200287179, 75.05104166840095559 ) ) ;
#42290 = CARTESIAN_POINT ( 'NONE',  ( 11.99999999999999822, 81.50828551894241514, -8.966570791699814080 ) ) ;
#42292 = CARTESIAN_POINT ( 'NONE',  ( -95.00000000000002842, 93.05995642670501411, 75.95062500173428077 ) ) ;
#42291 = CARTESIAN_POINT ( 'NONE',  ( 97.64999999999999147, 90.00000000000002842, 76.42687500173430237 ) ) ;
#42293 = ORIENTED_EDGE ( 'NONE', *, *, #42204, .F. ) ;
#42294 = CARTESIAN_POINT ( 'NONE',  ( 92.69370383062498320, 88.66845928578037217, 77.78947916753381264 ) ) ;
#42295 = EDGE_CURVE ( 'NONE', #56438, #40273, #28054, .T. ) ;
#42296 = CARTESIAN_POINT ( 'NONE',  ( 95.00000000000000000, -209.9999999999999716, 90.00000000000000000 ) ) ;
#42297 = LINE ( 'NONE', #65226, #72708 ) ;
#42298 = CARTESIAN_POINT ( 'NONE',  ( 5.000000000000000000, -26.79245525562738095, 32.34446384429961796 ) ) ;
#42299 = CARTESIAN_POINT ( 'NONE',  ( 10.00000000000000000, 30.80686688397041451, -21.53537804866048688 ) ) ;
#42300 = CARTESIAN_POINT ( 'NONE',  ( 11.99999999999999822, 50.23322058963348979, 64.81221759200361987 ) ) ;
#42301 = ORIENTED_EDGE ( 'NONE', *, *, #22693, .F. ) ;
#42302 = DIRECTION ( 'NONE',  ( 0.000000000000000000, 0.000000000000000000, -1.000000000000000000 ) ) ;
#42303 = DIRECTION ( 'NONE',  ( -1.000000000000000000, 0.000000000000000000, -0.000000000000000000 ) ) ;
#42304 = EDGE_LOOP ( 'NONE', ( #67322, #2638, #61478, #42930 ) ) ;
#42305 = ORIENTED_EDGE ( 'NONE', *, *, #35000, .F. ) ;
#42306 = EDGE_CURVE ( 'NONE', #10235, #27941, #32984, .T. ) ;
#42307 = CARTESIAN_POINT ( 'NONE',  ( 26.09152095774781799, -124.8716048804687375, -5.500000000000000000 ) ) ;
#42308 = PRODUCT_DEFINITION_SHAPE ( 'NONE', 'NONE',  #74376 ) ;
#42309 = LINE ( 'NONE', #60710, #69935 ) ;
#42310 = DIRECTION ( 'NONE',  ( 0.000000000000000000, 0.000000000000000000, 1.000000000000000000 ) ) ;
#42311 = DIRECTION ( 'NONE',  ( -1.000000000000000000, -0.000000000000000000, -0.000000000000000000 ) ) ;
#42312 = CARTESIAN_POINT ( 'NONE',  ( -93.84685191531248449, -208.0026889286704943, 74.98489583420048632 ) ) ;
#42313 = EDGE_CURVE ( 'NONE', #55375, #44604, #68670, .T. ) ;
#42314 = ORIENTED_EDGE ( 'NONE', *, *, #14147, .T. ) ;
#42315 = DIRECTION ( 'NONE',  ( 0.000000000000000000, 0.000000000000000000, 1.000000000000000000 ) ) ;
#42316 = DIRECTION ( 'NONE',  ( 0.5000000000000006661, -0.8660254037844383745, 0.000000000000000000 ) ) ;
#42317 = AXIS2_PLACEMENT_3D ( 'NONE', #45848, #17992, #17 ) ;
#42318 = DIRECTION ( 'NONE',  ( 0.000000000000000000, 0.000000000000000000, 1.000000000000000000 ) ) ;
#42319 = LINE ( 'NONE', #65253, #68949 ) ;
#42320 = DIRECTION ( 'NONE',  ( 0.000000000000000000, 0.000000000000000000, 1.000000000000000000 ) ) ;
#42321 = DIRECTION ( 'NONE',  ( -1.000000000000000000, 0.000000000000000000, -0.000000000000000000 ) ) ;
#42322 = DIRECTION ( 'NONE',  ( 7.962523111839282146E-16, -1.065814103640130873E-14, -1.000000000000000000 ) ) ;
#42323 = DIRECTION ( 'NONE',  ( 0.000000000000000000, -0.8660254037844384856, -0.5000000000000004441 ) ) ;
#42324 = CIRCLE ( 'NONE', #20675, 31.99999999999998579 ) ;
#42325 = CIRCLE ( 'NONE', #45929, 77.49899999999999523 ) ;
#42326 = CARTESIAN_POINT ( 'NONE',  ( 96.15314808468748708, 88.00268892867053694, 83.02822916753380866 ) ) ;
#42327 = CARTESIAN_POINT ( 'NONE',  ( -92.69370383062498320, -208.6684592857803295, 88.26697916753381890 ) ) ;
#42328 = CARTESIAN_POINT ( 'NONE',  ( 10.00000000000000000, 55.38113227695782115, 54.21277698773695164 ) ) ;
#42329 = VERTEX_POINT ( 'NONE', #281 ) ;
#42330 = CARTESIAN_POINT ( 'NONE',  ( 10.00000000000000000, -26.79245525562691199, -32.34446384430000876 ) ) ;
#42331 = CARTESIAN_POINT ( 'NONE',  ( -96.32499999999996021, -207.7050326799711968, 82.90916666666666401 ) ) ;
#42332 = CARTESIAN_POINT ( 'NONE',  ( -96.15314808468751551, 88.00268892867056536, 77.68364583420047609 ) ) ;
#42333 = CIRCLE ( 'NONE', #67487, 31.99999999999998579 ) ;
#42334 = VECTOR ( 'NONE', #46646, 1000.000000000000114 ) ;
#42335 = CARTESIAN_POINT ( 'NONE',  ( 92.69370383062501162, -209.9999999999999716, 87.73781250086713612 ) ) ;
#42336 = VERTEX_POINT ( 'NONE', #24281 ) ;
#42337 = VERTEX_POINT ( 'NONE', #48313 ) ;
#42338 = ORIENTED_EDGE ( 'NONE', *, *, #49150, .F. ) ;
#42339 = EDGE_CURVE ( 'NONE', #55666, #58910, #6644, .T. ) ;
#42340 = DIRECTION ( 'NONE',  ( -1.000000000000000000, 0.000000000000000000, -0.000000000000000000 ) ) ;
#42341 = FACE_OUTER_BOUND ( 'NONE', #39682, .T. ) ;
#42342 = EDGE_CURVE ( 'NONE', #766, #46613, #31009, .T. ) ;
#42343 = ORIENTED_EDGE ( 'NONE', *, *, #24846, .F. ) ;
#42344 = DIRECTION ( 'NONE',  ( -1.000000000000000000, -0.000000000000000000, 0.000000000000000000 ) ) ;
#42345 = CARTESIAN_POINT ( 'NONE',  ( 96.15314808468750130, -211.9973110713294489, 79.85322916753381151 ) ) ;
#42346 = EDGE_CURVE ( 'NONE', #19051, #25675, #19833, .T. ) ;
#42347 = CARTESIAN_POINT ( 'NONE',  ( -10.00000000000000000, 0.000000000000000000, 0.000000000000000000 ) ) ;
#42348 = LINE ( 'NONE', #2541, #26779 ) ;
#42349 = DIRECTION ( 'NONE',  ( 0.000000000000000000, 0.000000000000000000, 1.000000000000000000 ) ) ;
#42350 = CYLINDRICAL_SURFACE ( 'NONE', #12266, 2.649999999999985700 ) ;
#42351 = DIRECTION ( 'NONE',  ( 0.000000000000000000, 0.000000000000000000, -1.000000000000000000 ) ) ;
#42352 = CARTESIAN_POINT ( 'NONE',  ( 96.32499999999998863, -212.2949673200287179, 80.68666666666665321 ) ) ;
#42353 = ORIENTED_EDGE ( 'NONE', *, *, #44555, .F. ) ;
#42354 = EDGE_CURVE ( 'NONE', #33832, #62989, #30624, .T. ) ;
#42355 =( GEOMETRIC_REPRESENTATION_CONTEXT ( 3 ) GLOBAL_UNCERTAINTY_ASSIGNED_CONTEXT ( ( #54336 ) ) GLOBAL_UNIT_ASSIGNED_CONTEXT ( ( #33659, #3999, #22385 ) ) REPRESENTATION_CONTEXT ( 'NONE', 'WORKASPACE' ) );
#42356 = ORIENTED_EDGE ( 'NONE', *, *, #71768, .F. ) ;
#42357 = ORIENTED_EDGE ( 'NONE', *, *, #70512, .T. ) ;
#42358 = ORIENTED_EDGE ( 'NONE', *, *, #11953, .T. ) ;
#42359 = CARTESIAN_POINT ( 'NONE',  ( 92.35000000000000853, -209.9999999999999716, 86.82500000000000284 ) ) ;
#42360 = CIRCLE ( 'NONE', #5140, 77.49899999999999523 ) ;
#42361 = CARTESIAN_POINT ( 'NONE',  ( -92.69370383062502583, 88.66845928578038638, 84.98614583420047097 ) ) ;
#42362 = DIRECTION ( 'NONE',  ( 0.000000000000000000, -0.9876883405951394357, 0.1564344650402205716 ) ) ;
#42363 = DIRECTION ( 'NONE',  ( 0.000000000000000000, 0.000000000000000000, -1.000000000000000000 ) ) ;
#42364 = CARTESIAN_POINT ( 'NONE',  ( 92.34999999999999432, 90.00000000000002842, 76.03000000000000114 ) ) ;
#42365 = ORIENTED_EDGE ( 'NONE', *, *, #67900, .F. ) ;
#42366 = DIRECTION ( 'NONE',  ( -0.000000000000000000, -0.000000000000000000, -1.000000000000000000 ) ) ;
#42367 = ORIENTED_EDGE ( 'NONE', *, *, #31381, .T. ) ;
#42368 = DIRECTION ( 'NONE',  ( 0.000000000000000000, 0.000000000000000000, -1.000000000000000000 ) ) ;
#42369 = EDGE_CURVE ( 'NONE', #29284, #61762, #70121, .T. ) ;
#42370 = ORIENTED_EDGE ( 'NONE', *, *, #27466, .T. ) ;
#42371 = CARTESIAN_POINT ( 'NONE',  ( -92.35000000000005116, 88.47002178664754979, 86.53395833506763779 ) ) ;
#42372 = AXIS2_PLACEMENT_3D ( 'NONE', #56685, #73951, #16077 ) ;
#42373 = CARTESIAN_POINT ( 'NONE',  ( 97.30629616937498838, 91.33154071421968467, 87.63197916753382799 ) ) ;
#42374 = EDGE_CURVE ( 'NONE', #27626, #69665, #25006, .T. ) ;
#42375 = CARTESIAN_POINT ( 'NONE',  ( 97.64999999994533653, -210.0000170172949367, 88.49187441316098557 ) ) ;
#42376 = CARTESIAN_POINT ( 'NONE',  ( -16.06301359042743115, -102.7814171781257357, 5.500000000000000000 ) ) ;
#42377 = CARTESIAN_POINT ( 'NONE',  ( -92.34999999999999432, -210.0000154727988217, 78.33187446658357089 ) ) ;
#42378 = PLANE ( 'NONE',  #5939 ) ;
#42379 = EDGE_LOOP ( 'NONE', ( #1259, #50191 ) ) ;
#42380 = DIRECTION ( 'NONE',  ( 0.000000000000000000, 0.000000000000000000, 1.000000000000000000 ) ) ;
#42381 = AXIS2_PLACEMENT_3D ( 'NONE', #15012, #65788, #65429 ) ;
#42382 = EDGE_CURVE ( 'NONE', #37462, #14784, #25390, .T. ) ;
#42383 = CARTESIAN_POINT ( 'NONE',  ( -94.99999999999997158, -207.3369185715606307, 74.87906250086713555 ) ) ;
#42384 = VERTEX_POINT ( 'NONE', #42676 ) ;
#42385 = ORIENTED_EDGE ( 'NONE', *, *, #73834, .T. ) ;
#42386 = DIRECTION ( 'NONE',  ( -0.000000000000000000, -1.156482317317870936E-15, -1.000000000000000000 ) ) ;
#42387 = ADVANCED_FACE ( 'NONE', ( #36658 ), #4248, .F. ) ;
#42388 = FACE_OUTER_BOUND ( 'NONE', #5570, .T. ) ;
#42389 = CARTESIAN_POINT ( 'NONE',  ( -97.65000000000001990, 91.52997821335253548, 75.42145833506764063 ) ) ;
#42390 = CARTESIAN_POINT ( 'NONE',  ( -92.69370383062498320, -211.3315407142195852, 86.25614583420048120 ) ) ;
#42391 = VERTEX_POINT ( 'NONE', #7359 ) ;
#42392 = LINE ( 'NONE', #37123, #9291 ) ;
#42393 = VERTEX_POINT ( 'NONE', #53219 ) ;
#42394 = ORIENTED_EDGE ( 'NONE', *, *, #42262, .T. ) ;
#42395 = CARTESIAN_POINT ( 'NONE',  ( 11.99999999999999822, 75.11725578898472122, -2.956366410619845730 ) ) ;
#42396 = DIRECTION ( 'NONE',  ( 0.000000000000000000, 0.000000000000000000, 1.000000000000000000 ) ) ;
#42397 = DIRECTION ( 'NONE',  ( 1.000000000000000000, -0.000000000000000000, -0.000000000000000000 ) ) ;
#42398 = CARTESIAN_POINT ( 'NONE',  ( 97.30629616937498838, 88.66845928578035796, 81.01739583420048518 ) ) ;
#42399 = DIRECTION ( 'NONE',  ( -0.9918136447140101231, 0.1276937514489694114, 0.000000000000000000 ) ) ;
#42400 = LINE ( 'NONE', #19820, #36184 ) ;
#42401 = CYLINDRICAL_SURFACE ( 'NONE', #59174, 12.50000000000000000 ) ;
#42402 = DIRECTION ( 'NONE',  ( 0.000000000000000000, 0.000000000000000000, 1.000000000000000000 ) ) ;
#42403 = CARTESIAN_POINT ( 'NONE',  ( -1.474095553543409487, -120.2775649455957989, 2.500000000000000000 ) ) ;
#42404 = LINE ( 'NONE', #29999, #23107 ) ;
#42405 = AXIS2_PLACEMENT_3D ( 'NONE', #51364, #58123, #45757 ) ;
#42406 = DIRECTION ( 'NONE',  ( -1.000000000000000000, -0.000000000000000000, -0.000000000000000000 ) ) ;
#42407 = PRODUCT_DEFINITION_CONTEXT ( 'detailed design', #70024, 'design' ) ;
#42408 = AXIS2_PLACEMENT_3D ( 'NONE', #73785, #43761, #21926 ) ;
#42409 = CARTESIAN_POINT ( 'NONE',  ( 1.560000000000000053, -0.8660254037844384856, 1.500000000000000000 ) ) ;
#42410 = VERTEX_POINT ( 'NONE', #18621 ) ;
#42411 = CARTESIAN_POINT ( 'NONE',  ( -96.15314808468752972, 91.99731107132950569, 87.63197916753379957 ) ) ;
#42412 = CARTESIAN_POINT ( 'NONE',  ( 0.000000000000000000, -34.94270380257585629, -74.18225833017926618 ) ) ;
#42413 = VECTOR ( 'NONE', #23301, 1000.000000000000000 ) ;
#42414 = CARTESIAN_POINT ( 'NONE',  ( -12.50000000000000000, -107.5000000000000000, 40.00000000000000000 ) ) ;
#42415 = ORIENTED_EDGE ( 'NONE', *, *, #21102, .F. ) ;
#42416 = AXIS2_PLACEMENT_3D ( 'NONE', #33647, #61493, #58340 ) ;
#42417 =( BOUNDED_CURVE ( )  B_SPLINE_CURVE ( 2, ( #22999, #57204, #40649, #10967, #69586, #1213, #28242, #5711, #51177 ),
 .UNSPECIFIED., .F., .F. ) 
 B_SPLINE_CURVE_WITH_KNOTS ( ( 3, 2, 2, 2, 3 ),
 ( 0.000000000000000000, 0.007055765540882327075, 0.01411153108176465415, 0.02116729662264698122, 0.02116741234828206988 ),
 .UNSPECIFIED. ) 
 CURVE ( )  GEOMETRIC_REPRESENTATION_ITEM ( )  RATIONAL_B_SPLINE_CURVE ( ( 1.000000000000000000, 0.8660254037844387076, 1.000000000000000000, 0.8660254037844387076, 1.000000000000000000, 0.8660254037844387076, 1.000000000000000000, 0.9999978026062312786, 0.9999956052845440091 ) ) 
 REPRESENTATION_ITEM ( '' )  );
#42418 = LINE ( 'NONE', #13824, #49866 ) ;
#42420 = DIRECTION ( 'NONE',  ( -0.000000000000000000, -1.156482317317870936E-15, -1.000000000000000000 ) ) ;
#42419 = CIRCLE ( 'NONE', #20843, 31.99999999999997868 ) ;
#42421 = CARTESIAN_POINT ( 'NONE',  ( 10.00000000000000000, 44.88180994100376608, 63.18004540533043922 ) ) ;
#42422 = EDGE_CURVE ( 'NONE', #53797, #70803, #43058, .T. ) ;
#42423 = AXIS2_PLACEMENT_3D ( 'NONE', #23267, #57850, #64972 ) ;
#42424 = AXIS2_PLACEMENT_3D ( 'NONE', #36110, #46653, #47031 ) ;
#42425 = AXIS2_PLACEMENT_3D ( 'NONE', #22818, #57023, #46109 ) ;
#42426 = CARTESIAN_POINT ( 'NONE',  ( 97.30629616937498838, -209.9999999999999716, 83.13406250086715943 ) ) ;
#42427 = EDGE_CURVE ( 'NONE', #13981, #58816, #7722, .T. ) ;
#42428 = ADVANCED_FACE ( 'NONE', ( #59229 ), #19365, .T. ) ;
#42429 = VERTEX_POINT ( 'NONE', #13356 ) ;
#42430 = ADVANCED_FACE ( 'NONE', ( #41558 ), #8089, .T. ) ;
#42431 = EDGE_LOOP ( 'NONE', ( #26928, #67620, #13426, #15885 ) ) ;
#42432 = CARTESIAN_POINT ( 'NONE',  ( 0.000000000000000000, 0.000000000000000000, 0.000000000000000000 ) ) ;
#42433 = ORIENTED_EDGE ( 'NONE', *, *, #47134, .T. ) ;
#42434 = CARTESIAN_POINT ( 'NONE',  ( -57.50000000000000000, 0.000000000000000000, -275.0000000000000000 ) ) ;
#42435 = EDGE_CURVE ( 'NONE', #38013, #19224, #18611, .T. ) ;
#42436 = CARTESIAN_POINT ( 'NONE',  ( 12.50000000000000000, -107.5000000000000000, -2.500000000000000000 ) ) ;
#42437 = ORIENTED_EDGE ( 'NONE', *, *, #40841, .T. ) ;
#42438 = CARTESIAN_POINT ( 'NONE',  ( 93.84685191531251292, -211.9973110713294489, 79.11239583420048405 ) ) ;
#42439 = EDGE_CURVE ( 'NONE', #41715, #1281, #16248, .T. ) ;
#42440 = ORIENTED_EDGE ( 'NONE', *, *, #60377, .F. ) ;
#42441 = DIRECTION ( 'NONE',  ( -0.000000000000000000, -0.000000000000000000, 1.000000000000000000 ) ) ;
#42442 = VERTEX_POINT ( 'NONE', #31380 ) ;
#42443 = EDGE_LOOP ( 'NONE', ( #1146, #35589, #69720, #58461 ) ) ;
#42444 = CARTESIAN_POINT ( 'NONE',  ( 3.429551818649054340, -146.3199197248623875, 5.500000000000000000 ) ) ;
#42445 = CARTESIAN_POINT ( 'NONE',  ( -96.32500000000001705, 92.29496732002878900, 82.90916666666666401 ) ) ;
#42446 = VERTEX_POINT ( 'NONE', #65250 ) ;
#42447 = CARTESIAN_POINT ( 'NONE',  ( 0.000000000000000000, 9.188173127307898369, -40.98264845739739570 ) ) ;
#42448 = CARTESIAN_POINT ( 'NONE',  ( 93.67500000000001137, -207.7050326799711968, 84.25854166840096582 ) ) ;
#42449 = CARTESIAN_POINT ( 'NONE',  ( 97.64999999999999147, 90.00000000000002842, 86.50750000000000739 ) ) ;
#42450 = VERTEX_POINT ( 'NONE', #48682 ) ;
#42451 = CARTESIAN_POINT ( 'NONE',  ( -0.0004442498525516064278, 0.001194404164626844313, -90.00000000000000000 ) ) ;
#42452 = DIRECTION ( 'NONE',  ( 0.000000000000000000, 0.000000000000000000, 1.000000000000000000 ) ) ;
#42453 = VECTOR ( 'NONE', #3229, 1000.000000000000000 ) ;
#42454 = VERTEX_POINT ( 'NONE', #20099 ) ;
#42455 = VERTEX_POINT ( 'NONE', #6975 ) ;
#42456 = CARTESIAN_POINT ( 'NONE',  ( -93.84685191531252713, 88.00268892867056536, 88.10822916753382117 ) ) ;
#42457 = CARTESIAN_POINT ( 'NONE',  ( 92.69370383062498320, 88.66845928578037217, 80.80572916753382628 ) ) ;
#42458 = ADVANCED_FACE ( 'NONE', ( #29898 ), #52852, .F. ) ;
#42459 = VERTEX_POINT ( 'NONE', #73078 ) ;
#42460 = CARTESIAN_POINT ( 'NONE',  ( 96.32499999999998863, 87.70503267997126784, 85.21104166840096639 ) ) ;
#42461 = ADVANCED_FACE ( 'NONE', ( #26860 ), #67086, .F. ) ;
#42462 = CARTESIAN_POINT ( 'NONE',  ( 0.000000000000000000, -27.13269053701078448, -25.88420570971428702 ) ) ;
#42463 = ORIENTED_EDGE ( 'NONE', *, *, #24044, .F. ) ;
#42464 = PLANE ( 'NONE',  #29669 ) ;
#42465 = EDGE_CURVE ( 'NONE', #3369, #72495, #9198, .T. ) ;
#42466 = EDGE_CURVE ( 'NONE', #40405, #28568, #2060, .T. ) ;
#42467 = ORIENTED_EDGE ( 'NONE', *, *, #5552, .T. ) ;
#42468 = AXIS2_PLACEMENT_3D ( 'NONE', #54365, #37458, #43099 ) ;
#42469 = ORIENTED_EDGE ( 'NONE', *, *, #56561, .F. ) ;
#42470 = ORIENTED_EDGE ( 'NONE', *, *, #32053, .T. ) ;
#42471 = CARTESIAN_POINT ( 'NONE',  ( -92.34999999999996589, 91.52997821335250705, 85.92541666666664923 ) ) ;
#42472 = CARTESIAN_POINT ( 'NONE',  ( 0.000000000000000000, -0.6853352020787742971, -37.58145647212455032 ) ) ;
#42473 = CARTESIAN_POINT ( 'NONE',  ( -92.35000000000005116, 91.52997821335253548, 84.65541666666666742 ) ) ;
#42474 = VERTEX_POINT ( 'NONE', #9938 ) ;
#42475 = EDGE_CURVE ( 'NONE', #13138, #15732, #10312, .T. ) ;
#42476 = DIRECTION ( 'NONE',  ( 0.000000000000000000, 0.000000000000000000, 1.000000000000000000 ) ) ;
#42477 = AXIS2_PLACEMENT_3D ( 'NONE', #20704, #32345, #54548 ) ;
#42478 = DIRECTION ( 'NONE',  ( -1.000000000000000000, -0.000000000000000000, 0.000000000000000000 ) ) ;
#42479 = ORIENTED_EDGE ( 'NONE', *, *, #55536, .T. ) ;
#42480 = DIRECTION ( 'NONE',  ( -1.000000000000000000, -0.000000000000000000, -0.000000000000000000 ) ) ;
#42481 = CARTESIAN_POINT ( 'NONE',  ( -93.84685191531248449, -208.0026889286704943, 83.71614583420047495 ) ) ;
#42482 = VERTEX_POINT ( 'NONE', #67832 ) ;
#42483 = DIRECTION ( 'NONE',  ( 0.3853207896976533209, -0.9227826878668545785, 0.000000000000000000 ) ) ;
#42484 = DIRECTION ( 'NONE',  ( 0.000000000000000000, 0.000000000000000000, 1.000000000000000000 ) ) ;
#42485 = CARTESIAN_POINT ( 'NONE',  ( -3.000000000000000000, 14.60985201121704513, 18.46759930825707841 ) ) ;
#42486 = DIRECTION ( 'NONE',  ( -2.628368902995164490E-16, -1.000000000000000000, 0.000000000000000000 ) ) ;
#42487 = CARTESIAN_POINT ( 'NONE',  ( 92.35000000049316782, -210.0000320386632495, 83.73041644179299681 ) ) ;
#42488 = VECTOR ( 'NONE', #61549, 1000.000000000000000 ) ;
#42489 = AXIS2_PLACEMENT_3D ( 'NONE', #55253, #73278, #20670 ) ;
#42490 = DIRECTION ( 'NONE',  ( 0.000000000000000000, 0.000000000000000000, 1.000000000000000000 ) ) ;
#42491 = CARTESIAN_POINT ( 'NONE',  ( -96.32499999999996021, -212.2949673200287179, 85.66083333333332916 ) ) ;
#42492 = CARTESIAN_POINT ( 'NONE',  ( 96.32499999999997442, 92.29496732002878900, 82.88270833506763324 ) ) ;
#42493 = DIRECTION ( 'NONE',  ( 0.000000000000000000, 0.000000000000000000, 1.000000000000000000 ) ) ;
#42494 = CARTESIAN_POINT ( 'NONE',  ( -95.00000000000002842, 92.66308142843932671, 89.64281250086715147 ) ) ;
#42495 = FACE_OUTER_BOUND ( 'NONE', #39785, .T. ) ;
#42496 = CARTESIAN_POINT ( 'NONE',  ( -10.00000000000000000, 0.000000000000000000, 0.000000000000000000 ) ) ;
#42497 = FACE_OUTER_BOUND ( 'NONE', #49802, .T. ) ;
#42498 = DIRECTION ( 'NONE',  ( -1.000000000000000000, -0.000000000000000000, -0.000000000000000000 ) ) ;
#42499 = CARTESIAN_POINT ( 'NONE',  ( 0.000000000000000000, 30.80686688397041451, -21.53537804866048688 ) ) ;
#42500 = FACE_OUTER_BOUND ( 'NONE', #21798, .T. ) ;
#42501 = FACE_OUTER_BOUND ( 'NONE', #21010, .T. ) ;
#42502 = CARTESIAN_POINT ( 'NONE',  ( 92.35000000005783249, 89.99998877583867340, 75.47473230081648410 ) ) ;
#42503 = CARTESIAN_POINT ( 'NONE',  ( -92.34999999999999432, -208.4700217866474645, 87.83041666666666458 ) ) ;
#42504 = DIRECTION ( 'NONE',  ( 1.000000000000000000, 0.000000000000000000, 0.000000000000000000 ) ) ;
#42505 = AXIS2_PLACEMENT_3D ( 'NONE', #67539, #17514, #32936 ) ;
#42506 = ORIENTED_EDGE ( 'NONE', *, *, #4612, .T. ) ;
#42507 = DIRECTION ( 'NONE',  ( -1.000000000000000000, -0.000000000000000000, -0.000000000000000000 ) ) ;
#42508 = DIRECTION ( 'NONE',  ( 1.000000000000000000, -0.000000000000000000, 0.000000000000000000 ) ) ;
#42509 = CARTESIAN_POINT ( 'NONE',  ( 0.000000000000000000, 0.000000000000000000, 0.000000000000000000 ) ) ;
#42510 = CIRCLE ( 'NONE', #19686, 31.99999999999999289 ) ;
#42511 = DIRECTION ( 'NONE',  ( 0.000000000000000000, 0.8660254037844432595, -0.4999999999999920064 ) ) ;
#42512 = ADVANCED_FACE ( 'NONE', ( #32861 ), #44911, .F. ) ;
#42513 = EDGE_CURVE ( 'NONE', #4178, #71089, #27023, .T. ) ;
#42514 = ORIENTED_EDGE ( 'NONE', *, *, #10449, .F. ) ;
#42515 = EDGE_CURVE ( 'NONE', #56886, #22041, #33229, .T. ) ;
#42516 = DIRECTION ( 'NONE',  ( -1.000000000000000000, -0.000000000000000000, -0.000000000000000000 ) ) ;
#42517 = CARTESIAN_POINT ( 'NONE',  ( -92.34999999999999432, -210.0000000207151629, 80.87187500099602744 ) ) ;
#42518 = ORIENTED_EDGE ( 'NONE', *, *, #64087, .F. ) ;
#42519 = AXIS2_PLACEMENT_3D ( 'NONE', #18756, #58615, #19497 ) ;
#42520 = CARTESIAN_POINT ( 'NONE',  ( 95.00000000000000000, -207.3369185715606307, 81.86406250086713499 ) ) ;
#42521 = CARTESIAN_POINT ( 'NONE',  ( 92.69370383062501162, -208.6684592857803295, 87.20864583420048177 ) ) ;
#42522 = VERTEX_POINT ( 'NONE', #27212 ) ;
#42523 = CARTESIAN_POINT ( 'NONE',  ( 97.30629616937498838, -208.6684592857803011, 88.26697916753381890 ) ) ;
#42524 = EDGE_LOOP ( 'NONE', ( #141, #31694, #23788, #4095 ) ) ;
#42525 = VECTOR ( 'NONE', #53969, 1000.000000000000000 ) ;
#42526 = FACE_BOUND ( 'NONE', #59253, .T. ) ;
#42527 = ORIENTED_EDGE ( 'NONE', *, *, #70833, .T. ) ;
#42528 = AXIS2_PLACEMENT_3D ( 'NONE', #20117, #32132, #43078 ) ;
#42529 = CARTESIAN_POINT ( 'NONE',  ( -95.00000000000002842, 87.33691857156074434, 75.99031250086716227 ) ) ;
#42530 = ORIENTED_EDGE ( 'NONE', *, *, #44507, .F. ) ;
#42531 = ORIENTED_EDGE ( 'NONE', *, *, #72952, .F. ) ;
#42532 = CARTESIAN_POINT ( 'NONE',  ( 4.999999999999999112, -21.40280677340345505, -36.13751322684441192 ) ) ;
#42533 = EDGE_LOOP ( 'NONE', ( #15747, #42916, #49291, #30356 ) ) ;
#42534 = DIRECTION ( 'NONE',  ( -1.000000000000000000, 0.000000000000000000, 0.000000000000000000 ) ) ;
#42535 = CARTESIAN_POINT ( 'NONE',  ( 93.67500000000001137, -212.2949673200287179, 79.31083333333333485 ) ) ;
#42536 = ADVANCED_FACE ( 'NONE', ( #55059 ), #3590, .T. ) ;
#42537 = ORIENTED_EDGE ( 'NONE', *, *, #45249, .F. ) ;
#42538 = CARTESIAN_POINT ( 'NONE',  ( 0.000000000000000000, 0.000000000000000000, 0.000000000000000000 ) ) ;
#42539 = AXIS2_PLACEMENT_3D ( 'NONE', #48799, #20607, #14211 ) ;
#42540 = ORIENTED_EDGE ( 'NONE', *, *, #2840, .F. ) ;
#42541 = CARTESIAN_POINT ( 'NONE',  ( -26.50000000000000355, -120.0000000000000000, -64.00000000000000000 ) ) ;
#42542 = ORIENTED_EDGE ( 'NONE', *, *, #48819, .T. ) ;
#42543 = CIRCLE ( 'NONE', #53330, 31.99999999999999289 ) ;
#42544 = ORIENTED_EDGE ( 'NONE', *, *, #3119, .F. ) ;
#42545 = VERTEX_POINT ( 'NONE', #27603 ) ;
#42546 = CARTESIAN_POINT ( 'NONE',  ( 97.30629616937498838, -208.6684592857803011, 79.21822916753380639 ) ) ;
#42548 = ADVANCED_FACE ( 'NONE', ( #8836, #49046 ), #50144, .F. ) ;
#42547 = FACE_OUTER_BOUND ( 'NONE', #24331, .T. ) ;
#42549 = ADVANCED_FACE ( 'NONE', ( #26856 ), #31751, .F. ) ;
#42550 = CARTESIAN_POINT ( 'NONE',  ( -97.65000000000000568, 88.47002178664753558, 81.79791666666665151 ) ) ;
#42551 = ORIENTED_EDGE ( 'NONE', *, *, #16579, .F. ) ;
#42552 = CARTESIAN_POINT ( 'NONE',  ( 0.000000000000000000, 0.000000000000000000, 0.000000000000000000 ) ) ;
#42553 = ORIENTED_EDGE ( 'NONE', *, *, #53884, .F. ) ;
#42554 = CARTESIAN_POINT ( 'NONE',  ( -95.00000000000002842, 86.94004357329504273, 80.63375000000000625 ) ) ;
#42555 = DIRECTION ( 'NONE',  ( -1.000000000000000000, 0.000000000000000000, -0.000000000000000000 ) ) ;
#42556 = CARTESIAN_POINT ( 'NONE',  ( 11.99999999999999822, 68.55367621811141987, 44.99326035066078333 ) ) ;
#42557 = DIRECTION ( 'NONE',  ( 2.603472992746261562E-14, 2.546204323184492723E-14, -1.000000000000000000 ) ) ;
#42558 = CARTESIAN_POINT ( 'NONE',  ( -97.30629616937497417, -211.3315407142195852, 82.07572916753380809 ) ) ;
#42559 = CARTESIAN_POINT ( 'NONE',  ( -97.30629616937501680, 88.66845928578038638, 78.42447916753380355 ) ) ;
#42560 = ORIENTED_EDGE ( 'NONE', *, *, #37379, .F. ) ;
#42561 = VECTOR ( 'NONE', #58856, 1000.000000000000000 ) ;
#42562 = CARTESIAN_POINT ( 'NONE',  ( 97.30629616937498838, 91.33154071421968467, 82.39322916753381776 ) ) ;
#42563 = ORIENTED_EDGE ( 'NONE', *, *, #50517, .T. ) ;
#42564 = PLANE ( 'NONE',  #10689 ) ;
#42565 = DIRECTION ( 'NONE',  ( 0.000000000000000000, 0.000000000000000000, -1.000000000000000000 ) ) ;
#42566 = CARTESIAN_POINT ( 'NONE',  ( 92.35004024445044024, 88.46999855150322389, 77.43229327564787923 ) ) ;
#42567 = CARTESIAN_POINT ( 'NONE',  ( -3.000000000000000000, -20.55727247249726020, -16.78983467731313084 ) ) ;
#42568 = CARTESIAN_POINT ( 'NONE',  ( 6.000000000000000000, -81.50828551894220197, -8.966570791701593990 ) ) ;
#42569 = CARTESIAN_POINT ( 'NONE',  ( -96.15314808468747287, -208.0026889286704943, 81.91697916753381037 ) ) ;
#42570 = CARTESIAN_POINT ( 'NONE',  ( 97.65000000000000568, 88.47002178664753558, 87.08958333333333712 ) ) ;
#42571 = CARTESIAN_POINT ( 'NONE',  ( -10.00000000000000000, 0.000000000000000000, 0.000000000000000000 ) ) ;
#42572 = FACE_OUTER_BOUND ( 'NONE', #13588, .T. ) ;
#42573 = ORIENTED_EDGE ( 'NONE', *, *, #16311, .T. ) ;
#42574 = AXIS2_PLACEMENT_3D ( 'NONE', #65745, #70996, #66493 ) ;
#42575 = ORIENTED_EDGE ( 'NONE', *, *, #23932, .F. ) ;
#42576 = DIRECTION ( 'NONE',  ( -1.000000000000000000, -0.000000000000000000, 0.000000000000000000 ) ) ;
#42577 = DIRECTION ( 'NONE',  ( 0.000000000000000000, 0.000000000000000000, 1.000000000000000000 ) ) ;
#42578 = CARTESIAN_POINT ( 'NONE',  ( 95.00000000002597744, 90.00000000000007105, -65.00000000000000000 ) ) ;
#42579 = CARTESIAN_POINT ( 'NONE',  ( -93.84685191531254134, 91.99731107132950569, 84.35114583420048007 ) ) ;
#42580 = DIRECTION ( 'NONE',  ( 0.000000000000000000, 0.9510565162951523099, 0.3090169943749517811 ) ) ;
#42581 = CARTESIAN_POINT ( 'NONE',  ( 10.00000000000000000, -0.8828120875903202602, 37.48860685352291000 ) ) ;
#42582 = CARTESIAN_POINT ( 'NONE',  ( 0.000000000000000000, 0.000000000000000000, 0.000000000000000000 ) ) ;
#42583 = AXIS2_PLACEMENT_3D ( 'NONE', #16246, #72625, #61749 ) ;
#42584 = ORIENTED_EDGE ( 'NONE', *, *, #52217, .F. ) ;
#42585 = AXIS2_PLACEMENT_3D ( 'NONE', #73034, #73416, #4285 ) ;
#42586 = CARTESIAN_POINT ( 'NONE',  ( -93.84685191531254134, 91.99731107132950569, 76.73114583420047552 ) ) ;
#42587 = AXIS2_PLACEMENT_3D ( 'NONE', #40764, #29451, #70050 ) ;
#42588 = DIRECTION ( 'NONE',  ( 0.000000000000000000, 0.000000000000000000, 1.000000000000000000 ) ) ;
#42589 = DIRECTION ( 'NONE',  ( -1.000000000000000000, 0.000000000000000000, -0.000000000000000000 ) ) ;
#42590 = CARTESIAN_POINT ( 'NONE',  ( 0.000000000000000000, 0.000000000000000000, 0.000000000000000000 ) ) ;
#42591 = DIRECTION ( 'NONE',  ( 0.000000000000000000, 0.5224985647159440250, 0.8526401643540951758 ) ) ;
#42592 = CARTESIAN_POINT ( 'NONE',  ( 92.35000000000007958, 88.47002178664747873, 86.24291666666667311 ) ) ;
#42593 = CARTESIAN_POINT ( 'NONE',  ( -97.30629616937495996, -209.9999999999999716, 81.54656250086715374 ) ) ;
#42594 =( NAMED_UNIT ( * ) SI_UNIT ( $, .STERADIAN. ) SOLID_ANGLE_UNIT ( ) );
#42595 = AXIS2_PLACEMENT_3D ( 'NONE', #51176, #57941, #46289 ) ;
#42596 = CARTESIAN_POINT ( 'NONE',  ( 10.00000000000000000, -38.55633173627023069, 16.65560815589396526 ) ) ;
#42597 = CIRCLE ( 'NONE', #31781, 77.49899999999999523 ) ;
#42598 = CARTESIAN_POINT ( 'NONE',  ( 10.00000000000000000, -40.98264845739755913, 9.188173127307164734 ) ) ;
#42599 = PRODUCT_RELATED_PRODUCT_CATEGORY ( 'part', '', ( #49365 ) ) ;
#42600 = AXIS2_PLACEMENT_3D ( 'NONE', #16481, #23242, #17590 ) ;
#42601 = ADVANCED_FACE ( 'NONE', ( #3956, #60718 ), #61077, .F. ) ;
#42602 = FACE_OUTER_BOUND ( 'NONE', #56862, .T. ) ;
#42603 = LINE ( 'NONE', #61377, #47804 ) ;
#42604 = ORIENTED_EDGE ( 'NONE', *, *, #50257, .F. ) ;
#42605 = DIRECTION ( 'NONE',  ( -1.000000000000000000, -0.000000000000000000, -0.000000000000000000 ) ) ;
#42606 = CARTESIAN_POINT ( 'NONE',  ( -97.65000000000001990, 90.00000000000004263, 90.00000000000000000 ) ) ;
#42607 = CYLINDRICAL_SURFACE ( 'NONE', #67812, 77.49899999999999523 ) ;
#42608 = EDGE_CURVE ( 'NONE', #56328, #37934, #32493, .T. ) ;
#42609 = CARTESIAN_POINT ( 'NONE',  ( 11.99999999999999822, 0.000000000000000000, 0.000000000000000000 ) ) ;
#42610 = CARTESIAN_POINT ( 'NONE',  ( 97.30629616937498838, -209.9999999999999716, 88.84906250086716284 ) ) ;
#42611 = ORIENTED_EDGE ( 'NONE', *, *, #70672, .T. ) ;
#42612 = EDGE_CURVE ( 'NONE', #21124, #42089, #71973, .T. ) ;
#42613 = CARTESIAN_POINT ( 'NONE',  ( 92.34999999999999432, 88.47002178664752137, 86.95729166840096980 ) ) ;
#42614 = CARTESIAN_POINT ( 'NONE',  ( -23.54415474984308787, -120.4156646670583086, 5.500000000000000000 ) ) ;
#42615 = ORIENTED_EDGE ( 'NONE', *, *, #14495, .F. ) ;
#42616 = EDGE_CURVE ( 'NONE', #35859, #23719, #14838, .T. ) ;
#42617 = CARTESIAN_POINT ( 'NONE',  ( 11.99999999999999822, 8.830959090343430518, -74.65491531819107252 ) ) ;
#42618 = ORIENTED_EDGE ( 'NONE', *, *, #29617, .T. ) ;
#42619 = CARTESIAN_POINT ( 'NONE',  ( 0.000000000000000000, 0.000000000000000000, 0.000000000000000000 ) ) ;
#42620 = AXIS2_PLACEMENT_3D ( 'NONE', #54018, #71276, #60039 ) ;
#42621 = VERTEX_POINT ( 'NONE', #15584 ) ;
#42622 = ORIENTED_EDGE ( 'NONE', *, *, #4867, .F. ) ;
#42623 = EDGE_LOOP ( 'NONE', ( #11265, #33455, #50543, #11090 ) ) ;
#42624 = LINE ( 'NONE', #59178, #55124 ) ;
#42625 = EDGE_CURVE ( 'NONE', #55755, #33844, #38517, .T. ) ;
#42626 = EDGE_CURVE ( 'NONE', #71453, #57971, #31857, .T. ) ;
#42627 = ORIENTED_EDGE ( 'NONE', *, *, #11630, .T. ) ;
#42628 = VERTEX_POINT ( 'NONE', #68951 ) ;
#42629 = CARTESIAN_POINT ( 'NONE',  ( 92.69370383062498320, 88.66845928578037217, 80.96447916753382401 ) ) ;
#42630 = CIRCLE ( 'NONE', #26998, 16.00000000000000000 ) ;
#42631 = LINE ( 'NONE', #66312, #34764 ) ;
#42633 = CARTESIAN_POINT ( 'NONE',  ( 10.00000000000000000, 70.53064760720278059, 26.01480285779964774 ) ) ;
#42632 = AXIS2_PLACEMENT_3D ( 'NONE', #62452, #63191, #40613 ) ;
#42634 = EDGE_LOOP ( 'NONE', ( #56410, #3741, #16749, #38184 ) ) ;
#42635 = ORIENTED_EDGE ( 'NONE', *, *, #34990, .F. ) ;
#42636 = ORIENTED_EDGE ( 'NONE', *, *, #51348, .F. ) ;
#42637 = LINE ( 'NONE', #19689, #50278 ) ;
#42638 = ORIENTED_EDGE ( 'NONE', *, *, #66650, .F. ) ;
#42639 = CIRCLE ( 'NONE', #31837, 31.99999999999999289 ) ;
#42640 = CARTESIAN_POINT ( 'NONE',  ( -13.50000000000001954, -72.99999999999998579, -205.0000000000000284 ) ) ;
#42641 = FACE_OUTER_BOUND ( 'NONE', #37753, .T. ) ;
#42642 = CARTESIAN_POINT ( 'NONE',  ( -3.000000000000000000, 0.000000000000000000, 0.000000000000000000 ) ) ;
#42643 = DIRECTION ( 'NONE',  ( 0.000000000000000000, -1.065814103640131662E-14, -1.000000000000000000 ) ) ;
#42644 = CARTESIAN_POINT ( 'NONE',  ( 10.00000000000000000, 0.000000000000000000, 0.000000000000000000 ) ) ;
#42645 = VECTOR ( 'NONE', #37128, 1000.000000000000000 ) ;
#42646 = CARTESIAN_POINT ( 'NONE',  ( -3.000000000000000000, -10.45096189432314837, -21.10159698893440350 ) ) ;
#42647 = CARTESIAN_POINT ( 'NONE',  ( 10.00000000000000000, 75.54627589209943039, 17.28742895386112721 ) ) ;
#42648 = CARTESIAN_POINT ( 'NONE',  ( -92.34999999999999432, -211.0689600337108232, 74.48490336299448700 ) ) ;
#42649 = CARTESIAN_POINT ( 'NONE',  ( -97.30629616937501680, 88.66845928578038638, 87.94947916753382344 ) ) ;
#42651 = CARTESIAN_POINT ( 'NONE',  ( -95.00000000000002842, 93.05995642670501411, 74.68062500173429896 ) ) ;
#42650 = CARTESIAN_POINT ( 'NONE',  ( 92.34999999999999432, 90.00000000000002842, 77.37937500173428873 ) ) ;
#42652 =( BOUNDED_CURVE ( )  B_SPLINE_CURVE ( 2, ( #33567, #9537, #26451, #72664, #44115, #56139, #4657, #32454, #32818 ),
 .UNSPECIFIED., .F., .F. ) 
 B_SPLINE_CURVE_WITH_KNOTS ( ( 3, 2, 2, 2, 3 ),
 ( 0.8043570860654217780, 0.8043572716605901229, 0.8114130372014725090, 0.8184688027423548951, 0.8255245790564514907 ),
 .UNSPECIFIED. ) 
 CURVE ( )  GEOMETRIC_REPRESENTATION_ITEM ( )  RATIONAL_B_SPLINE_CURVE ( ( 0.9999929520380047565, 0.9999964759263050285, 1.000000000000000000, 0.8660254037844387076, 1.000000000000000000, 0.8660254037844387076, 1.000000000000000000, 0.8660254037844387076, 1.000000000000000000 ) ) 
 REPRESENTATION_ITEM ( '' )  );
#42653 = ORIENTED_EDGE ( 'NONE', *, *, #2540, .T. ) ;
#42654 = CARTESIAN_POINT ( 'NONE',  ( 92.69370383062498320, 88.66845928578037217, 75.88447916753382572 ) ) ;
#42655 = DIRECTION ( 'NONE',  ( -1.000000000000000000, -0.000000000000000000, -0.000000000000000000 ) ) ;
#42656 = CARTESIAN_POINT ( 'NONE',  ( 10.00000000000000000, 33.80338159004307386, -16.23288003029461279 ) ) ;
#42657 = DIRECTION ( 'NONE',  ( 1.000000000000000000, 0.000000000000000000, 0.000000000000000000 ) ) ;
#42658 = AXIS2_PLACEMENT_3D ( 'NONE', #25815, #71668, #55505 ) ;
#42659 = DIRECTION ( 'NONE',  ( -0.9781476007338069101, 0.2079116908177532363, 0.000000000000000000 ) ) ;
#42660 = CYLINDRICAL_SURFACE ( 'NONE', #10290, 12.49999999999999645 ) ;
#42661 = ORIENTED_EDGE ( 'NONE', *, *, #50167, .T. ) ;
#42662 = CARTESIAN_POINT ( 'NONE',  ( 6.000000000000000000, 29.01471420065673712, -76.69515212745984911 ) ) ;
#42663 = DIRECTION ( 'NONE',  ( -1.000000000000000000, 0.000000000000000000, -0.000000000000000000 ) ) ;
#42664 = ORIENTED_EDGE ( 'NONE', *, *, #72785, .F. ) ;
#42665 = ORIENTED_EDGE ( 'NONE', *, *, #72538, .F. ) ;
#42666 = CARTESIAN_POINT ( 'NONE',  ( 26.00000000000000355, 2.445500000000000007, 0.000000000000000000 ) ) ;
#42667 = DIRECTION ( 'NONE',  ( 0.000000000000000000, 0.000000000000000000, 1.000000000000000000 ) ) ;
#42668 = DIRECTION ( 'NONE',  ( -1.000000000000000000, 0.000000000000000000, 0.000000000000000000 ) ) ;
#42669 = CARTESIAN_POINT ( 'NONE',  ( -10.00000000000000000, 0.000000000000000000, 0.000000000000000000 ) ) ;
#42670 = CARTESIAN_POINT ( 'NONE',  ( -97.65000000000001990, 90.00000000000004263, 76.10937500173430692 ) ) ;
#42671 = DIRECTION ( 'NONE',  ( 0.000000000000000000, 0.000000000000000000, 1.000000000000000000 ) ) ;
#42672 = VERTEX_POINT ( 'NONE', #11418 ) ;
#42673 = EDGE_CURVE ( 'NONE', #48200, #11638, #53438, .T. ) ;
#42674 = DIRECTION ( 'NONE',  ( 1.000000000000000000, 0.000000000000000000, 0.000000000000000000 ) ) ;
#42675 = VECTOR ( 'NONE', #47543, 1000.000000000000000 ) ;
#42676 = CARTESIAN_POINT ( 'NONE',  ( 97.64999999999996305, 90.00000034979572661, 77.69687501385438111 ) ) ;
#42677 = CARTESIAN_POINT ( 'NONE',  ( 10.00000000000000000, -15.48615015657555816, -39.04073710021360455 ) ) ;
#42678 = DIRECTION ( 'NONE',  ( -0.2306669878475622604, -0.9730327541852497042, 0.000000000000000000 ) ) ;
#42679 = LINE ( 'NONE', #71977, #19714 ) ;
#42680 = PLANE ( 'NONE',  #53861 ) ;
#42681 = EDGE_CURVE ( 'NONE', #43075, #55006, #60705, .T. ) ;
#42682 = LINE ( 'NONE', #66725, #1404 ) ;
#42683 = FACE_OUTER_BOUND ( 'NONE', #16095, .T. ) ;
#42684 = EDGE_CURVE ( 'NONE', #52914, #4552, #33037, .T. ) ;
#42685 = DIRECTION ( 'NONE',  ( 0.000000000000000000, 0.9238795325112878487, -0.3826834323650874503 ) ) ;
#42686 = AXIS2_PLACEMENT_3D ( 'NONE', #52490, #50466, #50083 ) ;
#42687 = CIRCLE ( 'NONE', #4274, 15.99999999999999822 ) ;
#42688 = CARTESIAN_POINT ( 'NONE',  ( 92.69370383062498320, 90.00000000000002842, 84.72156250086715090 ) ) ;
#42689 = EDGE_CURVE ( 'NONE', #22980, #21912, #50903, .T. ) ;
#42690 = CARTESIAN_POINT ( 'NONE',  ( -92.69370383062498320, -208.6684592857803295, 86.36197916753383197 ) ) ;
#42691 = CARTESIAN_POINT ( 'NONE',  ( 0.000000000000000000, 63.97538442413498672, -51.29473840253155004 ) ) ;
#42692 = ORIENTED_EDGE ( 'NONE', *, *, #37442, .F. ) ;
#42693 = CARTESIAN_POINT ( 'NONE',  ( 0.000000000000000000, 41.81611651403868990, -3.925862922255709542 ) ) ;
#42694 = CARTESIAN_POINT ( 'NONE',  ( -94.99999999999997158, -206.9400435732949575, 80.95125000000000171 ) ) ;
#42695 = CYLINDRICAL_SURFACE ( 'NONE', #16131, 16.00000000000000000 ) ;
#42696 = CIRCLE ( 'NONE', #65556, 77.49899999999999523 ) ;
#42697 = AXIS2_PLACEMENT_3D ( 'NONE', #7358, #59986, #31008 ) ;
#42698 = CARTESIAN_POINT ( 'NONE',  ( 96.15314808468750130, -211.9973110713294489, 83.50447916753381605 ) ) ;
#42699 = VERTEX_POINT ( 'NONE', #58028 ) ;
#42700 = CARTESIAN_POINT ( 'NONE',  ( 11.99999999999999822, -34.44570377933549565, -69.42325613327476219 ) ) ;
#42701 = ORIENTED_EDGE ( 'NONE', *, *, #46282, .T. ) ;
#42702 = VECTOR ( 'NONE', #48211, 1000.000000000000000 ) ;
#42703 = EDGE_CURVE ( 'NONE', #4987, #27575, #22722, .T. ) ;
#42704 = VECTOR ( 'NONE', #68799, 1000.000000000000000 ) ;
#42705 = VERTEX_POINT ( 'NONE', #62964 ) ;
#42706 = CARTESIAN_POINT ( 'NONE',  ( 6.000000000000000000, -81.90746397400391743, 3.894527615417579636 ) ) ;
#42707 = VECTOR ( 'NONE', #20035, 1000.000000000000000 ) ;
#42708 = VERTEX_POINT ( 'NONE', #16326 ) ;
#42709 = DIRECTION ( 'NONE',  ( 0.000000000000000000, 0.000000000000000000, 1.000000000000000000 ) ) ;
#42710 = CARTESIAN_POINT ( 'NONE',  ( 93.84685191531251292, -211.9973110713294489, 79.74739583420048916 ) ) ;
#42711 = ADVANCED_FACE ( 'NONE', ( #46020 ), #17438, .T. ) ;
#42712 = CARTESIAN_POINT ( 'NONE',  ( -92.34999999999988063, -208.4700217866474929, 80.84541666666663673 ) ) ;
#42713 = EDGE_CURVE ( 'NONE', #18663, #34276, #5440, .T. ) ;
#42714 = CYLINDRICAL_SURFACE ( 'NONE', #16008, 42.00000000000000000 ) ;
#42715 = LINE ( 'NONE', #59266, #55654 ) ;
#42716 = DIRECTION ( 'NONE',  ( -1.000000000000000000, -0.000000000000000000, 0.000000000000000000 ) ) ;
#42717 = EDGE_CURVE ( 'NONE', #13516, #44140, #5437, .T. ) ;
#42718 = DIRECTION ( 'NONE',  ( 0.000000000000000000, 0.9510565162951544194, -0.3090169943749447867 ) ) ;
#42719 = CARTESIAN_POINT ( 'NONE',  ( 97.64999999999997726, -208.4700217866474645, 82.75041666666665208 ) ) ;
#42720 = VERTEX_POINT ( 'NONE', #5804 ) ;
#42721 = VERTEX_POINT ( 'NONE', #559 ) ;
#42722 = ORIENTED_EDGE ( 'NONE', *, *, #36829, .F. ) ;
#42723 = EDGE_LOOP ( 'NONE', ( #58799, #72028, #63090, #12402 ) ) ;
#42724 = LINE ( 'NONE', #30683, #29781 ) ;
#42725 = CARTESIAN_POINT ( 'NONE',  ( -96.15314808468752972, 91.99731107132950569, 83.98072916753382344 ) ) ;
#42727 = B_SPLINE_CURVE_WITH_KNOTS ( 'NONE', 1,
 ( #29409, #11395 ),
 .UNSPECIFIED., .F., .F.,
 ( 2, 2 ),
 ( 0.000000000000000000, 1.000000000000000000 ),
 .UNSPECIFIED. ) ;
#42726 = CARTESIAN_POINT ( 'NONE',  ( -97.65000000000001990, 90.00001272874953884, 81.82437456149077093 ) ) ;
#42728 = CYLINDRICAL_SURFACE ( 'NONE', #30581, 82.00000000000000000 ) ;
#42729 = CARTESIAN_POINT ( 'NONE',  ( 97.64999999999996305, 88.93104485797731229, 75.04052853044674976 ) ) ;
#42730 = CARTESIAN_POINT ( 'NONE',  ( -95.00000000000002842, 90.00000000000004263, 90.00000000000000000 ) ) ;
#42731 = VERTEX_POINT ( 'NONE', #51652 ) ;
#42732 = CARTESIAN_POINT ( 'NONE',  ( -94.99999999999997158, -213.0599564267049857, 86.42812500173430124 ) ) ;
#42733 = ORIENTED_EDGE ( 'NONE', *, *, #46456, .F. ) ;
#42734 = CARTESIAN_POINT ( 'NONE',  ( 12.49999999999999645, 1.530808498934191127E-15, 125.0000000000000000 ) ) ;
#42735 = EDGE_LOOP ( 'NONE', ( #18453, #29838, #43755, #65740 ) ) ;
#42736 = CARTESIAN_POINT ( 'NONE',  ( -95.00000000000002842, 93.05995642670501411, 86.74562500173429669 ) ) ;
#42737 = VERTEX_POINT ( 'NONE', #62582 ) ;
#42738 = CARTESIAN_POINT ( 'NONE',  ( 96.15314808468748708, 91.99731107132950569, 88.31989583420048007 ) ) ;
#42739 = CIRCLE ( 'NONE', #51154, 31.99999999999999289 ) ;
#42740 = DIRECTION ( 'NONE',  ( 0.000000000000000000, -0.9510565162951500895, -0.3090169943749583314 ) ) ;
#42741 = CARTESIAN_POINT ( 'NONE',  ( -93.33864827737279768, 88.39919842643631398, 74.79754476654878204 ) ) ;
#42742 = CARTESIAN_POINT ( 'NONE',  ( 93.67499999999999716, 87.70503267997126784, 88.83583333333334053 ) ) ;
#42743 = CARTESIAN_POINT ( 'NONE',  ( 6.000000000000000000, -15.33399622253541317, 80.55351364060584274 ) ) ;
#42744 = ORIENTED_EDGE ( 'NONE', *, *, #72032, .F. ) ;
#42745 = CARTESIAN_POINT ( 'NONE',  ( 10.00000000000000000, -26.08949754953044220, 27.05870788708222818 ) ) ;
#42746 = AXIS2_PLACEMENT_3D ( 'NONE', #49003, #55021, #2820 ) ;
#42747 = DIRECTION ( 'NONE',  ( -4.476705744456276711E-17, 1.000000000000000000, -0.000000000000000000 ) ) ;
#42748 = VERTEX_POINT ( 'NONE', #40746 ) ;
#42749 = CIRCLE ( 'NONE', #48751, 37.49900000000000944 ) ;
#42750 = ORIENTED_EDGE ( 'NONE', *, *, #56006, .T. ) ;
#42752 = FACE_BOUND ( 'NONE', #27338, .T. ) ;
#42751 = VECTOR ( 'NONE', #37601, 1000.000000000000000 ) ;
#42753 = PRODUCT_DEFINITION_SHAPE ( 'NONE', 'NONE',  #74349 ) ;
#42754 = DIRECTION ( 'NONE',  ( 0.000000000000000000, 0.000000000000000000, -1.000000000000000000 ) ) ;
#42755 = AXIS2_PLACEMENT_3D ( 'NONE', #4314, #50133, #10302 ) ;
#42756 = VECTOR ( 'NONE', #17698, 1000.000000000000000 ) ;
#42757 = CARTESIAN_POINT ( 'NONE',  ( 2.459674775249762302, 3.512261536898573354E-15, 1.958521724562357923E-15 ) ) ;
#42758 = CARTESIAN_POINT ( 'NONE',  ( -93.84685191531247028, -211.9973110713294489, 83.02822916753380866 ) ) ;
#42759 = ORIENTED_EDGE ( 'NONE', *, *, #17608, .T. ) ;
#42760 = FACE_OUTER_BOUND ( 'NONE', #19995, .T. ) ;
#42761 = ORIENTED_EDGE ( 'NONE', *, *, #53289, .T. ) ;
#42762 = EDGE_CURVE ( 'NONE', #25706, #55085, #36642, .T. ) ;
#42763 = ORIENTED_EDGE ( 'NONE', *, *, #39240, .T. ) ;
#42764 = DIRECTION ( 'NONE',  ( 1.000000000000000000, 0.000000000000000000, 0.000000000000000000 ) ) ;
#42765 = CARTESIAN_POINT ( 'NONE',  ( 92.69370383062498320, 91.33154071421968467, 88.47864583420047779 ) ) ;
#42766 = CIRCLE ( 'NONE', #60803, 31.99999999999998579 ) ;
#42767 = DIRECTION ( 'NONE',  ( -0.08130631524010117905, 0.9966891607226784355, 0.000000000000000000 ) ) ;
#42768 = CARTESIAN_POINT ( 'NONE',  ( 92.69370383062498320, 90.00000000000002842, 81.38781250086714181 ) ) ;
#42769 = CARTESIAN_POINT ( 'NONE',  ( 11.99999999999999822, 31.46837873495072913, -68.27212725128242710 ) ) ;
#42770 = CARTESIAN_POINT ( 'NONE',  ( 11.99999999999999822, 0.000000000000000000, 0.000000000000000000 ) ) ;
#42771 = EDGE_CURVE ( 'NONE', #7429, #23521, #55856, .T. ) ;
#42772 = DIRECTION ( 'NONE',  ( 0.000000000000000000, -0.9723699203976789995, 0.2334453638558957322 ) ) ;
#42773 = CARTESIAN_POINT ( 'NONE',  ( 96.40521225739021816, 91.86781405990345206, 74.80441578173235939 ) ) ;
#42774 = CARTESIAN_POINT ( 'NONE',  ( 10.00000000000000000, 0.000000000000000000, 0.000000000000000000 ) ) ;
#42775 = EDGE_CURVE ( 'NONE', #38604, #34215, #5068, .T. ) ;
#42776 = CARTESIAN_POINT ( 'NONE',  ( 10.00000000000000000, 0.000000000000000000, 0.000000000000000000 ) ) ;
#42777 = CARTESIAN_POINT ( 'NONE',  ( 10.00000000000000000, -71.27951684758005513, -30.41916302227188851 ) ) ;
#42778 = EDGE_CURVE ( 'NONE', #11835, #35754, #32169, .T. ) ;
#42779 = LINE ( 'NONE', #18357, #61383 ) ;
#42780 = ORIENTED_EDGE ( 'NONE', *, *, #41581, .T. ) ;
#42781 = CARTESIAN_POINT ( 'NONE',  ( -97.30629616937501680, 88.66845928578038638, 87.15572916753380639 ) ) ;
#42782 = DIRECTION ( 'NONE',  ( 0.5200609990132993854, 0.8541291221503275466, 0.000000000000000000 ) ) ;
#42783 = CLOSED_SHELL ( 'NONE', ( #64028, #32504, #45108, #29703, #19415, #25559 ) ) ;
#42784 = CARTESIAN_POINT ( 'NONE',  ( 0.000000000000000000, -63.97538442413390669, -51.29473840253292138 ) ) ;
#42785 = EDGE_LOOP ( 'NONE', ( #17172, #57454, #49407, #28958 ) ) ;
#42786 = CARTESIAN_POINT ( 'NONE',  ( 96.32499999999998863, -207.7050326799711968, 83.43833333333333258 ) ) ;
#42787 = CARTESIAN_POINT ( 'NONE',  ( 10.00000000000000000, -0.8828120875903202602, 37.48860685352291000 ) ) ;
#42788 = EDGE_CURVE ( 'NONE', #42186, #46015, #29436, .T. ) ;
#42789 = CIRCLE ( 'NONE', #55989, 82.00000000000000000 ) ;
#42790 = CYLINDRICAL_SURFACE ( 'NONE', #43138, 37.49900000000000233 ) ;
#42791 = CARTESIAN_POINT ( 'NONE',  ( 97.30629616937498838, -209.9999999999999716, 83.76906250086716454 ) ) ;
#42792 = AXIS2_PLACEMENT_3D ( 'NONE', #19974, #65495, #60232 ) ;
#42793 = VERTEX_POINT ( 'NONE', #52379 ) ;
#42794 = CIRCLE ( 'NONE', #55998, 77.49900000000000944 ) ;
#42795 = ORIENTED_EDGE ( 'NONE', *, *, #67215, .T. ) ;
#42796 = ADVANCED_FACE ( 'NONE', ( #928 ), #39265, .F. ) ;
#42797 = LINE ( 'NONE', #26604, #40394 ) ;
#42798 = VERTEX_POINT ( 'NONE', #68204 ) ;
#42799 = EDGE_CURVE ( 'NONE', #18231, #26331, #16700, .T. ) ;
#42800 = CIRCLE ( 'NONE', #10390, 31.99999999999998224 ) ;
#42801 = CARTESIAN_POINT ( 'NONE',  ( 10.00000000000000000, 31.52238457039638320, -27.75498641678709788 ) ) ;
#42802 = AXIS2_PLACEMENT_3D ( 'NONE', #3386, #49221, #15008 ) ;
#42803 = DIRECTION ( 'NONE',  ( 0.000000000000000000, -1.000000000000000000, -1.040834085586084730E-14 ) ) ;
#42804 = ORIENTED_EDGE ( 'NONE', *, *, #662, .F. ) ;
#42805 = DIRECTION ( 'NONE',  ( 0.000000000000000000, 0.000000000000000000, 1.000000000000000000 ) ) ;
#42806 = CARTESIAN_POINT ( 'NONE',  ( 97.30629616937498838, -208.6684592857803011, 74.93197916753381094 ) ) ;
#42807 = ORIENTED_EDGE ( 'NONE', *, *, #55692, .T. ) ;
#42808 = CARTESIAN_POINT ( 'NONE',  ( 97.65000000000000568, 88.47002178664752137, 79.46958333333331836 ) ) ;
#42809 = ORIENTED_EDGE ( 'NONE', *, *, #31878, .T. ) ;
#42810 = VERTEX_POINT ( 'NONE', #70033 ) ;
#42811 = DIRECTION ( 'NONE',  ( 0.3311129884571281101, 0.9435911131814402886, -0.000000000000000000 ) ) ;
#42812 = CIRCLE ( 'NONE', #2020, 15.99999999999999822 ) ;
#42813 = PRESENTATION_STYLE_ASSIGNMENT (( #25880 ) ) ;
#42814 = CARTESIAN_POINT ( 'NONE',  ( -95.00000000000002842, 93.05995642670504253, 89.28562500173430294 ) ) ;
#42815 = ORIENTED_EDGE ( 'NONE', *, *, #19451, .F. ) ;
#42816 = CARTESIAN_POINT ( 'NONE',  ( 0.000000000000000000, 11.30684508768450591, -76.66974797899824523 ) ) ;
#42817 = CARTESIAN_POINT ( 'NONE',  ( 92.35000000000002274, -208.4700217866474645, 84.94645833506763211 ) ) ;
#42818 = CARTESIAN_POINT ( 'NONE',  ( 96.32499999999997442, 92.29496732002878900, 85.34333333333333371 ) ) ;
#42819 = EDGE_LOOP ( 'NONE', ( #46004, #12461, #40913, #6112 ) ) ;
#42820 = CARTESIAN_POINT ( 'NONE',  ( 10.00000000000000000, 0.000000000000000000, 0.000000000000000000 ) ) ;
#42821 = CARTESIAN_POINT ( 'NONE',  ( 93.67499999999998295, 92.29496732002878900, 81.08354166840096866 ) ) ;
#42822 = ORIENTED_EDGE ( 'NONE', *, *, #2596, .F. ) ;
#42823 = ORIENTED_EDGE ( 'NONE', *, *, #34732, .F. ) ;
#42824 = CARTESIAN_POINT ( 'NONE',  ( -92.69370383062504004, 90.00000000000004263, 86.30906250086715659 ) ) ;
#42825 = CARTESIAN_POINT ( 'NONE',  ( 94.99999999999998579, 92.66308142843935514, 81.22906250086715829 ) ) ;
#42826 = ORIENTED_EDGE ( 'NONE', *, *, #1316, .T. ) ;
#42827 = CARTESIAN_POINT ( 'NONE',  ( 92.34999999999999432, 88.47002178664753558, 83.78229166840095843 ) ) ;
#42828 = CARTESIAN_POINT ( 'NONE',  ( 10.00000000000000000, 69.42325613327439271, 34.44570377933623462 ) ) ;
#42829 = VERTEX_POINT ( 'NONE', #7272 ) ;
#42830 = CARTESIAN_POINT ( 'NONE',  ( -92.34999999999990905, -211.5299782133523934, 86.45458333333331780 ) ) ;
#42831 = ORIENTED_EDGE ( 'NONE', *, *, #26884, .T. ) ;
#42832 = VECTOR ( 'NONE', #50051, 1000.000000000000114 ) ;
#42833 = ORIENTED_EDGE ( 'NONE', *, *, #68193, .F. ) ;
#42834 = VERTEX_POINT ( 'NONE', #41475 ) ;
#42835 = LINE ( 'NONE', #2656, #24095 ) ;
#42836 = CARTESIAN_POINT ( 'NONE',  ( 92.35000000005783249, 89.99998877583867340, 75.47473230081648410 ) ) ;
#42837 = CARTESIAN_POINT ( 'NONE',  ( -95.00000000000002842, 86.94004357329504273, 83.17374999999999829 ) ) ;
#42838 = ORIENTED_EDGE ( 'NONE', *, *, #4625, .T. ) ;
#42839 = DIRECTION ( 'NONE',  ( -1.000000000000000000, 0.000000000000000000, 0.000000000000000000 ) ) ;
#42840 = EDGE_CURVE ( 'NONE', #44003, #13441, #58775, .T. ) ;
#42841 = CARTESIAN_POINT ( 'NONE',  ( 92.34999999999999432, 90.00000000000002842, 89.44437500173430067 ) ) ;
#42842 = ORIENTED_EDGE ( 'NONE', *, *, #39464, .F. ) ;
#42843 = CARTESIAN_POINT ( 'NONE',  ( 92.35000000000000853, -209.9999999999999716, 84.92000000000000171 ) ) ;
#42844 = CARTESIAN_POINT ( 'NONE',  ( -97.30629616937495996, -209.9999999999999716, 78.84781250086714977 ) ) ;
#42845 = ORIENTED_EDGE ( 'NONE', *, *, #30570, .F. ) ;
#42846 = CARTESIAN_POINT ( 'NONE',  ( 2.500000000000029754, 73.00000000000001421, -255.0000000000000000 ) ) ;
#42847 = CIRCLE ( 'NONE', #3258, 31.99999999999998579 ) ;
#42848 = DIRECTION ( 'NONE',  ( 0.000000000000000000, 0.4539904997395413644, 0.8910065241883706744 ) ) ;
#42849 = CARTESIAN_POINT ( 'NONE',  ( -34.02017708624680381, -130.1428571428571388, 2.500000000000000000 ) ) ;
#42850 = CARTESIAN_POINT ( 'NONE',  ( 11.41210121379328335, -99.40233154247455616, 5.500000000000000000 ) ) ;
#42851 = ADVANCED_FACE ( 'NONE', ( #53129 ), #1305, .T. ) ;
#42852 = AXIS2_PLACEMENT_3D ( 'NONE', #17381, #18127, #23401 ) ;
#42853 = DIRECTION ( 'NONE',  ( 0.000000000000000000, 0.2079116908177664480, -0.9781476007338041345 ) ) ;
#42854 = EDGE_CURVE ( 'NONE', #20620, #28223, #7632, .T. ) ;
#42855 = AXIS2_PLACEMENT_3D ( 'NONE', #59489, #7980, #2388 ) ;
#42856 = FACE_OUTER_BOUND ( 'NONE', #4835, .T. ) ;
#42857 = DIRECTION ( 'NONE',  ( -1.000000000000000000, 0.000000000000000000, 0.000000000000000000 ) ) ;
#42858 = VECTOR ( 'NONE', #23874, 1000.000000000000000 ) ;
#42859 = CARTESIAN_POINT ( 'NONE',  ( 10.00000000000000000, 0.000000000000000000, 0.000000000000000000 ) ) ;
#42860 = EDGE_CURVE ( 'NONE', #65939, #4011, #38195, .T. ) ;
#42861 = CARTESIAN_POINT ( 'NONE',  ( 11.99999999999999822, 62.50884508063487033, -41.76106447765422303 ) ) ;
#42862 = CARTESIAN_POINT ( 'NONE',  ( 10.00000000000000000, -75.54627589209955829, 17.28742895386058009 ) ) ;
#42863 = CARTESIAN_POINT ( 'NONE',  ( -92.69370383062502583, 88.66845928578038638, 75.30239583420048177 ) ) ;
#42864 = DIRECTION ( 'NONE',  ( 0.000000000000000000, 0.000000000000000000, 1.000000000000000000 ) ) ;
#42865 = DIRECTION ( 'NONE',  ( -1.000000000000000000, -0.000000000000000000, 0.000000000000000000 ) ) ;
#42866 = VECTOR ( 'NONE', #9756, 1000.000000000000114 ) ;
#42867 =( BOUNDED_CURVE ( )  B_SPLINE_CURVE ( 2, ( #2895, #20886, #32532, #66757, #15246 ),
 .UNSPECIFIED., .F., .F. ) 
 B_SPLINE_CURVE_WITH_KNOTS ( ( 3, 2, 3 ),
 ( 0.9525283480321510288, 0.9595841135600021721, 0.9629953541049922627 ),
 .UNSPECIFIED. ) 
 CURVE ( )  GEOMETRIC_REPRESENTATION_ITEM ( )  RATIONAL_B_SPLINE_CURVE ( ( 1.000000000000000000, 0.8660254037844387076, 1.000000000000000000, 0.9352274998423413255, 0.9330859296547716619 ) ) 
 REPRESENTATION_ITEM ( '' )  );
#42868 = CARTESIAN_POINT ( 'NONE',  ( 10.00000000000000000, 68.26794271651262136, 31.47745569255165066 ) ) ;
#42869 = UNCERTAINTY_MEASURE_WITH_UNIT (LENGTH_MEASURE( 1.000000000000000082E-05 ), #15634, 'distance_accuracy_value', 'NONE');
#42870 = LINE ( 'NONE', #15392, #22037 ) ;
#42871 = CIRCLE ( 'NONE', #52460, 26.50000000000000355 ) ;
#42872 = EDGE_CURVE ( 'NONE', #34012, #61374, #30552, .T. ) ;
#42873 = UNCERTAINTY_MEASURE_WITH_UNIT (LENGTH_MEASURE( 1.000000000000000082E-05 ), #64632, 'distance_accuracy_value', 'NONE');
#42874 = DIRECTION ( 'NONE',  ( -1.000000000000000000, 0.000000000000000000, 0.000000000000000000 ) ) ;
#42875 = CARTESIAN_POINT ( 'NONE',  ( 10.00000000000000000, 0.000000000000000000, 0.000000000000000000 ) ) ;
#42876 = CARTESIAN_POINT ( 'NONE',  ( 10.00000000000000000, -64.81221759200380461, 50.23322058963325532 ) ) ;
#42877 = CARTESIAN_POINT ( 'NONE',  ( 0.000000000000000000, 31.47745569255237896, -68.26794271651228030 ) ) ;
#42878 = VECTOR ( 'NONE', #51029, 1000.000000000000000 ) ;
#42879 = DIRECTION ( 'NONE',  ( -1.000000000000000000, 0.000000000000000000, -0.000000000000000000 ) ) ;
#42880 = CARTESIAN_POINT ( 'NONE',  ( -92.34999999999999432, -208.4700217866474645, 87.19541666666667368 ) ) ;
#42881 = CIRCLE ( 'NONE', #40461, 37.49900000000000944 ) ;
#42882 = CARTESIAN_POINT ( 'NONE',  ( 5.000000000000002665, -2.886751345948134873, -5.553418012614792509 ) ) ;
#42883 = EDGE_CURVE ( 'NONE', #26087, #503, #59890, .T. ) ;
#42884 = ORIENTED_EDGE ( 'NONE', *, *, #13310, .T. ) ;
#42885 = CYLINDRICAL_SURFACE ( 'NONE', #67184, 82.00000000000000000 ) ;
#42886 = EDGE_CURVE ( 'NONE', #1170, #1681, #68213, .T. ) ;
#42887 = CYLINDRICAL_SURFACE ( 'NONE', #64697, 31.99999999999999289 ) ;
#42888 = DIRECTION ( 'NONE',  ( 0.000000000000000000, 1.078060571631605650E-14, 1.000000000000000000 ) ) ;
#42889 = PLANE ( 'NONE',  #40174 ) ;
#42890 = EDGE_CURVE ( 'NONE', #63489, #17145, #35767, .T. ) ;
#42891 = ORIENTED_EDGE ( 'NONE', *, *, #45061, .T. ) ;
#42892 = DIRECTION ( 'NONE',  ( 0.000000000000000000, -0.5877852522924802425, 0.8090169943749422332 ) ) ;
#42893 = ADVANCED_FACE ( 'NONE', ( #58394 ), #36966, .F. ) ;
#42894 = CARTESIAN_POINT ( 'NONE',  ( 10.00000000000000000, 0.000000000000000000, 0.000000000000000000 ) ) ;
#42895 = ORIENTED_EDGE ( 'NONE', *, *, #71635, .F. ) ;
#42896 = CARTESIAN_POINT ( 'NONE',  ( 93.84685191531251292, -211.9973110713294489, 81.49364583420047836 ) ) ;
#42897 = CARTESIAN_POINT ( 'NONE',  ( 92.69370383062501162, -211.3315407142195852, 89.21947916753381946 ) ) ;
#42898 = VECTOR ( 'NONE', #64222, 1000.000000000000000 ) ;
#42899 = ORIENTED_EDGE ( 'NONE', *, *, #21651, .F. ) ;
#42900 = CARTESIAN_POINT ( 'NONE',  ( 95.00000000000000000, -212.6630814284392557, 87.42031250086715488 ) ) ;
#42901 = CIRCLE ( 'NONE', #65713, 31.99999999999999289 ) ;
#42902 = EDGE_CURVE ( 'NONE', #3846, #45970, #1006, .T. ) ;
#42903 = ORIENTED_EDGE ( 'NONE', *, *, #2865, .F. ) ;
#42904 = DIRECTION ( 'NONE',  ( 0.000000000000000000, 0.000000000000000000, 1.000000000000000000 ) ) ;
#42905 = ORIENTED_EDGE ( 'NONE', *, *, #65373, .T. ) ;
#42906 = CARTESIAN_POINT ( 'NONE',  ( -92.69370383062502583, 88.66845928578038638, 77.36614583420048064 ) ) ;
#42907 = ORIENTED_EDGE ( 'NONE', *, *, #21034, .T. ) ;
#42908 = ORIENTED_EDGE ( 'NONE', *, *, #71898, .F. ) ;
#42909 = CARTESIAN_POINT ( 'NONE',  ( 10.00000000000000000, 0.000000000000000000, 0.000000000000000000 ) ) ;
#42910 = AXIS2_PLACEMENT_3D ( 'NONE', #28714, #33987, #51654 ) ;
#42911 = VERTEX_POINT ( 'NONE', #71138 ) ;
#42912 = DIRECTION ( 'NONE',  ( -1.000000000000000000, 0.000000000000000000, -0.000000000000000000 ) ) ;
#42913 = DIRECTION ( 'NONE',  ( 0.000000000000000000, -1.000000000000000000, 0.000000000000000000 ) ) ;
#42914 = ORIENTED_EDGE ( 'NONE', *, *, #32179, .T. ) ;
#42915 = CARTESIAN_POINT ( 'NONE',  ( 11.99999999999999822, -68.27212725128298132, 31.46837873494953541 ) ) ;
#42916 = ORIENTED_EDGE ( 'NONE', *, *, #25125, .F. ) ;
#42917 = CARTESIAN_POINT ( 'NONE',  ( 6.250000000000005329, 0.000000000000000000, 3.000000000000000888 ) ) ;
#42918 = VERTEX_POINT ( 'NONE', #2034 ) ;
#42919 = ORIENTED_EDGE ( 'NONE', *, *, #28004, .F. ) ;
#42920 = VERTEX_POINT ( 'NONE', #36942 ) ;
#42921 = CARTESIAN_POINT ( 'NONE',  ( 97.30629616937498838, -211.3315407142195852, 77.20739583420046870 ) ) ;
#42922 = DIRECTION ( 'NONE',  ( 0.3853207896976533209, -0.9227826878668545785, 0.000000000000000000 ) ) ;
#42923 = CARTESIAN_POINT ( 'NONE',  ( -93.67500000000003979, 87.70503267997129626, 81.95666666666666345 ) ) ;
#42924 = ORIENTED_EDGE ( 'NONE', *, *, #69620, .F. ) ;
#42925 = VECTOR ( 'NONE', #61492, 1000.000000000000114 ) ;
#42926 = FACE_OUTER_BOUND ( 'NONE', #66746, .T. ) ;
#42927 = ORIENTED_EDGE ( 'NONE', *, *, #58817, .F. ) ;
#42928 = DIRECTION ( 'NONE',  ( 0.000000000000000000, 0.000000000000000000, 1.000000000000000000 ) ) ;
#42929 = CARTESIAN_POINT ( 'NONE',  ( 15.00000000000000000, 8.688484142253932063, -21.88630264137371029 ) ) ;
#42930 = ORIENTED_EDGE ( 'NONE', *, *, #485, .F. ) ;
#42931 = CARTESIAN_POINT ( 'NONE',  ( -93.67499999999998295, -207.7050326799711968, 88.59770833506763665 ) ) ;
#42932 = CARTESIAN_POINT ( 'NONE',  ( 0.000000000000000000, 21.32104025579114648, 30.84782396557224970 ) ) ;
#42933 = CARTESIAN_POINT ( 'NONE',  ( -97.30629616937497417, -211.3315407142195852, 80.80572916753382628 ) ) ;
#42934 = AXIS2_PLACEMENT_3D ( 'NONE', #58623, #7861, #19506 ) ;
#42935 = CARTESIAN_POINT ( 'NONE',  ( -93.84685191531254134, 91.99731107132950569, 77.52489583420047836 ) ) ;
#42936 = ORIENTED_EDGE ( 'NONE', *, *, #13987, .F. ) ;
#42937 = CARTESIAN_POINT ( 'NONE',  ( 96.15314808468748708, 88.00268892867053694, 80.96447916753380980 ) ) ;
#42938 = ORIENTED_EDGE ( 'NONE', *, *, #33714, .T. ) ;
#42939 = DIRECTION ( 'NONE',  ( 0.000000000000000000, 0.000000000000000000, -1.000000000000000000 ) ) ;
#42940 = DIRECTION ( 'NONE',  ( 0.9966891607226785466, 0.08130631524009969413, 0.000000000000000000 ) ) ;
#42941 = DIRECTION ( 'NONE',  ( 0.000000000000000000, 0.3090169943749482839, -0.9510565162951533091 ) ) ;
#42942 = LINE ( 'NONE', #59125, #9129 ) ;
#42943 = CARTESIAN_POINT ( 'NONE',  ( 0.000000000000000000, 10.74501242461333028, -35.92658777277499382 ) ) ;
#42944 = CARTESIAN_POINT ( 'NONE',  ( -97.30629616937497417, -208.6684592857803295, 81.33489583420048064 ) ) ;
#42945 = EDGE_CURVE ( 'NONE', #17492, #59102, #24942, .T. ) ;
#42946 = DIRECTION ( 'NONE',  ( 0.000000000000000000, 0.000000000000000000, 1.000000000000000000 ) ) ;
#42947 = LINE ( 'NONE', #54230, #13858 ) ;
#42948 = DIRECTION ( 'NONE',  ( -1.000000000000000000, -0.000000000000000000, 0.000000000000000000 ) ) ;
#42949 = ORIENTED_EDGE ( 'NONE', *, *, #32765, .F. ) ;
#42950 = EDGE_CURVE ( 'NONE', #44755, #25438, #70588, .T. ) ;
#42951 = ORIENTED_EDGE ( 'NONE', *, *, #70342, .T. ) ;
#42952 = CARTESIAN_POINT ( 'NONE',  ( 10.00000000000000000, -30.80686688396994910, -21.53537804866113703 ) ) ;
#42953 = EDGE_CURVE ( 'NONE', #63042, #14951, #70775, .T. ) ;
#42954 = EDGE_CURVE ( 'NONE', #55121, #41779, #53762, .T. ) ;
#42955 = CARTESIAN_POINT ( 'NONE',  ( -92.35000000000003695, 90.00000000000004263, 75.71250000000000568 ) ) ;
#42956 = DIRECTION ( 'NONE',  ( 0.000000000000000000, -0.6494480483301739993, -0.7604059656000390355 ) ) ;
#42957 = CARTESIAN_POINT ( 'NONE',  ( -97.30629616937501680, 90.00000000000004263, 85.19781250086714408 ) ) ;
#42958 = CARTESIAN_POINT ( 'NONE',  ( -97.45337789172090481, -209.5154774236565061, 74.90854212414869551 ) ) ;
#42959 = DIRECTION ( 'NONE',  ( -1.000000000000000000, -0.000000000000000000, 0.000000000000000000 ) ) ;
#42960 = DIRECTION ( 'NONE',  ( -1.000000000000000000, -0.000000000000000000, -0.000000000000000000 ) ) ;
#42961 = AXIS2_PLACEMENT_3D ( 'NONE', #71357, #26616, #66487 ) ;
#42962 = ORIENTED_EDGE ( 'NONE', *, *, #73074, .T. ) ;
#42963 = DIRECTION ( 'NONE',  ( 0.000000000000000000, 0.000000000000000000, 1.000000000000000000 ) ) ;
#42964 = COLOUR_RGB ( '', 0.40784314, 0.44705882, 0.49803922) ;
#42965 = LINE ( 'NONE', #61365, #18976 ) ;
#42966 = CARTESIAN_POINT ( 'NONE',  ( -97.64996285368390261, 91.52999965978816022, 82.40645685155122635 ) ) ;
#42967 = AXIS2_PLACEMENT_3D ( 'NONE', #27777, #1745, #16127 ) ;
#42968 = DIRECTION ( 'NONE',  ( -0.000000000000000000, -0.000000000000000000, 1.000000000000000000 ) ) ;
#42969 = DIRECTION ( 'NONE',  ( 1.000000000000000000, 0.000000000000000000, 0.000000000000000000 ) ) ;
#42970 = CYLINDRICAL_SURFACE ( 'NONE', #47205, 82.00000000000000000 ) ;
#42971 = CARTESIAN_POINT ( 'NONE',  ( -97.30629616937497417, -211.3315407142195852, 83.50447916753383026 ) ) ;
#42972 = AXIS2_PLACEMENT_3D ( 'NONE', #72257, #54970, #37330 ) ;
#42973 = EDGE_CURVE ( 'NONE', #29448, #4640, #74212, .T. ) ;
#42974 = CARTESIAN_POINT ( 'NONE',  ( 0.000000000000000000, 75.54627589209943039, 17.28742895386112721 ) ) ;
#42975 = CARTESIAN_POINT ( 'NONE',  ( 97.30629616937498838, 90.00000000000002842, 74.87906250086714977 ) ) ;
#42976 = DIRECTION ( 'NONE',  ( -1.000000000000000000, -0.000000000000000000, -0.000000000000000000 ) ) ;
#42977 = DIRECTION ( 'NONE',  ( -0.8774505977381983346, -0.4796670183876294291, 0.000000000000000000 ) ) ;
#42978 = ORIENTED_EDGE ( 'NONE', *, *, #8601, .F. ) ;
#42979 = LINE ( 'NONE', #14393, #59377 ) ;
#42980 = FACE_OUTER_BOUND ( 'NONE', #38733, .T. ) ;
#42981 = DIRECTION ( 'NONE',  ( -7.962523111838990267E-16, -1.065814103640131188E-14, -1.000000000000000000 ) ) ;
#42982 = EDGE_CURVE ( 'NONE', #47885, #27527, #46574, .T. ) ;
#42983 = EDGE_CURVE ( 'NONE', #59758, #45592, #12966, .T. ) ;
#42984 = AXIS2_PLACEMENT_3D ( 'NONE', #38930, #56603, #50945 ) ;
#42985 = AXIS2_PLACEMENT_3D ( 'NONE', #34102, #57046, #5555 ) ;
#42987 = AXIS2_PLACEMENT_3D ( 'NONE', #23560, #52127, #52489 ) ;
#42986 = CARTESIAN_POINT ( 'NONE',  ( 10.00000000000000000, -35.92658777277502935, -10.74501242461320594 ) ) ;
#42988 = CARTESIAN_POINT ( 'NONE',  ( 93.84685191531249870, -208.0026889286704943, 88.42572916753381662 ) ) ;
#42989 = ORIENTED_EDGE ( 'NONE', *, *, #36575, .F. ) ;
#42990 = AXIS2_PLACEMENT_3D ( 'NONE', #64415, #12891, #42588 ) ;
#42991 = CARTESIAN_POINT ( 'NONE',  ( 15.00000000000000000, -22.67460108101782978, -6.353146135317906840 ) ) ;
#42992 = ORIENTED_EDGE ( 'NONE', *, *, #65401, .F. ) ;
#42993 = DIRECTION ( 'NONE',  ( 0.000000000000000000, 0.000000000000000000, 1.000000000000000000 ) ) ;
#42994 = EDGE_LOOP ( 'NONE', ( #39117, #7307, #2940, #70727 ) ) ;
#42995 = CARTESIAN_POINT ( 'NONE',  ( 10.00000000000000000, -12.26510123303284594, 35.53030884539080603 ) ) ;
#42996 = ORIENTED_EDGE ( 'NONE', *, *, #59021, .T. ) ;
#42997 = ORIENTED_EDGE ( 'NONE', *, *, #47393, .F. ) ;
#42998 = ORIENTED_EDGE ( 'NONE', *, *, #18076, .T. ) ;
#42999 = VERTEX_POINT ( 'NONE', #29809 ) ;
#43000 = LINE ( 'NONE', #66305, #59920 ) ;
#43001 = ORIENTED_EDGE ( 'NONE', *, *, #61234, .F. ) ;
#43002 = ORIENTED_EDGE ( 'NONE', *, *, #59816, .F. ) ;
#43003 = CARTESIAN_POINT ( 'NONE',  ( 96.15314808468748708, 88.00268892867053694, 81.12322916753382174 ) ) ;
#43004 = CARTESIAN_POINT ( 'NONE',  ( 22.75000000000000000, 0.000000000000000000, 0.000000000000000000 ) ) ;
#43005 = COLOUR_RGB ( '', 0.08235294, 0.09019608, 0.10196078) ;
#43006 = CARTESIAN_POINT ( 'NONE',  ( -12.50000000000000000, -107.5000000000000000, -2.500000000000000000 ) ) ;
#43007 = VECTOR ( 'NONE', #18622, 1000.000000000000000 ) ;
#43008 = ORIENTED_EDGE ( 'NONE', *, *, #68143, .F. ) ;
#43009 = AXIS2_PLACEMENT_3D ( 'NONE', #4051, #3685, #25843 ) ;
#43010 = ORIENTED_EDGE ( 'NONE', *, *, #25612, .T. ) ;
#43011 = ORIENTED_EDGE ( 'NONE', *, *, #65355, .T. ) ;
#43012 = DIRECTION ( 'NONE',  ( 0.000000000000000000, 0.000000000000000000, -1.000000000000000000 ) ) ;
#43013 = VERTEX_POINT ( 'NONE', #52763 ) ;
#43014 = DIRECTION ( 'NONE',  ( -2.055370009866793940E-16, -2.543136972160332564E-16, 0.9999999999999998890 ) ) ;
#43015 = DIRECTION ( 'NONE',  ( 0.000000000000000000, -0.5000000000000028866, -0.8660254037844369313 ) ) ;
#43016 = AXIS2_PLACEMENT_3D ( 'NONE', #17787, #24187, #11764 ) ;
#43017 = CARTESIAN_POINT ( 'NONE',  ( 12.00000000000000000, -14.54903810567644484, 22.19967320028775504 ) ) ;
#43018 = CARTESIAN_POINT ( 'NONE',  ( 10.00000000000000000, -36.88895765772637247, 6.736453364083436313 ) ) ;
#43019 = AXIS2_PLACEMENT_3D ( 'NONE', #6272, #56668, #62302 ) ;
#43020 = CARTESIAN_POINT ( 'NONE',  ( 97.64999999999999147, 90.00000000000002842, 90.00000000000000000 ) ) ;
#43021 = DIRECTION ( 'NONE',  ( -1.000000000000000000, -0.000000000000000000, 0.000000000000000000 ) ) ;
#43022 = LINE ( 'NONE', #65961, #58835 ) ;
#43023 = CARTESIAN_POINT ( 'NONE',  ( -97.30629616937495996, -209.9999999999999716, 89.64281250086713726 ) ) ;
#43024 = CARTESIAN_POINT ( 'NONE',  ( -93.84685191531254134, 91.99731107132950569, 89.58989583420049030 ) ) ;
#43025 = ORIENTED_EDGE ( 'NONE', *, *, #30312, .T. ) ;
#43027 = CARTESIAN_POINT ( 'NONE',  ( -93.84685191531252713, 88.00268892867056536, 89.21947916753380525 ) ) ;
#43026 = CARTESIAN_POINT ( 'NONE',  ( 94.99999999999998579, 86.94004357329500010, 77.53812500173428646 ) ) ;
#43028 = VERTEX_POINT ( 'NONE', #47129 ) ;
#43029 = CARTESIAN_POINT ( 'NONE',  ( 96.15314808468748708, 91.99731107132950569, 76.25489583420049655 ) ) ;
#43030 = CYLINDRICAL_SURFACE ( 'NONE', #50555, 77.49899999999999523 ) ;
#43031 = CYLINDRICAL_SURFACE ( 'NONE', #59487, 2.649999999999985700 ) ;
#43032 = DIRECTION ( 'NONE',  ( 0.000000000000000000, 0.000000000000000000, 1.000000000000000000 ) ) ;
#43033 = CARTESIAN_POINT ( 'NONE',  ( -97.64999999989197477, 90.00001510551047090, 78.64888723592453346 ) ) ;
#43034 = CARTESIAN_POINT ( 'NONE',  ( 0.000000000000000000, 46.54456581323805153, 59.03342792756280488 ) ) ;
#43035 = VECTOR ( 'NONE', #33614, 1000.000000000000000 ) ;
#43036 = ORIENTED_EDGE ( 'NONE', *, *, #19005, .T. ) ;
#43037 = EDGE_CURVE ( 'NONE', #18122, #11167, #9377, .T. ) ;
#43038 = CARTESIAN_POINT ( 'NONE',  ( -93.67499999999998295, -212.2949673200287179, 80.05166666666666231 ) ) ;
#43039 = CARTESIAN_POINT ( 'NONE',  ( 0.000000000000000000, 0.000000000000000000, 20.00000000000000000 ) ) ;
#43040 = ORIENTED_EDGE ( 'NONE', *, *, #73686, .F. ) ;
#43041 = VECTOR ( 'NONE', #47078, 1000.000000000000000 ) ;
#43042 = ADVANCED_FACE ( 'NONE', ( #48597 ), #66632, .T. ) ;
#43043 = ORIENTED_EDGE ( 'NONE', *, *, #838, .T. ) ;
#43044 = VECTOR ( 'NONE', #31447, 1000.000000000000000 ) ;
#43045 = AXIS2_PLACEMENT_3D ( 'NONE', #60657, #2801, #60295 ) ;
#43046 = CIRCLE ( 'NONE', #10605, 82.00000000000000000 ) ;
#43047 = EDGE_CURVE ( 'NONE', #47629, #64038, #43350, .T. ) ;
#43048 = DIRECTION ( 'NONE',  ( -1.000000000000000000, -0.000000000000000000, -0.000000000000000000 ) ) ;
#43049 = DIRECTION ( 'NONE',  ( -1.000000000000000000, 0.000000000000000000, 0.000000000000000000 ) ) ;
#43050 = LINE ( 'NONE', #20839, #12301 ) ;
#43051 = LINE ( 'NONE', #25000, #72307 ) ;
#43052 = CARTESIAN_POINT ( 'NONE',  ( 11.99999999999999822, 68.26794271651307611, -31.47745569255064169 ) ) ;
#43053 = CARTESIAN_POINT ( 'NONE',  ( -97.30629616937497417, -211.3315407142195852, 75.24947916753383481 ) ) ;
#43054 = AXIS2_PLACEMENT_3D ( 'NONE', #58690, #30103, #7190 ) ;
#43055 = EDGE_CURVE ( 'NONE', #34723, #56976, #43708, .T. ) ;
#43056 = ORIENTED_EDGE ( 'NONE', *, *, #32317, .F. ) ;
#43057 = CYLINDRICAL_SURFACE ( 'NONE', #10275, 42.00000000000000000 ) ;
#43058 = LINE ( 'NONE', #65614, #40244 ) ;
#43059 = CARTESIAN_POINT ( 'NONE',  ( 10.00000000000000000, 49.70050353004977239, -59.46389618801908483 ) ) ;
#43060 = CYLINDRICAL_SURFACE ( 'NONE', #34528, 77.49899999999999523 ) ;
#43061 = DIRECTION ( 'NONE',  ( 0.000000000000000000, 0.000000000000000000, 1.000000000000000000 ) ) ;
#43062 = DIRECTION ( 'NONE',  ( 0.000000000000000000, -0.000000000000000000, 1.000000000000000000 ) ) ;
#43063 = UNCERTAINTY_MEASURE_WITH_UNIT (LENGTH_MEASURE( 1.000000000000000082E-05 ), #64548, 'distance_accuracy_value', 'NONE');
#43064 = DIRECTION ( 'NONE',  ( 0.000000000000000000, -0.8090169943749532244, 0.5877852522924652545 ) ) ;
#43065 = DIRECTION ( 'NONE',  ( -1.000000000000000000, -0.000000000000000000, -0.000000000000000000 ) ) ;
#43066 = EDGE_CURVE ( 'NONE', #9907, #55876, #54967, .T. ) ;
#43067 = DIRECTION ( 'NONE',  ( 0.000000000000000000, -0.8660254037844363761, -0.5000000000000039968 ) ) ;
#43068 = EDGE_CURVE ( 'NONE', #16005, #43091, #44447, .T. ) ;
#43069 = CIRCLE ( 'NONE', #23902, 16.00000000000000000 ) ;
#43070 = CARTESIAN_POINT ( 'NONE',  ( 97.30629616937498838, 90.00000000000002842, 83.13406250086715943 ) ) ;
#43071 = AXIS2_PLACEMENT_3D ( 'NONE', #199, #68952, #33230 ) ;
#43072 = VECTOR ( 'NONE', #18996, 1000.000000000000000 ) ;
#43073 = CARTESIAN_POINT ( 'NONE',  ( -92.69370383062498320, -211.3315407142195852, 84.35114583420050849 ) ) ;
#43074 = CARTESIAN_POINT ( 'NONE',  ( 0.000000000000000000, 11.30684508768339569, 76.66974797899841576 ) ) ;
#43075 = VERTEX_POINT ( 'NONE', #26399 ) ;
#43076 = DIRECTION ( 'NONE',  ( -1.000000000000000000, 0.000000000000000000, 0.000000000000000000 ) ) ;
#43077 = CARTESIAN_POINT ( 'NONE',  ( -93.67499999999998295, -212.2949673200287179, 78.78166666666666629 ) ) ;
#43078 = DIRECTION ( 'NONE',  ( 0.000000000000000000, 0.000000000000000000, 1.000000000000000000 ) ) ;
#43079 = EDGE_CURVE ( 'NONE', #42336, #38466, #42965, .T. ) ;
#43080 = ADVANCED_FACE ( 'NONE', ( #20006 ), #32398, .F. ) ;
#43081 = AXIS2_PLACEMENT_3D ( 'NONE', #54510, #47752, #35723 ) ;
#43082 = CIRCLE ( 'NONE', #34685, 16.00000000000000000 ) ;
#43083 = CARTESIAN_POINT ( 'NONE',  ( 95.00000000000000000, -212.6630814284392557, 83.45156250086714067 ) ) ;
#43084 = ORIENTED_EDGE ( 'NONE', *, *, #15952, .F. ) ;
#43085 = DIRECTION ( 'NONE',  ( -1.000000000000000000, -0.000000000000000000, -0.000000000000000000 ) ) ;
#43086 = ORIENTED_EDGE ( 'NONE', *, *, #58654, .T. ) ;
#43087 = ORIENTED_EDGE ( 'NONE', *, *, #19577, .F. ) ;
#43088 = VECTOR ( 'NONE', #38522, 1000.000000000000114 ) ;
#43089 = CARTESIAN_POINT ( 'NONE',  ( 1.560000000000000053, 0.8660254037844389297, 1.500000000000000000 ) ) ;
#43090 = VECTOR ( 'NONE', #49558, 1000.000000000000000 ) ;
#43091 = VERTEX_POINT ( 'NONE', #72611 ) ;
#43092 = CIRCLE ( 'NONE', #74256, 77.49900000000000944 ) ;
#43093 = DIRECTION ( 'NONE',  ( -0.7585478161175706058, -0.6516173805718078471, 0.000000000000000000 ) ) ;
#43094 = AXIS2_PLACEMENT_3D ( 'NONE', #52672, #7920, #41758 ) ;
#43095 = CARTESIAN_POINT ( 'NONE',  ( 96.15314808468748708, -208.0026889286704943, 77.52489583420047836 ) ) ;
#43096 = DIRECTION ( 'NONE',  ( 1.000000000000000000, 0.000000000000000000, 0.000000000000000000 ) ) ;
#43097 = DIRECTION ( 'NONE',  ( -0.000000000000000000, -0.000000000000000000, 1.000000000000000000 ) ) ;
#43098 = AXIS2_PLACEMENT_3D ( 'NONE', #50168, #73102, #9600 ) ;
#43099 = DIRECTION ( 'NONE',  ( 0.000000000000000000, 0.000000000000000000, 1.000000000000000000 ) ) ;
#43100 =( BOUNDED_CURVE ( )  B_SPLINE_CURVE ( 2, ( #34615, #35368, #11317, #74096, #57192, #63582, #40266, #22233, #62856 ),
 .UNSPECIFIED., .F., .F. ) 
 B_SPLINE_CURVE_WITH_KNOTS ( ( 3, 2, 2, 2, 3 ),
 ( 0.2751748541904413536, 0.2822306216352944430, 0.2892863871761764960, 0.2963421527170586045, 0.2963422021981254040 ),
 .UNSPECIFIED. ) 
 CURVE ( )  GEOMETRIC_REPRESENTATION_ITEM ( )  RATIONAL_B_SPLINE_CURVE ( ( 1.000000000000000000, 0.8660254037844387076, 1.000000000000000000, 0.8660254037844387076, 1.000000000000000000, 0.8660254037844387076, 1.000000000000000000, 0.9999990604554662710, 0.9999981209241102231 ) ) 
 REPRESENTATION_ITEM ( '' )  );
#43101 = CARTESIAN_POINT ( 'NONE',  ( 11.99999999999999822, -51.29473840253177741, -63.97538442413483750 ) ) ;
#43102 = CARTESIAN_POINT ( 'NONE',  ( 92.35000000000002274, -211.5299782133524502, 80.52791666666665549 ) ) ;
#43103 = ORIENTED_EDGE ( 'NONE', *, *, #14319, .T. ) ;
#43104 = VERTEX_POINT ( 'NONE', #27122 ) ;
#43105 = ORIENTED_EDGE ( 'NONE', *, *, #59350, .T. ) ;
#43106 = ORIENTED_EDGE ( 'NONE', *, *, #55346, .T. ) ;
#43107 = DIRECTION ( 'NONE',  ( -1.000000000000000000, 0.000000000000000000, 0.000000000000000000 ) ) ;
#43108 = CARTESIAN_POINT ( 'NONE',  ( -92.69370383062502583, 91.33154071421968467, 85.09197916753380753 ) ) ;
#43109 = DIRECTION ( 'NONE',  ( 0.000000000000000000, -0.9969173337331287410, 0.07845909572783495156 ) ) ;
#43110 = EDGE_CURVE ( 'NONE', #69197, #39310, #72982, .T. ) ;
#43111 = CARTESIAN_POINT ( 'NONE',  ( 0.000000000000000000, -3.925862922256468046, 41.81611651403860463 ) ) ;
#43112 = DIRECTION ( 'NONE',  ( 1.000000000000000000, 0.000000000000000000, 0.000000000000000000 ) ) ;
#43113 = ADVANCED_FACE ( 'NONE', ( #60265 ), #60982, .T. ) ;
#43114 = ORIENTED_EDGE ( 'NONE', *, *, #41843, .T. ) ;
#43115 = CIRCLE ( 'NONE', #74328, 77.49900000000000944 ) ;
#43116 = CARTESIAN_POINT ( 'NONE',  ( -96.32499999999996021, -212.2949673200287179, 87.64520833506762187 ) ) ;
#43117 = VERTEX_POINT ( 'NONE', #21486 ) ;
#43118 = FACE_OUTER_BOUND ( 'NONE', #7142, .T. ) ;
#43120 = ORIENTED_EDGE ( 'NONE', *, *, #24786, .F. ) ;
#43119 = EDGE_CURVE ( 'NONE', #7439, #67004, #56084, .T. ) ;
#43121 = CARTESIAN_POINT ( 'NONE',  ( -93.67500000000003979, 92.29496732002878900, 87.96270833506763154 ) ) ;
#43122 = VECTOR ( 'NONE', #68922, 999.9999999999998863 ) ;
#43123 = EDGE_LOOP ( 'NONE', ( #41189, #61754, #69248, #65485 ) ) ;
#43124 = CARTESIAN_POINT ( 'NONE',  ( 92.69370383062498320, 91.33154071421968467, 85.30364583420048064 ) ) ;
#43125 = CARTESIAN_POINT ( 'NONE',  ( 0.000000000000000000, 26.79245525562762253, -32.34446384429942611 ) ) ;
#43126 = CIRCLE ( 'NONE', #62336, 77.49900000000000944 ) ;
#43127 = EDGE_CURVE ( 'NONE', #61999, #7767, #55342, .T. ) ;
#43128 = CARTESIAN_POINT ( 'NONE',  ( 10.00000000000000000, 64.81221759200417409, -50.23322058963275794 ) ) ;
#43129 = LINE ( 'NONE', #49850, #10225 ) ;
#43130 = DIRECTION ( 'NONE',  ( 0.000000000000000000, -0.000000000000000000, 1.000000000000000000 ) ) ;
#43131 = ORIENTED_EDGE ( 'NONE', *, *, #18913, .T. ) ;
#43132 = CARTESIAN_POINT ( 'NONE',  ( 2.074714256722481664, -4.575665857285986959, -5.989444439476606874 ) ) ;
#43133 = CARTESIAN_POINT ( 'NONE',  ( 0.000000000000000000, 0.000000000000000000, 125.0000000000000000 ) ) ;
#43134 = ORIENTED_EDGE ( 'NONE', *, *, #70463, .F. ) ;
#43135 = AXIS2_PLACEMENT_3D ( 'NONE', #60533, #9757, #67275 ) ;
#43136 = EDGE_CURVE ( 'NONE', #22755, #52246, #65901, .T. ) ;
#43137 = EDGE_LOOP ( 'NONE', ( #59075, #3532 ) ) ;
#43138 = AXIS2_PLACEMENT_3D ( 'NONE', #55175, #48424, #30747 ) ;
#43139 = LINE ( 'NONE', #19068, #10984 ) ;
#43140 = CARTESIAN_POINT ( 'NONE',  ( -31.74999999999995737, 0.000000000000000000, 3.000000000000000888 ) ) ;
#43141 = CARTESIAN_POINT ( 'NONE',  ( 11.99999999999999822, -34.44570377933647620, 69.42325613327427902 ) ) ;
#43142 = CARTESIAN_POINT ( 'NONE',  ( -96.15314808468747287, -208.0026889286704943, 84.61572916753381435 ) ) ;
#43143 = ORIENTED_EDGE ( 'NONE', *, *, #67831, .F. ) ;
#43144 = EDGE_CURVE ( 'NONE', #33185, #20050, #38426, .T. ) ;
#43145 = CARTESIAN_POINT ( 'NONE',  ( -99.99999999999997158, -214.9999999999999716, 90.00000000000000000 ) ) ;
#43146 = ORIENTED_EDGE ( 'NONE', *, *, #58317, .T. ) ;
#43147 = AXIS2_PLACEMENT_3D ( 'NONE', #39729, #52463, #74297 ) ;
#43148 = AXIS2_PLACEMENT_3D ( 'NONE', #72269, #43724, #20769 ) ;
#43149 = DIRECTION ( 'NONE',  ( 0.000000000000000000, -0.1564344650402172410, -0.9876883405951399908 ) ) ;
#43150 = AXIS2_PLACEMENT_3D ( 'NONE', #3061, #48883, #20318 ) ;
#43151 = VECTOR ( 'NONE', #4847, 1000.000000000000000 ) ;
#43152 = LINE ( 'NONE', #2944, #59944 ) ;
#43153 = DIRECTION ( 'NONE',  ( 0.000000000000000000, 0.000000000000000000, -1.000000000000000000 ) ) ;
#43154 = CARTESIAN_POINT ( 'NONE',  ( 92.69370383062498320, 90.00000000000002842, 78.21281250086714465 ) ) ;
#43155 = LINE ( 'NONE', #8176, #34055 ) ;
#43156 = FACE_OUTER_BOUND ( 'NONE', #50087, .T. ) ;
#43157 = DIRECTION ( 'NONE',  ( 1.000000000000000000, 0.000000000000000000, 0.000000000000000000 ) ) ;
#43158 = AXIS2_PLACEMENT_3D ( 'NONE', #10068, #32989, #9703 ) ;
#43159 = CARTESIAN_POINT ( 'NONE',  ( -9.974659986866640793E-15, -5.773502691896262640, -5.553418012614792509 ) ) ;
#43160 = DIRECTION ( 'NONE',  ( 0.000000000000000000, 0.000000000000000000, 1.000000000000000000 ) ) ;
#43161 = EDGE_CURVE ( 'NONE', #42263, #54097, #44067, .T. ) ;
#43162 = CARTESIAN_POINT ( 'NONE',  ( 10.00000000000000000, 0.000000000000000000, 0.000000000000000000 ) ) ;
#43163 = ADVANCED_FACE ( 'NONE', ( #14380 ), #10216, .F. ) ;
#43164 = APPLICATION_CONTEXT ( 'automotive_design' ) ;
#43165 = AXIS2_PLACEMENT_3D ( 'NONE', #25418, #60013, #31413 ) ;
#43166 = DIRECTION ( 'NONE',  ( 0.000000000000000000, -0.8090169943749531134, 0.5877852522924654766 ) ) ;
#43167 = PRODUCT_DEFINITION_CONTEXT ( 'detailed design', #52245, 'design' ) ;
#43168 = DIRECTION ( 'NONE',  ( -1.000000000000000000, -0.000000000000000000, 0.000000000000000000 ) ) ;
#43169 = ORIENTED_EDGE ( 'NONE', *, *, #52705, .F. ) ;
#43170 = B_SPLINE_CURVE_WITH_KNOTS ( 'NONE', 1,
 ( #46562, #28898 ),
 .UNSPECIFIED., .F., .F.,
 ( 2, 2 ),
 ( 0.000000000000000000, 1.000000000000000000 ),
 .UNSPECIFIED. ) ;
#43171 = CARTESIAN_POINT ( 'NONE',  ( -95.00000000000002842, 87.33691857156074434, 82.81656250086712134 ) ) ;
#43172 = DIRECTION ( 'NONE',  ( -1.000000000000000000, -0.000000000000000000, -0.000000000000000000 ) ) ;
#43173 = CARTESIAN_POINT ( 'NONE',  ( 21.07894319797337701, -103.8699611390234878, -2.500000000000000444 ) ) ;
#43174 = ORIENTED_EDGE ( 'NONE', *, *, #22323, .F. ) ;
#43176 = CARTESIAN_POINT ( 'NONE',  ( -97.65000000000001990, 90.00000000000004263, 90.00000000000000000 ) ) ;
#43175 = AXIS2_PLACEMENT_3D ( 'NONE', #32373, #50409, #62080 ) ;
#43177 = DIRECTION ( 'NONE',  ( -1.000000000000000000, 0.000000000000000000, 0.000000000000000000 ) ) ;
#43178 = CARTESIAN_POINT ( 'NONE',  ( 11.99999999999999822, -65.58780272294048075, -36.73666225445966660 ) ) ;
#43179 = AXIS2_PLACEMENT_3D ( 'NONE', #61772, #27914, #38834 ) ;
#43180 = VECTOR ( 'NONE', #31115, 1000.000000000000000 ) ;
#43181 = CIRCLE ( 'NONE', #7162, 82.00000000000000000 ) ;
#43182 = CARTESIAN_POINT ( 'NONE',  ( 92.69370383062501162, -211.3315407142195852, 79.05947916753382287 ) ) ;
#43183 = AXIS2_PLACEMENT_3D ( 'NONE', #22455, #15698, #38637 ) ;
#43184 = ORIENTED_EDGE ( 'NONE', *, *, #60968, .F. ) ;
#43185 = ORIENTED_EDGE ( 'NONE', *, *, #29943, .F. ) ;
#43186 = EDGE_CURVE ( 'NONE', #43075, #42393, #71509, .T. ) ;
#43187 = DIRECTION ( 'NONE',  ( -1.000000000000000000, 0.000000000000000000, 0.000000000000000000 ) ) ;
#43188 = DIRECTION ( 'NONE',  ( -1.000000000000000000, -0.000000000000000000, 0.000000000000000000 ) ) ;
#43189 = CARTESIAN_POINT ( 'NONE',  ( -2.499999999999971578, 69.70000000000001705, -204.9999999999999716 ) ) ;
#43190 = ORIENTED_EDGE ( 'NONE', *, *, #19825, .F. ) ;
#43191 = CARTESIAN_POINT ( 'NONE',  ( -5.000000000000000000, 2.886751345948126879, -6.000000000000000000 ) ) ;
#43192 = CARTESIAN_POINT ( 'NONE',  ( 92.69370383062501162, -208.6684592857803011, 77.68364583420047609 ) ) ;
#43193 = CIRCLE ( 'NONE', #13110, 15.70000000000000284 ) ;
#43194 = ORIENTED_EDGE ( 'NONE', *, *, #24304, .F. ) ;
#43195 = CARTESIAN_POINT ( 'NONE',  ( 97.64999999999999147, 90.00000000000002842, 90.00000000000000000 ) ) ;
#43196 = ORIENTED_EDGE ( 'NONE', *, *, #50527, .F. ) ;
#43197 = ORIENTED_EDGE ( 'NONE', *, *, #19258, .F. ) ;
#43198 = CARTESIAN_POINT ( 'NONE',  ( -97.65000000000010516, 88.47002178664759242, 83.06791666666666174 ) ) ;
#43199 = VECTOR ( 'NONE', #35149, 1000.000000000000000 ) ;
#43200 = VECTOR ( 'NONE', #22411, 1000.000000000000000 ) ;
#43201 = CARTESIAN_POINT ( 'NONE',  ( 0.000000000000000000, 73.95703589263973754, 23.16143007188453851 ) ) ;
#43202 = EDGE_CURVE ( 'NONE', #66290, #29385, #54607, .T. ) ;
#43203 = CIRCLE ( 'NONE', #10782, 77.49899999999999523 ) ;
#43204 = ORIENTED_EDGE ( 'NONE', *, *, #44555, .T. ) ;
#43205 = CARTESIAN_POINT ( 'NONE',  ( 0.000000000000000000, 74.65491531819118620, -8.830959090342659579 ) ) ;
#43206 = CARTESIAN_POINT ( 'NONE',  ( 93.67500000000001137, -207.7050326799711968, 81.71854166840095957 ) ) ;
#43207 = CARTESIAN_POINT ( 'NONE',  ( 96.32499999999997442, 92.29496732002878900, 84.70833333333332860 ) ) ;
#43208 = EDGE_CURVE ( 'NONE', #58563, #18479, #24635, .T. ) ;
#43209 = EDGE_LOOP ( 'NONE', ( #32173, #15618, #37981, #21276 ) ) ;
#43210 = DIRECTION ( 'NONE',  ( 0.000000000000000000, 0.000000000000000000, 1.000000000000000000 ) ) ;
#43211 = CARTESIAN_POINT ( 'NONE',  ( 10.00000000000000000, 0.000000000000000000, 0.000000000000000000 ) ) ;
#43212 = ORIENTED_EDGE ( 'NONE', *, *, #46293, .F. ) ;
#43213 = EDGE_LOOP ( 'NONE', ( #11190, #61611, #31684, #30681 ) ) ;
#43214 = CARTESIAN_POINT ( 'NONE',  ( -97.30629616937501680, 88.66845928578038638, 87.31447916753381833 ) ) ;
#43215 = CARTESIAN_POINT ( 'NONE',  ( 92.69370383062498320, 91.33154071421968467, 81.33489583420048064 ) ) ;
#43216 = ORIENTED_EDGE ( 'NONE', *, *, #3870, .F. ) ;
#43217 = CARTESIAN_POINT ( 'NONE',  ( 94.99999999999998579, 86.94004357329500010, 82.61812500173428475 ) ) ;
#43218 = EDGE_CURVE ( 'NONE', #7502, #52797, #62102, .T. ) ;
#43219 = ADVANCED_FACE ( 'NONE', ( #40278 ), #35011, .F. ) ;
#43220 = CARTESIAN_POINT ( 'NONE',  ( 0.000000000000000000, -65.58780272294048075, -36.73666225445966660 ) ) ;
#43221 = ORIENTED_EDGE ( 'NONE', *, *, #42039, .F. ) ;
#43222 = CARTESIAN_POINT ( 'NONE',  ( 95.00000000000000000, -213.0599564267049857, 78.09374999999998579 ) ) ;
#43223 = ORIENTED_EDGE ( 'NONE', *, *, #38258, .F. ) ;
#43224 = ORIENTED_EDGE ( 'NONE', *, *, #41961, .F. ) ;
#43225 = ORIENTED_EDGE ( 'NONE', *, *, #55184, .F. ) ;
#43226 = FACE_OUTER_BOUND ( 'NONE', #30302, .T. ) ;
#43227 = DIRECTION ( 'NONE',  ( 0.000000000000000000, 0.4999999999999998335, -0.8660254037844387076 ) ) ;
#43228 = CARTESIAN_POINT ( 'NONE',  ( -96.32500000000001705, 87.70503267997129626, 84.39083333333333314 ) ) ;
#43229 = ORIENTED_EDGE ( 'NONE', *, *, #73273, .F. ) ;
#43230 = LINE ( 'NONE', #49945, #27551 ) ;
#43231 = DIRECTION ( 'NONE',  ( -1.000000000000000000, 0.000000000000000000, 0.000000000000000000 ) ) ;
#43232 = ORIENTED_EDGE ( 'NONE', *, *, #722, .F. ) ;
#43233 = DIRECTION ( 'NONE',  ( 0.000000000000000000, 0.000000000000000000, 1.000000000000000000 ) ) ;
#43234 = CARTESIAN_POINT ( 'NONE',  ( -94.99999999999997158, -212.6630814284392557, 77.73656250086713726 ) ) ;
#43235 = ORIENTED_EDGE ( 'NONE', *, *, #72396, .T. ) ;
#43236 = AXIS2_PLACEMENT_3D ( 'NONE', #64533, #42344, #18652 ) ;
#43238 = EDGE_CURVE ( 'NONE', #50408, #59461, #33347, .T. ) ;
#43237 = CYLINDRICAL_SURFACE ( 'NONE', #9828, 15.69999999999999929 ) ;
#43239 = CARTESIAN_POINT ( 'NONE',  ( 0.000000000000000000, 27.13269053701096922, 25.88420570971410228 ) ) ;
#43240 = DIRECTION ( 'NONE',  ( 0.000000000000000000, -0.5877852522924801315, 0.8090169943749421222 ) ) ;
#43241 = DIRECTION ( 'NONE',  ( -1.000000000000000000, 0.000000000000000000, 0.000000000000000000 ) ) ;
#43242 = AXIS2_PLACEMENT_3D ( 'NONE', #64855, #36634, #42657 ) ;
#43243 = CIRCLE ( 'NONE', #54009, 30.50000000000000000 ) ;
#43244 = CARTESIAN_POINT ( 'NONE',  ( 97.64998666484373757, -208.4700140875914087, 83.46479220096851748 ) ) ;
#43245 = CARTESIAN_POINT ( 'NONE',  ( -17.26469406256017791, -140.1601175325492648, 5.500000000000000000 ) ) ;
#43247 = CARTESIAN_POINT ( 'NONE',  ( 93.84685191531248449, 91.99731107132950569, 88.90197916753380980 ) ) ;
#43246 = CIRCLE ( 'NONE', #48053, 1.000000000000000888 ) ;
#43248 = CARTESIAN_POINT ( 'NONE',  ( -97.65000000000003411, -211.5299782133523934, 85.60791666666665378 ) ) ;
#43249 = DIRECTION ( 'NONE',  ( 0.000000000000000000, 0.000000000000000000, 1.000000000000000000 ) ) ;
#43250 = DIRECTION ( 'NONE',  ( 0.000000000000000000, 0.000000000000000000, 1.000000000000000000 ) ) ;
#43251 = EDGE_CURVE ( 'NONE', #24836, #8405, #10968, .T. ) ;
#43252 = CARTESIAN_POINT ( 'NONE',  ( -97.30629616937501680, 91.33154071421968467, 76.25489583420049655 ) ) ;
#43253 = DIRECTION ( 'NONE',  ( -1.000000000000000000, 0.000000000000000000, -0.000000000000000000 ) ) ;
#43254 = CARTESIAN_POINT ( 'NONE',  ( 0.000000000000000000, -0.9646360437372163421, -23.52805723605591126 ) ) ;
#43255 = FACE_OUTER_BOUND ( 'NONE', #22659, .T. ) ;
#43256 = EDGE_CURVE ( 'NONE', #51311, #14366, #57944, .T. ) ;
#43257 = LINE ( 'NONE', #43621, #64070 ) ;
#43258 = AXIS2_PLACEMENT_3D ( 'NONE', #53680, #20198, #55539 ) ;
#43259 = CARTESIAN_POINT ( 'NONE',  ( 10.00000000000000000, 2.543863470249530856, -81.96053171279901051 ) ) ;
#43261 = FACE_OUTER_BOUND ( 'NONE', #36220, .T. ) ;
#43260 = AXIS2_PLACEMENT_3D ( 'NONE', #71939, #20453, #2088 ) ;
#43262 = VECTOR ( 'NONE', #48934, 1000.000000000000000 ) ;
#43263 = CARTESIAN_POINT ( 'NONE',  ( 97.64999999999999147, -209.9999999999999716, 77.61749999999999261 ) ) ;
#43264 = CYLINDRICAL_SURFACE ( 'NONE', #34046, 2.499999999999999556 ) ;
#43265 = CARTESIAN_POINT ( 'NONE',  ( -92.34999999999999432, -211.5299782133524502, 88.99458333333333826 ) ) ;
#43266 = CIRCLE ( 'NONE', #32438, 32.00000000000000000 ) ;
#43267 = AXIS2_PLACEMENT_3D ( 'NONE', #18108, #12453, #29731 ) ;
#43268 = CARTESIAN_POINT ( 'NONE',  ( 0.000000000000000000, 0.000000000000000000, -43.79999999999998295 ) ) ;
#43269 = EDGE_LOOP ( 'NONE', ( #46707, #268, #16309, #44203 ) ) ;
#43270 = DIRECTION ( 'NONE',  ( -1.000000000000000000, 0.000000000000000000, 0.000000000000000000 ) ) ;
#43271 = CARTESIAN_POINT ( 'NONE',  ( 10.00000000000000000, -21.32104025579091910, -30.84782396557241313 ) ) ;
#43272 = CARTESIAN_POINT ( 'NONE',  ( 10.00000000000000000, 5.202137450156907761, -37.22597642581151689 ) ) ;
#43273 = CIRCLE ( 'NONE', #58883, 82.00000000000000000 ) ;
#43274 = EDGE_LOOP ( 'NONE', ( #27587, #72857, #37201, #16441 ) ) ;
#43275 = ORIENTED_EDGE ( 'NONE', *, *, #37441, .F. ) ;
#43276 = CARTESIAN_POINT ( 'NONE',  ( 0.000000000000000000, 0.000000000000000000, 0.000000000000000000 ) ) ;
#43277 = DIRECTION ( 'NONE',  ( 0.000000000000000000, 0.000000000000000000, 1.000000000000000000 ) ) ;
#43278 = VERTEX_POINT ( 'NONE', #21870 ) ;
#43279 = ADVANCED_FACE ( 'NONE', ( #51922 ), #10582, .T. ) ;
#43280 = CARTESIAN_POINT ( 'NONE',  ( 95.00000000000000000, -207.3369185715606307, 80.59406250086715318 ) ) ;
#43281 = CARTESIAN_POINT ( 'NONE',  ( 92.69370383062501162, -208.6684592857803295, 85.30364583420048064 ) ) ;
#43282 = ORIENTED_EDGE ( 'NONE', *, *, #39639, .T. ) ;
#43283 = CARTESIAN_POINT ( 'NONE',  ( 92.69370383062501162, -208.6684592857803011, 85.93864583420048575 ) ) ;
#43284 = VERTEX_POINT ( 'NONE', #28614 ) ;
#43285 = CARTESIAN_POINT ( 'NONE',  ( -10.00000000000000000, 0.000000000000000000, 0.000000000000000000 ) ) ;
#43286 = ORIENTED_EDGE ( 'NONE', *, *, #9609, .T. ) ;
#43287 = VECTOR ( 'NONE', #57021, 1000.000000000000000 ) ;
#43288 = CARTESIAN_POINT ( 'NONE',  ( -93.84685191531254134, 91.99731107132950569, 78.15989583420049769 ) ) ;
#43289 = ADVANCED_FACE ( 'NONE', ( #34259 ), #50439, .F. ) ;
#43290 = ORIENTED_EDGE ( 'NONE', *, *, #73766, .T. ) ;
#43291 = VERTEX_POINT ( 'NONE', #74110 ) ;
#43292 = VECTOR ( 'NONE', #4477, 1000.000000000000000 ) ;
#43293 = CARTESIAN_POINT ( 'NONE',  ( 0.000000000000000000, -65.59268652807183742, -36.72794159290312166 ) ) ;
#43294 = EDGE_CURVE ( 'NONE', #46015, #45314, #69424, .T. ) ;
#43295 = ORIENTED_EDGE ( 'NONE', *, *, #29714, .T. ) ;
#43296 = DIRECTION ( 'NONE',  ( -0.000000000000000000, 0.5000000000000038858, 0.8660254037844363761 ) ) ;
#43297 = PRESENTATION_STYLE_ASSIGNMENT (( #19956 ) ) ;
#43298 = ORIENTED_EDGE ( 'NONE', *, *, #67960, .F. ) ;
#43299 = LINE ( 'NONE', #55295, #47850 ) ;
#43300 = ORIENTED_EDGE ( 'NONE', *, *, #58478, .F. ) ;
#43301 = CARTESIAN_POINT ( 'NONE',  ( 92.35000000000000853, -209.9999627172523162, 81.18937371225271704 ) ) ;
#43302 = VERTEX_POINT ( 'NONE', #108 ) ;
#43303 = CIRCLE ( 'NONE', #46888, 12.49999999999999645 ) ;
#43304 = ADVANCED_FACE ( 'NONE', ( #45935 ), #22621, .T. ) ;
#43305 = ORIENTED_EDGE ( 'NONE', *, *, #35783, .T. ) ;
#43306 = ORIENTED_EDGE ( 'NONE', *, *, #59661, .F. ) ;
#43307 = CARTESIAN_POINT ( 'NONE',  ( 95.00000000000000000, -207.3369185715606307, 78.05406250086714692 ) ) ;
#43308 = PLANE ( 'NONE',  #28063 ) ;
#43309 = ITEM_DEFINED_TRANSFORMATION ( 'NONE', 'NONE', #33982,  #43395 ) ;
#43310 = CARTESIAN_POINT ( 'NONE',  ( 2.369999999999999662, 5.817072295949927426E-16, -4.750000000000000000 ) ) ;
#43311 = VERTEX_POINT ( 'NONE', #39170 ) ;
#43312 = ORIENTED_EDGE ( 'NONE', *, *, #20454, .T. ) ;
#43313 = DIRECTION ( 'NONE',  ( 0.000000000000000000, 0.000000000000000000, 1.000000000000000000 ) ) ;
#43314 = ORIENTED_EDGE ( 'NONE', *, *, #45709, .T. ) ;
#43315 = DIRECTION ( 'NONE',  ( -2.628368902995164490E-16, -1.000000000000000000, 0.000000000000000000 ) ) ;
#43316 = VECTOR ( 'NONE', #12758, 1000.000000000000000 ) ;
#43317 = CARTESIAN_POINT ( 'NONE',  ( -11.99999999999999645, 13.90444123027096879, 0.000000000000000000 ) ) ;
#43318 = CARTESIAN_POINT ( 'NONE',  ( -97.30629616937501680, 91.33154071421968467, 80.22364583420048234 ) ) ;
#43319 = ORIENTED_EDGE ( 'NONE', *, *, #65447, .F. ) ;
#43320 = ADVANCED_FACE ( 'NONE', ( #45567 ), #33509, .F. ) ;
#43321 = CARTESIAN_POINT ( 'NONE',  ( 96.15314808468748708, 88.00268892867053694, 76.51947916753380241 ) ) ;
#43322 =( BOUNDED_CURVE ( )  B_SPLINE_CURVE ( 2, ( #60610, #53480, #71490, #19990, #53112, #13617, #36922 ),
 .UNSPECIFIED., .F., .F. ) 
 B_SPLINE_CURVE_WITH_KNOTS ( ( 3, 2, 2, 3 ),
 ( 0.02083333333333322115, 0.02777777777777762705, 0.03472222222222204335, 0.04166666666666644231 ),
 .UNSPECIFIED. ) 
 CURVE ( )  GEOMETRIC_REPRESENTATION_ITEM ( )  RATIONAL_B_SPLINE_CURVE ( ( 1.000000000000002220, 0.8660254037844365982, 1.000000000000000000, 0.8660254037844387076, 1.000000000000000000, 0.8660254037844430375, 0.9999999999999956701 ) ) 
 REPRESENTATION_ITEM ( '' )  );
#43323 = EDGE_LOOP ( 'NONE', ( #64923, #28767, #61993, #42831 ) ) ;
#43324 = DIRECTION ( 'NONE',  ( 1.000000000000000000, 0.000000000000000000, 0.000000000000000000 ) ) ;
#43325 = CYLINDRICAL_SURFACE ( 'NONE', #6004, 16.00000000000000000 ) ;
#43327 = EDGE_CURVE ( 'NONE', #30858, #71384, #23823, .T. ) ;
#43326 = CARTESIAN_POINT ( 'NONE',  ( 96.91640186574962001, 88.16968857444116736, 74.99954695036821306 ) ) ;
#43328 = DIRECTION ( 'NONE',  ( 0.000000000000000000, -0.9969173337331271867, -0.07845909572785571273 ) ) ;
#43329 = DIRECTION ( 'NONE',  ( 0.000000000000000000, 0.4539904997395477482, -0.8910065241883673437 ) ) ;
#43330 = EDGE_CURVE ( 'NONE', #29098, #42263, #14199, .T. ) ;
#43331 = CARTESIAN_POINT ( 'NONE',  ( -96.15314808468747287, -208.0026889286704943, 84.45697916753380241 ) ) ;
#43332 = CARTESIAN_POINT ( 'NONE',  ( 0.000000000000000000, 71.91182617369187824, 28.89263327155772387 ) ) ;
#43333 = EDGE_CURVE ( 'NONE', #59348, #40890, #40650, .T. ) ;
#43334 = DIRECTION ( 'NONE',  ( -1.000000000000000000, -0.000000000000000000, -0.000000000000000000 ) ) ;
#43335 = ORIENTED_EDGE ( 'NONE', *, *, #36891, .F. ) ;
#43336 = VERTEX_POINT ( 'NONE', #53041 ) ;
#43337 = FACE_BOUND ( 'NONE', #60193, .T. ) ;
#43338 = DIRECTION ( 'NONE',  ( -1.000000000000000000, 0.000000000000000000, 0.000000000000000000 ) ) ;
#43339 = CARTESIAN_POINT ( 'NONE',  ( -3.000000000000002665, 0.000000000000000000, 0.000000000000000000 ) ) ;
#43340 = EDGE_CURVE ( 'NONE', #73769, #34394, #57414, .T. ) ;
#43341 = CARTESIAN_POINT ( 'NONE',  ( -95.00000000000002842, 92.66308142843932671, 85.03906250086714635 ) ) ;
#43342 = CARTESIAN_POINT ( 'NONE',  ( -96.73564493164495559, -208.2604367189442200, 74.87701898318920257 ) ) ;
#43343 = LINE ( 'NONE', #8741, #26575 ) ;
#43344 = CARTESIAN_POINT ( 'NONE',  ( 15.00000000000000000, 26.49999999999999645, 1.499999999999995781 ) ) ;
#43345 = ORIENTED_EDGE ( 'NONE', *, *, #2840, .T. ) ;
#43346 = DIRECTION ( 'NONE',  ( 1.000000000000000000, 1.427937372958405461E-15, 7.962523111839130290E-16 ) ) ;
#43347 = AXIS2_PLACEMENT_3D ( 'NONE', #12980, #40845, #70126 ) ;
#43348 = CIRCLE ( 'NONE', #22946, 77.49899999999999523 ) ;
#43349 = DIRECTION ( 'NONE',  ( -1.000000000000000000, 0.000000000000000000, -0.000000000000000000 ) ) ;
#43350 = LINE ( 'NONE', #66986, #72947 ) ;
#43351 = DIRECTION ( 'NONE',  ( -1.000000000000000000, -0.000000000000000000, -0.000000000000000000 ) ) ;
#43352 = FACE_OUTER_BOUND ( 'NONE', #25583, .T. ) ;
#43353 = CARTESIAN_POINT ( 'NONE',  ( 6.000000000000000000, -81.90746397400386059, -3.894527615418766242 ) ) ;
#43354 = CARTESIAN_POINT ( 'NONE',  ( 0.000000000000000000, 0.000000000000000000, 0.000000000000000000 ) ) ;
#43355 = CARTESIAN_POINT ( 'NONE',  ( -93.84685191531247028, -211.9973110713294489, 83.02822916753380866 ) ) ;
#43356 = DIRECTION ( 'NONE',  ( -1.000000000000000000, 0.000000000000000000, -0.000000000000000000 ) ) ;
#43357 = CARTESIAN_POINT ( 'NONE',  ( 10.00000000000000000, 0.000000000000000000, 0.000000000000000000 ) ) ;
#43358 = DIRECTION ( 'NONE',  ( -1.000000000000000000, 0.000000000000000000, 0.000000000000000000 ) ) ;
#43359 = CARTESIAN_POINT ( 'NONE',  ( 92.34999999999999432, 90.00000000000002842, 88.73000000000000398 ) ) ;
#43360 = AXIS2_PLACEMENT_3D ( 'NONE', #15378, #71771, #43610 ) ;
#43361 = VERTEX_POINT ( 'NONE', #24830 ) ;
#43362 = LINE ( 'NONE', #59906, #1729 ) ;
#43363 = CARTESIAN_POINT ( 'NONE',  ( 0.000000000000000000, 68.27212725128275395, 31.46837873495001503 ) ) ;
#43364 = CARTESIAN_POINT ( 'NONE',  ( 0.000000000000000000, 46.11716303203186840, 67.80270845531904911 ) ) ;
#43365 = AXIS2_PLACEMENT_3D ( 'NONE', #61525, #62273, #31537 ) ;
#43366 = VECTOR ( 'NONE', #38396, 1000.000000000000000 ) ;
#43367 = AXIS2_PLACEMENT_3D ( 'NONE', #59894, #33421, #27795 ) ;
#43368 = CARTESIAN_POINT ( 'NONE',  ( 0.000000000000000000, -0.8299999999999999600, 0.000000000000000000 ) ) ;
#43369 = ORIENTED_EDGE ( 'NONE', *, *, #66562, .F. ) ;
#43370 = CARTESIAN_POINT ( 'NONE',  ( 11.99999999999999822, -26.02418014898260878, -70.52718814184285634 ) ) ;
#43371 = DIRECTION ( 'NONE',  ( 0.000000000000000000, 0.000000000000000000, -1.000000000000000000 ) ) ;
#43372 = ORIENTED_EDGE ( 'NONE', *, *, #4776, .F. ) ;
#43373 = DIRECTION ( 'NONE',  ( -1.000000000000000000, 0.000000000000000000, 0.000000000000000000 ) ) ;
#43374 = ORIENTED_EDGE ( 'NONE', *, *, #73991, .T. ) ;
#43375 = ADVANCED_FACE ( 'NONE', ( #1215 ), #24109, .T. ) ;
#43376 = EDGE_CURVE ( 'NONE', #33774, #17478, #36849, .T. ) ;
#43377 = VERTEX_POINT ( 'NONE', #23722 ) ;
#43378 = CARTESIAN_POINT ( 'NONE',  ( 0.000000000000000000, 71.21200624218852226, -40.65526001592539984 ) ) ;
#43379 = EDGE_CURVE ( 'NONE', #62067, #73125, #1578, .T. ) ;
#43380 = ORIENTED_EDGE ( 'NONE', *, *, #4043, .F. ) ;
#43381 = ORIENTED_EDGE ( 'NONE', *, *, #18248, .F. ) ;
#43383 = EDGE_LOOP ( 'NONE', ( #12821, #48885, #32285, #33940, #23957, #59730, #48724, #17388, #66594, #26745, #28755, #53349, #21218, #44244, #72550, #68621 ) ) ;
#43382 = ADVANCED_FACE ( 'NONE', ( #25211 ), #6445, .T. ) ;
#43384 = ORIENTED_EDGE ( 'NONE', *, *, #26665, .F. ) ;
#43385 = CARTESIAN_POINT ( 'NONE',  ( 94.99999999999998579, 90.00000000000002842, 90.00000000000000000 ) ) ;
#43386 = EDGE_LOOP ( 'NONE', ( #8453, #72712, #50385, #27733 ) ) ;
#43387 = PRODUCT_DEFINITION_SHAPE ( 'NONE', 'NONE',  #63750 ) ;
#43389 = EDGE_CURVE ( 'NONE', #30416, #46309, #70674, .T. ) ;
#43388 = ORIENTED_EDGE ( 'NONE', *, *, #13670, .F. ) ;
#43390 = CARTESIAN_POINT ( 'NONE',  ( 96.15314808468748708, 88.00268892867053694, 76.67822916753381435 ) ) ;
#43391 = DIRECTION ( 'NONE',  ( 0.000000000000000000, -0.8090169943749530024, 0.5877852522924653655 ) ) ;
#43392 = LINE ( 'NONE', #9149, #30833 ) ;
#43393 = ORIENTED_EDGE ( 'NONE', *, *, #53498, .T. ) ;
#43394 = EDGE_LOOP ( 'NONE', ( #1899, #9331, #72904, #26811 ) ) ;
#43395 = AXIS2_PLACEMENT_3D ( 'NONE', #48320, #71232, #19735 ) ;
#43396 = VECTOR ( 'NONE', #17500, 1000.000000000000000 ) ;
#43397 = ORIENTED_EDGE ( 'NONE', *, *, #37848, .F. ) ;
#43398 = CARTESIAN_POINT ( 'NONE',  ( 97.30629616937498838, 91.33154071421968467, 88.74322916753379786 ) ) ;
#43399 = AXIS2_PLACEMENT_3D ( 'NONE', #42036, #12703, #8177 ) ;
#43400 = ORIENTED_EDGE ( 'NONE', *, *, #6547, .F. ) ;
#43401 = CARTESIAN_POINT ( 'NONE',  ( 92.69370383062501162, -209.9999999999999716, 89.00781250086714635 ) ) ;
#43402 = CARTESIAN_POINT ( 'NONE',  ( 8.500000000000035527, 73.00000000000001421, -255.0000000000000000 ) ) ;
#43403 = CARTESIAN_POINT ( 'NONE',  ( 96.32499999999997442, 92.29496732002878900, 84.07333333333333769 ) ) ;
#43405 = CIRCLE ( 'NONE', #30329, 3.299999999999983391 ) ;
#43404 = CARTESIAN_POINT ( 'NONE',  ( -97.49696879394610960, 90.24436280099767771, 74.91343443312149475 ) ) ;
#43406 = PLANE ( 'NONE',  #61763 ) ;
#43407 = DIRECTION ( 'NONE',  ( 0.000000000000000000, 0.000000000000000000, 1.000000000000000000 ) ) ;
#43408 = CARTESIAN_POINT ( 'NONE',  ( 8.452893869119503023, -12.51233732111638375, -1.199999999999999956 ) ) ;
#43409 = DIRECTION ( 'NONE',  ( -1.000000000000000000, 0.000000000000000000, 0.000000000000000000 ) ) ;
#43410 = CARTESIAN_POINT ( 'NONE',  ( -94.99999999999997158, -207.3369185715606307, 89.48406250086713953 ) ) ;
#43411 = CARTESIAN_POINT ( 'NONE',  ( -97.30629616937501680, 90.00000000000004263, 88.53156250086716739 ) ) ;
#43412 = VECTOR ( 'NONE', #24706, 1000.000000000000000 ) ;
#43413 = ORIENTED_EDGE ( 'NONE', *, *, #57579, .T. ) ;
#43415 = CARTESIAN_POINT ( 'NONE',  ( -92.69370383062504004, 90.00000000000004263, 89.32531250086714181 ) ) ;
#43414 = CARTESIAN_POINT ( 'NONE',  ( 96.15314808468748708, 88.00268892867053694, 87.31447916753380412 ) ) ;
#43416 = ORIENTED_EDGE ( 'NONE', *, *, #59584, .F. ) ;
#43417 = CARTESIAN_POINT ( 'NONE',  ( 93.84685191531248449, 88.00268892867053694, 76.57239583420049200 ) ) ;
#43418 = CARTESIAN_POINT ( 'NONE',  ( 97.64999999999999147, 90.00000000000002842, 82.06250000000000000 ) ) ;
#43419 = CARTESIAN_POINT ( 'NONE',  ( 93.67500000000001137, -212.2949673200287179, 87.56583333333333030 ) ) ;
#43420 = DIRECTION ( 'NONE',  ( 1.000000000000000000, -3.061616997868382648E-16, -0.000000000000000000 ) ) ;
#43421 = CARTESIAN_POINT ( 'NONE',  ( -92.35000000018069954, 89.99996905681452120, 78.33187387208522523 ) ) ;
#43422 = LINE ( 'NONE', #49403, #59338 ) ;
#43423 = CARTESIAN_POINT ( 'NONE',  ( -96.32499999999996021, -212.2949673200287179, 79.94583333333332575 ) ) ;
#43424 = CONICAL_SURFACE ( 'NONE', #73376, 2.055000000000000160, 0.7853981633974479459 ) ;
#43425 = EDGE_CURVE ( 'NONE', #68450, #30858, #7909, .T. ) ;
#43426 = ADVANCED_FACE ( 'NONE', ( #42500 ), #36112, .T. ) ;
#43427 = DIRECTION ( 'NONE',  ( 0.000000000000000000, -0.4539904997395351471, -0.8910065241883737830 ) ) ;
#43428 = ORIENTED_EDGE ( 'NONE', *, *, #54640, .T. ) ;
#43429 = CIRCLE ( 'NONE', #58971, 32.00000000000000711 ) ;
#43430 = EDGE_LOOP ( 'NONE', ( #72178, #54721, #35343, #48260 ) ) ;
#43431 = CIRCLE ( 'NONE', #3809, 77.49900000000000944 ) ;
#43432 = CARTESIAN_POINT ( 'NONE',  ( 11.99999999999999822, 0.000000000000000000, 0.000000000000000000 ) ) ;
#43433 = ADVANCED_FACE ( 'NONE', ( #30828 ), #41031, .F. ) ;
#43434 = CARTESIAN_POINT ( 'NONE',  ( 50.00005079999999680, 0.000000000000000000, 0.000000000000000000 ) ) ;
#43435 = CARTESIAN_POINT ( 'NONE',  ( -97.64999999950680376, -210.0000320386661485, 83.73041644189096644 ) ) ;
#43436 = DIRECTION ( 'NONE',  ( 0.000000000000000000, 0.000000000000000000, 1.000000000000000000 ) ) ;
#43437 = DIRECTION ( 'NONE',  ( -1.000000000000000000, 0.000000000000000000, 0.000000000000000000 ) ) ;
#43438 = CARTESIAN_POINT ( 'NONE',  ( 97.65000000000000568, 88.47002178664753558, 84.54958333333334508 ) ) ;
#43439 = ORIENTED_EDGE ( 'NONE', *, *, #28436, .T. ) ;
#43440 = CARTESIAN_POINT ( 'NONE',  ( -92.69370383062504004, 90.00000000000004263, 81.70531250086713726 ) ) ;
#43441 = FACE_OUTER_BOUND ( 'NONE', #26787, .T. ) ;
#43442 = DIRECTION ( 'NONE',  ( 1.000000000000000000, 0.000000000000000000, -0.000000000000000000 ) ) ;
#43443 = CARTESIAN_POINT ( 'NONE',  ( 0.000000000000000000, 74.65491531819118620, 23.16904090965732621 ) ) ;
#43444 = CARTESIAN_POINT ( 'NONE',  ( 11.99999999999999822, 71.91182617369190666, 28.89263327155770966 ) ) ;
#43445 = LINE ( 'NONE', #14091, #35342 ) ;
#43446 = DIRECTION ( 'NONE',  ( -1.000000000000000000, 0.000000000000000000, -0.000000000000000000 ) ) ;
#43447 = CARTESIAN_POINT ( 'NONE',  ( 97.64999999999999147, -209.9999998456624155, 79.60187500750917877 ) ) ;
#43448 = DIRECTION ( 'NONE',  ( -7.962523111839282146E-16, 1.065814103640130873E-14, 1.000000000000000000 ) ) ;
#43449 = CARTESIAN_POINT ( 'NONE',  ( 4.999999999999999112, 36.13751322684449008, -21.40280677340332716 ) ) ;
#43450 = CARTESIAN_POINT ( 'NONE',  ( 97.30629616937498838, 90.00000000000002842, 79.32406250086715715 ) ) ;
#43451 = CARTESIAN_POINT ( 'NONE',  ( -93.84685191531247028, -211.9973110713294489, 83.66322916753382799 ) ) ;
#43452 = DIRECTION ( 'NONE',  ( -0.000000000000000000, 0.000000000000000000, -1.000000000000000000 ) ) ;
#43453 = VERTEX_POINT ( 'NONE', #2315 ) ;
#43454 = DIRECTION ( 'NONE',  ( 0.000000000000000000, 0.000000000000000000, 1.000000000000000000 ) ) ;
#43455 = UNCERTAINTY_MEASURE_WITH_UNIT (LENGTH_MEASURE( 1.000000000000000082E-05 ), #29209, 'distance_accuracy_value', 'NONE');
#43456 = CIRCLE ( 'NONE', #33819, 37.49900000000000233 ) ;
#43457 = CARTESIAN_POINT ( 'NONE',  ( -97.64999999999996305, -209.9999999999999716, 79.20499999999999829 ) ) ;
#43458 = CARTESIAN_POINT ( 'NONE',  ( 95.00000000000000000, -206.9400435732949575, 78.41125000000000966 ) ) ;
#43459 = VECTOR ( 'NONE', #55335, 1000.000000000000000 ) ;
#43460 = CARTESIAN_POINT ( 'NONE',  ( 95.00000000000000000, -207.3369185715606307, 83.76906250086713612 ) ) ;
#43461 = VERTEX_POINT ( 'NONE', #7179 ) ;
#43462 = CIRCLE ( 'NONE', #49442, 15.70000000000000284 ) ;
#43463 = CARTESIAN_POINT ( 'NONE',  ( 0.000000000000000000, -21.60688246758530440, -79.10210256391390260 ) ) ;
#43464 = ORIENTED_EDGE ( 'NONE', *, *, #6862, .F. ) ;
#43465 = AXIS2_PLACEMENT_3D ( 'NONE', #51318, #16754, #22773 ) ;
#43466 = CARTESIAN_POINT ( 'NONE',  ( 10.00000000000000000, 64.81221759200342092, 50.23322058963369585 ) ) ;
#43467 = ORIENTED_EDGE ( 'NONE', *, *, #21083, .T. ) ;
#43468 = AXIS2_PLACEMENT_3D ( 'NONE', #44668, #32983, #49541 ) ;
#43469 = CARTESIAN_POINT ( 'NONE',  ( 0.000000000000000000, -107.5000000000000000, 40.00000000000000711 ) ) ;
#43470 = AXIS2_PLACEMENT_3D ( 'NONE', #57812, #6318, #56331 ) ;
#43471 = EDGE_CURVE ( 'NONE', #21162, #45686, #13904, .T. ) ;
#43472 = VECTOR ( 'NONE', #56190, 1000.000000000000000 ) ;
#43473 = ORIENTED_EDGE ( 'NONE', *, *, #29551, .T. ) ;
#43474 = EDGE_CURVE ( 'NONE', #63558, #26140, #1050, .T. ) ;
#43475 = CARTESIAN_POINT ( 'NONE',  ( 97.30629616937498838, -208.6684592857803295, 77.47197916753381719 ) ) ;
#43476 = CARTESIAN_POINT ( 'NONE',  ( 0.000000000000000000, 0.000000000000000000, 0.000000000000000000 ) ) ;
#43477 = LINE ( 'NONE', #31782, #64060 ) ;
#43478 = CARTESIAN_POINT ( 'NONE',  ( -97.50728577674146891, 89.65937732759918788, 74.92458348457971340 ) ) ;
#43479 = CARTESIAN_POINT ( 'NONE',  ( 0.000000000000000000, 9.615535125378773529, 24.73947219025917121 ) ) ;
#43480 = EDGE_CURVE ( 'NONE', #64655, #6829, #35378, .T. ) ;
#43481 = DIRECTION ( 'NONE',  ( 1.000000000000000000, 0.000000000000000000, 0.000000000000000000 ) ) ;
#43482 = CARTESIAN_POINT ( 'NONE',  ( 92.35000000000002274, -208.4700217866474645, 82.32708333333332007 ) ) ;
#43483 = ORIENTED_EDGE ( 'NONE', *, *, #6206, .F. ) ;
#43484 = ORIENTED_EDGE ( 'NONE', *, *, #59497, .F. ) ;
#43485 = ORIENTED_EDGE ( 'NONE', *, *, #32824, .T. ) ;
#43486 = ORIENTED_EDGE ( 'NONE', *, *, #47771, .T. ) ;
#43487 = CARTESIAN_POINT ( 'NONE',  ( 92.35000000000006537, -211.5299782133524218, 86.87791666666664980 ) ) ;
#43488 = CARTESIAN_POINT ( 'NONE',  ( -92.69370383062504004, 90.00000000000004263, 85.03906250086714635 ) ) ;
#43489 = CARTESIAN_POINT ( 'NONE',  ( 0.000000000000000000, -62.20884554314051940, 46.21855187248608132 ) ) ;
#43490 = LINE ( 'NONE', #3638, #61843 ) ;
#43491 = CARTESIAN_POINT ( 'NONE',  ( 94.99999999999998579, 86.94004357329500010, 76.18874999999999886 ) ) ;
#43492 = ADVANCED_FACE ( 'NONE', ( #71049 ), #19553, .T. ) ;
#43493 = CARTESIAN_POINT ( 'NONE',  ( 0.000000000000000000, 0.8660254037844389297, -1.500000000000000000 ) ) ;
#43494 = VERTEX_POINT ( 'NONE', #29350 ) ;
#43495 = CARTESIAN_POINT ( 'NONE',  ( -92.34999999999999432, -208.4700217866474645, 84.73479166840097321 ) ) ;
#43496 = ORIENTED_EDGE ( 'NONE', *, *, #36815, .T. ) ;
#43497 = ADVANCED_FACE ( 'NONE', ( #58308 ), #18446, .T. ) ;
#43498 = DIRECTION ( 'NONE',  ( 0.000000000000000000, 0.000000000000000000, 1.000000000000000000 ) ) ;
#43499 = ORIENTED_EDGE ( 'NONE', *, *, #64536, .T. ) ;
#43500 = CARTESIAN_POINT ( 'NONE',  ( -92.35000000000003695, 90.00000000000004263, 82.14187500173429157 ) ) ;
#43501 = B_SPLINE_CURVE_WITH_KNOTS ( 'NONE', 3,
 ( #43159, #26945, #3312, #60808 ),
 .UNSPECIFIED., .F., .F.,
 ( 4, 4 ),
 ( 2.380735200943099693E-07, 0.002921158011986722466 ),
 .UNSPECIFIED. ) ;
#43502 = ORIENTED_EDGE ( 'NONE', *, *, #51809, .F. ) ;
#43503 = CARTESIAN_POINT ( 'NONE',  ( 92.69370383062498320, 90.00000000000002842, 87.26156250086715715 ) ) ;
#43504 = LINE ( 'NONE', #3649, #69420 ) ;
#43505 = DIRECTION ( 'NONE',  ( -1.000000000000000000, 0.000000000000000000, 0.000000000000000000 ) ) ;
#43506 = CARTESIAN_POINT ( 'NONE',  ( 12.00000000000000000, -4.261787119644963262, 26.19803753235780164 ) ) ;
#43507 = CARTESIAN_POINT ( 'NONE',  ( 5.000000000000002665, -80.55351364060578589, -15.33399622253568673 ) ) ;
#43508 = AXIS2_PLACEMENT_3D ( 'NONE', #40535, #17242, #34158 ) ;
#43509 = DIRECTION ( 'NONE',  ( 0.000000000000000000, -0.4067366430758009854, -0.9135454576426004225 ) ) ;
#43510 = ORIENTED_EDGE ( 'NONE', *, *, #20894, .F. ) ;
#43511 = DIRECTION ( 'NONE',  ( -1.000000000000000000, 0.000000000000000000, 0.000000000000000000 ) ) ;
#43512 = ADVANCED_FACE ( 'NONE', ( #52294 ), #837, .F. ) ;
#43513 = ADVANCED_FACE ( 'NONE', ( #25936 ), #54157, .T. ) ;
#43514 = DIRECTION ( 'NONE',  ( 0.000000000000000000, 0.000000000000000000, 1.000000000000000000 ) ) ;
#43515 = VERTEX_POINT ( 'NONE', #71787 ) ;
#43516 = CIRCLE ( 'NONE', #69873, 31.99999999999999645 ) ;
#43517 = ORIENTED_EDGE ( 'NONE', *, *, #1834, .T. ) ;
#43518 = CARTESIAN_POINT ( 'NONE',  ( 11.99999999999999822, 0.000000000000000000, 0.000000000000000000 ) ) ;
#43519 = AXIS2_PLACEMENT_3D ( 'NONE', #42299, #37401, #59966 ) ;
#43520 = DIRECTION ( 'NONE',  ( -1.000000000000000000, -0.000000000000000000, -0.000000000000000000 ) ) ;
#43521 = CARTESIAN_POINT ( 'NONE',  ( 0.000000000000000000, -77.49459641780886443, 0.8261519478428377417 ) ) ;
#43522 = VECTOR ( 'NONE', #51062, 1000.000000000000000 ) ;
#43523 = CARTESIAN_POINT ( 'NONE',  ( -96.15314808468747287, -208.0026889286704943, 83.98072916753382344 ) ) ;
#43524 = VERTEX_POINT ( 'NONE', #60540 ) ;
#43525 = PLANE ( 'NONE',  #26089 ) ;
#43526 = ORIENTED_EDGE ( 'NONE', *, *, #64244, .F. ) ;
#43527 = DIRECTION ( 'NONE',  ( -1.000000000000000000, -0.000000000000000000, -0.000000000000000000 ) ) ;
#43528 = CIRCLE ( 'NONE', #62749, 23.50000000000000355 ) ;
#43529 = FACE_BOUND ( 'NONE', #16272, .T. ) ;
#43530 = DIRECTION ( 'NONE',  ( 0.000000000000000000, 0.000000000000000000, -1.000000000000000000 ) ) ;
#43531 = CARTESIAN_POINT ( 'NONE',  ( 96.15314808468748708, 91.99731107132950569, 79.27114583420046756 ) ) ;
#43532 = CARTESIAN_POINT ( 'NONE',  ( 0.000000000000000000, 0.000000000000000000, 0.000000000000000000 ) ) ;
#43533 = CARTESIAN_POINT ( 'NONE',  ( 94.99999999999998579, 93.05995642670504253, 86.74562500173429669 ) ) ;
#43534 = CARTESIAN_POINT ( 'NONE',  ( 10.00000000000000000, 3.925862922256769583, -41.81611651403858332 ) ) ;
#43535 = DIRECTION ( 'NONE',  ( -1.000000000000000000, 0.000000000000000000, 0.000000000000000000 ) ) ;
#43536 = CARTESIAN_POINT ( 'NONE',  ( 0.000000000000000000, 80.55351364060589958, 15.33399622253512540 ) ) ;
#43537 = CARTESIAN_POINT ( 'NONE',  ( 92.35000000000000853, -209.9999999999999716, 84.28499999999999659 ) ) ;
#43538 = CARTESIAN_POINT ( 'NONE',  ( 0.000000000000000000, 12.42422080174688404, -35.38097989696498047 ) ) ;
#43539 = CARTESIAN_POINT ( 'NONE',  ( 97.64999999999999147, 90.00000000000002842, 89.04749999999999943 ) ) ;
#43540 = ORIENTED_EDGE ( 'NONE', *, *, #49968, .F. ) ;
#43541 = CARTESIAN_POINT ( 'NONE',  ( -96.15314808468751551, 88.00268892867056536, 84.03364583420047040 ) ) ;
#43542 = CARTESIAN_POINT ( 'NONE',  ( 5.999999999999999112, 74.74816331893430288, 33.71516098798768724 ) ) ;
#43543 = CARTESIAN_POINT ( 'NONE',  ( -3.000000000000000000, -19.89357724624987256, -12.59942793731086041 ) ) ;
#43544 = EDGE_CURVE ( 'NONE', #10016, #8802, #48867, .T. ) ;
#43545 = EDGE_LOOP ( 'NONE', ( #64248, #27996, #44108, #49080 ) ) ;
#43546 =( BOUNDED_CURVE ( )  B_SPLINE_CURVE ( 2, ( #53663, #70938, #2200, #42389, #13793, #36737, #46921, #69835, #3670 ),
 .UNSPECIFIED., .F., .F. ) 
 B_SPLINE_CURVE_WITH_KNOTS ( ( 3, 2, 2, 2, 3 ),
 ( 0.9313609857393202462, 0.9313610513964741822, 0.9384168169373561241, 0.9454725824782379551, 0.9525283480321510288 ),
 .UNSPECIFIED. ) 
 CURVE ( )  GEOMETRIC_REPRESENTATION_ITEM ( )  RATIONAL_B_SPLINE_CURVE ( ( 0.9999975066323323336, 0.9999987533045651134, 1.000000000000000000, 0.8660254037844387076, 1.000000000000000000, 0.8660254037844387076, 1.000000000000000000, 0.8660254037844387076, 1.000000000000000000 ) ) 
 REPRESENTATION_ITEM ( '' )  );
#43547 = CARTESIAN_POINT ( 'NONE',  ( 62.50000000000000000, 0.000000000000000000, -275.0000000000000000 ) ) ;
#43548 = CARTESIAN_POINT ( 'NONE',  ( 0.000000000000000000, 0.000000000000000000, 53.20000000000001705 ) ) ;
#43549 = CARTESIAN_POINT ( 'NONE',  ( 96.66135172262724495, 88.39919842643632819, 74.79754476654878204 ) ) ;
#43550 = EDGE_CURVE ( 'NONE', #21162, #10732, #43046, .T. ) ;
#43551 = PRESENTATION_LAYER_ASSIGNMENT (  '', '', ( #44774 ) ) ;
#43552 = FACE_OUTER_BOUND ( 'NONE', #30063, .T. ) ;
#43553 = CARTESIAN_POINT ( 'NONE',  ( 92.69370383062501162, -211.3315407142195852, 78.42447916753380355 ) ) ;
#43554 = AXIS2_PLACEMENT_3D ( 'NONE', #68635, #51699, #63009 ) ;
#43555 = EDGE_CURVE ( 'NONE', #39400, #15161, #16051, .T. ) ;
#43556 = ORIENTED_EDGE ( 'NONE', *, *, #45943, .F. ) ;
#43557 = EDGE_LOOP ( 'NONE', ( #48693, #48393, #13839, #36450 ) ) ;
#43558 = EDGE_CURVE ( 'NONE', #38750, #61799, #16803, .T. ) ;
#43559 = VECTOR ( 'NONE', #19722, 1000.000000000000000 ) ;
#43560 = CARTESIAN_POINT ( 'NONE',  ( 2.047646702416564768, -96.54137380445985173, -5.500000000000000000 ) ) ;
#43561 = FACE_BOUND ( 'NONE', #59558, .T. ) ;
#43562 = CIRCLE ( 'NONE', #20731, 16.00000000000000000 ) ;
#43563 = DIRECTION ( 'NONE',  ( 0.000000000000000000, -0.8910065241883721177, 0.4539904997395382003 ) ) ;
#43564 = EDGE_CURVE ( 'NONE', #13681, #67162, #71416, .T. ) ;
#43565 = CARTESIAN_POINT ( 'NONE',  ( 93.84685191531249870, -208.0026889286704943, 76.36072916753381890 ) ) ;
#43566 = VERTEX_POINT ( 'NONE', #19916 ) ;
#43567 = DIRECTION ( 'NONE',  ( 0.000000000000000000, -0.4539904997395541320, 0.8910065241883640130 ) ) ;
#43568 = ORIENTED_EDGE ( 'NONE', *, *, #3257, .T. ) ;
#43569 = CIRCLE ( 'NONE', #14727, 3.299999999999983391 ) ;
#43570 = ORIENTED_EDGE ( 'NONE', *, *, #66083, .T. ) ;
#43571 = DIRECTION ( 'NONE',  ( -1.000000000000000000, 0.000000000000000000, -0.000000000000000000 ) ) ;
#43572 = VECTOR ( 'NONE', #69577, 1000.000000000000000 ) ;
#43573 = CARTESIAN_POINT ( 'NONE',  ( 19.12409105625795291, -101.5943176906707919, 5.500000000000000000 ) ) ;
#43574 = ORIENTED_EDGE ( 'NONE', *, *, #20173, .F. ) ;
#43575 = DIRECTION ( 'NONE',  ( 0.000000000000000000, 0.000000000000000000, -1.000000000000000000 ) ) ;
#43576 = CARTESIAN_POINT ( 'NONE',  ( 93.67500000000001137, -212.2949673200287179, 80.02520833506763154 ) ) ;
#43577 = CARTESIAN_POINT ( 'NONE',  ( 92.34999999999999432, 88.47002178664753558, 85.60791666666665378 ) ) ;
#43578 = EDGE_CURVE ( 'NONE', #3442, #24796, #47857, .T. ) ;
#43579 = ORIENTED_EDGE ( 'NONE', *, *, #49703, .F. ) ;
#43580 = CARTESIAN_POINT ( 'NONE',  ( 0.000000000000000000, 74.74816331893430288, 33.71516098798768013 ) ) ;
#43581 = EDGE_CURVE ( 'NONE', #64357, #18753, #37237, .T. ) ;
#43582 = CARTESIAN_POINT ( 'NONE',  ( 92.35000000052950497, 90.00003365185392568, 81.18829462297337329 ) ) ;
#43583 = ORIENTED_EDGE ( 'NONE', *, *, #68418, .T. ) ;
#43584 = DIRECTION ( 'NONE',  ( 0.9038112904824853189, -0.4279312458752977388, 0.000000000000000000 ) ) ;
#43585 = CARTESIAN_POINT ( 'NONE',  ( -93.84685191531252713, 88.00268892867056536, 84.29822916753381890 ) ) ;
#43586 = CARTESIAN_POINT ( 'NONE',  ( 92.69370383062498320, 88.66845928578037217, 82.71072916753379900 ) ) ;
#43587 = ORIENTED_EDGE ( 'NONE', *, *, #21142, .F. ) ;
#43588 = CARTESIAN_POINT ( 'NONE',  ( -4.250000000000000000, -13.95926121303099343, 0.000000000000000000 ) ) ;
#43589 = VERTEX_POINT ( 'NONE', #22065 ) ;
#43590 = CARTESIAN_POINT ( 'NONE',  ( 11.99999999999999822, 0.000000000000000000, 0.000000000000000000 ) ) ;
#43591 = EDGE_LOOP ( 'NONE', ( #6999, #24866, #44645, #37619 ) ) ;
#43592 = ORIENTED_EDGE ( 'NONE', *, *, #14501, .F. ) ;
#43593 = ORIENTED_EDGE ( 'NONE', *, *, #54355, .T. ) ;
#43594 = DIRECTION ( 'NONE',  ( 0.000000000000000000, -0.000000000000000000, -1.000000000000000000 ) ) ;
#43595 = ORIENTED_EDGE ( 'NONE', *, *, #46443, .F. ) ;
#43596 = CARTESIAN_POINT ( 'NONE',  ( 94.99999999999998579, 90.00000000000002842, 90.00000000000000000 ) ) ;
#43597 = APPLICATION_CONTEXT ( 'automotive_design' ) ;
#43598 = CARTESIAN_POINT ( 'NONE',  ( 10.00000000000000000, -3.925862922256464493, 41.81611651403861174 ) ) ;
#43599 = ORIENTED_EDGE ( 'NONE', *, *, #52782, .T. ) ;
#43600 = FACE_OUTER_BOUND ( 'NONE', #64735, .T. ) ;
#43601 = CARTESIAN_POINT ( 'NONE',  ( -92.69370383062498320, -211.3315407142195852, 80.38239583420049428 ) ) ;
#43602 = ORIENTED_EDGE ( 'NONE', *, *, #14750, .F. ) ;
#43603 = CARTESIAN_POINT ( 'NONE',  ( -96.32500000000001705, 87.70503267997129626, 86.29583333333333428 ) ) ;
#43604 = DIRECTION ( 'NONE',  ( -1.000000000000000000, -0.000000000000000000, 0.000000000000000000 ) ) ;
#43605 = PLANE ( 'NONE',  #60927 ) ;
#43606 = CARTESIAN_POINT ( 'NONE',  ( 15.00000000000000000, 14.60985201121729737, 18.46759930825687235 ) ) ;
#43607 = AXIS2_PLACEMENT_3D ( 'NONE', #61035, #5400, #55768 ) ;
#43608 = DIRECTION ( 'NONE',  ( -1.000000000000000000, 0.000000000000000000, 0.000000000000000000 ) ) ;
#43609 = VECTOR ( 'NONE', #62330, 1000.000000000000000 ) ;
#43610 = DIRECTION ( 'NONE',  ( -1.000000000000000000, 1.047380211910311281E-14, 2.618450529775778123E-14 ) ) ;
#43611 = CARTESIAN_POINT ( 'NONE',  ( 94.99999999999998579, 87.33691857156068750, 87.89656250086713385 ) ) ;
#43612 = CARTESIAN_POINT ( 'NONE',  ( 10.00000000000000000, 12.26510123303308752, -35.53030884539072787 ) ) ;
#43613 = CARTESIAN_POINT ( 'NONE',  ( 0.000000000000000000, 40.98264845739763018, -9.188173127306864529 ) ) ;
#43614 = CARTESIAN_POINT ( 'NONE',  ( -97.65000000000001990, 91.52997821335253548, 88.75645833506762017 ) ) ;
#43615 = DIRECTION ( 'NONE',  ( -1.000000000000000000, 0.000000000000000000, 0.000000000000000000 ) ) ;
#43616 = CARTESIAN_POINT ( 'NONE',  ( -13.05994868825747446, -139.5943292883446532, 2.500000000000000000 ) ) ;
#43617 = CARTESIAN_POINT ( 'NONE',  ( -97.65000000000001990, 88.47002178664754979, 87.59229166840096070 ) ) ;
#43618 = CIRCLE ( 'NONE', #9997, 77.49899999999999523 ) ;
#43619 = DIRECTION ( 'NONE',  ( 0.000000000000000000, -0.8526401643540970632, 0.5224985647159409163 ) ) ;
#43620 = CIRCLE ( 'NONE', #7589, 31.99999999999999645 ) ;
#43621 = CARTESIAN_POINT ( 'NONE',  ( 15.00000000000000000, -26.23277895567245466, 4.042438405570107918 ) ) ;
#43622 = ADVANCED_FACE ( 'NONE', ( #45010 ), #59797, .F. ) ;
#43623 = VECTOR ( 'NONE', #56747, 1000.000000000000114 ) ;
#43624 = DIRECTION ( 'NONE',  ( -0.9997280174009349762, 0.02332147558787674504, 0.000000000000000000 ) ) ;
#43625 = DIRECTION ( 'NONE',  ( 0.000000000000000000, 0.000000000000000000, 1.000000000000000000 ) ) ;
#43626 = CYLINDRICAL_SURFACE ( 'NONE', #18424, 2.649999999999985700 ) ;
#43627 = CARTESIAN_POINT ( 'NONE',  ( -93.67499999999998295, -207.7050326799711968, 87.24833333333333485 ) ) ;
#43628 = ADVANCED_FACE ( 'NONE', ( #3045 ), #20297, .F. ) ;
#43629 = ADVANCED_FACE ( 'NONE', ( #43261 ), #54881, .T. ) ;
#43630 = CARTESIAN_POINT ( 'NONE',  ( 11.99999999999999822, 63.18004540533092239, -44.88180994100307686 ) ) ;
#43631 = VERTEX_POINT ( 'NONE', #28065 ) ;
#43632 = DIRECTION ( 'NONE',  ( 0.000000000000000000, 0.000000000000000000, 1.000000000000000000 ) ) ;
#43633 = CARTESIAN_POINT ( 'NONE',  ( 10.00000000000000000, -59.03342792756231461, -46.54456581323868392 ) ) ;
#43634 = DIRECTION ( 'NONE',  ( -1.000000000000000000, 0.000000000000000000, 0.000000000000000000 ) ) ;
#43635 = EDGE_CURVE ( 'NONE', #32074, #24150, #63081, .T. ) ;
#43636 = DIRECTION ( 'NONE',  ( 0.000000000000000000, 0.000000000000000000, 1.000000000000000000 ) ) ;
#43637 = VERTEX_POINT ( 'NONE', #59525 ) ;
#43638 = ORIENTED_EDGE ( 'NONE', *, *, #65170, .T. ) ;
#43639 = DIRECTION ( 'NONE',  ( -1.000000000000000000, 0.000000000000000000, 0.000000000000000000 ) ) ;
#43640 = CYLINDRICAL_SURFACE ( 'NONE', #48766, 32.00000000000000000 ) ;
#43641 = ORIENTED_EDGE ( 'NONE', *, *, #21364, .T. ) ;
#43642 = AXIS2_PLACEMENT_3D ( 'NONE', #51744, #289, #23185 ) ;
#43643 = CARTESIAN_POINT ( 'NONE',  ( 95.00000000000000000, -212.6630814284392557, 80.91156250086714863 ) ) ;
#43644 = CARTESIAN_POINT ( 'NONE',  ( 97.30629616937498838, -211.3315407142195852, 83.71614583420048916 ) ) ;
#43645 = ADVANCED_FACE ( 'NONE', ( #41854 ), #7643, .T. ) ;
#43646 = ORIENTED_EDGE ( 'NONE', *, *, #27041, .T. ) ;
#43647 = CARTESIAN_POINT ( 'NONE',  ( 92.69370383062501162, -211.3315407142195852, 87.31447916753381833 ) ) ;
#43648 = ORIENTED_EDGE ( 'NONE', *, *, #72485, .F. ) ;
#43649 = FACE_OUTER_BOUND ( 'NONE', #25982, .T. ) ;
#43650 = EDGE_LOOP ( 'NONE', ( #52, #57884, #39477, #51597 ) ) ;
#43651 = CARTESIAN_POINT ( 'NONE',  ( -92.69370383062502583, 91.33154071421968467, 76.83697916753382628 ) ) ;
#43652 = AXIS2_PLACEMENT_3D ( 'NONE', #26147, #53615, #71637 ) ;
#43653 = ORIENTED_EDGE ( 'NONE', *, *, #70111, .T. ) ;
#43654 = ORIENTED_EDGE ( 'NONE', *, *, #60061, .F. ) ;
#43655 = PLANE ( 'NONE',  #1676 ) ;
#43656 = ORIENTED_EDGE ( 'NONE', *, *, #61209, .T. ) ;
#43657 = DIRECTION ( 'NONE',  ( 0.000000000000000000, 0.000000000000000000, 1.000000000000000000 ) ) ;
#43658 = CARTESIAN_POINT ( 'NONE',  ( 11.99999999999999822, 62.50329211542494789, -41.76937507738723099 ) ) ;
#43659 = ADVANCED_FACE ( 'NONE', ( #8385 ), #30196, .T. ) ;
#43660 = VERTEX_POINT ( 'NONE', #53875 ) ;
#43661 = DIRECTION ( 'NONE',  ( 1.000000000000000000, 0.000000000000000000, 0.000000000000000000 ) ) ;
#43662 = ADVANCED_FACE ( 'NONE', ( #18909 ), #7279, .T. ) ;
#43663 = AXIS2_PLACEMENT_3D ( 'NONE', #23311, #51876, #34576 ) ;
#43664 = ORIENTED_EDGE ( 'NONE', *, *, #63076, .T. ) ;
#43665 = CARTESIAN_POINT ( 'NONE',  ( 92.35000000052950497, -209.9999663481461027, 81.18829462297289012 ) ) ;
#43666 = EDGE_CURVE ( 'NONE', #73391, #16056, #70783, .T. ) ;
#43667 = AXIS2_PLACEMENT_3D ( 'NONE', #6630, #63790, #47225 ) ;
#43668 = ORIENTED_EDGE ( 'NONE', *, *, #30632, .F. ) ;
#43669 = VERTEX_POINT ( 'NONE', #2043 ) ;
#43670 = CIRCLE ( 'NONE', #59333, 31.99999999999999289 ) ;
#43671 = ORIENTED_EDGE ( 'NONE', *, *, #38136, .F. ) ;
#43672 = CARTESIAN_POINT ( 'NONE',  ( 95.00000000000000000, -212.6630814284392557, 77.73656250086713726 ) ) ;
#43673 = CONTEXT_DEPENDENT_SHAPE_REPRESENTATION ( #35456, #34426 ) ;
#43674 = DIRECTION ( 'NONE',  ( 0.000000000000000000, 0.000000000000000000, -1.000000000000000000 ) ) ;
#43675 = VERTEX_POINT ( 'NONE', #1678 ) ;
#43676 = ORIENTED_EDGE ( 'NONE', *, *, #5722, .F. ) ;
#43677 = VERTEX_POINT ( 'NONE', #25311 ) ;
#43678 = CARTESIAN_POINT ( 'NONE',  ( 0.000000000000000000, 0.000000000000000000, 0.000000000000000000 ) ) ;
#43679 = PLANE ( 'NONE',  #61138 ) ;
#43680 = CARTESIAN_POINT ( 'NONE',  ( -92.69370383062504004, 90.00000000000004263, 78.05406250086716113 ) ) ;
#43681 = ORIENTED_EDGE ( 'NONE', *, *, #70494, .F. ) ;
#43682 = CARTESIAN_POINT ( 'NONE',  ( 96.15314808468748708, 91.99731107132950569, 79.27114583420046756 ) ) ;
#43683 = VERTEX_POINT ( 'NONE', #36576 ) ;
#43684 = FACE_OUTER_BOUND ( 'NONE', #47367, .T. ) ;
#43685 = CARTESIAN_POINT ( 'NONE',  ( -94.99999999999997158, -207.3369185715606307, 89.48406250086713953 ) ) ;
#43686 = CYLINDRICAL_SURFACE ( 'NONE', #62608, 16.00000000000000000 ) ;
#43687 = FACE_OUTER_BOUND ( 'NONE', #25287, .T. ) ;
#43688 = LINE ( 'NONE', #66608, #35694 ) ;
#43689 = CARTESIAN_POINT ( 'NONE',  ( -96.15314808468747287, -208.0026889286704943, 81.28197916753380525 ) ) ;
#43690 = VECTOR ( 'NONE', #74163, 1000.000000000000000 ) ;
#43691 = DIRECTION ( 'NONE',  ( -1.000000000000000000, -0.000000000000000000, 0.000000000000000000 ) ) ;
#43692 = FACE_OUTER_BOUND ( 'NONE', #27854, .T. ) ;
#43693 = DIRECTION ( 'NONE',  ( -1.000000000000000000, 0.000000000000000000, -0.000000000000000000 ) ) ;
#43694 = ORIENTED_EDGE ( 'NONE', *, *, #49460, .T. ) ;
#43695 = ORIENTED_EDGE ( 'NONE', *, *, #3578, .F. ) ;
#43696 = DIRECTION ( 'NONE',  ( 3.035766082959412415E-16, 1.000000000000000000, 0.000000000000000000 ) ) ;
#43697 = FACE_OUTER_BOUND ( 'NONE', #23032, .T. ) ;
#43698 = CARTESIAN_POINT ( 'NONE',  ( 10.00000000000000000, 23.16143007188426850, 73.95703589263983702 ) ) ;
#43699 = CARTESIAN_POINT ( 'NONE',  ( -93.84685191531252713, 88.00268892867056536, 85.40947916753380298 ) ) ;
#43700 = LINE ( 'NONE', #73354, #37055 ) ;
#43701 = CARTESIAN_POINT ( 'NONE',  ( -17.09243336300205129, -103.8724235629982502, -2.500000000000000000 ) ) ;
#43702 = CIRCLE ( 'NONE', #7670, 12.50000000000000000 ) ;
#43703 = ORIENTED_EDGE ( 'NONE', *, *, #15700, .T. ) ;
#43704 = CARTESIAN_POINT ( 'NONE',  ( 10.00000000000000000, 33.17418723428307459, 17.67226234102837878 ) ) ;
#43705 = AXIS2_PLACEMENT_3D ( 'NONE', #50445, #73367, #21876 ) ;
#43706 = EDGE_CURVE ( 'NONE', #39794, #11001, #8011, .T. ) ;
#43707 = CARTESIAN_POINT ( 'NONE',  ( 0.000000000000000000, -120.0000000000000000, -40.00000000000000711 ) ) ;
#43708 = LINE ( 'NONE', #66269, #64605 ) ;
#43709 = AXIS2_PLACEMENT_3D ( 'NONE', #53442, #6837, #30132 ) ;
#43710 = CARTESIAN_POINT ( 'NONE',  ( 10.00000000000000000, 40.65526001592713357, -71.21200624218752750 ) ) ;
#43711 = CARTESIAN_POINT ( 'NONE',  ( 10.00000000000000000, -9.188173127307592836, 40.98264845739746676 ) ) ;
#43712 = CARTESIAN_POINT ( 'NONE',  ( 10.00000000000000000, -32.34446384429951138, -26.79245525562750530 ) ) ;
#43713 = CARTESIAN_POINT ( 'NONE',  ( -93.84685191531248449, -208.0026889286704943, 83.23989583420049598 ) ) ;
#43714 = EDGE_CURVE ( 'NONE', #9521, #7284, #58782, .T. ) ;
#43715 = EDGE_CURVE ( 'NONE', #15962, #73126, #44215, .T. ) ;
#43716 = CARTESIAN_POINT ( 'NONE',  ( -97.64999999999996305, -211.5299782133524218, 86.95729166840096980 ) ) ;
#43717 = CIRCLE ( 'NONE', #55719, 82.00000000000000000 ) ;
#43718 = DIRECTION ( 'NONE',  ( -1.000000000000000000, -0.000000000000000000, -0.000000000000000000 ) ) ;
#43719 = CARTESIAN_POINT ( 'NONE',  ( -0.0004442498505991059293, 0.001194404164628348752, -75.00000000000000000 ) ) ;
#43720 = DIRECTION ( 'NONE',  ( 0.000000000000000000, 0.000000000000000000, 1.000000000000000000 ) ) ;
#43721 = ORIENTED_EDGE ( 'NONE', *, *, #59921, .T. ) ;
#43722 = EDGE_CURVE ( 'NONE', #35508, #48259, #47499, .T. ) ;
#43723 = CARTESIAN_POINT ( 'NONE',  ( 2.047646702416564768, -96.54137380445985173, -5.500000000000000000 ) ) ;
#43724 = DIRECTION ( 'NONE',  ( -1.000000000000000000, 0.000000000000000000, 0.000000000000000000 ) ) ;
#43725 = CARTESIAN_POINT ( 'NONE',  ( 93.67500000000001137, -207.7050326799711968, 79.73416666666666686 ) ) ;
#43726 = VECTOR ( 'NONE', #21588, 1000.000000000000000 ) ;
#43727 = CIRCLE ( 'NONE', #60525, 16.00000000000000355 ) ;
#43728 = CARTESIAN_POINT ( 'NONE',  ( 0.000000000000000000, 8.840884882375075193, 74.65374052328651544 ) ) ;
#43729 = VERTEX_POINT ( 'NONE', #42598 ) ;
#43730 = CARTESIAN_POINT ( 'NONE',  ( 23.49916127795269460, -121.5130826919798039, -5.500000000000000000 ) ) ;
#43731 = DIRECTION ( 'NONE',  ( 1.000000000000000000, -0.000000000000000000, -0.000000000000000000 ) ) ;
#43732 = EDGE_CURVE ( 'NONE', #32439, #23087, #48606, .T. ) ;
#43733 = ORIENTED_EDGE ( 'NONE', *, *, #45406, .F. ) ;
#43734 = CARTESIAN_POINT ( 'NONE',  ( 92.35000000000000853, -209.9999999999999716, 75.39499999999999602 ) ) ;
#43735 = DIRECTION ( 'NONE',  ( 0.000000000000000000, 0.000000000000000000, 1.000000000000000000 ) ) ;
#43736 = EDGE_CURVE ( 'NONE', #278, #4935, #50261, .T. ) ;
#43737 = ORIENTED_EDGE ( 'NONE', *, *, #43997, .T. ) ;
#43738 = PLANE ( 'NONE',  #66669 ) ;
#43739 = VERTEX_POINT ( 'NONE', #64425 ) ;
#43740 = DIRECTION ( 'NONE',  ( -1.000000000000000000, 0.000000000000000000, -0.000000000000000000 ) ) ;
#43741 = ORIENTED_EDGE ( 'NONE', *, *, #27863, .F. ) ;
#43742 = VERTEX_POINT ( 'NONE', #2784 ) ;
#43743 = ORIENTED_EDGE ( 'NONE', *, *, #47945, .T. ) ;
#43744 = EDGE_LOOP ( 'NONE', ( #50487, #3294, #36595 ) ) ;
#43745 = CARTESIAN_POINT ( 'NONE',  ( 11.99999999999999822, -75.11764819372149304, 2.946379043146075905 ) ) ;
#43746 = EDGE_CURVE ( 'NONE', #32002, #1736, #45517, .T. ) ;
#43747 = VERTEX_POINT ( 'NONE', #35834 ) ;
#43748 = EDGE_CURVE ( 'NONE', #3791, #50602, #71888, .T. ) ;
#43749 = AXIS2_PLACEMENT_3D ( 'NONE', #39722, #51351, #22045 ) ;
#43750 = ORIENTED_EDGE ( 'NONE', *, *, #55019, .F. ) ;
#43751 =( BOUNDED_CURVE ( )  B_SPLINE_CURVE ( 2, ( #4820, #10054, #23201, #40118, #39756, #62707, #39378 ),
 .UNSPECIFIED., .F., .F. ) 
 B_SPLINE_CURVE_WITH_KNOTS ( ( 3, 2, 2, 3 ),
 ( 0.2328402629019980796, 0.2398960283900005708, 0.2469517939308829568, 0.2540073681283129825 ),
 .UNSPECIFIED. ) 
 CURVE ( )  GEOMETRIC_REPRESENTATION_ITEM ( )  RATIONAL_B_SPLINE_CURVE ( ( 1.000000000000000000, 0.8660254037844387076, 1.000000000000000000, 0.8660254037844387076, 1.000000000000000000, 0.8660290370063220555, 0.9999927337532901195 ) ) 
 REPRESENTATION_ITEM ( '' )  );
#43752 = CARTESIAN_POINT ( 'NONE',  ( 93.84685191531248449, 91.99731107132950569, 75.09072916753380866 ) ) ;
#43753 = DIRECTION ( 'NONE',  ( -1.000000000000000000, 0.000000000000000000, -0.000000000000000000 ) ) ;
#43754 = CARTESIAN_POINT ( 'NONE',  ( -97.65000000000006253, 88.47002178664754979, 84.97291666666667709 ) ) ;
#43755 = ORIENTED_EDGE ( 'NONE', *, *, #71390, .F. ) ;
#43756 = ORIENTED_EDGE ( 'NONE', *, *, #4341, .T. ) ;
#43757 = EDGE_LOOP ( 'NONE', ( #57014, #4440, #57348, #18750 ) ) ;
#43758 = CARTESIAN_POINT ( 'NONE',  ( 92.69370383062498320, 91.33154071421968467, 88.95489583420048518 ) ) ;
#43759 = ORIENTED_EDGE ( 'NONE', *, *, #49828, .T. ) ;
#43760 = CARTESIAN_POINT ( 'NONE',  ( 97.30629616937498838, -208.6684592857803011, 88.10822916753380696 ) ) ;
#43761 = DIRECTION ( 'NONE',  ( 1.000000000000000000, 0.000000000000000000, -5.551115123125782702E-17 ) ) ;
#43762 = LINE ( 'NONE', #33946, #1836 ) ;
#43763 = CARTESIAN_POINT ( 'NONE',  ( 0.000000000000000000, -16.65972982744876774, -80.28980883073775487 ) ) ;
#43764 = CARTESIAN_POINT ( 'NONE',  ( 5.000000000000000000, 15.48615015657637706, -39.04073710021327770 ) ) ;
#43765 = DIRECTION ( 'NONE',  ( -1.000000000000000000, 0.000000000000000000, 0.000000000000000000 ) ) ;
#43766 = DIRECTION ( 'NONE',  ( 1.000000000000000000, 0.000000000000000000, 0.000000000000000000 ) ) ;
#43767 = DIRECTION ( 'NONE',  ( -1.000000000000000000, 0.000000000000000000, 0.000000000000000000 ) ) ;
#43768 = CARTESIAN_POINT ( 'NONE',  ( -97.64999999999996305, -209.9999999999999716, 76.74437500173429783 ) ) ;
#43769 = CARTESIAN_POINT ( 'NONE',  ( -96.15314808468752972, 91.99731107132950569, 89.06072916753382174 ) ) ;
#43770 = ORIENTED_EDGE ( 'NONE', *, *, #33272, .T. ) ;
#43771 = UNCERTAINTY_MEASURE_WITH_UNIT (LENGTH_MEASURE( 1.000000000000000082E-05 ), #4204, 'distance_accuracy_value', 'NONE');
#43773 = CARTESIAN_POINT ( 'NONE',  ( -92.69370383062502583, 88.66845928578038638, 86.73239583420047438 ) ) ;
#43772 = CARTESIAN_POINT ( 'NONE',  ( 93.84685191531248449, 88.00268892867053694, 87.84364583420047268 ) ) ;
#43774 = AXIS2_PLACEMENT_3D ( 'NONE', #47622, #69441, #19413 ) ;
#43775 = ORIENTED_EDGE ( 'NONE', *, *, #66241, .F. ) ;
#43776 = CARTESIAN_POINT ( 'NONE',  ( 15.00000000000000000, -18.13022148937242761, 15.02647892043569122 ) ) ;
#43777 = VECTOR ( 'NONE', #38064, 1000.000000000000000 ) ;
#43778 = CARTESIAN_POINT ( 'NONE',  ( 19.29194287201271862, -133.5026271600380880, -5.500000000000000000 ) ) ;
#43779 = DIRECTION ( 'NONE',  ( -0.000000000000000000, -0.000000000000000000, -1.000000000000000000 ) ) ;
#43780 = CARTESIAN_POINT ( 'NONE',  ( 97.65000000000000568, 91.52997821335252127, 82.19479166840095274 ) ) ;
#43781 = DIRECTION ( 'NONE',  ( 0.000000000000000000, -0.8090169943749403458, -0.5877852522924830181 ) ) ;
#43782 = FACE_OUTER_BOUND ( 'NONE', #10547, .T. ) ;
#43784 = LINE ( 'NONE', #61811, #24195 ) ;
#43783 = AXIS2_PLACEMENT_3D ( 'NONE', #58398, #63316, #58778 ) ;
#43785 = CIRCLE ( 'NONE', #49764, 31.99999999999999289 ) ;
#43786 = DIRECTION ( 'NONE',  ( 0.000000000000000000, 0.000000000000000000, -1.000000000000000000 ) ) ;
#43787 = ORIENTED_EDGE ( 'NONE', *, *, #69841, .T. ) ;
#43788 = ORIENTED_EDGE ( 'NONE', *, *, #52262, .T. ) ;
#43789 = CIRCLE ( 'NONE', #11340, 35.50000000000000711 ) ;
#43790 = CARTESIAN_POINT ( 'NONE',  ( -96.32500000000001705, 87.70503267997129626, 79.94583333333332575 ) ) ;
#43791 = DIRECTION ( 'NONE',  ( 1.000000000000000000, -0.000000000000000000, -0.000000000000000000 ) ) ;
#43792 = CARTESIAN_POINT ( 'NONE',  ( 10.00000000000000000, 0.000000000000000000, 0.000000000000000000 ) ) ;
#43793 = CARTESIAN_POINT ( 'NONE',  ( 10.00000000000000000, -34.44570377933649041, 69.42325613327427902 ) ) ;
#43794 = AXIS2_PLACEMENT_3D ( 'NONE', #53338, #58240, #63897 ) ;
#43795 = DIRECTION ( 'NONE',  ( -2.603472992746261562E-14, -2.546204323184492723E-14, 1.000000000000000000 ) ) ;
#43796 = CARTESIAN_POINT ( 'NONE',  ( 0.000000000000000000, 0.000000000000000000, 0.000000000000000000 ) ) ;
#43797 = CARTESIAN_POINT ( 'NONE',  ( -92.69370383062498320, -211.3315407142195852, 75.46114583420049371 ) ) ;
#43798 = ORIENTED_EDGE ( 'NONE', *, *, #56477, .T. ) ;
#43799 = CARTESIAN_POINT ( 'NONE',  ( -97.30629616937501680, 91.33154071421968467, 81.96989583420048575 ) ) ;
#43800 = CIRCLE ( 'NONE', #72573, 31.99999999999998579 ) ;
#43801 = EDGE_CURVE ( 'NONE', #23851, #68126, #29867, .T. ) ;
#43802 = FACE_OUTER_BOUND ( 'NONE', #72345, .T. ) ;
#43803 = DIRECTION ( 'NONE',  ( 1.000000000000000000, -0.000000000000000000, 0.000000000000000000 ) ) ;
#43804 = EDGE_CURVE ( 'NONE', #60565, #22189, #4239, .T. ) ;
#43805 =( NAMED_UNIT ( * ) PLANE_ANGLE_UNIT ( ) SI_UNIT ( $, .RADIAN. ) );
#43806 = DIRECTION ( 'NONE',  ( 0.000000000000000000, -0.2334453638558921240, -0.9723699203976797767 ) ) ;
#43807 = CARTESIAN_POINT ( 'NONE',  ( -3.000000000000000000, -13.04903810567647682, -19.60159698893442481 ) ) ;
#43808 = CARTESIAN_POINT ( 'NONE',  ( -97.64999999999996305, -208.4700217866474645, 87.40708333333333258 ) ) ;
#43809 = CARTESIAN_POINT ( 'NONE',  ( 11.99999999999999822, -27.74655509720618696, -77.16300072079690153 ) ) ;
#43810 = EDGE_CURVE ( 'NONE', #15441, #22641, #26270, .T. ) ;
#43811 = CARTESIAN_POINT ( 'NONE',  ( 100.0000000000260201, 95.00000000000001421, 74.99999999999998579 ) ) ;
#43812 = CARTESIAN_POINT ( 'NONE',  ( 97.30629616937498838, 91.33154071421968467, 81.91697916753383879 ) ) ;
#43813 = CARTESIAN_POINT ( 'NONE',  ( -93.84685191531248449, -208.0026889286704943, 82.60489583420049087 ) ) ;
#43814 = DIRECTION ( 'NONE',  ( 0.000000000000000000, -0.1045284632676429099, -0.9945218953682744001 ) ) ;
#43815 = ORIENTED_EDGE ( 'NONE', *, *, #54519, .T. ) ;
#43816 = ADVANCED_FACE ( 'NONE', ( #14753 ), #66994, .T. ) ;
#43817 = CARTESIAN_POINT ( 'NONE',  ( 0.000000000000000000, -63.97538442413463855, 51.29473840253199768 ) ) ;
#43818 = CARTESIAN_POINT ( 'NONE',  ( -94.99999999999997158, -206.9400435732949575, 77.14124999999999943 ) ) ;
#43819 = CARTESIAN_POINT ( 'NONE',  ( 95.00000000000000000, -209.9999999999999716, 90.00000000000000000 ) ) ;
#43820 = AXIS2_PLACEMENT_3D ( 'NONE', #68258, #61505, #16374 ) ;
#43821 = CARTESIAN_POINT ( 'NONE',  ( -97.30629616937501680, 88.66845928578038638, 77.15447916753382174 ) ) ;
#43822 = CARTESIAN_POINT ( 'NONE',  ( 97.30629616937498838, -208.6684592857803011, 83.02822916753379445 ) ) ;
#43823 = ORIENTED_EDGE ( 'NONE', *, *, #66718, .F. ) ;
#43824 = DIRECTION ( 'NONE',  ( 0.08130631524010117905, -0.9966891607226784355, 0.000000000000000000 ) ) ;
#43825 = EDGE_CURVE ( 'NONE', #68714, #13386, #15122, .T. ) ;
#43826 = VERTEX_POINT ( 'NONE', #21878 ) ;
#43827 = CARTESIAN_POINT ( 'NONE',  ( 5.000000000000000000, -31.52238457039619490, 27.75498641678731104 ) ) ;
#43828 = EDGE_CURVE ( 'NONE', #14697, #1375, #20405, .T. ) ;
#43829 = AXIS2_PLACEMENT_3D ( 'NONE', #55394, #3915, #26814 ) ;
#43830 = ORIENTED_EDGE ( 'NONE', *, *, #7118, .F. ) ;
#43831 = CARTESIAN_POINT ( 'NONE',  ( 0.000000000000000000, -81.90746397400393164, 3.894527615417586741 ) ) ;
#43832 = EDGE_CURVE ( 'NONE', #68149, #41131, #46677, .T. ) ;
#43833 = EDGE_CURVE ( 'NONE', #28422, #10181, #56095, .T. ) ;
#43834 = CARTESIAN_POINT ( 'NONE',  ( 97.30629616937498838, -209.9999999999999716, 76.78406250086715090 ) ) ;
#43835 = CARTESIAN_POINT ( 'NONE',  ( 1.474095553543393056, -119.7224350544041869, -2.500000000000000000 ) ) ;
#43836 = ADVANCED_FACE ( 'NONE', ( #44453 ), #49694, .T. ) ;
#43837 = DIRECTION ( 'NONE',  ( -1.000000000000000000, -0.000000000000000000, -0.000000000000000000 ) ) ;
#43838 = DIRECTION ( 'NONE',  ( -1.000000000000000000, -0.000000000000000000, -0.000000000000000000 ) ) ;
#43839 = CARTESIAN_POINT ( 'NONE',  ( 93.84685191531248449, 88.00268892867053694, 86.09739583420049769 ) ) ;
#43840 = CARTESIAN_POINT ( 'NONE',  ( -97.64999999953499810, 89.99996900126896548, 83.09538598081491045 ) ) ;
#43841 = CARTESIAN_POINT ( 'NONE',  ( 95.00000000000000000, -213.0599564267049857, 81.90374999999998806 ) ) ;
#43842 = EDGE_LOOP ( 'NONE', ( #50097, #16739, #44142, #31181 ) ) ;
#43843 = EDGE_CURVE ( 'NONE', #25675, #67853, #51505, .T. ) ;
#43844 = VERTEX_POINT ( 'NONE', #15496 ) ;
#43845 = EDGE_LOOP ( 'NONE', ( #10175, #42275, #63643, #9313 ) ) ;
#43846 = ORIENTED_EDGE ( 'NONE', *, *, #1774, .F. ) ;
#43847 = CARTESIAN_POINT ( 'NONE',  ( -7.399999999999985256, 2.363091343437615473E-13, 22.90000000000041069 ) ) ;
#43848 = CARTESIAN_POINT ( 'NONE',  ( -92.69370383062502583, 88.66845928578038638, 83.08114583420048405 ) ) ;
#43849 = AXIS2_PLACEMENT_3D ( 'NONE', #71598, #12975, #54330 ) ;
#43850 = CARTESIAN_POINT ( 'NONE',  ( -97.64999999999992042, -208.4700217866474929, 77.24708333333332178 ) ) ;
#43851 = DIRECTION ( 'NONE',  ( 0.000000000000000000, 0.000000000000000000, 1.000000000000000000 ) ) ;
#43852 = CARTESIAN_POINT ( 'NONE',  ( 11.99999999999999822, -51.02545421589363883, 55.20638768913742922 ) ) ;
#43853 = CARTESIAN_POINT ( 'NONE',  ( -94.99999999999997158, -213.0599564267049857, 83.88812500173429498 ) ) ;
#43854 = ORIENTED_EDGE ( 'NONE', *, *, #2229, .F. ) ;
#43855 = CARTESIAN_POINT ( 'NONE',  ( -92.34999999999999432, -211.5299782133524502, 87.16895833506762870 ) ) ;
#43856 = VERTEX_POINT ( 'NONE', #10224 ) ;
#43857 = DIRECTION ( 'NONE',  ( 0.7585478161175723821, 0.6516173805718057377, -0.000000000000000000 ) ) ;
#43858 = ORIENTED_EDGE ( 'NONE', *, *, #49580, .T. ) ;
#43859 = CARTESIAN_POINT ( 'NONE',  ( -97.65000000000001990, 91.52997821335253548, 83.04145833506763097 ) ) ;
#43860 = ORIENTED_EDGE ( 'NONE', *, *, #62822, .F. ) ;
#43861 = CARTESIAN_POINT ( 'NONE',  ( 93.84685191531248449, 88.00268892867053694, 86.73239583420048859 ) ) ;
#43862 = DIRECTION ( 'NONE',  ( -0.000000000000000000, -0.000000000000000000, -1.000000000000000000 ) ) ;
#43863 = CARTESIAN_POINT ( 'NONE',  ( 15.00000000000000000, -11.95096189432345746, -23.69967320028757030 ) ) ;
#43864 = CARTESIAN_POINT ( 'NONE',  ( 5.000000000000000000, 60.67117009219216328, -55.16347631942977614 ) ) ;
#43865 = DIRECTION ( 'NONE',  ( -1.000000000000000000, 0.000000000000000000, -0.000000000000000000 ) ) ;
#43866 = DIRECTION ( 'NONE',  ( 1.000000000000000000, 0.000000000000000000, 0.000000000000000000 ) ) ;
#43867 = ORIENTED_EDGE ( 'NONE', *, *, #28203, .F. ) ;
#43868 = CARTESIAN_POINT ( 'NONE',  ( 92.35000000000009379, -208.4700217866474361, 77.88208333333332689 ) ) ;
#43869 = LINE ( 'NONE', #26926, #32324 ) ;
#43870 = AXIS2_PLACEMENT_3D ( 'NONE', #70828, #42286, #14433 ) ;
#43871 = ORIENTED_EDGE ( 'NONE', *, *, #25041, .F. ) ;
#43872 = ORIENTED_EDGE ( 'NONE', *, *, #67206, .F. ) ;
#43873 = CARTESIAN_POINT ( 'NONE',  ( 10.00000000000000000, -5.256550761633413060, 77.32052557432841411 ) ) ;
#43874 = CARTESIAN_POINT ( 'NONE',  ( 10.00000000000000000, -75.11764819372149304, 2.946379043146075905 ) ) ;
#43875 = LINE ( 'NONE', #14167, #16097 ) ;
#43876 = CARTESIAN_POINT ( 'NONE',  ( -94.99999999999997158, -212.6630814284392557, 85.51531250086713953 ) ) ;
#43877 = ORIENTED_EDGE ( 'NONE', *, *, #12745, .F. ) ;
#43878 = VECTOR ( 'NONE', #46096, 1000.000000000000000 ) ;
#43879 = DIRECTION ( 'NONE',  ( 1.000000000000000000, 0.000000000000000000, 0.000000000000000000 ) ) ;
#43880 = AXIS2_PLACEMENT_3D ( 'NONE', #27459, #15072, #38011 ) ;
#43881 = ORIENTED_EDGE ( 'NONE', *, *, #34360, .T. ) ;
#43882 = EDGE_CURVE ( 'NONE', #5740, #65693, #33458, .T. ) ;
#43883 = DIRECTION ( 'NONE',  ( 0.000000000000000000, 0.000000000000000000, 1.000000000000000000 ) ) ;
#43884 = VECTOR ( 'NONE', #49161, 1000.000000000000000 ) ;
#43885 = CARTESIAN_POINT ( 'NONE',  ( -31.74999999999995737, 6.123233995736766282E-16, -5.000000000000000000 ) ) ;
#43886 = EDGE_CURVE ( 'NONE', #24664, #3543, #35880, .T. ) ;
#43887 = DIRECTION ( 'NONE',  ( -1.000000000000000000, -0.000000000000000000, 0.000000000000000000 ) ) ;
#43888 = CARTESIAN_POINT ( 'NONE',  ( 93.84685191531248449, 88.00268892867053694, 78.31864583420048120 ) ) ;
#43889 = PLANE ( 'NONE',  #71270 ) ;
#43890 = DIRECTION ( 'NONE',  ( -1.000000000000000000, -0.000000000000000000, 0.000000000000000000 ) ) ;
#43891 = AXIS2_PLACEMENT_3D ( 'NONE', #46842, #69759, #28800 ) ;
#43892 = CARTESIAN_POINT ( 'NONE',  ( 0.000000000000000000, 71.21200624218795383, 40.65526001592638039 ) ) ;
#43893 = CARTESIAN_POINT ( 'NONE',  ( 0.000000000000000000, 37.58145647212453611, 16.68533520207917675 ) ) ;
#43894 = EDGE_CURVE ( 'NONE', #6380, #70995, #11832, .T. ) ;
#43896 = EDGE_CURVE ( 'NONE', #40236, #10267, #50447, .T. ) ;
#43895 = DIRECTION ( 'NONE',  ( -1.000000000000000000, -0.000000000000000000, 0.000000000000000000 ) ) ;
#43897 = CARTESIAN_POINT ( 'NONE',  ( -97.64999999999989200, -211.5299782133524218, 86.87791666666664980 ) ) ;
#43898 = CARTESIAN_POINT ( 'NONE',  ( -92.74366017909918014, -209.4495095149826511, 74.79348190356849102 ) ) ;
#43899 = AXIS2_PLACEMENT_3D ( 'NONE', #5046, #68562, #67809 ) ;
#43900 = DIRECTION ( 'NONE',  ( -1.000000000000000000, 0.000000000000000000, -0.000000000000000000 ) ) ;
#43901 = EDGE_LOOP ( 'NONE', ( #25691, #51118, #13569, #14700 ) ) ;
#43902 = CARTESIAN_POINT ( 'NONE',  ( -95.00000000000002842, 87.33691857156074434, 81.54656250086713953 ) ) ;
#43903 = DIRECTION ( 'NONE',  ( -1.000000000000000000, 0.000000000000000000, 0.000000000000000000 ) ) ;
#43904 = AXIS2_PLACEMENT_3D ( 'NONE', #54989, #26047, #43371 ) ;
#43905 = ADVANCED_FACE ( 'NONE', ( #44824 ), #67749, .T. ) ;
#43906 = EDGE_CURVE ( 'NONE', #73517, #30173, #15431, .T. ) ;
#43907 = CARTESIAN_POINT ( 'NONE',  ( 6.377742925735834234, -145.7647898336708181, 5.500000000000000000 ) ) ;
#43908 = ORIENTED_EDGE ( 'NONE', *, *, #5539, .T. ) ;
#43909 = FACE_OUTER_BOUND ( 'NONE', #3246, .T. ) ;
#43910 = FACE_OUTER_BOUND ( 'NONE', #62658, .T. ) ;
#43911 = FACE_OUTER_BOUND ( 'NONE', #35503, .T. ) ;
#43912 = FACE_OUTER_BOUND ( 'NONE', #34009, .T. ) ;
#43913 = ADVANCED_FACE ( 'NONE', ( #48960 ), #9858, .T. ) ;
#43914 = ADVANCED_FACE ( 'NONE', ( #22629 ), #12081, .F. ) ;
#43915 = CARTESIAN_POINT ( 'NONE',  ( 96.15314808468750130, -211.9973110713294489, 77.31322916753381946 ) ) ;
#43916 = VERTEX_POINT ( 'NONE', #4984 ) ;
#43917 = EDGE_LOOP ( 'NONE', ( #36791, #30566, #10540, #5197 ) ) ;
#43918 = CARTESIAN_POINT ( 'NONE',  ( 11.99999999999999822, 0.000000000000000000, 0.000000000000000000 ) ) ;
#43919 = DIRECTION ( 'NONE',  ( 1.000000000000000000, 0.000000000000000000, -0.000000000000000000 ) ) ;
#43920 = CARTESIAN_POINT ( 'NONE',  ( 0.000000000000000000, 25.88420570971400991, 27.13269053701105449 ) ) ;
#43921 = CARTESIAN_POINT ( 'NONE',  ( 5.999999999999999112, -50.23322058963299241, -64.81221759200397514 ) ) ;
#43922 = AXIS2_PLACEMENT_3D ( 'NONE', #49400, #32098, #47922 ) ;
#43923 = SURFACE_STYLE_FILL_AREA ( #20609 ) ;
#43924 = CARTESIAN_POINT ( 'NONE',  ( 92.69370383062501162, -209.9999999999999716, 77.73656250086715147 ) ) ;
#43925 = ORIENTED_EDGE ( 'NONE', *, *, #6117, .F. ) ;
#43926 = DIRECTION ( 'NONE',  ( -1.000000000000000000, 0.000000000000000000, -0.000000000000000000 ) ) ;
#43927 = ORIENTED_EDGE ( 'NONE', *, *, #72158, .T. ) ;
#43928 = CIRCLE ( 'NONE', #37910, 82.00000000000000000 ) ;
#43929 = ORIENTED_EDGE ( 'NONE', *, *, #49891, .T. ) ;
#43930 = FACE_OUTER_BOUND ( 'NONE', #65744, .T. ) ;
#43931 = AXIS2_PLACEMENT_3D ( 'NONE', #68508, #35025, #6816 ) ;
#43932 = CARTESIAN_POINT ( 'NONE',  ( 10.00000000000000000, 2.543863470248371783, 81.96053171279901051 ) ) ;
#43933 = AXIS2_PLACEMENT_3D ( 'NONE', #46755, #195, #17437 ) ;
#43934 = ORIENTED_EDGE ( 'NONE', *, *, #7805, .F. ) ;
#43935 = DIRECTION ( 'NONE',  ( 1.000000000000000000, -0.000000000000000000, -0.000000000000000000 ) ) ;
#43936 = CARTESIAN_POINT ( 'NONE',  ( 96.32499999999998863, -212.2949673200287179, 80.13104166840095388 ) ) ;
#43937 = CARTESIAN_POINT ( 'NONE',  ( 97.64999999999997726, 88.47002178664753558, 84.54958333333333087 ) ) ;
#43938 = EDGE_LOOP ( 'NONE', ( #74239, #31254, #67373, #64280 ) ) ;
#43939 = DIRECTION ( 'NONE',  ( 0.000000000000000000, -0.9510565162951502005, -0.3090169943749581094 ) ) ;
#43940 = DIRECTION ( 'NONE',  ( 1.000000000000000000, -0.000000000000000000, 0.000000000000000000 ) ) ;
#43941 = AXIS2_PLACEMENT_3D ( 'NONE', #46372, #40734, #36192 ) ;
#43942 = ORIENTED_EDGE ( 'NONE', *, *, #34961, .T. ) ;
#43943 = VECTOR ( 'NONE', #66611, 1000.000000000000000 ) ;
#43944 = CARTESIAN_POINT ( 'NONE',  ( 92.34999999999999432, 91.52997821335252127, 84.31145833506762699 ) ) ;
#43945 = CARTESIAN_POINT ( 'NONE',  ( -96.15314808468751551, 88.00268892867056536, 84.82739583420048746 ) ) ;
#43946 = CARTESIAN_POINT ( 'NONE',  ( 94.99999999999998579, 87.33691857156068750, 81.54656250086715374 ) ) ;
#43947 = ORIENTED_EDGE ( 'NONE', *, *, #51254, .T. ) ;
#43948 = CYLINDRICAL_SURFACE ( 'NONE', #27653, 2.649999999999985700 ) ;
#43949 = ORIENTED_EDGE ( 'NONE', *, *, #45332, .F. ) ;
#43950 = DIRECTION ( 'NONE',  ( -0.9997280174009349762, 0.02332147558787823691, 0.000000000000000000 ) ) ;
#43951 = VERTEX_POINT ( 'NONE', #847 ) ;
#43952 = ORIENTED_EDGE ( 'NONE', *, *, #50818, .T. ) ;
#43953 = CARTESIAN_POINT ( 'NONE',  ( 94.99999999999998579, 86.94004357329502852, 79.99874999999998693 ) ) ;
#43954 = EDGE_LOOP ( 'NONE', ( #30032, #4333, #67034, #34906 ) ) ;
#43955 = DIRECTION ( 'NONE',  ( 0.000000000000000000, 0.000000000000000000, 1.000000000000000000 ) ) ;
#43956 =( BOUNDED_CURVE ( )  B_SPLINE_CURVE ( 2, ( #29990, #52187, #735, #52935, #6702, #63135, #18708, #36004, #17247 ),
 .UNSPECIFIED., .F., .F. ) 
 B_SPLINE_CURVE_WITH_KNOTS ( ( 3, 2, 2, 2, 3 ),
 ( 0.3810111478265171270, 0.3810113392076479588, 0.3880671047485307334, 0.3951228702894135636, 0.4021785743327777052 ),
 .UNSPECIFIED. ) 
 CURVE ( )  GEOMETRIC_REPRESENTATION_ITEM ( )  RATIONAL_B_SPLINE_CURVE ( ( 0.9999927323224930831, 0.9999963660626793871, 1.000000000000000000, 0.8660254037844387076, 1.000000000000000000, 0.8660254037844387076, 1.000000000000000000, 0.8660265714968831130, 0.9999976645954666843 ) ) 
 REPRESENTATION_ITEM ( '' )  );
#43957 = CARTESIAN_POINT ( 'NONE',  ( 11.99999999999999822, 68.27212725128275395, 31.46837873495001503 ) ) ;
#43958 = EDGE_LOOP ( 'NONE', ( #6419, #25968, #36703, #37305 ) ) ;
#43959 = DIRECTION ( 'NONE',  ( -0.000000000000000000, -0.000000000000000000, 1.000000000000000000 ) ) ;
#43960 = CARTESIAN_POINT ( 'NONE',  ( -92.69370383062498320, -209.9999999999999716, 77.89531250086714920 ) ) ;
#43961 = ORIENTED_EDGE ( 'NONE', *, *, #49968, .T. ) ;
#43962 = CARTESIAN_POINT ( 'NONE',  ( 12.00000000000000000, 20.85821328998756385, 10.92862929874494249 ) ) ;
#43963 = PLANE ( 'NONE',  #18833 ) ;
#43964 = LINE ( 'NONE', #3028, #16545 ) ;
#43965 = CARTESIAN_POINT ( 'NONE',  ( -92.34999999999999432, -209.9999999999999716, 89.12687500173430521 ) ) ;
#43966 = ADVANCED_FACE ( 'NONE', ( #10978 ), #68499, .T. ) ;
#43967 = DIRECTION ( 'NONE',  ( 0.000000000000000000, 0.4539904997395414754, 0.8910065241883706744 ) ) ;
#43968 = EDGE_CURVE ( 'NONE', #68824, #13504, #28698, .T. ) ;
#43969 = DIRECTION ( 'NONE',  ( -1.000000000000000000, -0.000000000000000000, -0.000000000000000000 ) ) ;
#43970 = CARTESIAN_POINT ( 'NONE',  ( 94.99999999999998579, 87.33691857156068750, 86.62656250086713783 ) ) ;
#43971 = DIRECTION ( 'NONE',  ( 0.000000000000000000, 0.000000000000000000, 1.000000000000000000 ) ) ;
#43972 = DIRECTION ( 'NONE',  ( -0.000000000000000000, -0.000000000000000000, -1.000000000000000000 ) ) ;
#43973 = DIRECTION ( 'NONE',  ( 0.000000000000000000, 0.000000000000000000, 1.000000000000000000 ) ) ;
#43975 = EDGE_CURVE ( 'NONE', #45509, #60565, #70694, .T. ) ;
#43974 = DIRECTION ( 'NONE',  ( -1.000000000000000000, 0.000000000000000000, -0.000000000000000000 ) ) ;
#43976 = DIRECTION ( 'NONE',  ( -1.000000000000000000, -0.000000000000000000, 0.000000000000000000 ) ) ;
#43977 = DIRECTION ( 'NONE',  ( -1.000000000000000000, 0.000000000000000000, 0.000000000000000000 ) ) ;
#43978 = DIRECTION ( 'NONE',  ( -1.000000000000000000, 0.000000000000000000, 0.000000000000000000 ) ) ;
#43979 = ADVANCED_FACE ( 'NONE', ( #63608 ), #17717, .T. ) ;
#43980 = CIRCLE ( 'NONE', #18731, 31.99999999999998934 ) ;
#43981 = CYLINDRICAL_SURFACE ( 'NONE', #50838, 2.649999999999985700 ) ;
#43982 = DIRECTION ( 'NONE',  ( -0.000000000000000000, -0.000000000000000000, 1.000000000000000000 ) ) ;
#43983 = CARTESIAN_POINT ( 'NONE',  ( 97.64999999999999147, 90.00000000000002842, 80.79249999999998977 ) ) ;
#43984 = CIRCLE ( 'NONE', #17569, 82.00000000000000000 ) ;
#43985 = CARTESIAN_POINT ( 'NONE',  ( -94.99999999999997158, -213.0599564267049857, 85.07874999999999943 ) ) ;
#43986 = AXIS2_PLACEMENT_3D ( 'NONE', #54746, #60768, #26906 ) ;
#43987 = ADVANCED_FACE ( 'NONE', ( #23010 ), #46666, .F. ) ;
#43988 = DIRECTION ( 'NONE',  ( 0.000000000000000000, -0.07845909572785221553, 0.9969173337331274087 ) ) ;
#43989 = EDGE_CURVE ( 'NONE', #60745, #55710, #56293, .T. ) ;
#43990 = PRODUCT_DEFINITION_SHAPE ( 'NONE', 'NONE',  #74341 ) ;
#43991 = AXIS2_PLACEMENT_3D ( 'NONE', #72964, #22986, #68845 ) ;
#43992 = CARTESIAN_POINT ( 'NONE',  ( -6.880223345695647197, -142.5202692415819854, 5.500000000000000000 ) ) ;
#43993 = DIRECTION ( 'NONE',  ( 0.000000000000000000, -0.000000000000000000, -1.000000000000000000 ) ) ;
#43994 = CARTESIAN_POINT ( 'NONE',  ( 10.00000000000000000, 0.000000000000000000, 0.000000000000000000 ) ) ;
#43995 = DIRECTION ( 'NONE',  ( 1.000000000000000000, 0.000000000000000000, -0.000000000000000000 ) ) ;
#43996 = ADVANCED_FACE ( 'NONE', ( #69600 ), #62111, .F. ) ;
#43997 = EDGE_CURVE ( 'NONE', #16929, #63232, #47912, .T. ) ;
#43998 = AXIS2_PLACEMENT_3D ( 'NONE', #68797, #4911, #50740 ) ;
#43999 = ORIENTED_EDGE ( 'NONE', *, *, #69699, .T. ) ;
#44000 = VERTEX_POINT ( 'NONE', #6455 ) ;
#44001 = CARTESIAN_POINT ( 'NONE',  ( 11.99999999999999822, 8.830959090343430518, -74.65491531819107252 ) ) ;
#44002 = CARTESIAN_POINT ( 'NONE',  ( 5.000000000000002665, -15.33399622253540961, 80.55351364060584274 ) ) ;
#44003 = VERTEX_POINT ( 'NONE', #10592 ) ;
#44004 = CARTESIAN_POINT ( 'NONE',  ( 96.15314808468748708, -208.0026889286704943, 83.08114583420048405 ) ) ;
#44005 = CARTESIAN_POINT ( 'NONE',  ( 97.30629616937498838, -208.6684592857803295, 85.09197916753380753 ) ) ;
#44006 = ORIENTED_EDGE ( 'NONE', *, *, #62038, .F. ) ;
#44007 = CARTESIAN_POINT ( 'NONE',  ( 92.69370383062501162, -209.9999999999999716, 85.99156250086716113 ) ) ;
#44008 = ORIENTED_EDGE ( 'NONE', *, *, #16061, .T. ) ;
#44009 = CYLINDRICAL_SURFACE ( 'NONE', #68316, 31.99999999999999289 ) ;
#44010 = ORIENTED_EDGE ( 'NONE', *, *, #11805, .F. ) ;
#44011 = CARTESIAN_POINT ( 'NONE',  ( -96.15314808468752972, 91.99731107132950569, 76.36072916753381890 ) ) ;
#44012 = CLOSED_SHELL ( 'NONE', ( #25683, #15708, #16414, #35909, #43979, #32896, #14523, #51033, #12715, #33691, #70088, #66825, #39628, #39663, #70407, #11434, #60100, #37402, #14661, #67910, #31489, #32606, #63516, #7243, #21987, #1394, #67326, #37371, #8516, #64252, #7416, #52475, #67069, #33245, #72975, #67838, #37755, #4338, #63087, #20907, #43996, #16222, #7724, #71867, #8678, #35384, #19444, #63506, #35774, #30774, #53479, #43914, #62410, #60354, #36898, #69448, #52208, #4601, #38115, #56124, #2615, #64331, #42276, #38293, #69193, #56574, #61279, #25222, #62868, #22797, #5697, #7710, #66381, #224, #38077, #16037, #31158, #12123, #72745, #24126, #46956, #72455, #52555, #24968, #7258, #4258, #14518, #14335, #48905, #10192, #35895, #49571, #53460, #53291, #20800, #35307, #68911, #13835, #21274, #16607, #62412, #74259, #16197, #61954, #64126, #64834, #25120, #39077, #72339, #74028, #5041, #47560, #66962, #33178, #41169, #58236, #43628, #56397, #74251, #65379, #68047, #36017, #70703, #25196, #44044, #71375, #46955, #22146, #24220, #62342, #1977, #49972, #60598, #16313, #10731, #20960, #61733, #20276, #57154, #36679, #70192, #2322, #50411, #37520, #62488, #20389, #36386, #8587, #20032, #11558, #11692, #27734, #22335, #7631, #43512, #54086, #7221, #21018, #20599, #64872, #9664, #46935, #53327, #67891, #42249, #52299, #30785, #13053, #67463, #71684 ) ) ;
#44013 = VERTEX_POINT ( 'NONE', #477 ) ;
#44014 = ORIENTED_EDGE ( 'NONE', *, *, #27040, .T. ) ;
#44015 = DIRECTION ( 'NONE',  ( 1.000000000000000000, 0.000000000000000000, 0.000000000000000000 ) ) ;
#44016 = EDGE_LOOP ( 'NONE', ( #68617, #25334, #27812, #48641 ) ) ;
#44017 = CARTESIAN_POINT ( 'NONE',  ( 6.782329983125267248, 10.49999999999999645, -125.0000000000000000 ) ) ;
#44018 = CARTESIAN_POINT ( 'NONE',  ( 22.94323693612312809, -114.6983135802921083, -5.500000000000000000 ) ) ;
#44019 = EDGE_LOOP ( 'NONE', ( #72059, #58627, #58624, #18423 ) ) ;
#44020 = CARTESIAN_POINT ( 'NONE',  ( -3.000000000000000000, 8.688484142254221609, -21.88630264137359660 ) ) ;
#44021 = ORIENTED_EDGE ( 'NONE', *, *, #32917, .T. ) ;
#44022 = CARTESIAN_POINT ( 'NONE',  ( 10.00000000000000000, 0.000000000000000000, 0.000000000000000000 ) ) ;
#44023 = VECTOR ( 'NONE', #16581, 1000.000000000000000 ) ;
#44024 = ORIENTED_EDGE ( 'NONE', *, *, #36563, .F. ) ;
#44025 = EDGE_CURVE ( 'NONE', #14912, #53848, #33519, .T. ) ;
#44026 = PRESENTATION_LAYER_ASSIGNMENT (  '', '', ( #65653 ) ) ;
#44027 = ORIENTED_EDGE ( 'NONE', *, *, #18747, .T. ) ;
#44028 = VERTEX_POINT ( 'NONE', #16991 ) ;
#44029 = CARTESIAN_POINT ( 'NONE',  ( -4.592054218142291866, -3.122278952918454031, -5.689399939901067071 ) ) ;
#44030 = CARTESIAN_POINT ( 'NONE',  ( 0.000000000000000000, 0.000000000000000000, 0.000000000000000000 ) ) ;
#44031 = ORIENTED_EDGE ( 'NONE', *, *, #18761, .T. ) ;
#44032 = VERTEX_POINT ( 'NONE', #62878 ) ;
#44033 = AXIS2_PLACEMENT_3D ( 'NONE', #31276, #37310, #36178 ) ;
#44035 = EDGE_CURVE ( 'NONE', #72017, #47938, #57481, .T. ) ;
#44034 = VERTEX_POINT ( 'NONE', #57951 ) ;
#44036 = CIRCLE ( 'NONE', #2052, 16.00000000000000000 ) ;
#44037 = LINE ( 'NONE', #44410, #31256 ) ;
#44038 = CARTESIAN_POINT ( 'NONE',  ( 92.35000000000000853, -209.9999999999999716, 90.00000000000000000 ) ) ;
#44039 = EDGE_CURVE ( 'NONE', #19772, #64359, #67067, .T. ) ;
#44040 = CARTESIAN_POINT ( 'NONE',  ( -93.84685191531252713, 88.00268892867056536, 76.04322916753382344 ) ) ;
#44041 = ORIENTED_EDGE ( 'NONE', *, *, #70616, .T. ) ;
#44042 = AXIS2_PLACEMENT_3D ( 'NONE', #10491, #10876, #44342 ) ;
#44043 = CARTESIAN_POINT ( 'NONE',  ( 93.84685191531248449, 88.00268892867053694, 78.31864583420048120 ) ) ;
#44044 = ADVANCED_FACE ( 'NONE', ( #5721 ), #28997, .F. ) ;
#44045 = ORIENTED_EDGE ( 'NONE', *, *, #69450, .T. ) ;
#44046 = CARTESIAN_POINT ( 'NONE',  ( -96.15314808468747287, -208.0026889286704943, 88.90197916753380980 ) ) ;
#44047 = FACE_OUTER_BOUND ( 'NONE', #20930, .T. ) ;
#44048 = CARTESIAN_POINT ( 'NONE',  ( -3.000000000000000000, -25.60904388321916159, -6.976881207771517879 ) ) ;
#44049 = FACE_OUTER_BOUND ( 'NONE', #45748, .T. ) ;
#44050 = CARTESIAN_POINT ( 'NONE',  ( -93.84685191531247028, -211.9973110713294489, 80.96447916753380980 ) ) ;
#44051 = EDGE_CURVE ( 'NONE', #63122, #45831, #21431, .T. ) ;
#44052 = DIRECTION ( 'NONE',  ( -1.000000000000000000, 0.000000000000000000, 0.000000000000000000 ) ) ;
#44053 = DIRECTION ( 'NONE',  ( -1.000000000000000000, -0.000000000000000000, -0.000000000000000000 ) ) ;
#44054 = CARTESIAN_POINT ( 'NONE',  ( -93.67499999999998295, -207.7050326799711968, 84.07333333333333769 ) ) ;
#44055 = EDGE_LOOP ( 'NONE', ( #1101, #37541 ) ) ;
#44056 = ORIENTED_EDGE ( 'NONE', *, *, #49157, .F. ) ;
#44057 = CARTESIAN_POINT ( 'NONE',  ( 100.0010000000000190, -123.9999999999999858, 39.99999999999996447 ) ) ;
#44058 = CARTESIAN_POINT ( 'NONE',  ( 0.000000000000000000, 0.000000000000000000, 0.000000000000000000 ) ) ;
#44059 = AXIS2_PLACEMENT_3D ( 'NONE', #68986, #17474, #11816 ) ;
#44060 = CARTESIAN_POINT ( 'NONE',  ( -96.15314808468751551, 88.00268892867056536, 80.85864583420047325 ) ) ;
#44061 = CARTESIAN_POINT ( 'NONE',  ( 0.3000000000000016542, 0.000000000000000000, 0.000000000000000000 ) ) ;
#44062 = CARTESIAN_POINT ( 'NONE',  ( 5.000000000000002665, -8.966570791701281351, 81.50828551894224461 ) ) ;
#44063 = EDGE_CURVE ( 'NONE', #991, #1255, #31043, .T. ) ;
#44064 = ORIENTED_EDGE ( 'NONE', *, *, #27040, .F. ) ;
#44065 = DIRECTION ( 'NONE',  ( -1.000000000000000000, 0.000000000000000000, -0.000000000000000000 ) ) ;
#44066 = CARTESIAN_POINT ( 'NONE',  ( -3.000000000000000000, 16.61724383029361718, 20.69703378468926402 ) ) ;
#44067 = LINE ( 'NONE', #9850, #40566 ) ;
#44068 = CARTESIAN_POINT ( 'NONE',  ( -0.0004442498507136653329, 0.001194404164628348752, -70.59999999999999432 ) ) ;
#44069 = DIRECTION ( 'NONE',  ( -1.000000000000000000, 0.000000000000000000, 0.000000000000000000 ) ) ;
#44070 = CARTESIAN_POINT ( 'NONE',  ( -92.69370383062498320, -211.3315407142195852, 81.81114583420048803 ) ) ;
#44071 = EDGE_CURVE ( 'NONE', #63658, #35409, #8245, .T. ) ;
#44072 = CARTESIAN_POINT ( 'NONE',  ( 0.000000000000000000, 0.000000000000000000, -54.99999999999998579 ) ) ;
#44073 = EDGE_CURVE ( 'NONE', #10923, #26528, #35388, .T. ) ;
#44074 = EDGE_CURVE ( 'NONE', #36328, #18041, #53417, .T. ) ;
#44075 = EDGE_LOOP ( 'NONE', ( #62132, #1602, #27384, #56226 ) ) ;
#44076 = CIRCLE ( 'NONE', #11643, 2.055000000000000160 ) ;
#44077 = CARTESIAN_POINT ( 'NONE',  ( 10.00000000000000000, 12.42422080174688404, -35.38097989696498047 ) ) ;
#44078 = CARTESIAN_POINT ( 'NONE',  ( 5.000000000000000000, -27.75498641678764855, 31.52238457039590358 ) ) ;
#44079 = LINE ( 'NONE', #55351, #1011 ) ;
#44080 = CIRCLE ( 'NONE', #17671, 12.50000000000000000 ) ;
#44081 = EDGE_LOOP ( 'NONE', ( #26629, #26952, #2772, #44623 ) ) ;
#44082 = DIRECTION ( 'NONE',  ( 0.000000000000000000, 0.000000000000000000, -1.000000000000000000 ) ) ;
#44083 = CARTESIAN_POINT ( 'NONE',  ( 92.35000000000000853, -209.9999999999999716, 79.83999999999998920 ) ) ;
#44084 = AXIS2_PLACEMENT_3D ( 'NONE', #21092, #48930, #56448 ) ;
#44085 = DIRECTION ( 'NONE',  ( -1.000000000000000000, -0.000000000000000000, 0.000000000000000000 ) ) ;
#44086 = ORIENTED_EDGE ( 'NONE', *, *, #1893, .T. ) ;
#44087 = CARTESIAN_POINT ( 'NONE',  ( 6.782329983125270800, 10.49999999999999467, -125.0000000000000000 ) ) ;
#44088 =( LENGTH_UNIT ( ) NAMED_UNIT ( * ) SI_UNIT ( .MILLI., .METRE. ) );
#44089 = ORIENTED_EDGE ( 'NONE', *, *, #6284, .T. ) ;
#44090 = LINE ( 'NONE', #20421, #61628 ) ;
#44091 = CARTESIAN_POINT ( 'NONE',  ( -10.00000000000000000, 0.000000000000000000, 0.000000000000000000 ) ) ;
#44092 = ORIENTED_EDGE ( 'NONE', *, *, #32602, .F. ) ;
#44093 = DIRECTION ( 'NONE',  ( 0.8541291221503261033, -0.5200609990133016058, 0.000000000000000000 ) ) ;
#44094 = EDGE_LOOP ( 'NONE', ( #46251, #27963, #13943, #44220 ) ) ;
#44095 = CARTESIAN_POINT ( 'NONE',  ( 12.00000000000000000, -13.04903810567646971, 19.60159698893442481 ) ) ;
#44096 = AXIS2_PLACEMENT_3D ( 'NONE', #39393, #55932, #67587 ) ;
#44097 = VERTEX_POINT ( 'NONE', #41395 ) ;
#44098 = ORIENTED_EDGE ( 'NONE', *, *, #70170, .T. ) ;
#44099 = VERTEX_POINT ( 'NONE', #12443 ) ;
#44100 = CARTESIAN_POINT ( 'NONE',  ( 0.000000000000000000, 10.41901085202135491, -40.68715046381917944 ) ) ;
#44101 = VECTOR ( 'NONE', #10631, 1000.000000000000000 ) ;
#44102 = EDGE_CURVE ( 'NONE', #24794, #13281, #69955, .T. ) ;
#44103 = ORIENTED_EDGE ( 'NONE', *, *, #15261, .T. ) ;
#44104 = ORIENTED_EDGE ( 'NONE', *, *, #32761, .T. ) ;
#44105 = CARTESIAN_POINT ( 'NONE',  ( 96.15314808468748708, 88.00268892867053694, 77.94822916753382458 ) ) ;
#44106 = CARTESIAN_POINT ( 'NONE',  ( 11.99999999999999822, 0.000000000000000000, 0.000000000000000000 ) ) ;
#44107 = CARTESIAN_POINT ( 'NONE',  ( 10.00000000000000000, 0.000000000000000000, 0.000000000000000000 ) ) ;
#44108 = ORIENTED_EDGE ( 'NONE', *, *, #15788, .F. ) ;
#44109 = ORIENTED_EDGE ( 'NONE', *, *, #41492, .T. ) ;
#44110 = VERTEX_POINT ( 'NONE', #2325 ) ;
#44111 = CARTESIAN_POINT ( 'NONE',  ( 96.15314808468748708, 91.99731107132950569, 88.79614583420047325 ) ) ;
#44112 = ORIENTED_EDGE ( 'NONE', *, *, #59449, .F. ) ;
#44113 = CARTESIAN_POINT ( 'NONE',  ( 92.69370383062501162, -209.9999999999999716, 85.83281250086714920 ) ) ;
#44114 = CARTESIAN_POINT ( 'NONE',  ( 10.00000000000000000, -12.42422080174614862, -35.38097989696524337 ) ) ;
#44115 = CARTESIAN_POINT ( 'NONE',  ( -96.32500000000001705, 92.29496732002878900, 77.27354166840096639 ) ) ;
#44116 = CARTESIAN_POINT ( 'NONE',  ( 10.00000000000000000, 26.79245525562714647, 32.34446384429980981 ) ) ;
#44117 = DIRECTION ( 'NONE',  ( 0.000000000000000000, 0.000000000000000000, 1.000000000000000000 ) ) ;
#44118 = ADVANCED_FACE ( 'NONE', ( #65081 ), #36858, .T. ) ;
#44119 = CARTESIAN_POINT ( 'NONE',  ( 94.99999999999998579, 90.00000000000002842, 90.00000000000000000 ) ) ;
#44120 = CARTESIAN_POINT ( 'NONE',  ( 10.00000000000000000, 0.000000000000000000, 0.000000000000000000 ) ) ;
#44121 = CARTESIAN_POINT ( 'NONE',  ( -94.99999999999997158, -207.3369185715606307, 88.21406250086714351 ) ) ;
#44122 = EDGE_CURVE ( 'NONE', #69246, #44776, #19561, .T. ) ;
#44123 = CARTESIAN_POINT ( 'NONE',  ( -93.84685191531254134, 91.99731107132950569, 84.50989583420049200 ) ) ;
#44124 = ORIENTED_EDGE ( 'NONE', *, *, #32995, .T. ) ;
#44125 = APPLICATION_CONTEXT ( 'automotive_design' ) ;
#44127 = CARTESIAN_POINT ( 'NONE',  ( -97.30629616937501680, 90.00000000000004263, 87.10281250086714522 ) ) ;
#44126 = CARTESIAN_POINT ( 'NONE',  ( 92.69370383062498320, 90.00000000000002842, 87.73781250086713612 ) ) ;
#44128 = VERTEX_POINT ( 'NONE', #1587 ) ;
#44129 = CARTESIAN_POINT ( 'NONE',  ( 92.35002600533573514, -211.5299932275399897, 84.41729270697884147 ) ) ;
#44130 = AXIS2_PLACEMENT_3D ( 'NONE', #38223, #27299, #32197 ) ;
#44131 = DIRECTION ( 'NONE',  ( 0.000000000000000000, 0.000000000000000000, 1.000000000000000000 ) ) ;
#44132 = DIRECTION ( 'NONE',  ( -1.000000000000000000, 0.000000000000000000, 0.000000000000000000 ) ) ;
#44133 = FACE_OUTER_BOUND ( 'NONE', #35046, .T. ) ;
#44134 = CARTESIAN_POINT ( 'NONE',  ( 10.00000000000000000, 10.41901085202078114, 40.68715046381932865 ) ) ;
#44135 = DIRECTION ( 'NONE',  ( -0.2867529058022035837, 0.9580045777625452175, 0.000000000000000000 ) ) ;
#44136 = EDGE_CURVE ( 'NONE', #49408, #16264, #59954, .T. ) ;
#44137 = EDGE_CURVE ( 'NONE', #54538, #62960, #2336, .T. ) ;
#44138 = DIRECTION ( 'NONE',  ( 0.000000000000000000, -0.8090169943749508930, 0.5877852522924682521 ) ) ;
#44139 = DIRECTION ( 'NONE',  ( -1.000000000000000000, -0.000000000000000000, -0.000000000000000000 ) ) ;
#44140 = VERTEX_POINT ( 'NONE', #18818 ) ;
#44141 = VECTOR ( 'NONE', #6, 1000.000000000000000 ) ;
#44142 = ORIENTED_EDGE ( 'NONE', *, *, #55670, .F. ) ;
#44143 = CIRCLE ( 'NONE', #64531, 31.99999999999999289 ) ;
#44144 = CARTESIAN_POINT ( 'NONE',  ( -95.00000000000002842, 93.05995642670501411, 81.58624999999999261 ) ) ;
#44145 = DIRECTION ( 'NONE',  ( -1.000000000000000000, 0.000000000000000000, 0.000000000000000000 ) ) ;
#44146 = CARTESIAN_POINT ( 'NONE',  ( -11.69999999999999929, 0.000000000000000000, 0.000000000000000000 ) ) ;
#44147 = DIRECTION ( 'NONE',  ( 0.000000000000000000, 0.07845909572784530439, -0.9969173337331279638 ) ) ;
#44148 = DIRECTION ( 'NONE',  ( -1.000000000000000000, 0.000000000000000000, -0.000000000000000000 ) ) ;
#44149 = DIRECTION ( 'NONE',  ( -1.000000000000000000, -0.000000000000000000, 0.000000000000000000 ) ) ;
#44150 = CARTESIAN_POINT ( 'NONE',  ( -92.35000000000003695, 89.99999989488615881, 86.58687499784845443 ) ) ;
#44151 = DIRECTION ( 'NONE',  ( -1.000000000000000000, -0.000000000000000000, -0.000000000000000000 ) ) ;
#44152 = ADVANCED_FACE ( 'NONE', ( #30836 ), #25223, .T. ) ;
#44153 = EDGE_LOOP ( 'NONE', ( #41155, #70103, #43517, #11948 ) ) ;
#44154 = CARTESIAN_POINT ( 'NONE',  ( -95.00000000000002842, 87.33691857156074434, 80.91156250086714863 ) ) ;
#44155 = CARTESIAN_POINT ( 'NONE',  ( 93.67499999999999716, 87.70503267997126784, 82.56520833506762358 ) ) ;
#44156 = DIRECTION ( 'NONE',  ( -1.000000000000000000, 0.000000000000000000, -0.000000000000000000 ) ) ;
#44157 = FILL_AREA_STYLE ('',( #26113 ) ) ;
#44158 = LINE ( 'NONE', #32497, #59710 ) ;
#44159 = PLANE ( 'NONE',  #47317 ) ;
#44160 = CARTESIAN_POINT ( 'NONE',  ( -92.34999999999999432, -209.9999999999999716, 87.14249999999999829 ) ) ;
#44161 = CARTESIAN_POINT ( 'NONE',  ( 10.00000000000000000, -30.84782396557233142, 21.32104025579104345 ) ) ;
#44162 = PLANE ( 'NONE',  #26873 ) ;
#44163 = AXIS2_PLACEMENT_3D ( 'NONE', #32766, #32028, #49328 ) ;
#44164 = EDGE_CURVE ( 'NONE', #32156, #35978, #11891, .T. ) ;
#44165 = EDGE_CURVE ( 'NONE', #46404, #12556, #64777, .T. ) ;
#44166 = ADVANCED_FACE ( 'NONE', ( #35738 ), #7558, .T. ) ;
#44167 = CIRCLE ( 'NONE', #24945, 15.70000000000327312 ) ;
#44168 = EDGE_CURVE ( 'NONE', #72371, #53358, #52750, .T. ) ;
#44169 = CARTESIAN_POINT ( 'NONE',  ( 97.30629616937498838, 88.66845928578035796, 81.17614583420049712 ) ) ;
#44170 = CARTESIAN_POINT ( 'NONE',  ( -92.69370383062498320, -209.9999999999999716, 84.40406250086715545 ) ) ;
#44171 = DIRECTION ( 'NONE',  ( -0.000000000000000000, -0.000000000000000000, 1.000000000000000000 ) ) ;
#44172 = ORIENTED_EDGE ( 'NONE', *, *, #40014, .T. ) ;
#44173 = CARTESIAN_POINT ( 'NONE',  ( -94.99999999999997158, -213.0599564267049857, 77.45874999999999488 ) ) ;
#44174 = CARTESIAN_POINT ( 'NONE',  ( 0.000000000000000000, -0.8299999999999999600, -1.199999999999999956 ) ) ;
#44175 = CARTESIAN_POINT ( 'NONE',  ( -96.15314808468752972, 91.99731107132950569, 78.26572916753382003 ) ) ;
#44176 = CARTESIAN_POINT ( 'NONE',  ( 92.69370383062501162, -208.6684592857803011, 84.50989583420046358 ) ) ;
#44177 = VERTEX_POINT ( 'NONE', #48512 ) ;
#44178 = CARTESIAN_POINT ( 'NONE',  ( 96.85456758451087467, 88.62117599715715244, 74.79348190356851944 ) ) ;
#44179 = ORIENTED_EDGE ( 'NONE', *, *, #9151, .T. ) ;
#44180 =( BOUNDED_CURVE ( )  B_SPLINE_CURVE ( 2, ( #69357, #18227, #5853, #17852, #12211, #29863, #63736, #6586, #17120, #57343, #7325 ),
 .UNSPECIFIED., .F., .F. ) 
 B_SPLINE_CURVE_WITH_KNOTS ( ( 3, 2, 2, 2, 2, 3 ),
 ( 0.1481709449575358828, 0.1481710763585298851, 0.1552268418994119104, 0.1622826074402939078, 0.1693383729811759331, 0.1693384224419982043 ),
 .UNSPECIFIED. ) 
 CURVE ( )  GEOMETRIC_REPRESENTATION_ITEM ( )  RATIONAL_B_SPLINE_CURVE ( ( 0.9999950100192072089, 0.9999975049631379953, 1.000000000000000000, 0.8660254037844387076, 1.000000000000000000, 0.8660254037844387076, 1.000000000000000000, 0.8660254037844387076, 1.000000000000000000, 0.9999990608398684477, 0.9999981216929038075 ) ) 
 REPRESENTATION_ITEM ( '' )  );
#44181 = AXIS2_PLACEMENT_3D ( 'NONE', #32248, #2985, #26243 ) ;
#44182 = CARTESIAN_POINT ( 'NONE',  ( -3.000000000000000000, 22.07842321921492612, -8.187992925817130896 ) ) ;
#44183 = VERTEX_POINT ( 'NONE', #1956 ) ;
#44184 = AXIS2_PLACEMENT_3D ( 'NONE', #14470, #61078, #54332 ) ;
#44185 = AXIS2_PLACEMENT_3D ( 'NONE', #44256, #67186, #55904 ) ;
#44186 = CARTESIAN_POINT ( 'NONE',  ( -96.32499999999996021, -207.7050326799711968, 83.54416666666666913 ) ) ;
#44187 = AXIS2_PLACEMENT_3D ( 'NONE', #67820, #15194, #16316 ) ;
#44188 = VERTEX_POINT ( 'NONE', #24837 ) ;
#44189 = VERTEX_POINT ( 'NONE', #41041 ) ;
#44190 = AXIS2_PLACEMENT_3D ( 'NONE', #931, #23817, #12530 ) ;
#44191 = DIRECTION ( 'NONE',  ( -1.000000000000000000, 0.000000000000000000, 0.000000000000000000 ) ) ;
#44192 = CYLINDRICAL_SURFACE ( 'NONE', #18917, 2.649999999999985700 ) ;
#44193 = LINE ( 'NONE', #67868, #40012 ) ;
#44194 = EDGE_CURVE ( 'NONE', #16169, #62276, #1163, .T. ) ;
#44195 = DIRECTION ( 'NONE',  ( 1.000000000000000000, 0.000000000000000000, 0.000000000000000000 ) ) ;
#44196 = CARTESIAN_POINT ( 'NONE',  ( 94.99999999999998579, 87.33691857156068750, 88.05531250086716000 ) ) ;
#44197 = CARTESIAN_POINT ( 'NONE',  ( 92.34999999999999432, 90.00000000000002842, 80.55437500173430010 ) ) ;
#44198 = CARTESIAN_POINT ( 'NONE',  ( 92.35000000000000853, -209.9999999999999716, 78.57000000000000739 ) ) ;
#44199 = EDGE_CURVE ( 'NONE', #17390, #53342, #4733, .T. ) ;
#44200 = VERTEX_POINT ( 'NONE', #42147 ) ;
#44201 = ORIENTED_EDGE ( 'NONE', *, *, #72875, .F. ) ;
#44202 = VERTEX_POINT ( 'NONE', #13553 ) ;
#44203 = ORIENTED_EDGE ( 'NONE', *, *, #56479, .T. ) ;
#44204 = CARTESIAN_POINT ( 'NONE',  ( 0.000000000000000000, 6.903761155838878061, -77.19088730480517313 ) ) ;
#44205 = EDGE_CURVE ( 'NONE', #54468, #53437, #65812, .T. ) ;
#44206 = AXIS2_PLACEMENT_3D ( 'NONE', #1794, #24679, #57795 ) ;
#44207 = DIRECTION ( 'NONE',  ( -1.000000000000000000, -0.000000000000000000, 0.000000000000000000 ) ) ;
#44208 = CARTESIAN_POINT ( 'NONE',  ( 10.00000000000000000, -22.64427369931148348, -30.00120703465229965 ) ) ;
#44209 = AXIS2_PLACEMENT_3D ( 'NONE', #64562, #11938, #13041 ) ;
#44210 = DIRECTION ( 'NONE',  ( 0.000000000000000000, 0.000000000000000000, 1.000000000000000000 ) ) ;
#44211 = EDGE_CURVE ( 'NONE', #21245, #2928, #3197, .T. ) ;
#44212 = DIRECTION ( 'NONE',  ( -1.000000000000000000, -0.000000000000000000, 0.000000000000000000 ) ) ;
#44213 = AXIS2_PLACEMENT_3D ( 'NONE', #16352, #61487, #15976 ) ;
#44214 = DIRECTION ( 'NONE',  ( 0.000000000000000000, 0.000000000000000000, 1.000000000000000000 ) ) ;
#44215 = CIRCLE ( 'NONE', #53809, 82.00000000000000000 ) ;
#44216 = ORIENTED_EDGE ( 'NONE', *, *, #36168, .T. ) ;
#44217 = CARTESIAN_POINT ( 'NONE',  ( -93.67499999999998295, -212.2949673200287179, 85.21104166840096639 ) ) ;
#44218 = ORIENTED_EDGE ( 'NONE', *, *, #57235, .T. ) ;
#44219 = DIRECTION ( 'NONE',  ( -0.000000000000000000, -0.000000000000000000, -1.000000000000000000 ) ) ;
#44220 = ORIENTED_EDGE ( 'NONE', *, *, #3615, .T. ) ;
#44221 = CARTESIAN_POINT ( 'NONE',  ( -92.35000000000005116, 88.47002178664754979, 84.62895833506763665 ) ) ;
#44222 = CIRCLE ( 'NONE', #10609, 42.00000000000000000 ) ;
#44223 = VERTEX_POINT ( 'NONE', #8669 ) ;
#44224 = CARTESIAN_POINT ( 'NONE',  ( 96.15314808468748708, 91.99731107132950569, 81.96989583420048575 ) ) ;
#44225 = CARTESIAN_POINT ( 'NONE',  ( 11.99999999999999822, 24.73286445877705475, 73.44644590900068692 ) ) ;
#44226 = LINE ( 'NONE', #5131, #73852 ) ;
#44227 = DIRECTION ( 'NONE',  ( 0.000000000000000000, 0.000000000000000000, 1.000000000000000000 ) ) ;
#44228 = LINE ( 'NONE', #72767, #9003 ) ;
#44229 = ADVANCED_FACE ( 'NONE', ( #60906 ), #42885, .T. ) ;
#44230 = CARTESIAN_POINT ( 'NONE',  ( 0.000000000000000000, 0.000000000000000000, 0.000000000000000000 ) ) ;
#44231 = VERTEX_POINT ( 'NONE', #14666 ) ;
#44232 = CARTESIAN_POINT ( 'NONE',  ( 11.99999999999999822, 44.99326035066052754, 68.55367621811160461 ) ) ;
#44233 = CYLINDRICAL_SURFACE ( 'NONE', #50312, 77.49899999999999523 ) ;
#44234 = ORIENTED_EDGE ( 'NONE', *, *, #47032, .T. ) ;
#44235 = ORIENTED_EDGE ( 'NONE', *, *, #14188, .F. ) ;
#44236 = CARTESIAN_POINT ( 'NONE',  ( 0.000000000000000000, 71.21200624218795383, 40.65526001592638039 ) ) ;
#44237 = EDGE_CURVE ( 'NONE', #49091, #53076, #20306, .T. ) ;
#44238 = LINE ( 'NONE', #32935, #47408 ) ;
#44239 = DIRECTION ( 'NONE',  ( -1.000000000000000000, 0.000000000000000000, 0.000000000000000000 ) ) ;
#44240 = CARTESIAN_POINT ( 'NONE',  ( -97.30629616937497417, -211.3315407142195852, 85.40947916753380298 ) ) ;
#44241 = ORIENTED_EDGE ( 'NONE', *, *, #72875, .T. ) ;
#44242 = CIRCLE ( 'NONE', #23841, 77.49899999999999523 ) ;
#44243 = EDGE_CURVE ( 'NONE', #5010, #20558, #61284, .T. ) ;
#44244 = ORIENTED_EDGE ( 'NONE', *, *, #4200, .F. ) ;
#44245 = AXIS2_PLACEMENT_3D ( 'NONE', #14096, #37044, #54339 ) ;
#44246 = EDGE_CURVE ( 'NONE', #22856, #11006, #72171, .T. ) ;
#44247 = CARTESIAN_POINT ( 'NONE',  ( -15.70044424985254850, 0.001194404164626844313, -85.59999999999999432 ) ) ;
#44248 = VECTOR ( 'NONE', #26753, 1000.000000000000000 ) ;
#44249 = CARTESIAN_POINT ( 'NONE',  ( 92.69370383062498320, 88.66845928578035796, 78.26572916753380582 ) ) ;
#44250 = CIRCLE ( 'NONE', #52605, 31.99999999999998224 ) ;
#44251 = CARTESIAN_POINT ( 'NONE',  ( 0.000000000000000000, 74.65374052328648702, 8.840884882375350529 ) ) ;
#44252 = DIRECTION ( 'NONE',  ( 0.000000000000000000, 0.000000000000000000, 1.000000000000000000 ) ) ;
#44253 = CARTESIAN_POINT ( 'NONE',  ( 0.000000000000000000, -62.50329211542407393, -41.76937507738853839 ) ) ;
#44254 = CARTESIAN_POINT ( 'NONE',  ( 92.48632958231164025, 89.99999999999990052, 74.91808492278045151 ) ) ;
#44255 = LINE ( 'NONE', #61553, #12555 ) ;
#44256 = CARTESIAN_POINT ( 'NONE',  ( 0.000000000000000000, 0.000000000000000000, -4.400000000000001243 ) ) ;
#44257 = EDGE_CURVE ( 'NONE', #22755, #15522, #71942, .T. ) ;
#44258 = DIRECTION ( 'NONE',  ( -1.000000000000000000, 0.000000000000000000, 0.000000000000000000 ) ) ;
#44259 = EDGE_CURVE ( 'NONE', #11277, #35768, #56352, .T. ) ;
#44260 = FACE_OUTER_BOUND ( 'NONE', #54284, .T. ) ;
#44261 = CYLINDRICAL_SURFACE ( 'NONE', #12104, 31.99999999999998579 ) ;
#44262 = AXIS2_PLACEMENT_3D ( 'NONE', #29823, #1322, #64067 ) ;
#44263 = ORIENTED_EDGE ( 'NONE', *, *, #35393, .T. ) ;
#44264 = CARTESIAN_POINT ( 'NONE',  ( -95.00000000000002842, 92.66308142843932671, 84.40406250086714124 ) ) ;
#44265 = FACE_OUTER_BOUND ( 'NONE', #19884, .T. ) ;
#44266 = AXIS2_PLACEMENT_3D ( 'NONE', #37643, #9057, #4928 ) ;
#44267 = VECTOR ( 'NONE', #10524, 1000.000000000000000 ) ;
#44268 = VECTOR ( 'NONE', #49335, 1000.000000000000000 ) ;
#44269 = DIRECTION ( 'NONE',  ( -1.000000000000000000, 0.000000000000000000, 0.000000000000000000 ) ) ;
#44270 = EDGE_LOOP ( 'NONE', ( #3629, #41432, #52988, #28742 ) ) ;
#44271 = VECTOR ( 'NONE', #57316, 1000.000000000000000 ) ;
#44272 = DIRECTION ( 'NONE',  ( 1.000000000000000000, 0.000000000000000000, 0.000000000000000000 ) ) ;
#44273 = CARTESIAN_POINT ( 'NONE',  ( 10.00000000000000000, -36.13751322684404244, -21.40280677340410165 ) ) ;
#44274 = DIRECTION ( 'NONE',  ( -1.000000000000000000, 0.000000000000000000, 0.000000000000000000 ) ) ;
#44275 = CARTESIAN_POINT ( 'NONE',  ( 0.000000000000000000, 0.000000000000000000, 0.000000000000000000 ) ) ;
#44276 = CARTESIAN_POINT ( 'NONE',  ( 97.30629616937498838, -211.3315407142195852, 79.90614583420048689 ) ) ;
#44277 = ORIENTED_EDGE ( 'NONE', *, *, #53789, .T. ) ;
#44278 = ORIENTED_EDGE ( 'NONE', *, *, #54671, .T. ) ;
#44279 = CIRCLE ( 'NONE', #38431, 3.299999999999997158 ) ;
#44280 = CARTESIAN_POINT ( 'NONE',  ( 10.00000000000000000, -31.47745569255092235, -68.26794271651296242 ) ) ;
#44281 = DIRECTION ( 'NONE',  ( -1.000000000000000000, 0.000000000000000000, 0.000000000000000000 ) ) ;
#44282 = DIRECTION ( 'NONE',  ( -1.000000000000000000, 0.000000000000000000, 0.000000000000000000 ) ) ;
#44283 = LINE ( 'NONE', #49907, #74141 ) ;
#44284 = CARTESIAN_POINT ( 'NONE',  ( 95.00000000000000000, -212.6630814284392557, 76.62531250086715318 ) ) ;
#44285 = CIRCLE ( 'NONE', #8210, 16.00000000000000000 ) ;
#44286 = AXIS2_PLACEMENT_3D ( 'NONE', #39088, #22164, #32678 ) ;
#44287 = ORIENTED_EDGE ( 'NONE', *, *, #29371, .T. ) ;
#44288 = EDGE_CURVE ( 'NONE', #33478, #58617, #37616, .T. ) ;
#44289 = ORIENTED_EDGE ( 'NONE', *, *, #36388, .F. ) ;
#44290 = EDGE_LOOP ( 'NONE', ( #31616, #36513, #47654, #13206 ) ) ;
#44291 = DIRECTION ( 'NONE',  ( -0.8225049752423776450, -0.5687579148473765889, 0.000000000000000000 ) ) ;
#44292 = EDGE_CURVE ( 'NONE', #33472, #18767, #67287, .T. ) ;
#44293 = CARTESIAN_POINT ( 'NONE',  ( -96.32500000000001705, 92.29496732002878900, 89.33854166840096411 ) ) ;
#44294 = VECTOR ( 'NONE', #15400, 1000.000000000000000 ) ;
#44295 = ORIENTED_EDGE ( 'NONE', *, *, #53316, .F. ) ;
#44296 = CARTESIAN_POINT ( 'NONE',  ( 94.99999999999998579, 86.94004357329502852, 87.61874999999999147 ) ) ;
#44297 = CARTESIAN_POINT ( 'NONE',  ( 92.35000000000000853, -209.9999999999999716, 78.64937500173429896 ) ) ;
#44298 = ADVANCED_FACE ( 'NONE', ( #27044 ), #32686, .T. ) ;
#44299 = CARTESIAN_POINT ( 'NONE',  ( 96.32499999999997442, 92.29496732002878900, 83.43833333333333258 ) ) ;
#44300 = ORIENTED_EDGE ( 'NONE', *, *, #40685, .F. ) ;
#44301 = CARTESIAN_POINT ( 'NONE',  ( 0.000000000000000000, -27.05870788708250885, 26.08949754953014022 ) ) ;
#44302 = ORIENTED_EDGE ( 'NONE', *, *, #27213, .T. ) ;
#44303 = CYLINDRICAL_SURFACE ( 'NONE', #2131, 31.99999999999999289 ) ;
#44304 = ORIENTED_EDGE ( 'NONE', *, *, #46619, .T. ) ;
#44305 = CARTESIAN_POINT ( 'NONE',  ( 10.00000000000000000, -51.02545421589285723, -55.20638768913812555 ) ) ;
#44306 = CARTESIAN_POINT ( 'NONE',  ( -92.69370383062505425, 91.33154071421968467, 85.09197916753380753 ) ) ;
#44307 = CARTESIAN_POINT ( 'NONE',  ( 92.69370383062498320, 90.00000000000002842, 79.48281250086714067 ) ) ;
#44308 = ORIENTED_EDGE ( 'NONE', *, *, #59887, .T. ) ;
#44309 = VECTOR ( 'NONE', #55325, 1000.000000000000000 ) ;
#44310 = DIRECTION ( 'NONE',  ( -1.000000000000000000, -0.000000000000000000, -0.000000000000000000 ) ) ;
#44311 = VECTOR ( 'NONE', #24085, 1000.000000000000000 ) ;
#44312 = LINE ( 'NONE', #21744, #3693 ) ;
#44313 = ORIENTED_EDGE ( 'NONE', *, *, #44770, .T. ) ;
#44314 = CARTESIAN_POINT ( 'NONE',  ( 0.000000000000000000, -31.46837873495025306, 68.27212725128265447 ) ) ;
#44315 = AXIS2_PLACEMENT_3D ( 'NONE', #72906, #26328, #38357 ) ;
#44317 = AXIS2_PLACEMENT_3D ( 'NONE', #42451, #65388, #8226 ) ;
#44316 = CARTESIAN_POINT ( 'NONE',  ( -92.69370383062498320, -208.6684592857803011, 82.39322916753381776 ) ) ;
#44318 = ORIENTED_EDGE ( 'NONE', *, *, #69502, .T. ) ;
#44319 = ORIENTED_EDGE ( 'NONE', *, *, #13513, .T. ) ;
#44320 = DIRECTION ( 'NONE',  ( 0.000000000000000000, -1.000000000000000000, -1.040834085586084730E-14 ) ) ;
#44321 = AXIS2_PLACEMENT_3D ( 'NONE', #27735, #60481, #73585 ) ;
#44322 = VECTOR ( 'NONE', #3414, 1000.000000000000000 ) ;
#44323 = ORIENTED_EDGE ( 'NONE', *, *, #63814, .F. ) ;
#44324 = CARTESIAN_POINT ( 'NONE',  ( -92.34999999999999432, -210.0000000207151629, 80.87187500099602744 ) ) ;
#44325 = AXIS2_PLACEMENT_3D ( 'NONE', #60379, #66020, #66389 ) ;
#44326 = CARTESIAN_POINT ( 'NONE',  ( 94.99999999999998579, 86.94004357329500010, 88.96812500173430749 ) ) ;
#44327 = ORIENTED_EDGE ( 'NONE', *, *, #36217, .F. ) ;
#44328 = CARTESIAN_POINT ( 'NONE',  ( -93.84685191531248449, -208.0026889286704943, 79.90614583420047268 ) ) ;
#44329 = VERTEX_POINT ( 'NONE', #31952 ) ;
#44330 = CARTESIAN_POINT ( 'NONE',  ( 10.00000000000000000, -2.956366410620109519, -75.11725578898472122 ) ) ;
#44331 = CARTESIAN_POINT ( 'NONE',  ( 10.00000000000000000, 0.000000000000000000, 0.000000000000000000 ) ) ;
#44332 = DIRECTION ( 'NONE',  ( 0.000000000000000000, 0.000000000000000000, 1.000000000000000000 ) ) ;
#44333 = DIRECTION ( 'NONE',  ( -1.000000000000000000, 0.000000000000000000, -0.000000000000000000 ) ) ;
#44334 = CARTESIAN_POINT ( 'NONE',  ( -93.67500000000003979, 87.70503267997129626, 81.32166666666667254 ) ) ;
#44335 = ADVANCED_FACE ( 'NONE', ( #26315 ), #15032, .F. ) ;
#44336 = ADVANCED_FACE ( 'NONE', ( #26680 ), #31581, .T. ) ;
#44337 = CARTESIAN_POINT ( 'NONE',  ( 0.000000000000000000, -75.11764819372145041, 29.05362095685286761 ) ) ;
#44338 = CARTESIAN_POINT ( 'NONE',  ( 93.84685191531248449, 88.00268892867053694, 87.84364583420047268 ) ) ;
#44339 = CARTESIAN_POINT ( 'NONE',  ( -3.000000000000000000, 0.000000000000000000, 0.000000000000000000 ) ) ;
#44340 = CARTESIAN_POINT ( 'NONE',  ( 10.00000000000000000, -17.80606268964563554, 33.00180498840040855 ) ) ;
#44341 = CARTESIAN_POINT ( 'NONE',  ( 0.000000000000000000, 16.61724383029361718, 20.69703378468926402 ) ) ;
#44342 = DIRECTION ( 'NONE',  ( 0.000000000000000000, 0.000000000000000000, 1.000000000000000000 ) ) ;
#44343 = VECTOR ( 'NONE', #11741, 1000.000000000000000 ) ;
#44344 = CARTESIAN_POINT ( 'NONE',  ( 0.000000000000000000, 30.00120703465236716, -22.64427369931138756 ) ) ;
#44345 = CARTESIAN_POINT ( 'NONE',  ( -92.35000000000003695, 89.99999996655868983, 87.85687500050293863 ) ) ;
#44346 = EDGE_CURVE ( 'NONE', #57622, #43494, #9768, .T. ) ;
#44347 = DIRECTION ( 'NONE',  ( 0.000000000000000000, 0.000000000000000000, 1.000000000000000000 ) ) ;
#44348 = CIRCLE ( 'NONE', #19106, 42.00000000000000000 ) ;
#44349 = DIRECTION ( 'NONE',  ( -0.000000000000000000, -0.000000000000000000, 1.000000000000000000 ) ) ;
#44350 = AXIS2_PLACEMENT_3D ( 'NONE', #28638, #51203, #39566 ) ;
#44351 = VECTOR ( 'NONE', #30374, 1000.000000000000000 ) ;
#44352 = VECTOR ( 'NONE', #24529, 1000.000000000000000 ) ;
#44353 = CARTESIAN_POINT ( 'NONE',  ( 10.00000000000000000, 5.202137450156389953, 37.22597642581160216 ) ) ;
#44355 = AXIS2_PLACEMENT_3D ( 'NONE', #40099, #62298, #46111 ) ;
#44354 = CYLINDRICAL_SURFACE ( 'NONE', #44286, 16.00000000000000000 ) ;
#44356 = CARTESIAN_POINT ( 'NONE',  ( -97.64999999999994884, -208.4700217866474645, 86.13708333333332234 ) ) ;
#44357 = AXIS2_PLACEMENT_3D ( 'NONE', #15785, #10507, #74034 ) ;
#44358 = CARTESIAN_POINT ( 'NONE',  ( 7.103376864691351012E-17, -120.0000000000000000, -80.00000000000000000 ) ) ;
#44359 = DIRECTION ( 'NONE',  ( -0.2306669878475637314, -0.9730327541852493711, 0.000000000000000000 ) ) ;
#44360 = DIRECTION ( 'NONE',  ( -1.000000000000000000, -0.000000000000000000, -0.000000000000000000 ) ) ;
#44361 = CARTESIAN_POINT ( 'NONE',  ( -3.000000000000000000, 5.835314593368772229, -22.81335362449846826 ) ) ;
#44362 = DIRECTION ( 'NONE',  ( 0.000000000000000000, 0.000000000000000000, 1.000000000000000000 ) ) ;
#44363 = AXIS2_PLACEMENT_3D ( 'NONE', #16871, #73249, #39431 ) ;
#44364 = AXIS2_PLACEMENT_3D ( 'NONE', #24606, #65213, #30604 ) ;
#44365 = VECTOR ( 'NONE', #35972, 1000.000000000000000 ) ;
#44366 = CARTESIAN_POINT ( 'NONE',  ( 95.00000000000000000, -212.6630814284392557, 88.69031250086716511 ) ) ;
#44367 = ORIENTED_EDGE ( 'NONE', *, *, #59406, .T. ) ;
#44368 = VECTOR ( 'NONE', #38470, 1000.000000000000000 ) ;
#44369 = EDGE_LOOP ( 'NONE', ( #43653, #1001, #56589, #47153 ) ) ;
#44370 = AXIS2_PLACEMENT_3D ( 'NONE', #10417, #28081, #73944 ) ;
#44371 = DIRECTION ( 'NONE',  ( 0.000000000000000000, -0.9876883405951393247, 0.1564344650402207104 ) ) ;
#44372 = DIRECTION ( 'NONE',  ( -0.8774505977381971134, -0.4796670183876317051, 0.000000000000000000 ) ) ;
#44373 = VERTEX_POINT ( 'NONE', #55263 ) ;
#44374 = CARTESIAN_POINT ( 'NONE',  ( 95.00000000000000000, -207.3369185715606307, 79.32406250086714294 ) ) ;
#44375 = CARTESIAN_POINT ( 'NONE',  ( 92.69370383062501162, -211.3315407142195852, 86.04447916753382231 ) ) ;
#44376 = VERTEX_POINT ( 'NONE', #50357 ) ;
#44377 = CARTESIAN_POINT ( 'NONE',  ( 92.69370383062501162, -211.3315407142195852, 86.04447916753382231 ) ) ;
#44378 = ORIENTED_EDGE ( 'NONE', *, *, #31836, .F. ) ;
#44379 = EDGE_CURVE ( 'NONE', #55291, #54928, #25947, .T. ) ;
#44380 = CARTESIAN_POINT ( 'NONE',  ( 10.00000000000000000, 34.94270380257639630, 74.18225833017902460 ) ) ;
#44381 = EDGE_LOOP ( 'NONE', ( #57892, #52233, #31161, #32546 ) ) ;
#44382 = FACE_OUTER_BOUND ( 'NONE', #45859, .T. ) ;
#44383 = EDGE_CURVE ( 'NONE', #2104, #2804, #5976, .T. ) ;
#44384 = ORIENTED_EDGE ( 'NONE', *, *, #58297, .F. ) ;
#44385 = CARTESIAN_POINT ( 'NONE',  ( 0.000000000000000000, 0.000000000000000000, 0.000000000000000000 ) ) ;
#44386 = ORIENTED_EDGE ( 'NONE', *, *, #25235, .F. ) ;
#44387 = CARTESIAN_POINT ( 'NONE',  ( 96.32499999999997442, 92.29496732002878900, 87.96270833506763154 ) ) ;
#44388 = CARTESIAN_POINT ( 'NONE',  ( 95.00000000000000000, -213.0599564267049857, 88.96812500173430749 ) ) ;
#44389 = EDGE_CURVE ( 'NONE', #41196, #53383, #47970, .T. ) ;
#44390 = ORIENTED_EDGE ( 'NONE', *, *, #68329, .T. ) ;
#44391 = DIRECTION ( 'NONE',  ( 0.000000000000000000, 0.000000000000000000, 1.000000000000000000 ) ) ;
#44392 = ORIENTED_EDGE ( 'NONE', *, *, #68849, .F. ) ;
#44393 =( BOUNDED_CURVE ( )  B_SPLINE_CURVE ( 2, ( #12981, #64506, #1021, #47580, #23914, #41207, #46854, #53226, #37695 ),
 .UNSPECIFIED., .F., .F. ) 
 B_SPLINE_CURVE_WITH_KNOTS ( ( 3, 2, 2, 2, 3 ),
 ( 0.2116728463006668226, 0.2116729662264711376, 0.2187287317673534959, 0.2257844973082358264, 0.2328402629019979686 ),
 .UNSPECIFIED. ) 
 CURVE ( )  GEOMETRIC_REPRESENTATION_ITEM ( )  RATIONAL_B_SPLINE_CURVE ( ( 0.9999954457845777744, 0.9999977228535845697, 1.000000000000000000, 0.8660254037844387076, 1.000000000000000000, 0.8660254037844387076, 1.000000000000000000, 0.8660254037844387076, 1.000000000000000000 ) ) 
 REPRESENTATION_ITEM ( '' )  );
#44394 = DIRECTION ( 'NONE',  ( -1.000000000000000000, -0.000000000000000000, -0.000000000000000000 ) ) ;
#44395 = ADVANCED_FACE ( 'NONE', ( #54889 ), #74033, .T. ) ;
#44396 = VECTOR ( 'NONE', #36451, 1000.000000000000000 ) ;
#44397 = ORIENTED_EDGE ( 'NONE', *, *, #1486, .F. ) ;
#44398 = CIRCLE ( 'NONE', #21, 82.00000000000000000 ) ;
#44399 = AXIS2_PLACEMENT_3D ( 'NONE', #35459, #46751, #41838 ) ;
#44400 = ADVANCED_FACE ( 'NONE', ( #56390 ), #4905, .F. ) ;
#44401 = ORIENTED_EDGE ( 'NONE', *, *, #63332, .T. ) ;
#44402 = ORIENTED_EDGE ( 'NONE', *, *, #31914, .F. ) ;
#44403 = CARTESIAN_POINT ( 'NONE',  ( -3.556264818047238485, -3.720292241887096285, -5.918341802876226687 ) ) ;
#44404 = ITEM_DEFINED_TRANSFORMATION ( 'NONE', 'NONE', #40003,  #43395 ) ;
#44405 = DIRECTION ( 'NONE',  ( -1.000000000000000000, 0.000000000000000000, 0.000000000000000000 ) ) ;
#44406 = ORIENTED_EDGE ( 'NONE', *, *, #51004, .T. ) ;
#44407 = ORIENTED_EDGE ( 'NONE', *, *, #51000, .F. ) ;
#44408 = CIRCLE ( 'NONE', #48002, 31.99999999999998934 ) ;
#44409 = VERTEX_POINT ( 'NONE', #39467 ) ;
#44410 = CARTESIAN_POINT ( 'NONE',  ( 4.999999999999999112, 2.663952781846732343, -41.91543099594814947 ) ) ;
#44411 = CARTESIAN_POINT ( 'NONE',  ( -92.34999999999999432, -209.9999999999999716, 88.41249999999999432 ) ) ;
#44412 = EDGE_CURVE ( 'NONE', #41638, #70257, #20317, .T. ) ;
#44413 = CARTESIAN_POINT ( 'NONE',  ( -97.65000000000001990, 90.00000000000004263, 89.36499999999999488 ) ) ;
#44414 = EDGE_CURVE ( 'NONE', #5889, #42911, #27801, .T. ) ;
#44415 = ORIENTED_EDGE ( 'NONE', *, *, #19660, .T. ) ;
#44416 = CARTESIAN_POINT ( 'NONE',  ( 93.84685191531248449, 91.99731107132950569, 77.47197916753380298 ) ) ;
#44417 = VERTEX_POINT ( 'NONE', #23286 ) ;
#44418 = CARTESIAN_POINT ( 'NONE',  ( -94.99999999999997158, -209.9999999999999716, 90.00000000000000000 ) ) ;
#44419 = CARTESIAN_POINT ( 'NONE',  ( -97.30629616937497417, -208.6684592857803011, 88.31989583420046586 ) ) ;
#44420 = EDGE_LOOP ( 'NONE', ( #21416, #39342, #54908, #29281 ) ) ;
#44421 = CARTESIAN_POINT ( 'NONE',  ( 5.000000000000000888, -2.886751345948134873, -2.080000000000000071 ) ) ;
#44422 = LINE ( 'NONE', #32742, #58402 ) ;
#44423 = LINE ( 'NONE', #27101, #69310 ) ;
#44424 = CARTESIAN_POINT ( 'NONE',  ( -96.15314808468745866, -211.9973110713294489, 80.85864583420047325 ) ) ;
#44425 = AXIS2_PLACEMENT_3D ( 'NONE', #69472, #64216, #58556 ) ;
#44426 = CARTESIAN_POINT ( 'NONE',  ( 10.00000000000000000, -11.30684508768395524, 76.66974797899831628 ) ) ;
#44427 = CARTESIAN_POINT ( 'NONE',  ( 5.000000000000002665, 34.94270380257639630, 74.18225833017899618 ) ) ;
#44428 = AXIS2_PLACEMENT_3D ( 'NONE', #9670, #32211, #65346 ) ;
#44429 = CARTESIAN_POINT ( 'NONE',  ( -92.35000000000006537, -208.4700217866474361, 84.02041666666666231 ) ) ;
#44430 = ORIENTED_EDGE ( 'NONE', *, *, #62246, .F. ) ;
#44431 = AXIS2_PLACEMENT_3D ( 'NONE', #9903, #9540, #5031 ) ;
#44432 = ADVANCED_FACE ( 'NONE', ( #17268 ), #45861, .T. ) ;
#44433 = EDGE_CURVE ( 'NONE', #29431, #66920, #39549, .T. ) ;
#44434 = AXIS2_PLACEMENT_3D ( 'NONE', #25735, #49765, #38123 ) ;
#44435 = ORIENTED_EDGE ( 'NONE', *, *, #13917, .F. ) ;
#44436 = CARTESIAN_POINT ( 'NONE',  ( 0.000000000000000000, 0.000000000000000000, 0.000000000000000000 ) ) ;
#44437 = VECTOR ( 'NONE', #17751, 1000.000000000000000 ) ;
#44438 = VECTOR ( 'NONE', #21137, 1000.000000000000000 ) ;
#44439 = CARTESIAN_POINT ( 'NONE',  ( -94.99999999999997158, -213.0599564267049857, 88.88875000000000171 ) ) ;
#44440 = CARTESIAN_POINT ( 'NONE',  ( 96.40521225739051658, -208.1321859400968606, 74.80441578173235939 ) ) ;
#44441 = CARTESIAN_POINT ( 'NONE',  ( -92.69370383062502583, 91.33154071421968467, 80.48822916753383083 ) ) ;
#44442 = PLANE ( 'NONE',  #56271 ) ;
#44443 = DIRECTION ( 'NONE',  ( -1.000000000000000000, 0.000000000000000000, 0.000000000000000000 ) ) ;
#44444 = VERTEX_POINT ( 'NONE', #34549 ) ;
#44445 = PLANE ( 'NONE',  #7595 ) ;
#44446 = DIRECTION ( 'NONE',  ( 0.000000000000000000, 0.000000000000000000, 1.000000000000000000 ) ) ;
#44447 = LINE ( 'NONE', #50055, #11725 ) ;
#44448 = DIRECTION ( 'NONE',  ( 1.000000000000000000, 1.427937372958405461E-15, 7.962523111839130290E-16 ) ) ;
#44449 = DIRECTION ( 'NONE',  ( 0.000000000000000000, 0.000000000000000000, 1.000000000000000000 ) ) ;
#44450 = CARTESIAN_POINT ( 'NONE',  ( -92.69370383062498320, -208.6684592857803011, 79.37697916753381833 ) ) ;
#44451 = DIRECTION ( 'NONE',  ( 0.000000000000000000, 0.000000000000000000, -1.000000000000000000 ) ) ;
#44452 = ORIENTED_EDGE ( 'NONE', *, *, #17994, .F. ) ;
#44453 = FACE_OUTER_BOUND ( 'NONE', #66196, .T. ) ;
#44454 = CARTESIAN_POINT ( 'NONE',  ( 96.32499999999997442, 92.29496732002878900, 76.53270833506762472 ) ) ;
#44455 = DIRECTION ( 'NONE',  ( -1.000000000000000000, -0.000000000000000000, -0.000000000000000000 ) ) ;
#44456 = ORIENTED_EDGE ( 'NONE', *, *, #45785, .F. ) ;
#44457 = CARTESIAN_POINT ( 'NONE',  ( 92.34999999999999432, 90.00000000000002842, 77.37937500173428873 ) ) ;
#44458 = AXIS2_PLACEMENT_3D ( 'NONE', #58960, #64974, #63869 ) ;
#44459 = DIRECTION ( 'NONE',  ( -1.000000000000000000, 0.000000000000000000, -0.000000000000000000 ) ) ;
#44460 = AXIS2_PLACEMENT_3D ( 'NONE', #1019, #25010, #47951 ) ;
#44461 = UNCERTAINTY_MEASURE_WITH_UNIT (LENGTH_MEASURE( 1.000000000000000082E-05 ), #46761, 'distance_accuracy_value', 'NONE');
#44462 = AXIS2_PLACEMENT_3D ( 'NONE', #14618, #20250, #27002 ) ;
#44463 = ADVANCED_FACE ( 'NONE', ( #56765 ), #62793, .T. ) ;
#44464 = VERTEX_POINT ( 'NONE', #50727 ) ;
#44465 = EDGE_CURVE ( 'NONE', #21230, #73771, #26327, .T. ) ;
#44466 = CARTESIAN_POINT ( 'NONE',  ( -5.000000000000000000, -2.886751345948137981, -5.553418012614792509 ) ) ;
#44467 = LINE ( 'NONE', #54270, #40292 ) ;
#44468 = ORIENTED_EDGE ( 'NONE', *, *, #18984, .T. ) ;
#44469 = EDGE_CURVE ( 'NONE', #41714, #32656, #66369, .T. ) ;
#44470 = CARTESIAN_POINT ( 'NONE',  ( 92.69370383062501162, -211.3315407142195852, 89.06072916753382174 ) ) ;
#44471 = CARTESIAN_POINT ( 'NONE',  ( 95.00000000000000000, -206.9400435732949575, 86.03125000000000000 ) ) ;
#44472 = EDGE_LOOP ( 'NONE', ( #36580, #25136, #15143, #53977 ) ) ;
#44473 = ADVANCED_FACE ( 'NONE', ( #51847 ), #22926, .T. ) ;
#44474 = PLANE ( 'NONE',  #19851 ) ;
#44475 = CIRCLE ( 'NONE', #21655, 16.00000000000000000 ) ;
#44476 = ORIENTED_EDGE ( 'NONE', *, *, #58219, .T. ) ;
#44477 = CARTESIAN_POINT ( 'NONE',  ( -92.35000000000003695, 90.00000000000004263, 88.41249999999999432 ) ) ;
#44478 = AXIS2_PLACEMENT_3D ( 'NONE', #27794, #68772, #4512 ) ;
#44479 = CIRCLE ( 'NONE', #36097, 31.99999999999998579 ) ;
#44480 = CARTESIAN_POINT ( 'NONE',  ( 93.67500000000001137, -212.2949673200287179, 81.85083333333332689 ) ) ;
#44481 = EDGE_LOOP ( 'NONE', ( #42903, #68803 ) ) ;
#44482 = EDGE_CURVE ( 'NONE', #30878, #29007, #69148, .T. ) ;
#44483 = ORIENTED_EDGE ( 'NONE', *, *, #71050, .T. ) ;
#44484 = AXIS2_PLACEMENT_3D ( 'NONE', #36585, #2053, #30572 ) ;
#44485 = CIRCLE ( 'NONE', #6076, 31.99999999999999289 ) ;
#44486 = ORIENTED_EDGE ( 'NONE', *, *, #34273, .T. ) ;
#44487 = DIRECTION ( 'NONE',  ( 0.000000000000000000, 0.000000000000000000, 1.000000000000000000 ) ) ;
#44488 = ORIENTED_EDGE ( 'NONE', *, *, #4365, .T. ) ;
#44489 = ORIENTED_EDGE ( 'NONE', *, *, #4103, .F. ) ;
#44490 = CARTESIAN_POINT ( 'NONE',  ( 92.69370383062498320, 90.00000000000002842, 76.46656250086715545 ) ) ;
#44491 = DIRECTION ( 'NONE',  ( -1.000000000000000000, 0.000000000000000000, -0.000000000000000000 ) ) ;
#44492 = EDGE_CURVE ( 'NONE', #56256, #20705, #23990, .T. ) ;
#44493 = DIRECTION ( 'NONE',  ( 1.000000000000000000, 0.000000000000000000, 0.000000000000000000 ) ) ;
#44494 = VERTEX_POINT ( 'NONE', #39090 ) ;
#44495 = ORIENTED_EDGE ( 'NONE', *, *, #24459, .T. ) ;
#44496 = ORIENTED_EDGE ( 'NONE', *, *, #55588, .F. ) ;
#44497 = CARTESIAN_POINT ( 'NONE',  ( 96.15314808468748708, 88.00268892867053694, 87.94947916753380923 ) ) ;
#44498 = ORIENTED_EDGE ( 'NONE', *, *, #67109, .F. ) ;
#44499 = CARTESIAN_POINT ( 'NONE',  ( 96.15314808468750130, -211.9973110713294489, 85.40947916753380298 ) ) ;
#44500 = LINE ( 'NONE', #56138, #57135 ) ;
#44501 = DIRECTION ( 'NONE',  ( 1.000000000000000000, 0.000000000000000000, 0.000000000000000000 ) ) ;
#44502 = DIRECTION ( 'NONE',  ( 0.000000000000000000, -0.9135454576426050854, -0.4067366430757908824 ) ) ;
#44503 = CARTESIAN_POINT ( 'NONE',  ( 10.00000000000000000, 70.53064760720278059, 26.01480285779964774 ) ) ;
#44504 = CARTESIAN_POINT ( 'NONE',  ( -12.83284365640956182, 0.000000000000000000, 0.000000000000000000 ) ) ;
#44505 = CARTESIAN_POINT ( 'NONE',  ( 11.99999999999999822, -62.50329211542407393, -41.76937507738853839 ) ) ;
#44506 = CARTESIAN_POINT ( 'NONE',  ( -92.69370383062498320, -208.6684592857803011, 88.74322916753379786 ) ) ;
#44507 = EDGE_CURVE ( 'NONE', #23563, #25482, #51614, .T. ) ;
#44508 = CARTESIAN_POINT ( 'NONE',  ( -95.00000000000002842, 87.33691857156074434, 87.42031250086715488 ) ) ;
#44509 = EDGE_CURVE ( 'NONE', #34480, #32553, #71998, .T. ) ;
#44510 = ORIENTED_EDGE ( 'NONE', *, *, #12415, .T. ) ;
#44512 = CARTESIAN_POINT ( 'NONE',  ( -97.30629616937501680, 90.00000000000004263, 86.46781250086714010 ) ) ;
#44511 = CARTESIAN_POINT ( 'NONE',  ( 92.69370383062498320, 88.66845928578037217, 88.42572916753380241 ) ) ;
#44513 = ORIENTED_EDGE ( 'NONE', *, *, #15809, .T. ) ;
#44514 = DIRECTION ( 'NONE',  ( -1.000000000000000000, 0.000000000000000000, 0.000000000000000000 ) ) ;
#44515 = DIRECTION ( 'NONE',  ( 1.000000000000000000, 0.000000000000000000, 0.000000000000000000 ) ) ;
#44516 = DIRECTION ( 'NONE',  ( -1.000000000000000000, 0.000000000000000000, -0.000000000000000000 ) ) ;
#44517 = DIRECTION ( 'NONE',  ( -1.000000000000000000, 0.000000000000000000, 0.000000000000000000 ) ) ;
#44518 = CARTESIAN_POINT ( 'NONE',  ( -93.67500000000003979, 92.29496732002878900, 86.61333333333332973 ) ) ;
#44519 = CARTESIAN_POINT ( 'NONE',  ( 95.00000000000000000, -206.9400435732949575, 82.22124999999999773 ) ) ;
#44520 = AXIS2_PLACEMENT_3D ( 'NONE', #63051, #51362, #51742 ) ;
#44521 = CARTESIAN_POINT ( 'NONE',  ( 11.99999999999999822, 0.8261519478441983200, -77.49459641780885022 ) ) ;
#44522 = CARTESIAN_POINT ( 'NONE',  ( 94.99999999999998579, 86.94004357329502852, 89.52374999999999261 ) ) ;
#44523 = EDGE_LOOP ( 'NONE', ( #47293, #39114, #62449, #5024 ) ) ;
#44524 = EDGE_LOOP ( 'NONE', ( #2452, #4071, #29554, #71726 ) ) ;
#44525 = CARTESIAN_POINT ( 'NONE',  ( -93.67500000000003979, 92.29496732002878900, 80.89833333333332632 ) ) ;
#44526 = CARTESIAN_POINT ( 'NONE',  ( 12.00000000000000000, -19.89357724624986901, 12.59942793731086219 ) ) ;
#44527 = CARTESIAN_POINT ( 'NONE',  ( -20.63749999999999574, -2.946905753440916183E-14, -1.643265707205091412E-14 ) ) ;
#44528 = DIRECTION ( 'NONE',  ( 1.000000000000000000, 0.000000000000000000, 0.000000000000000000 ) ) ;
#44529 = DIRECTION ( 'NONE',  ( -1.000000000000000000, 0.000000000000000000, -0.000000000000000000 ) ) ;
#44530 = DIRECTION ( 'NONE',  ( -1.000000000000000000, 0.000000000000000000, -0.000000000000000000 ) ) ;
#44531 = FACE_OUTER_BOUND ( 'NONE', #19638, .T. ) ;
#44532 = DIRECTION ( 'NONE',  ( 0.000000000000000000, 0.000000000000000000, 1.000000000000000000 ) ) ;
#44533 = VERTEX_POINT ( 'NONE', #22168 ) ;
#44534 = CARTESIAN_POINT ( 'NONE',  ( -96.15314808468751551, 88.00268892867056536, 83.39864583420047950 ) ) ;
#44535 = AXIS2_PLACEMENT_3D ( 'NONE', #73631, #40185, #33794 ) ;
#44536 = DIRECTION ( 'NONE',  ( -2.603472992746261562E-14, -2.546204323184492723E-14, 1.000000000000000000 ) ) ;
#44537 = CIRCLE ( 'NONE', #43365, 82.00000000000000000 ) ;
#44538 = CARTESIAN_POINT ( 'NONE',  ( -92.35000000000015064, 88.47002178664750716, 85.81958333333332689 ) ) ;
#44539 = AXIS2_PLACEMENT_3D ( 'NONE', #56806, #61336, #5681 ) ;
#44540 = CARTESIAN_POINT ( 'NONE',  ( 11.99999999999999822, 0.000000000000000000, 0.000000000000000000 ) ) ;
#44541 = CARTESIAN_POINT ( 'NONE',  ( 89.99999999999998579, 85.00000000000002842, 90.00000000000000000 ) ) ;
#44542 = CARTESIAN_POINT ( 'NONE',  ( -3.000000000000000000, 16.83928648764923253, 16.46020748918050458 ) ) ;
#44543 =( NAMED_UNIT ( * ) PLANE_ANGLE_UNIT ( ) SI_UNIT ( $, .RADIAN. ) );
#44544 = CIRCLE ( 'NONE', #51768, 32.00000000000000000 ) ;
#44545 =( BOUNDED_CURVE ( )  B_SPLINE_CURVE ( 2, ( #11212, #67988, #63112, #34140, #57087, #22880, #68740 ),
 .UNSPECIFIED., .F., .F. ) 
 B_SPLINE_CURVE_WITH_KNOTS ( ( 3, 2, 2, 3 ),
 ( 0.7916666666666669627, 0.7986111111111114935, 0.8055555555555558023, 0.8125000000000002220 ),
 .UNSPECIFIED. ) 
 CURVE ( )  GEOMETRIC_REPRESENTATION_ITEM ( )  RATIONAL_B_SPLINE_CURVE ( ( 0.9999999999999935607, 0.8660254037844451469, 1.000000000000000000, 0.8660254037844387076, 1.000000000000000000, 0.8660254037844343777, 1.000000000000004219 ) ) 
 REPRESENTATION_ITEM ( '' )  );
#44546 = CARTESIAN_POINT ( 'NONE',  ( 10.00000000000000000, 75.11764819372149304, -2.946379043146603482 ) ) ;
#44547 = EDGE_CURVE ( 'NONE', #48910, #61428, #62413, .T. ) ;
#44548 = CARTESIAN_POINT ( 'NONE',  ( 94.99999999999998579, 92.66308142843932671, 80.75281250086716511 ) ) ;
#44549 = CARTESIAN_POINT ( 'NONE',  ( -94.99999999999997158, -207.3369185715606307, 84.56281250086716739 ) ) ;
#44550 = DIRECTION ( 'NONE',  ( -1.000000000000000000, 0.000000000000000000, -0.000000000000000000 ) ) ;
#44551 = ORIENTED_EDGE ( 'NONE', *, *, #20343, .T. ) ;
#44552 = CARTESIAN_POINT ( 'NONE',  ( -97.65000000000001990, 91.52997821335253548, 83.04145833506764518 ) ) ;
#44553 = CARTESIAN_POINT ( 'NONE',  ( -94.99999999999997158, -213.0599564267049857, 78.72875000000001933 ) ) ;
#44554 = DIRECTION ( 'NONE',  ( -1.000000000000000000, -0.000000000000000000, 0.000000000000000000 ) ) ;
#44555 = EDGE_CURVE ( 'NONE', #16009, #56786, #8194, .T. ) ;
#44556 = CARTESIAN_POINT ( 'NONE',  ( -95.00000000000002842, 92.66308142843932671, 78.84781250086714977 ) ) ;
#44557 = CARTESIAN_POINT ( 'NONE',  ( 95.00000000000000000, -212.6630814284392557, 80.91156250086714863 ) ) ;
#44558 = ORIENTED_EDGE ( 'NONE', *, *, #59741, .T. ) ;
#44559 = EDGE_CURVE ( 'NONE', #61302, #53203, #28813, .T. ) ;
#44560 = ORIENTED_EDGE ( 'NONE', *, *, #11899, .T. ) ;
#44561 = CARTESIAN_POINT ( 'NONE',  ( 10.00000000000000000, 0.000000000000000000, 0.000000000000000000 ) ) ;
#44562 = VERTEX_POINT ( 'NONE', #63885 ) ;
#44563 = EDGE_CURVE ( 'NONE', #9702, #46802, #2235, .T. ) ;
#44564 = EDGE_CURVE ( 'NONE', #20634, #70074, #52580, .T. ) ;
#44565 = VECTOR ( 'NONE', #67181, 1000.000000000000000 ) ;
#44566 = VECTOR ( 'NONE', #41914, 1000.000000000000000 ) ;
#44568 = AXIS2_PLACEMENT_3D ( 'NONE', #2029, #24914, #36556 ) ;
#44567 = DIRECTION ( 'NONE',  ( 1.000000000000000000, 0.000000000000000000, 0.000000000000000000 ) ) ;
#44569 = ORIENTED_EDGE ( 'NONE', *, *, #33938, .F. ) ;
#44570 = VERTEX_POINT ( 'NONE', #13466 ) ;
#44571 = ORIENTED_EDGE ( 'NONE', *, *, #33105, .F. ) ;
#44572 = LINE ( 'NONE', #55842, #53961 ) ;
#44573 = ORIENTED_EDGE ( 'NONE', *, *, #26377, .T. ) ;
#44574 = APPLICATION_CONTEXT ( 'automotive_design' ) ;
#44575 = CARTESIAN_POINT ( 'NONE',  ( 5.000000000000000000, 2.886751345948125991, -6.000000000000000000 ) ) ;
#44576 = CARTESIAN_POINT ( 'NONE',  ( 97.65000000000006253, -211.5299782133524218, 83.91458333333333997 ) ) ;
#44577 = CARTESIAN_POINT ( 'NONE',  ( 94.99999999999998579, 87.33691857156068750, 86.15031250086714465 ) ) ;
#44578 = ADVANCED_FACE ( 'NONE', ( #18365, #12721 ), #70594, .T. ) ;
#44579 = CARTESIAN_POINT ( 'NONE',  ( 97.65000000000000568, 88.47002178664752137, 80.81895833506763438 ) ) ;
#44580 = CARTESIAN_POINT ( 'NONE',  ( 92.35000000000002274, -208.4700217866474645, 79.15208333333332291 ) ) ;
#44581 = ORIENTED_EDGE ( 'NONE', *, *, #22646, .T. ) ;
#44582 = ORIENTED_EDGE ( 'NONE', *, *, #12730, .F. ) ;
#44583 = ORIENTED_EDGE ( 'NONE', *, *, #74106, .F. ) ;
#44584 = ORIENTED_EDGE ( 'NONE', *, *, #55860, .F. ) ;
#44585 = CARTESIAN_POINT ( 'NONE',  ( 0.000000000000000000, 0.000000000000000000, 0.000000000000000000 ) ) ;
#44586 = VECTOR ( 'NONE', #31644, 1000.000000000000114 ) ;
#44587 = CIRCLE ( 'NONE', #36141, 12.49999999999999645 ) ;
#44588 = SHAPE_REPRESENTATION_RELATIONSHIP ( 'NONE' , 'NONE' ,  #50888, #52570 ) ;
#44589 = DIRECTION ( 'NONE',  ( -0.000000000000000000, -0.000000000000000000, 1.000000000000000000 ) ) ;
#44590 = DIRECTION ( 'NONE',  ( -1.000000000000000000, -0.000000000000000000, -0.000000000000000000 ) ) ;
#44591 = AXIS2_PLACEMENT_3D ( 'NONE', #31763, #66006, #66372 ) ;
#44592 = CARTESIAN_POINT ( 'NONE',  ( 10.00000000000000000, 0.000000000000000000, 0.000000000000000000 ) ) ;
#44593 = CYLINDRICAL_SURFACE ( 'NONE', #11944, 2.649999999999985700 ) ;
#44594 = DIRECTION ( 'NONE',  ( 0.000000000000000000, -1.065814103640131662E-14, -1.000000000000000000 ) ) ;
#44595 = ORIENTED_EDGE ( 'NONE', *, *, #59825, .F. ) ;
#44596 = CARTESIAN_POINT ( 'NONE',  ( -94.99999999999997158, -213.0599564267049857, 82.61812500173428475 ) ) ;
#44598 = ORIENTED_EDGE ( 'NONE', *, *, #45607, .T. ) ;
#44597 = EDGE_CURVE ( 'NONE', #40423, #46611, #18730, .T. ) ;
#44599 = DIRECTION ( 'NONE',  ( -1.000000000000000000, 0.000000000000000000, -0.000000000000000000 ) ) ;
#44600 = ORIENTED_EDGE ( 'NONE', *, *, #23923, .F. ) ;
#44602 = CARTESIAN_POINT ( 'NONE',  ( -96.32500000000001705, 87.70503267997129626, 83.20020833506764291 ) ) ;
#44601 = CARTESIAN_POINT ( 'NONE',  ( 97.64999999999997726, 88.47002178664753558, 82.72395833506762131 ) ) ;
#44603 = AXIS2_PLACEMENT_3D ( 'NONE', #38341, #20676, #15780 ) ;
#44605 = EDGE_CURVE ( 'NONE', #33726, #2166, #59715, .T. ) ;
#44604 = VERTEX_POINT ( 'NONE', #13825 ) ;
#44606 = CARTESIAN_POINT ( 'NONE',  ( 97.30629616937498838, 88.66845928578037217, 83.08114583420048405 ) ) ;
#44607 = CARTESIAN_POINT ( 'NONE',  ( -96.32500000000001705, 87.70503267997129626, 76.13583333333333769 ) ) ;
#44608 = CARTESIAN_POINT ( 'NONE',  ( -97.64999999999996305, -209.9999999999999716, 82.45937500173430124 ) ) ;
#44609 = CYLINDRICAL_SURFACE ( 'NONE', #26584, 31.99999999999998579 ) ;
#44610 = CARTESIAN_POINT ( 'NONE',  ( 4.999999999999999112, 16.65560815589411092, 38.55633173627015253 ) ) ;
#44611 = LINE ( 'NONE', #73897, #70894 ) ;
#44612 = ORIENTED_EDGE ( 'NONE', *, *, #44164, .F. ) ;
#44613 = CYLINDRICAL_SURFACE ( 'NONE', #62737, 77.49899999999999523 ) ;
#44614 = CARTESIAN_POINT ( 'NONE',  ( 13.36581099891334645, -139.3288669181958710, -2.500000000000000000 ) ) ;
#44615 = LINE ( 'NONE', #34057, #68422 ) ;
#44616 = ORIENTED_EDGE ( 'NONE', *, *, #48876, .F. ) ;
#44617 = VERTEX_POINT ( 'NONE', #46954 ) ;
#44618 = PRODUCT_DEFINITION_SHAPE ( 'NONE', 'NONE',  #52691 ) ;
#44619 = CARTESIAN_POINT ( 'NONE',  ( 10.00000000000000000, 79.10210256391397365, -21.60688246758502373 ) ) ;
#44620 = CARTESIAN_POINT ( 'NONE',  ( -93.67500000000003979, 87.70503267997129626, 80.13104166840095388 ) ) ;
#44621 = CARTESIAN_POINT ( 'NONE',  ( -92.35000000000000853, -209.9999996502046429, 77.69687501385436690 ) ) ;
#44622 = CARTESIAN_POINT ( 'NONE',  ( -94.99999999999997158, -207.3369185715606307, 81.38781250086715602 ) ) ;
#44623 = ORIENTED_EDGE ( 'NONE', *, *, #30134, .T. ) ;
#44624 = DIRECTION ( 'NONE',  ( 1.000000000000000000, 0.000000000000000000, 0.000000000000000000 ) ) ;
#44625 = VERTEX_POINT ( 'NONE', #52961 ) ;
#44626 = AXIS2_PLACEMENT_3D ( 'NONE', #8352, #19986, #42941 ) ;
#44627 = DIRECTION ( 'NONE',  ( 1.000000000000000000, 0.000000000000000000, 0.000000000000000000 ) ) ;
#44628 = AXIS2_PLACEMENT_3D ( 'NONE', #66088, #15680, #61550 ) ;
#44629 = CARTESIAN_POINT ( 'NONE',  ( 97.65000000000000568, 88.47002178664752137, 82.08895833506764461 ) ) ;
#44630 = CIRCLE ( 'NONE', #63847, 32.00000000000000000 ) ;
#44631 = FACE_OUTER_BOUND ( 'NONE', #12275, .T. ) ;
#44632 = CARTESIAN_POINT ( 'NONE',  ( 97.30629616937498838, 88.66845928578035796, 77.20739583420046870 ) ) ;
#44633 = CYLINDRICAL_SURFACE ( 'NONE', #35289, 37.49900000000000233 ) ;
#44634 = LINE ( 'NONE', #9286, #73412 ) ;
#44635 = CARTESIAN_POINT ( 'NONE',  ( 0.000000000000000000, 0.000000000000000000, 0.000000000000000000 ) ) ;
#44636 = CARTESIAN_POINT ( 'NONE',  ( -92.35000000000395914, -210.0000045800647115, 76.42687486209126746 ) ) ;
#44637 = CARTESIAN_POINT ( 'NONE',  ( 0.000000000000000000, 17.80606268964585226, -33.00180498840028775 ) ) ;
#44638 = CARTESIAN_POINT ( 'NONE',  ( -42.50000000000000000, 0.000000000000000000, 0.000000000000000000 ) ) ;
#44639 = AXIS2_PLACEMENT_3D ( 'NONE', #39708, #4386, #33293 ) ;
#44640 =( BOUNDED_CURVE ( )  B_SPLINE_CURVE ( 2, ( #48375, #14156, #3652, #26177, #48744, #3288, #32183 ),
 .UNSPECIFIED., .F., .F. ) 
 B_SPLINE_CURVE_WITH_KNOTS ( ( 3, 2, 2, 3 ),
 ( 0.3598440426530882807, 0.3668998081258831867, 0.3739555736667656283, 0.3810111478265171270 ),
 .UNSPECIFIED. ) 
 CURVE ( )  GEOMETRIC_REPRESENTATION_ITEM ( )  RATIONAL_B_SPLINE_CURVE ( ( 1.000000000000000000, 0.8660254037844387076, 1.000000000000000000, 0.8660254037844387076, 1.000000000000000000, 0.8660290377217593205, 0.9999927323224930831 ) ) 
 REPRESENTATION_ITEM ( '' )  );
#44641 = DIRECTION ( 'NONE',  ( -0.000000000000000000, -0.9135454576426058626, -0.4067366430757889395 ) ) ;
#44642 = CARTESIAN_POINT ( 'NONE',  ( 92.69370383062498320, 91.33154071421968467, 89.11364583420049712 ) ) ;
#44643 = CARTESIAN_POINT ( 'NONE',  ( -30.50000000000000000, -120.0000000000000000, 5.500000000000000888 ) ) ;
#44644 = CARTESIAN_POINT ( 'NONE',  ( 94.99999999999998579, 93.05995642670504253, 89.20624999999999716 ) ) ;
#44646 = EDGE_CURVE ( 'NONE', #31921, #18187, #70975, .T. ) ;
#44645 = ORIENTED_EDGE ( 'NONE', *, *, #71042, .T. ) ;
#44647 = CARTESIAN_POINT ( 'NONE',  ( -93.84685191531252713, 88.00268892867056536, 84.13947916753380696 ) ) ;
#44648 = AXIS2_PLACEMENT_3D ( 'NONE', #28597, #55189, #50277 ) ;
#44649 = CARTESIAN_POINT ( 'NONE',  ( 5.999999999999999112, 46.11716303203186840, 67.80270845531904911 ) ) ;
#44650 = VECTOR ( 'NONE', #14524, 999.9999999999998863 ) ;
#44651 = AXIS2_PLACEMENT_3D ( 'NONE', #20858, #2870, #43814 ) ;
#44652 = EDGE_CURVE ( 'NONE', #10620, #37614, #38417, .T. ) ;
#44653 = CARTESIAN_POINT ( 'NONE',  ( 92.35000000000000853, -209.9999999999999716, 90.00000000000000000 ) ) ;
#44654 = EDGE_CURVE ( 'NONE', #64184, #61415, #23647, .T. ) ;
#44655 = ORIENTED_EDGE ( 'NONE', *, *, #4077, .T. ) ;
#44656 = DIRECTION ( 'NONE',  ( -1.000000000000000000, -0.000000000000000000, -0.000000000000000000 ) ) ;
#44657 = DIRECTION ( 'NONE',  ( -1.000000000000000000, 0.000000000000000000, 0.000000000000000000 ) ) ;
#44658 = CARTESIAN_POINT ( 'NONE',  ( 10.00000000000000000, 16.45098606841126454, 33.79645857604518966 ) ) ;
#44659 = EDGE_CURVE ( 'NONE', #70889, #42280, #36393, .T. ) ;
#44660 = LINE ( 'NONE', #22084, #59960 ) ;
#44661 = CARTESIAN_POINT ( 'NONE',  ( 92.69370383062501162, -211.3315407142195852, 80.32947916753381890 ) ) ;
#44662 = EDGE_LOOP ( 'NONE', ( #47595, #37464, #2912, #33254 ) ) ;
#44663 = ORIENTED_EDGE ( 'NONE', *, *, #38442, .F. ) ;
#44664 = CARTESIAN_POINT ( 'NONE',  ( -97.64998530214792538, -208.4700133008386445, 81.77145774807794965 ) ) ;
#44665 = EDGE_CURVE ( 'NONE', #4451, #40893, #45295, .T. ) ;
#44666 = CARTESIAN_POINT ( 'NONE',  ( 10.00000000000000000, 0.000000000000000000, 0.000000000000000000 ) ) ;
#44667 = DIRECTION ( 'NONE',  ( -1.000000000000000000, 3.061616997868383141E-16, 0.000000000000000000 ) ) ;
#44668 = CARTESIAN_POINT ( 'NONE',  ( 10.00000000000000000, 0.000000000000000000, 0.000000000000000000 ) ) ;
#44669 = EDGE_CURVE ( 'NONE', #4640, #17707, #68427, .T. ) ;
#44670 = DIRECTION ( 'NONE',  ( -0.000000000000000000, -0.000000000000000000, -1.000000000000000000 ) ) ;
#44671 = CARTESIAN_POINT ( 'NONE',  ( 92.35000000000002274, -211.5299782133524502, 86.87791666666664980 ) ) ;
#44672 = AXIS2_PLACEMENT_3D ( 'NONE', #34902, #74000, #46549 ) ;
#44673 = ORIENTED_EDGE ( 'NONE', *, *, #22417, .T. ) ;
#44674 = CARTESIAN_POINT ( 'NONE',  ( -97.64999999999996305, -209.9999999999999716, 88.09499999999999886 ) ) ;
#44675 = EDGE_LOOP ( 'NONE', ( #47900, #45268, #35265, #6810 ) ) ;
#44676 = VERTEX_POINT ( 'NONE', #30009 ) ;
#44677 = FACE_OUTER_BOUND ( 'NONE', #44524, .T. ) ;
#44678 =( LENGTH_UNIT ( ) NAMED_UNIT ( * ) SI_UNIT ( .MILLI., .METRE. ) );
#44679 = FACE_OUTER_BOUND ( 'NONE', #57920, .T. ) ;
#44680 = ORIENTED_EDGE ( 'NONE', *, *, #53988, .F. ) ;
#44681 = CARTESIAN_POINT ( 'NONE',  ( 93.67500000000001137, -207.7050326799711968, 78.54354166840096241 ) ) ;
#44682 = CARTESIAN_POINT ( 'NONE',  ( 92.35000000000002274, -211.5299782133524502, 80.60729166840097548 ) ) ;
#44683 = CARTESIAN_POINT ( 'NONE',  ( 93.67499999999998295, 92.29496732002878900, 81.63916666666666799 ) ) ;
#44684 = ORIENTED_EDGE ( 'NONE', *, *, #15374, .T. ) ;
#44685 = LINE ( 'NONE', #67602, #55147 ) ;
#44686 = ORIENTED_EDGE ( 'NONE', *, *, #58091, .F. ) ;
#44687 = EDGE_CURVE ( 'NONE', #36429, #21975, #39604, .T. ) ;
#44688 = LINE ( 'NONE', #16096, #62698 ) ;
#44689 = ORIENTED_EDGE ( 'NONE', *, *, #16403, .F. ) ;
#44690 = FACE_OUTER_BOUND ( 'NONE', #21428, .T. ) ;
#44691 = AXIS2_PLACEMENT_3D ( 'NONE', #13322, #58826, #6225 ) ;
#44692 = CARTESIAN_POINT ( 'NONE',  ( -96.15314808468752972, 91.99731107132950569, 85.25072916753381946 ) ) ;
#44693 = CARTESIAN_POINT ( 'NONE',  ( 96.15314808468748708, 91.99731107132950569, 78.63614583420047666 ) ) ;
#44694 = ORIENTED_EDGE ( 'NONE', *, *, #51838, .F. ) ;
#44695 = DIRECTION ( 'NONE',  ( -1.000000000000000000, -0.000000000000000000, 0.000000000000000000 ) ) ;
#44696 = CARTESIAN_POINT ( 'NONE',  ( -92.35000000000312070, 89.99999595380251094, 77.06187486178039592 ) ) ;
#44697 = CYLINDRICAL_SURFACE ( 'NONE', #16186, 77.49899999999999523 ) ;
#44698 = DIRECTION ( 'NONE',  ( 0.000000000000000000, 0.000000000000000000, 1.000000000000000000 ) ) ;
#44699 = VERTEX_POINT ( 'NONE', #12356 ) ;
#44700 = FACE_OUTER_BOUND ( 'NONE', #70921, .T. ) ;
#44701 = AXIS2_PLACEMENT_3D ( 'NONE', #25049, #54003, #14122 ) ;
#44702 = VECTOR ( 'NONE', #71128, 1000.000000000000000 ) ;
#44703 = CARTESIAN_POINT ( 'NONE',  ( -97.30629616937495996, -209.9999999999999716, 81.38781250086714181 ) ) ;
#44704 = VERTEX_POINT ( 'NONE', #53693 ) ;
#44705 = ORIENTED_EDGE ( 'NONE', *, *, #8766, .T. ) ;
#44706 = DIRECTION ( 'NONE',  ( 0.000000000000000000, -0.8526401643540970632, 0.5224985647159409163 ) ) ;
#44707 = ORIENTED_EDGE ( 'NONE', *, *, #8831, .T. ) ;
#44708 = DIRECTION ( 'NONE',  ( -1.000000000000000000, -0.000000000000000000, -0.000000000000000000 ) ) ;
#44709 = CARTESIAN_POINT ( 'NONE',  ( 97.64999999999989200, 88.47002178664749295, 80.73958333333335702 ) ) ;
#44710 = ORIENTED_EDGE ( 'NONE', *, *, #38369, .F. ) ;
#44711 = CARTESIAN_POINT ( 'NONE',  ( -96.15314808468747287, -208.0026889286704943, 76.83697916753381207 ) ) ;
#44712 = VERTEX_POINT ( 'NONE', #19474 ) ;
#44713 = LINE ( 'NONE', #43962, #6258 ) ;
#44714 = DIRECTION ( 'NONE',  ( 1.000000000000000000, 0.000000000000000000, 0.000000000000000000 ) ) ;
#44715 = CARTESIAN_POINT ( 'NONE',  ( 97.64999999999999147, 90.00000000000002842, 89.12687500173430521 ) ) ;
#44716 = DIRECTION ( 'NONE',  ( 0.000000000000000000, 0.000000000000000000, 1.000000000000000000 ) ) ;
#44717 = CARTESIAN_POINT ( 'NONE',  ( -8.637688417678527131, 13.69818742750669394, 52.00000000000002132 ) ) ;
#44718 = UNCERTAINTY_MEASURE_WITH_UNIT (LENGTH_MEASURE( 1.000000000000000082E-05 ), #66125, 'distance_accuracy_value', 'NONE');
#44719 = CARTESIAN_POINT ( 'NONE',  ( 10.00000000000000000, -37.48860685352291711, 0.8828120875899322373 ) ) ;
#44720 = CARTESIAN_POINT ( 'NONE',  ( 97.30629616937498838, 88.66845928578035796, 88.63739583420047552 ) ) ;
#44721 = DIRECTION ( 'NONE',  ( 3.061616997868382648E-16, 1.000000000000000000, 0.000000000000000000 ) ) ;
#44722 = CARTESIAN_POINT ( 'NONE',  ( 0.000000000000000000, 0.000000000000000000, 0.000000000000000000 ) ) ;
#44723 = CARTESIAN_POINT ( 'NONE',  ( 10.00000000000000000, -36.88895765772628010, -6.736453364083947015 ) ) ;
#44724 = CARTESIAN_POINT ( 'NONE',  ( 92.35000000019410038, 89.99998015720535705, 86.27002759516707897 ) ) ;
#44725 = DIRECTION ( 'NONE',  ( -0.000000000000000000, -0.000000000000000000, 1.000000000000000000 ) ) ;
#44726 = CARTESIAN_POINT ( 'NONE',  ( -19.90058851926621131, -132.5883508287165853, 5.500000000000000000 ) ) ;
#44727 = DIRECTION ( 'NONE',  ( 0.8541291221503261033, -0.5200609990133016058, 0.000000000000000000 ) ) ;
#44728 = CARTESIAN_POINT ( 'NONE',  ( 0.000000000000000000, 0.000000000000000000, 0.000000000000000000 ) ) ;
#44729 = EDGE_CURVE ( 'NONE', #50232, #41327, #71612, .T. ) ;
#44730 =( GEOMETRIC_REPRESENTATION_CONTEXT ( 3 ) GLOBAL_UNCERTAINTY_ASSIGNED_CONTEXT ( ( #44718 ) ) GLOBAL_UNIT_ASSIGNED_CONTEXT ( ( #66125, #71729, #8965 ) ) REPRESENTATION_CONTEXT ( 'NONE', 'WORKASPACE' ) );
#44731 = CARTESIAN_POINT ( 'NONE',  ( 10.00000000000000000, 73.72996012237460661, -14.67089635893632504 ) ) ;
#44732 = DIRECTION ( 'NONE',  ( 0.000000000000000000, 0.3090169943749410120, 0.9510565162951557516 ) ) ;
#44733 = CARTESIAN_POINT ( 'NONE',  ( 10.00000000000000000, 0.000000000000000000, 0.000000000000000000 ) ) ;
#44734 = EDGE_CURVE ( 'NONE', #69518, #55377, #55548, .T. ) ;
#44735 = CARTESIAN_POINT ( 'NONE',  ( -96.32499999999996021, -207.7050326799711968, 86.08416666666666117 ) ) ;
#44736 = EDGE_CURVE ( 'NONE', #24497, #7244, #60822, .T. ) ;
#44737 = ADVANCED_FACE ( 'NONE', ( #20957 ), #49893, .T. ) ;
#44738 = AXIS2_PLACEMENT_3D ( 'NONE', #28324, #27593, #38508 ) ;
#44739 = CARTESIAN_POINT ( 'NONE',  ( -94.26002770235261607, 87.43182282693500440, 75.00000000000000000 ) ) ;
#44740 = EDGE_CURVE ( 'NONE', #27990, #62190, #26597, .T. ) ;
#44741 = DIRECTION ( 'NONE',  ( 0.000000000000000000, 0.000000000000000000, 1.000000000000000000 ) ) ;
#44742 = DIRECTION ( 'NONE',  ( -1.000000000000000000, 0.000000000000000000, 0.000000000000000000 ) ) ;
#44743 = CARTESIAN_POINT ( 'NONE',  ( 0.000000000000000000, 0.000000000000000000, 0.000000000000000000 ) ) ;
#44744 = ADVANCED_FACE ( 'NONE', ( #54076 ), #26961, .T. ) ;
#44745 = AXIS2_PLACEMENT_3D ( 'NONE', #24453, #17066, #39997 ) ;
#44746 = VECTOR ( 'NONE', #70293, 1000.000000000000000 ) ;
#44747 = CARTESIAN_POINT ( 'NONE',  ( 97.30629616937498838, -211.3315407142195852, 87.52614583420049144 ) ) ;
#44748 = VERTEX_POINT ( 'NONE', #71333 ) ;
#44749 = EDGE_LOOP ( 'NONE', ( #48843, #18065, #70704, #71675 ) ) ;
#44750 = DIRECTION ( 'NONE',  ( -1.000000000000000000, -0.000000000000000000, -0.000000000000000000 ) ) ;
#44751 = ORIENTED_EDGE ( 'NONE', *, *, #1486, .T. ) ;
#44752 = DIRECTION ( 'NONE',  ( -0.000000000000000000, -0.000000000000000000, 1.000000000000000000 ) ) ;
#44753 = CARTESIAN_POINT ( 'NONE',  ( 95.00000000000000000, -212.6630814284392557, 79.64156250086713840 ) ) ;
#44755 = VERTEX_POINT ( 'NONE', #61568 ) ;
#44754 = ADVANCED_FACE ( 'NONE', ( #43910 ), #15315, .T. ) ;
#44756 = CARTESIAN_POINT ( 'NONE',  ( 92.69370383062501162, -211.3315407142195852, 82.86947916753382515 ) ) ;
#44757 = ORIENTED_EDGE ( 'NONE', *, *, #49306, .F. ) ;
#44758 = DIRECTION ( 'NONE',  ( 0.000000000000000000, -0.5877852522924689183, -0.8090169943749504489 ) ) ;
#44759 = EDGE_LOOP ( 'NONE', ( #21567, #38745, #53710, #27245 ) ) ;
#44760 = EDGE_CURVE ( 'NONE', #7655, #7152, #70812, .T. ) ;
#44761 = EDGE_CURVE ( 'NONE', #30109, #47902, #58808, .T. ) ;
#44762 = CARTESIAN_POINT ( 'NONE',  ( 0.000000000000000000, 81.96053171279902472, -2.543863470248677316 ) ) ;
#44763 = ORIENTED_EDGE ( 'NONE', *, *, #3695, .F. ) ;
#44764 = DIRECTION ( 'NONE',  ( -0.000000000000000000, -0.000000000000000000, 1.000000000000000000 ) ) ;
#44765 = ORIENTED_EDGE ( 'NONE', *, *, #4695, .F. ) ;
#44766 = DIRECTION ( 'NONE',  ( -0.000000000000000000, -0.000000000000000000, 1.000000000000000000 ) ) ;
#44767 = CARTESIAN_POINT ( 'NONE',  ( 1.560000000000000053, 1.299038105676658228, -0.7500000000000009992 ) ) ;
#44768 = ORIENTED_EDGE ( 'NONE', *, *, #34103, .F. ) ;
#44769 = CARTESIAN_POINT ( 'NONE',  ( 10.00000000000000178, 0.000000000000000000, 0.000000000000000000 ) ) ;
#44770 = EDGE_CURVE ( 'NONE', #35604, #2536, #46793, .T. ) ;
#44771 = EDGE_LOOP ( 'NONE', ( #7851, #58521, #51983, #36602 ) ) ;
#44772 = DIRECTION ( 'NONE',  ( 0.000000000000000000, 0.000000000000000000, 1.000000000000000000 ) ) ;
#44773 = VERTEX_POINT ( 'NONE', #31863 ) ;
#44774 = STYLED_ITEM ( 'NONE', ( #71649 ), #72270 ) ;
#44775 = VERTEX_POINT ( 'NONE', #4064 ) ;
#44776 = VERTEX_POINT ( 'NONE', #14578 ) ;
#44777 = CARTESIAN_POINT ( 'NONE',  ( -2.712167343862821323, -4.207632145829752979, -6.000000000000000888 ) ) ;
#44778 = ITEM_DEFINED_TRANSFORMATION ( 'NONE', 'NONE', #55609,  #43395 ) ;
#44779 = CARTESIAN_POINT ( 'NONE',  ( 10.00000000000000000, -3.894527615418464705, 81.90746397400387480 ) ) ;
#44780 = VERTEX_POINT ( 'NONE', #44273 ) ;
#44781 = VECTOR ( 'NONE', #63339, 1000.000000000000000 ) ;
#44782 = ORIENTED_EDGE ( 'NONE', *, *, #31230, .T. ) ;
#44783 = EDGE_LOOP ( 'NONE', ( #32078, #2183, #45870, #33063 ) ) ;
#44784 = CARTESIAN_POINT ( 'NONE',  ( -97.64999999999996305, -209.9999999999999716, 84.28499999999999659 ) ) ;
#44785 = CARTESIAN_POINT ( 'NONE',  ( 0.000000000000000000, 26.02418014898407961, -70.52718814184231633 ) ) ;
#44786 = CARTESIAN_POINT ( 'NONE',  ( -92.69370383062502583, 91.33154071421968467, 75.56697916753383026 ) ) ;
#44787 = ORIENTED_EDGE ( 'NONE', *, *, #214, .T. ) ;
#44788 = CARTESIAN_POINT ( 'NONE',  ( 94.99999999999998579, 87.33691857156068750, 77.73656250086713726 ) ) ;
#44789 = VECTOR ( 'NONE', #13394, 1000.000000000000000 ) ;
#44790 = VERTEX_POINT ( 'NONE', #2612 ) ;
#44791 = CARTESIAN_POINT ( 'NONE',  ( 0.000000000000000000, 22.07842321921492612, -8.187992925817130896 ) ) ;
#44792 = CARTESIAN_POINT ( 'NONE',  ( -94.99999999999997158, -212.6630814284392557, 85.35656250086714181 ) ) ;
#44793 = ORIENTED_EDGE ( 'NONE', *, *, #41022, .T. ) ;
#44794 = CARTESIAN_POINT ( 'NONE',  ( 15.00000000000000000, -20.55727247249748402, -16.78983467731284307 ) ) ;
#44795 = CARTESIAN_POINT ( 'NONE',  ( 11.99999999999999822, 78.73519480814985627, -22.90783923731548199 ) ) ;
#44796 = CYLINDRICAL_SURFACE ( 'NONE', #36878, 2.649999999999999467 ) ;
#44797 = CARTESIAN_POINT ( 'NONE',  ( -97.30629616937497417, -208.6684592857803295, 78.15989583420048348 ) ) ;
#44798 = DIRECTION ( 'NONE',  ( 0.000000000000000000, 0.7604059656000322631, -0.6494480483301821039 ) ) ;
#44799 = CARTESIAN_POINT ( 'NONE',  ( 15.00000000000000000, -26.23277895567245466, 4.042438405570107918 ) ) ;
#44800 = DIRECTION ( 'NONE',  ( -1.000000000000000000, -0.000000000000000000, 0.000000000000000000 ) ) ;
#44801 = ORIENTED_EDGE ( 'NONE', *, *, #34712, .F. ) ;
#44802 = ORIENTED_EDGE ( 'NONE', *, *, #46250, .T. ) ;
#44803 = DIRECTION ( 'NONE',  ( 0.000000000000000000, 0.000000000000000000, 1.000000000000000000 ) ) ;
#44804 = CARTESIAN_POINT ( 'NONE',  ( -2.977765906491215642, 0.000000000000000000, -15.77977592589476608 ) ) ;
#44805 = LINE ( 'NONE', #39160, #35558 ) ;
#44806 = CARTESIAN_POINT ( 'NONE',  ( -97.30629616937501680, 88.66845928578038638, 80.17072916753379275 ) ) ;
#44807 = DIRECTION ( 'NONE',  ( 0.000000000000000000, 0.000000000000000000, 1.000000000000000000 ) ) ;
#44808 = CARTESIAN_POINT ( 'NONE',  ( 0.000000000000000000, 50.95692526931329525, 58.39081064771768581 ) ) ;
#44809 = VERTEX_POINT ( 'NONE', #25491 ) ;
#44810 = LINE ( 'NONE', #21867, #56982 ) ;
#44811 = ADVANCED_FACE ( 'NONE', ( #37526 ), #57642, .F. ) ;
#44812 = CYLINDRICAL_SURFACE ( 'NONE', #44850, 31.99999999999999289 ) ;
#44813 = CARTESIAN_POINT ( 'NONE',  ( 0.000000000000000000, 0.000000000000000000, 40.00000000000000000 ) ) ;
#44814 = CARTESIAN_POINT ( 'NONE',  ( 0.000000000000000000, -23.29833615347109443, 3.418703333116492438 ) ) ;
#44815 = EDGE_CURVE ( 'NONE', #34136, #57179, #3331, .T. ) ;
#44816 = CYLINDRICAL_SURFACE ( 'NONE', #70569, 82.00000000000000000 ) ;
#44817 = CARTESIAN_POINT ( 'NONE',  ( 0.000000000000000000, -21.32104025579091910, -30.84782396557241313 ) ) ;
#44818 = CARTESIAN_POINT ( 'NONE',  ( -93.84685191531247028, -211.9973110713294489, 80.48822916753381662 ) ) ;
#44819 = EDGE_CURVE ( 'NONE', #4256, #60757, #72087, .T. ) ;
#44820 = ADVANCED_FACE ( 'NONE', ( #60462 ), #37154, .T. ) ;
#44821 = DIRECTION ( 'NONE',  ( -1.000000000000000000, -0.000000000000000000, -0.000000000000000000 ) ) ;
#44822 = VECTOR ( 'NONE', #69397, 1000.000000000000114 ) ;
#44823 = VERTEX_POINT ( 'NONE', #20597 ) ;
#44824 = FACE_OUTER_BOUND ( 'NONE', #27455, .T. ) ;
#44825 = CARTESIAN_POINT ( 'NONE',  ( -97.65000000000010516, 91.52997821335249284, 88.67708333333332860 ) ) ;
#44826 = CARTESIAN_POINT ( 'NONE',  ( 11.99999999999999822, 0.000000000000000000, 0.000000000000000000 ) ) ;
#44827 = VERTEX_POINT ( 'NONE', #66466 ) ;
#44828 = AXIS2_PLACEMENT_3D ( 'NONE', #29486, #57716, #63359 ) ;
#44829 = CARTESIAN_POINT ( 'NONE',  ( 92.34999999999999432, 91.52997821335252127, 77.32645833506762756 ) ) ;
#44830 = CARTESIAN_POINT ( 'NONE',  ( 0.000000000000000000, -39.47590169984793818, -71.87247863392457248 ) ) ;
#44831 = VECTOR ( 'NONE', #32054, 1000.000000000000000 ) ;
#44832 = CARTESIAN_POINT ( 'NONE',  ( 10.00000000000000000, 0.000000000000000000, 0.000000000000000000 ) ) ;
#44833 = ADVANCED_FACE ( 'NONE', ( #9304 ), #32225, .T. ) ;
#44834 = ORIENTED_EDGE ( 'NONE', *, *, #47359, .F. ) ;
#44835 = CARTESIAN_POINT ( 'NONE',  ( 11.99999999999999822, 0.000000000000000000, 0.000000000000000000 ) ) ;
#44836 = CYLINDRICAL_SURFACE ( 'NONE', #66749, 82.00000000000000000 ) ;
#44837 = EDGE_LOOP ( 'NONE', ( #25595, #42826, #6045, #38437, #67542 ) ) ;
#44838 =( BOUNDED_CURVE ( )  B_SPLINE_CURVE ( 2, ( #29124, #52422, #68995, #41525, #6223, #53179, #12936 ),
 .UNSPECIFIED., .F., .F. ) 
 B_SPLINE_CURVE_WITH_KNOTS ( ( 3, 2, 2, 3 ),
 ( 0.1458333333333334536, 0.1527777777777778734, 0.1597222222222222654, 0.1666666666666666852 ),
 .UNSPECIFIED. ) 
 CURVE ( )  GEOMETRIC_REPRESENTATION_ITEM ( )  RATIONAL_B_SPLINE_CURVE ( ( 0.9999999999999978906, 0.8660254037844408170, 1.000000000000000000, 0.8660254037844387076, 1.000000000000000000, 0.8660254037844381525, 1.000000000000000444 ) ) 
 REPRESENTATION_ITEM ( '' )  );
#44839 = CARTESIAN_POINT ( 'NONE',  ( 97.30629616937498838, -211.3315407142195852, 87.36739583420047950 ) ) ;
#44840 = CARTESIAN_POINT ( 'NONE',  ( -97.65000000000001990, 90.00000000000004263, 77.93499999999998806 ) ) ;
#44841 = CIRCLE ( 'NONE', #43667, 12.49999999999999645 ) ;
#44842 = ORIENTED_EDGE ( 'NONE', *, *, #36575, .T. ) ;
#44843 = DIRECTION ( 'NONE',  ( -1.000000000000000000, 0.000000000000000000, 0.000000000000000000 ) ) ;
#44844 = VERTEX_POINT ( 'NONE', #62318 ) ;
#44845 = AXIS2_PLACEMENT_3D ( 'NONE', #3680, #20579, #66445 ) ;
#44846 = FACE_OUTER_BOUND ( 'NONE', #28577, .T. ) ;
#44847 = EDGE_LOOP ( 'NONE', ( #21086, #30853, #10094, #19493 ) ) ;
#44848 = VECTOR ( 'NONE', #32676, 1000.000000000000000 ) ;
#44849 = EDGE_CURVE ( 'NONE', #34228, #24727, #67229, .T. ) ;
#44851 = ADVANCED_FACE ( 'NONE', ( #23198 ), #10801, .F. ) ;
#44850 = AXIS2_PLACEMENT_3D ( 'NONE', #56083, #4602, #44446 ) ;
#44852 = DIRECTION ( 'NONE',  ( -0.000000000000000000, -0.000000000000000000, 1.000000000000000000 ) ) ;
#44853 = ORIENTED_EDGE ( 'NONE', *, *, #153, .F. ) ;
#44854 = VERTEX_POINT ( 'NONE', #16816 ) ;
#44855 = VERTEX_POINT ( 'NONE', #10051 ) ;
#44856 = CARTESIAN_POINT ( 'NONE',  ( 8.700667342345820288, -98.11853780484867116, 5.500000000000000000 ) ) ;
#44857 = EDGE_LOOP ( 'NONE', ( #15631, #60136, #10167, #44289 ) ) ;
#44858 = EDGE_LOOP ( 'NONE', ( #26703, #36517, #5790, #36409 ) ) ;
#44859 = CARTESIAN_POINT ( 'NONE',  ( 94.99999999999998579, 87.33691857156068750, 75.35531250086715715 ) ) ;
#44860 = DIRECTION ( 'NONE',  ( -1.000000000000000000, -0.000000000000000000, -0.000000000000000000 ) ) ;
#44861 = DIRECTION ( 'NONE',  ( -1.000000000000000000, 0.000000000000000000, 0.000000000000000000 ) ) ;
#44862 = ORIENTED_EDGE ( 'NONE', *, *, #35488, .F. ) ;
#44863 = ORIENTED_EDGE ( 'NONE', *, *, #38868, .T. ) ;
#44864 = ORIENTED_EDGE ( 'NONE', *, *, #6167, .F. ) ;
#44865 = CARTESIAN_POINT ( 'NONE',  ( 94.99999999999998579, 92.66308142843935514, 86.94406250086714749 ) ) ;
#44866 = ORIENTED_EDGE ( 'NONE', *, *, #71390, .T. ) ;
#44867 = CARTESIAN_POINT ( 'NONE',  ( 96.15314808468750130, -211.9973110713294489, 84.77447916753381207 ) ) ;
#44868 = PRODUCT_CONTEXT ( 'NONE', #61373, 'mechanical' ) ;
#44869 = DIRECTION ( 'NONE',  ( -1.000000000000000000, 0.000000000000000000, -0.000000000000000000 ) ) ;
#44870 = CYLINDRICAL_SURFACE ( 'NONE', #45020, 37.49900000000000233 ) ;
#44871 = DIRECTION ( 'NONE',  ( 0.000000000000000000, 0.4067366430757908824, -0.9135454576426050854 ) ) ;
#44872 = FACE_OUTER_BOUND ( 'NONE', #72304, .T. ) ;
#44873 = CYLINDRICAL_SURFACE ( 'NONE', #44431, 82.00000000000000000 ) ;
#44874 = CARTESIAN_POINT ( 'NONE',  ( -2.499999999999973355, 65.00000000000000000, -90.00000000000000000 ) ) ;
#44875 = CARTESIAN_POINT ( 'NONE',  ( -93.84685191531248449, -208.0026889286704943, 88.79614583420047325 ) ) ;
#44876 = CARTESIAN_POINT ( 'NONE',  ( -96.15314808468752972, 91.99731107132950569, 85.25072916753381946 ) ) ;
#44877 = ORIENTED_EDGE ( 'NONE', *, *, #25811, .T. ) ;
#44878 = VECTOR ( 'NONE', #49429, 1000.000000000000000 ) ;
#44880 = CARTESIAN_POINT ( 'NONE',  ( -92.69370383062504004, 90.00000000000004263, 84.88031250086713442 ) ) ;
#44879 = CARTESIAN_POINT ( 'NONE',  ( 92.69370383062498320, 90.00000000000002842, 89.00781250086714635 ) ) ;
#44881 = ORIENTED_EDGE ( 'NONE', *, *, #62869, .F. ) ;
#44882 = DIRECTION ( 'NONE',  ( -1.000000000000000000, 0.000000000000000000, 0.000000000000000000 ) ) ;
#44883 = DIRECTION ( 'NONE',  ( -1.000000000000000000, -0.000000000000000000, -0.000000000000000000 ) ) ;
#44884 = CARTESIAN_POINT ( 'NONE',  ( 2.600913415846943225E-12, -120.0000000000000000, -65.00000000000000000 ) ) ;
#44885 = CARTESIAN_POINT ( 'NONE',  ( 95.00000000000000000, -209.9999999999999716, 90.00000000000000000 ) ) ;
#44886 = CARTESIAN_POINT ( 'NONE',  ( -97.30629616937495996, -209.9999999999999716, 88.37281250086715545 ) ) ;
#44887 = VECTOR ( 'NONE', #26762, 1000.000000000000000 ) ;
#44888 = CYLINDRICAL_SURFACE ( 'NONE', #43899, 32.00000000000000000 ) ;
#44889 = CARTESIAN_POINT ( 'NONE',  ( -97.30629616937501680, 88.66845928578038638, 82.23447916753383424 ) ) ;
#44890 = FACE_OUTER_BOUND ( 'NONE', #45074, .T. ) ;
#44891 = DIRECTION ( 'NONE',  ( -1.000000000000000000, -0.000000000000000000, 0.000000000000000000 ) ) ;
#44892 = DIRECTION ( 'NONE',  ( 0.000000000000000000, 0.000000000000000000, 1.000000000000000000 ) ) ;
#44893 = EDGE_LOOP ( 'NONE', ( #56974, #31234, #59819, #32245 ) ) ;
#44894 = AXIS2_PLACEMENT_3D ( 'NONE', #62619, #33262, #55845 ) ;
#44895 = ORIENTED_EDGE ( 'NONE', *, *, #18109, .T. ) ;
#44896 = CARTESIAN_POINT ( 'NONE',  ( -96.32500000000001705, 87.70503267997129626, 81.85083333333332689 ) ) ;
#44897 = DIRECTION ( 'NONE',  ( -0.1850432970638667129, 0.9827303690289281857, 0.000000000000000000 ) ) ;
#44898 = CARTESIAN_POINT ( 'NONE',  ( -95.00000000000002842, 86.94004357329504273, 78.72875000000001933 ) ) ;
#44899 = DIRECTION ( 'NONE',  ( 0.000000000000000000, 0.000000000000000000, 1.000000000000000000 ) ) ;
#44900 = CARTESIAN_POINT ( 'NONE',  ( -97.64999999994212487, -210.0000112241608292, 75.47473230080855444 ) ) ;
#44901 = LINE ( 'NONE', #10673, #56768 ) ;
#44902 = DIRECTION ( 'NONE',  ( -1.000000000000000000, -0.000000000000000000, 0.000000000000000000 ) ) ;
#44903 = CARTESIAN_POINT ( 'NONE',  ( 0.000000000000000000, -10.96151621346514382, 35.95386929396252640 ) ) ;
#44904 = AXIS2_PLACEMENT_3D ( 'NONE', #69691, #58787, #18188 ) ;
#44905 = ORIENTED_EDGE ( 'NONE', *, *, #12129, .F. ) ;
#44906 = PRODUCT_RELATED_PRODUCT_CATEGORY ( 'part', '', ( #59551 ) ) ;
#44907 = CARTESIAN_POINT ( 'NONE',  ( -97.30629616937501680, 88.66845928578038638, 80.17072916753379275 ) ) ;
#44908 = EDGE_CURVE ( 'NONE', #34500, #50378, #56678, .T. ) ;
#44909 = CARTESIAN_POINT ( 'NONE',  ( 0.000000000000000000, -3.948201729842037544, -23.21447184625298021 ) ) ;
#44910 = AXIS2_PLACEMENT_3D ( 'NONE', #68489, #16981, #39920 ) ;
#44911 = CYLINDRICAL_SURFACE ( 'NONE', #11421, 2.649999999999985700 ) ;
#44912 = DIRECTION ( 'NONE',  ( -1.000000000000000000, 0.000000000000000000, 0.000000000000000000 ) ) ;
#44913 = EDGE_CURVE ( 'NONE', #13679, #56468, #11952, .T. ) ;
#44914 = DIRECTION ( 'NONE',  ( -1.000000000000000000, -0.000000000000000000, 0.000000000000000000 ) ) ;
#44915 = CARTESIAN_POINT ( 'NONE',  ( -92.35000000000003695, 90.00000000000004263, 90.00000000000000000 ) ) ;
#44916 = DIRECTION ( 'NONE',  ( 0.000000000000000000, 0.000000000000000000, 1.000000000000000000 ) ) ;
#44917 = FILL_AREA_STYLE_COLOUR ( '', #62607 ) ;
#44918 = ADVANCED_FACE ( 'NONE', ( #308 ), #69060, .F. ) ;
#44919 = ADVANCED_FACE ( 'NONE', ( #73565 ), #34097, .F. ) ;
#44920 = CARTESIAN_POINT ( 'NONE',  ( 93.84685191531248449, 88.00268892867053694, 81.65239583420049030 ) ) ;
#44921 = AXIS2_PLACEMENT_3D ( 'NONE', #42285, #3918, #65211 ) ;
#44922 = CARTESIAN_POINT ( 'NONE',  ( -92.69370383062498320, -208.6684592857803295, 78.74197916753381321 ) ) ;
#44923 = FACE_OUTER_BOUND ( 'NONE', #65493, .T. ) ;
#44924 = ORIENTED_EDGE ( 'NONE', *, *, #53995, .F. ) ;
#44925 = DIRECTION ( 'NONE',  ( -0.000000000000000000, -0.2079116908177653378, 0.9781476007338044676 ) ) ;
#44926 = DIRECTION ( 'NONE',  ( 0.000000000000000000, 0.9876883405951382144, -0.1564344650402276493 ) ) ;
#44927 = CARTESIAN_POINT ( 'NONE',  ( -97.30629616937501680, 90.00000000000004263, 77.73656250086715147 ) ) ;
#44929 = ADVANCED_FACE ( 'NONE', ( #5919 ), #17544, .T. ) ;
#44928 = CARTESIAN_POINT ( 'NONE',  ( 97.30629616937498838, -211.3315407142195852, 79.74739583420047495 ) ) ;
#44930 = ORIENTED_EDGE ( 'NONE', *, *, #67126, .T. ) ;
#44931 = EDGE_CURVE ( 'NONE', #30791, #66690, #70720, .T. ) ;
#44932 = CIRCLE ( 'NONE', #22112, 82.00000000000000000 ) ;
#44933 = DIRECTION ( 'NONE',  ( -1.000000000000000000, 0.000000000000000000, 0.000000000000000000 ) ) ;
#44934 = ORIENTED_EDGE ( 'NONE', *, *, #36435, .F. ) ;
#44935 = CARTESIAN_POINT ( 'NONE',  ( -96.32499999999996021, -207.7050326799711968, 88.06854166840095388 ) ) ;
#44936 = ORIENTED_EDGE ( 'NONE', *, *, #26910, .T. ) ;
#44937 = DIRECTION ( 'NONE',  ( 0.000000000000000000, 1.000000000000000000, 0.000000000000000000 ) ) ;
#44938 = ADVANCED_FACE ( 'NONE', ( #51381 ), #67947, .F. ) ;
#44939 = VECTOR ( 'NONE', #42534, 1000.000000000000000 ) ;
#44940 = ORIENTED_EDGE ( 'NONE', *, *, #71022, .F. ) ;
#44941 = VERTEX_POINT ( 'NONE', #4431 ) ;
#44942 = ORIENTED_EDGE ( 'NONE', *, *, #27311, .T. ) ;
#44943 = CARTESIAN_POINT ( 'NONE',  ( 93.84685191531249870, -208.0026889286704943, 75.72572916753382799 ) ) ;
#44944 = ORIENTED_EDGE ( 'NONE', *, *, #31422, .T. ) ;
#44945 = DIRECTION ( 'NONE',  ( -1.000000000000000000, -0.000000000000000000, -0.000000000000000000 ) ) ;
#44946 = DIRECTION ( 'NONE',  ( 0.000000000000000000, -0.3090169943749548342, 0.9510565162951511997 ) ) ;
#44947 = CARTESIAN_POINT ( 'NONE',  ( 92.69370383062498320, 88.66845928578037217, 87.31447916753381833 ) ) ;
#44948 = VECTOR ( 'NONE', #57598, 1000.000000000000000 ) ;
#44949 = DIRECTION ( 'NONE',  ( -1.000000000000000000, -0.000000000000000000, -0.000000000000000000 ) ) ;
#44950 = CARTESIAN_POINT ( 'NONE',  ( 97.64999999999997726, -211.5299782133524502, 78.19958333333332234 ) ) ;
#44951 = VERTEX_POINT ( 'NONE', #73198 ) ;
#44952 = ORIENTED_EDGE ( 'NONE', *, *, #20207, .T. ) ;
#44953 = ORIENTED_EDGE ( 'NONE', *, *, #40427, .F. ) ;
#44954 = VERTEX_POINT ( 'NONE', #51020 ) ;
#44955 = FACE_OUTER_BOUND ( 'NONE', #36157, .T. ) ;
#44956 = CYLINDRICAL_SURFACE ( 'NONE', #34307, 31.99999999999997868 ) ;
#44957 = CARTESIAN_POINT ( 'NONE',  ( 11.99999999999999822, 0.000000000000000000, 0.000000000000000000 ) ) ;
#44958 = CYLINDRICAL_SURFACE ( 'NONE', #1825, 2.649999999999985700 ) ;
#44959 = CARTESIAN_POINT ( 'NONE',  ( -93.67499999999998295, -212.2949673200287179, 88.38604166840097776 ) ) ;
#44960 = DIRECTION ( 'NONE',  ( -1.000000000000000000, 0.000000000000000000, 0.000000000000000000 ) ) ;
#44961 = ORIENTED_EDGE ( 'NONE', *, *, #9185, .T. ) ;
#44962 = CARTESIAN_POINT ( 'NONE',  ( -94.99999999999997158, -206.9400435732949575, 84.20562500173429044 ) ) ;
#44963 = VERTEX_POINT ( 'NONE', #16435 ) ;
#44964 = CARTESIAN_POINT ( 'NONE',  ( 10.00000000000000000, -37.16516213103273714, -4.992566952385376844 ) ) ;
#44965 = AXIS2_PLACEMENT_3D ( 'NONE', #4535, #28182, #74043 ) ;
#44966 = ORIENTED_EDGE ( 'NONE', *, *, #49642, .F. ) ;
#44968 = CARTESIAN_POINT ( 'NONE',  ( -93.67500000000003979, 87.70503267997129626, 82.67104166840096013 ) ) ;
#44967 = CARTESIAN_POINT ( 'NONE',  ( 97.64999999999999147, 90.00000000000002842, 82.14187500173429157 ) ) ;
#44969 = ORIENTED_EDGE ( 'NONE', *, *, #38907, .T. ) ;
#44970 = CARTESIAN_POINT ( 'NONE',  ( 97.30629616937498838, 88.66845928578037217, 84.35114583420049428 ) ) ;
#44971 = DIRECTION ( 'NONE',  ( -1.000000000000000000, -0.000000000000000000, 0.000000000000000000 ) ) ;
#44973 = EDGE_CURVE ( 'NONE', #31529, #105, #4816, .T. ) ;
#44972 = LINE ( 'NONE', #73893, #22243 ) ;
#44974 = CIRCLE ( 'NONE', #27021, 23.50000000000000355 ) ;
#44975 = CARTESIAN_POINT ( 'NONE',  ( 11.99999999999999822, -74.18225833017864090, -34.94270380257717790 ) ) ;
#44976 = DIRECTION ( 'NONE',  ( 1.000000000000000000, -0.000000000000000000, -0.000000000000000000 ) ) ;
#44977 = PLANE ( 'NONE',  #16884 ) ;
#44978 = ORIENTED_EDGE ( 'NONE', *, *, #25903, .T. ) ;
#44979 = CARTESIAN_POINT ( 'NONE',  ( 0.000000000000000000, 55.38113227695782115, 54.21277698773695164 ) ) ;
#44980 = LINE ( 'NONE', #44614, #7346 ) ;
#44981 = DIRECTION ( 'NONE',  ( -0.9918136447140104561, 0.1276937514489679681, 0.000000000000000000 ) ) ;
#44982 = VERTEX_POINT ( 'NONE', #61938 ) ;
#44983 = VERTEX_POINT ( 'NONE', #21698 ) ;
#44984 = EDGE_CURVE ( 'NONE', #43091, #59828, #1222, .T. ) ;
#44985 = EDGE_CURVE ( 'NONE', #67887, #11862, #39005, .T. ) ;
#44986 = CYLINDRICAL_SURFACE ( 'NONE', #60101, 15.99999999999999645 ) ;
#44987 = CARTESIAN_POINT ( 'NONE',  ( -92.34999999999999432, -209.9999999999999716, 85.87249999999998806 ) ) ;
#44988 = CARTESIAN_POINT ( 'NONE',  ( -103.9230484541323705, -180.0000000000004832, -5.500000000000000000 ) ) ;
#44989 = CARTESIAN_POINT ( 'NONE',  ( -92.69370383062498320, -208.6684592857803011, 81.91697916753381037 ) ) ;
#44990 = ORIENTED_EDGE ( 'NONE', *, *, #44288, .T. ) ;
#44991 = CARTESIAN_POINT ( 'NONE',  ( -93.84685191531252713, 88.00268892867056536, 89.21947916753380525 ) ) ;
#44992 = VERTEX_POINT ( 'NONE', #27716 ) ;
#44993 = AXIS2_PLACEMENT_3D ( 'NONE', #59992, #59609, #42322 ) ;
#44994 = EDGE_CURVE ( 'NONE', #48071, #42429, #60286, .T. ) ;
#44995 = FACE_OUTER_BOUND ( 'NONE', #54197, .T. ) ;
#44996 = CIRCLE ( 'NONE', #6563, 77.49900000000000944 ) ;
#44997 = DIRECTION ( 'NONE',  ( 0.1736481776669309418, -0.9848077530122080203, 0.000000000000000000 ) ) ;
#44998 = CARTESIAN_POINT ( 'NONE',  ( 11.99999999999999822, 74.65491531819118620, -8.830959090342659579 ) ) ;
#44999 = CARTESIAN_POINT ( 'NONE',  ( 96.15314808468748708, 91.99731107132950569, 76.09614583420047040 ) ) ;
#45000 = DIRECTION ( 'NONE',  ( -1.000000000000000000, 0.000000000000000000, 0.000000000000000000 ) ) ;
#45001 = CARTESIAN_POINT ( 'NONE',  ( 11.99999999999999822, -18.89407956138204980, -75.16055320797050854 ) ) ;
#45002 = CARTESIAN_POINT ( 'NONE',  ( 97.64999999999990621, -209.9999992849081139, 85.31687502647973531 ) ) ;
#45003 = CARTESIAN_POINT ( 'NONE',  ( 12.00000000000000000, 26.50000000000000355, -1.500000000000000000 ) ) ;
#45004 = CARTESIAN_POINT ( 'NONE',  ( 2.500000000000000000, 16.00000000000000000, -10.00000000000000178 ) ) ;
#45005 = DIRECTION ( 'NONE',  ( 0.000000000000000000, 0.000000000000000000, 1.000000000000000000 ) ) ;
#45006 = AXIS2_PLACEMENT_3D ( 'NONE', #10765, #67538, #33693 ) ;
#45007 = EDGE_CURVE ( 'NONE', #67479, #53775, #16850, .T. ) ;
#45008 = CARTESIAN_POINT ( 'NONE',  ( 0.000000000000000000, -21.40280677340345505, -36.13751322684441192 ) ) ;
#45009 = AXIS2_PLACEMENT_3D ( 'NONE', #39967, #69993, #46342 ) ;
#45010 = FACE_OUTER_BOUND ( 'NONE', #29479, .T. ) ;
#45011 = CARTESIAN_POINT ( 'NONE',  ( -92.69370383062498320, -209.9999999999999716, 89.48406250086715374 ) ) ;
#45012 = DIRECTION ( 'NONE',  ( -1.000000000000000000, 0.000000000000000000, 0.000000000000000000 ) ) ;
#45013 = ORIENTED_EDGE ( 'NONE', *, *, #70260, .F. ) ;
#45014 = CARTESIAN_POINT ( 'NONE',  ( 0.000000000000000000, -16.23288003029473359, -33.80338159004301701 ) ) ;
#45015 = CARTESIAN_POINT ( 'NONE',  ( -96.15314808468752972, 91.99731107132950569, 78.74197916753381321 ) ) ;
#45016 = AXIS2_PLACEMENT_3D ( 'NONE', #53882, #19657, #60645 ) ;
#45018 = EDGE_CURVE ( 'NONE', #21751, #40611, #29549, .T. ) ;
#45017 = DIRECTION ( 'NONE',  ( -1.000000000000000000, -0.000000000000000000, -0.000000000000000000 ) ) ;
#45019 = ADVANCED_FACE ( 'NONE', ( #2795 ), #25684, .T. ) ;
#45020 = AXIS2_PLACEMENT_3D ( 'NONE', #73787, #50493, #32082 ) ;
#45021 = ORIENTED_EDGE ( 'NONE', *, *, #62824, .F. ) ;
#45022 = CARTESIAN_POINT ( 'NONE',  ( 92.35000000000002274, -209.9999762675151658, 79.91937418090955703 ) ) ;
#45023 = EDGE_CURVE ( 'NONE', #7584, #8374, #48618, .T. ) ;
#45024 = CARTESIAN_POINT ( 'NONE',  ( 5.999999999999999112, -51.29473840253177030, -63.97538442413482329 ) ) ;
#45025 = DIRECTION ( 'NONE',  ( 1.000000000000000000, 0.000000000000000000, -0.000000000000000000 ) ) ;
#45026 = CARTESIAN_POINT ( 'NONE',  ( 96.15314808468748708, -208.0026889286704943, 76.25489583420049655 ) ) ;
#45027 = ORIENTED_EDGE ( 'NONE', *, *, #62151, .F. ) ;
#45028 = VERTEX_POINT ( 'NONE', #36967 ) ;
#45029 = DIRECTION ( 'NONE',  ( 0.000000000000000000, 0.000000000000000000, 1.000000000000000000 ) ) ;
#45030 = DIRECTION ( 'NONE',  ( -1.000000000000000000, -0.000000000000000000, 0.000000000000000000 ) ) ;
#45031 = VECTOR ( 'NONE', #37891, 1000.000000000000000 ) ;
#45032 = CARTESIAN_POINT ( 'NONE',  ( 11.99999999999999822, -74.65374052328654386, 8.840884882374837161 ) ) ;
#45033 = CARTESIAN_POINT ( 'NONE',  ( 10.00000000000000000, 33.00180498840046539, 17.80606268964551120 ) ) ;
#45034 = CARTESIAN_POINT ( 'NONE',  ( 92.35000000000000853, -211.5299782133524218, 81.87729166840097150 ) ) ;
#45035 = CARTESIAN_POINT ( 'NONE',  ( 97.64999999999997726, -211.5299782133524502, 87.72458333333332803 ) ) ;
#45036 = ORIENTED_EDGE ( 'NONE', *, *, #17229, .F. ) ;
#45037 = DIRECTION ( 'NONE',  ( 0.000000000000000000, -0.000000000000000000, -1.000000000000000000 ) ) ;
#45038 = ORIENTED_EDGE ( 'NONE', *, *, #30371, .T. ) ;
#45039 = ORIENTED_EDGE ( 'NONE', *, *, #56301, .T. ) ;
#45040 = PLANE ( 'NONE',  #46594 ) ;
#45041 = AXIS2_PLACEMENT_3D ( 'NONE', #37835, #49470, #42363 ) ;
#45042 = SURFACE_STYLE_USAGE ( .BOTH. , #28104 ) ;
#45043 = CARTESIAN_POINT ( 'NONE',  ( -95.00000000000002842, 90.00000000000004263, 90.00000000000000000 ) ) ;
#45044 = ORIENTED_EDGE ( 'NONE', *, *, #12415, .F. ) ;
#45045 = FACE_OUTER_BOUND ( 'NONE', #49123, .T. ) ;
#45046 = CARTESIAN_POINT ( 'NONE',  ( 97.64999999999999147, -209.9999999999999716, 75.79187500173429726 ) ) ;
#45047 = CARTESIAN_POINT ( 'NONE',  ( 93.67499999999999716, 87.70503267997126784, 81.85083333333332689 ) ) ;
#45048 = ORIENTED_EDGE ( 'NONE', *, *, #62579, .T. ) ;
#45049 = DIRECTION ( 'NONE',  ( 1.000000000000000000, 0.000000000000000000, 0.000000000000000000 ) ) ;
#45050 = ORIENTED_EDGE ( 'NONE', *, *, #46017, .F. ) ;
#45051 = CARTESIAN_POINT ( 'NONE',  ( 5.000000000000000888, -2.886751345948134873, -2.080000000000000071 ) ) ;
#45052 = ORIENTED_EDGE ( 'NONE', *, *, #45154, .F. ) ;
#45053 = FACE_OUTER_BOUND ( 'NONE', #37365, .T. ) ;
#45054 = CARTESIAN_POINT ( 'NONE',  ( -93.84685191531252713, 88.00268892867056536, 86.20322916753382003 ) ) ;
#45055 = AXIS2_PLACEMENT_3D ( 'NONE', #64491, #11858, #17881 ) ;
#45056 = CARTESIAN_POINT ( 'NONE',  ( 96.15314808468748708, 91.99731107132950569, 79.27114583420046756 ) ) ;
#45057 = AXIS2_PLACEMENT_3D ( 'NONE', #52255, #63556, #46620 ) ;
#45058 = ORIENTED_EDGE ( 'NONE', *, *, #22615, .T. ) ;
#45059 = CARTESIAN_POINT ( 'NONE',  ( 10.00000000000000000, 35.95386929396256903, -10.96151621346501237 ) ) ;
#45060 = DIRECTION ( 'NONE',  ( 0.000000000000000000, 0.000000000000000000, 1.000000000000000000 ) ) ;
#45061 = EDGE_CURVE ( 'NONE', #7474, #65748, #30335, .T. ) ;
#45062 = CARTESIAN_POINT ( 'NONE',  ( 0.000000000000000000, 0.000000000000000000, 0.000000000000000000 ) ) ;
#45063 = DIRECTION ( 'NONE',  ( -1.000000000000000000, 0.000000000000000000, -0.000000000000000000 ) ) ;
#45064 = VERTEX_POINT ( 'NONE', #8023 ) ;
#45065 = CARTESIAN_POINT ( 'NONE',  ( -97.64999999999989200, -211.5299782133525071, 86.24291666666667311 ) ) ;
#45066 = AXIS2_PLACEMENT_3D ( 'NONE', #55485, #67508, #9983 ) ;
#45067 = CARTESIAN_POINT ( 'NONE',  ( -92.69370383062498320, -211.3315407142195852, 78.47739583420047893 ) ) ;
#45068 = ORIENTED_EDGE ( 'NONE', *, *, #72531, .T. ) ;
#45069 = EDGE_LOOP ( 'NONE', ( #6849, #49553, #39763, #19606 ) ) ;
#45070 = EDGE_CURVE ( 'NONE', #51530, #19604, #54269, .T. ) ;
#45072 = DIRECTION ( 'NONE',  ( -1.000000000000000000, -0.000000000000000000, 0.000000000000000000 ) ) ;
#45071 = VECTOR ( 'NONE', #8, 1000.000000000000000 ) ;
#45073 = EDGE_CURVE ( 'NONE', #70981, #56782, #60652, .T. ) ;
#45074 = EDGE_LOOP ( 'NONE', ( #14806, #41787, #35225, #52612 ) ) ;
#45075 = LINE ( 'NONE', #67997, #54029 ) ;
#45076 = CYLINDRICAL_SURFACE ( 'NONE', #5283, 16.00000000000000000 ) ;
#45077 = ORIENTED_EDGE ( 'NONE', *, *, #59722, .T. ) ;
#45078 =( BOUNDED_CURVE ( )  B_SPLINE_CURVE ( 2, ( #68808, #40225, #12379, #36790, #2258, #30768, #13495 ),
 .UNSPECIFIED., .F., .F. ) 
 B_SPLINE_CURVE_WITH_KNOTS ( ( 3, 2, 2, 3 ),
 ( 0.6250000000000003331, 0.6319444444444446418, 0.6388888888888890616, 0.6458333333333334814 ),
 .UNSPECIFIED. ) 
 CURVE ( )  GEOMETRIC_REPRESENTATION_ITEM ( )  RATIONAL_B_SPLINE_CURVE ( ( 0.9999999999999935607, 0.8660254037844451469, 1.000000000000000000, 0.8660254037844387076, 1.000000000000000000, 0.8660254037844365982, 1.000000000000002220 ) ) 
 REPRESENTATION_ITEM ( '' )  );
#45079 = CARTESIAN_POINT ( 'NONE',  ( -93.84685191531248449, -208.0026889286704943, 76.73114583420047552 ) ) ;
#45080 = EDGE_LOOP ( 'NONE', ( #71494, #67769, #10717, #41632 ) ) ;
#45081 = CARTESIAN_POINT ( 'NONE',  ( 14.53333333333331545, 0.000000000000000000, -1.466666666666671670 ) ) ;
#45082 = FACE_OUTER_BOUND ( 'NONE', #53655, .T. ) ;
#45083 = DIRECTION ( 'NONE',  ( -1.000000000000000000, 0.000000000000000000, 0.000000000000000000 ) ) ;
#45084 = FACE_OUTER_BOUND ( 'NONE', #58414, .T. ) ;
#45085 = CIRCLE ( 'NONE', #65465, 77.49900000000000944 ) ;
#45086 = ADVANCED_FACE ( 'NONE', ( #53889 ), #6282, .T. ) ;
#45087 = CARTESIAN_POINT ( 'NONE',  ( 0.000000000000000000, 0.000000000000000000, 0.000000000000000000 ) ) ;
#45088 = VECTOR ( 'NONE', #53582, 1000.000000000000000 ) ;
#45089 = DIRECTION ( 'NONE',  ( -0.000000000000000000, 0.4067366430758000417, -0.9135454576426009776 ) ) ;
#45090 = CARTESIAN_POINT ( 'NONE',  ( 92.69370383062498320, 90.00000000000002842, 85.19781250086714408 ) ) ;
#45091 = LINE ( 'NONE', #15763, #14775 ) ;
#45092 = CARTESIAN_POINT ( 'NONE',  ( -97.65000000000001990, 90.00000000000004263, 75.39499999999999602 ) ) ;
#45093 = DIRECTION ( 'NONE',  ( -2.628368902995175337E-16, -1.000000000000000000, 0.000000000000000000 ) ) ;
#45094 = DIRECTION ( 'NONE',  ( 0.9827303690289279636, 0.1850432970638682395, 0.000000000000000000 ) ) ;
#45095 = FACE_OUTER_BOUND ( 'NONE', #20945, .T. ) ;
#45096 = CARTESIAN_POINT ( 'NONE',  ( 0.1709976663248966577, 5.674777143212787145, -1.879366290983712107 ) ) ;
#45097 = CARTESIAN_POINT ( 'NONE',  ( 11.99999999999999822, -55.20638768913724448, -51.02545421589383068 ) ) ;
#45098 = CARTESIAN_POINT ( 'NONE',  ( 11.99999999999999822, 0.000000000000000000, 0.000000000000000000 ) ) ;
#45099 = EDGE_CURVE ( 'NONE', #71285, #31085, #69414, .T. ) ;
#45100 = CARTESIAN_POINT ( 'NONE',  ( 30.50000000000000000, -120.0000000000000000, -2.500000000000000000 ) ) ;
#45101 = LINE ( 'NONE', #20400, #7291 ) ;
#45102 = CARTESIAN_POINT ( 'NONE',  ( -95.00000000000002842, 87.33691857156074434, 88.53156250086716739 ) ) ;
#45103 = CIRCLE ( 'NONE', #69081, 42.00000000000000000 ) ;
#45104 = CARTESIAN_POINT ( 'NONE',  ( 5.000000000000002665, 10.30890764327501863, -81.34940948281325745 ) ) ;
#45105 = CARTESIAN_POINT ( 'NONE',  ( -93.67499999999998295, -207.7050326799711968, 85.34333333333333371 ) ) ;
#45106 = DIRECTION ( 'NONE',  ( -1.000000000000000000, 0.000000000000000000, 0.000000000000000000 ) ) ;
#45107 = ADVANCED_FACE ( 'NONE', ( #71903 ), #48251, .T. ) ;
#45108 = ADVANCED_FACE ( 'NONE', ( #6637 ), #670, .T. ) ;
#45109 = CARTESIAN_POINT ( 'NONE',  ( 5.999999999999999112, 55.16347631943131802, -60.67117009219074930 ) ) ;
#45110 = CIRCLE ( 'NONE', #40319, 16.00000000000000355 ) ;
#45111 = DIRECTION ( 'NONE',  ( 1.000000000000000000, 0.000000000000000000, 0.000000000000000000 ) ) ;
#45112 = CARTESIAN_POINT ( 'NONE',  ( -12.40464318976454727, 10.41032311384371667, -45.00000000000000000 ) ) ;
#45113 = CARTESIAN_POINT ( 'NONE',  ( -10.00000000000000000, 0.000000000000000000, 0.000000000000000000 ) ) ;
#45114 = VECTOR ( 'NONE', #70081, 1000.000000000000000 ) ;
#45115 = CARTESIAN_POINT ( 'NONE',  ( 92.69370383062501162, -211.3315407142195852, 86.04447916753382231 ) ) ;
#45116 = VERTEX_POINT ( 'NONE', #63798 ) ;
#45117 = AXIS2_PLACEMENT_3D ( 'NONE', #49865, #32941, #16038 ) ;
#45118 = ORIENTED_EDGE ( 'NONE', *, *, #57784, .F. ) ;
#45119 = CARTESIAN_POINT ( 'NONE',  ( 2.047646702416564768, -96.54137380445985173, 5.500000000000000000 ) ) ;
#45120 = EDGE_LOOP ( 'NONE', ( #40895, #28834, #21246, #34860 ) ) ;
#45121 =( REPRESENTATION_RELATIONSHIP ('NONE','NONE', #31117, #33525 ) REPRESENTATION_RELATIONSHIP_WITH_TRANSFORMATION ( #430 )SHAPE_REPRESENTATION_RELATIONSHIP( ) );
#45122 = AXIS2_PLACEMENT_3D ( 'NONE', #14458, #15193, #19720 ) ;
#45123 = FACE_OUTER_BOUND ( 'NONE', #19713, .T. ) ;
#45124 = CIRCLE ( 'NONE', #12690, 77.49900000000000944 ) ;
#45125 = CARTESIAN_POINT ( 'NONE',  ( 92.69370383062501162, -211.3315407142195852, 79.53572916753380184 ) ) ;
#45126 = ORIENTED_EDGE ( 'NONE', *, *, #22921, .F. ) ;
#45127 = CARTESIAN_POINT ( 'NONE',  ( 95.00000000000000000, -207.3369185715606307, 83.92781250086716227 ) ) ;
#45128 = ORIENTED_EDGE ( 'NONE', *, *, #73829, .T. ) ;
#45129 = DIRECTION ( 'NONE',  ( 0.000000000000000000, 0.000000000000000000, 1.000000000000000000 ) ) ;
#45130 = VERTEX_POINT ( 'NONE', #12270 ) ;
#45131 = EDGE_LOOP ( 'NONE', ( #6084, #51602, #9516, #3090, #68812 ) ) ;
#45132 = DIRECTION ( 'NONE',  ( -1.000000000000000000, 0.000000000000000000, 0.000000000000000000 ) ) ;
#45133 = DIRECTION ( 'NONE',  ( 0.000000000000000000, 1.000000000000000000, 1.301042606982602757E-15 ) ) ;
#45134 = VERTEX_POINT ( 'NONE', #58141 ) ;
#45135 = CARTESIAN_POINT ( 'NONE',  ( 94.99999999999998579, 93.05995642670504253, 86.03125000000000000 ) ) ;
#45136 = DIRECTION ( 'NONE',  ( 0.000000000000000000, -0.3826834323650969427, 0.9238795325112837409 ) ) ;
#45137 = EDGE_LOOP ( 'NONE', ( #42763, #67875, #25975, #18886 ) ) ;
#45138 = CYLINDRICAL_SURFACE ( 'NONE', #27443, 77.49899999999999523 ) ;
#45139 = EDGE_CURVE ( 'NONE', #9979, #30261, #44485, .T. ) ;
#45140 = ORIENTED_EDGE ( 'NONE', *, *, #7869, .F. ) ;
#45141 = CYLINDRICAL_SURFACE ( 'NONE', #18016, 16.00000000000000355 ) ;
#45142 = VERTEX_POINT ( 'NONE', #56491 ) ;
#45143 = EDGE_CURVE ( 'NONE', #61669, #66673, #64886, .T. ) ;
#45144 = ORIENTED_EDGE ( 'NONE', *, *, #52444, .F. ) ;
#45145 = VERTEX_POINT ( 'NONE', #62124 ) ;
#45146 = CARTESIAN_POINT ( 'NONE',  ( 93.84685191531251292, -211.9973110713294489, 75.77864583420047495 ) ) ;
#45147 = CONTEXT_DEPENDENT_SHAPE_REPRESENTATION ( #10976, #40442 ) ;
#45148 = CARTESIAN_POINT ( 'NONE',  ( -10.00000000000000000, 0.000000000000000000, 0.000000000000000000 ) ) ;
#45150 = EDGE_CURVE ( 'NONE', #6105, #19678, #58873, .T. ) ;
#45149 = ORIENTED_EDGE ( 'NONE', *, *, #20726, .T. ) ;
#45151 = ORIENTED_EDGE ( 'NONE', *, *, #45708, .T. ) ;
#45152 = VERTEX_POINT ( 'NONE', #73382 ) ;
#45153 = DIRECTION ( 'NONE',  ( -1.000000000000000000, -0.000000000000000000, -0.000000000000000000 ) ) ;
#45154 = EDGE_CURVE ( 'NONE', #62613, #65045, #61003, .T. ) ;
#45155 = LINE ( 'NONE', #16198, #43366 ) ;
#45156 = CARTESIAN_POINT ( 'NONE',  ( -92.69370383062504004, 90.00000000000004263, 74.87906250086714977 ) ) ;
#45157 = VERTEX_POINT ( 'NONE', #44087 ) ;
#45158 = CARTESIAN_POINT ( 'NONE',  ( 94.99999999999998579, 87.33691857156068750, 75.19656250086714522 ) ) ;
#45159 = EDGE_LOOP ( 'NONE', ( #24156, #27725, #15524, #37732 ) ) ;
#45160 = PRESENTATION_STYLE_ASSIGNMENT (( #21087 ) ) ;
#45161 = CARTESIAN_POINT ( 'NONE',  ( -92.69370383062498320, -211.3315407142195852, 86.09739583420048348 ) ) ;
#45162 = VERTEX_POINT ( 'NONE', #21889 ) ;
#45163 = CARTESIAN_POINT ( 'NONE',  ( 4.282125186551308360, -3.301216562737187221, -1.327869168827487290 ) ) ;
#45164 = AXIS2_PLACEMENT_3D ( 'NONE', #46360, #69288, #40719 ) ;
#45165 = DIRECTION ( 'NONE',  ( -1.000000000000000000, -0.000000000000000000, -0.000000000000000000 ) ) ;
#45166 = DIRECTION ( 'NONE',  ( -0.000000000000000000, -0.000000000000000000, -1.000000000000000000 ) ) ;
#45167 = CARTESIAN_POINT ( 'NONE',  ( -92.69370383062498320, -209.9999999999999716, 78.53031250086714010 ) ) ;
#45168 = EDGE_CURVE ( 'NONE', #47715, #24191, #26776, .T. ) ;
#45169 = DIRECTION ( 'NONE',  ( -1.000000000000000000, -0.000000000000000000, 0.000000000000000000 ) ) ;
#45170 = CARTESIAN_POINT ( 'NONE',  ( 0.000000000000000000, 5.256550761632864166, 77.32052557432842832 ) ) ;
#45171 = CARTESIAN_POINT ( 'NONE',  ( 0.000000000000000000, -46.21855187248673502, 62.20884554314003623 ) ) ;
#45172 = AXIS2_PLACEMENT_3D ( 'NONE', #50457, #21886, #23736 ) ;
#45173 = ORIENTED_EDGE ( 'NONE', *, *, #28596, .F. ) ;
#45174 = CARTESIAN_POINT ( 'NONE',  ( 10.00000000000000000, 31.52238457039599595, 27.75498641678753842 ) ) ;
#45175 = CIRCLE ( 'NONE', #36730, 77.49900000000000944 ) ;
#45176 = CARTESIAN_POINT ( 'NONE',  ( -12.75000000000000000, -120.0000000000000000, -85.60000000000000853 ) ) ;
#45177 = CARTESIAN_POINT ( 'NONE',  ( 96.73972734126404305, -208.4859488783623362, 74.79348190356850523 ) ) ;
#45178 = CARTESIAN_POINT ( 'NONE',  ( -93.84685191531254134, 91.99731107132950569, 82.44614583420046472 ) ) ;
#45179 = CARTESIAN_POINT ( 'NONE',  ( -97.65000000000001990, 90.00000000000004263, 85.55499999999999261 ) ) ;
#45180 = FACE_OUTER_BOUND ( 'NONE', #27545, .T. ) ;
#45181 = VECTOR ( 'NONE', #4220, 1000.000000000000000 ) ;
#45182 = EDGE_CURVE ( 'NONE', #62894, #60745, #20432, .T. ) ;
#45183 = AXIS2_PLACEMENT_3D ( 'NONE', #16212, #62090, #11314 ) ;
#45184 = VERTEX_POINT ( 'NONE', #44466 ) ;
#45185 = EDGE_CURVE ( 'NONE', #39781, #68825, #4626, .T. ) ;
#45186 = CARTESIAN_POINT ( 'NONE',  ( -0.0004442498525516064278, 0.001194404164626844313, -85.59999999999999432 ) ) ;
#45187 = EDGE_CURVE ( 'NONE', #34606, #9528, #37719, .T. ) ;
#45188 = FACE_OUTER_BOUND ( 'NONE', #6736, .T. ) ;
#45189 = DIRECTION ( 'NONE',  ( -0.8225049752423776450, -0.5687579148473765889, 0.000000000000000000 ) ) ;
#45190 = CARTESIAN_POINT ( 'NONE',  ( 0.000000000000000000, -78.73519480814938731, -22.90783923731713756 ) ) ;
#45191 = CARTESIAN_POINT ( 'NONE',  ( 11.99999999999999822, 0.000000000000000000, 0.000000000000000000 ) ) ;
#45192 = AXIS2_PLACEMENT_3D ( 'NONE', #53426, #42157, #58327 ) ;
#45193 = CARTESIAN_POINT ( 'NONE',  ( 1.474095553543393056, -119.7224350544041869, 2.500000000000000000 ) ) ;
#45194 = CARTESIAN_POINT ( 'NONE',  ( -97.30629616937497417, -208.6684592857803011, 79.58864583420047722 ) ) ;
#45195 = DIRECTION ( 'NONE',  ( -1.000000000000000000, 0.000000000000000000, 0.000000000000000000 ) ) ;
#45196 = EDGE_CURVE ( 'NONE', #13202, #61584, #27896, .T. ) ;
#45197 = ORIENTED_EDGE ( 'NONE', *, *, #50132, .F. ) ;
#45198 = DIRECTION ( 'NONE',  ( 0.000000000000000000, 0.000000000000000000, 1.000000000000000000 ) ) ;
#45199 = CARTESIAN_POINT ( 'NONE',  ( -97.65000000000001990, 90.00001557635633276, 80.55437446300187787 ) ) ;
#45200 = CYLINDRICAL_SURFACE ( 'NONE', #2185, 16.00000000000000000 ) ;
#45201 = EDGE_CURVE ( 'NONE', #588, #19443, #63655, .T. ) ;
#45202 = CARTESIAN_POINT ( 'NONE',  ( 7.543218489614351263, -11.91259227951415056, -1.199999999999999956 ) ) ;
#45203 = DIRECTION ( 'NONE',  ( 0.000000000000000000, -0.3826834323650772363, -0.9238795325112919565 ) ) ;
#45204 = CLOSED_SHELL ( 'NONE', ( #25488, #2987, #12876, #8423, #43905, #56634, #65696, #52098, #8648, #71695, #16491, #63160, #52772, #14585, #43816, #71467, #65896, #32144, #40318, #63618, #71983, #30861, #151, #30355, #56611, #43042, #6788, #30872, #64607, #38701, #62845, #57886, #61700, #51410, #63902, #25738, #63238, #48407, #49387, #67462, #65396, #49605, #53984, #22652, #16489, #37723, #22602, #25360, #27081, #63953, #46837, #67662, #51500, #40743, #45849, #24629, #3781, #54101, #43662, #23122, #40745, #59666, #69706, #53553, #15470, #49622, #42115, #24756, #55699, #10706, #34832, #12112, #48638, #8231, #20896, #53463, #46507, #24414, #43913, #70323, #9306, #21125, #57312, #37694, #23708, #59700, #71435, #5443, #17079, #10240, #32340, #24988, #23746, #31415, #54983, #14874, #50156, #73752, #70032, #18088, #35546, #53744, #30571, #61015, #24278, #9010, #14226, #65626, #37938, #41511, #12351, #56184, #50440, #57372, #70330, #12817, #21191, #2697, #37451, #57124, #40859, #27203, #11042, #13655, #58048, #67581, #22884, #69282, #5313, #12809, #24293, #60184, #11646, #3854, #42851, #9340, #43629, #18079, #58416, #73173, #49886, #3070, #35969, #21830, #65269, #72564, #2515, #57983, #20352, #47251, #4236, #18525, #29679, #2106, #37281, #16902, #47059, #52632, #28971, #41275, #44473, #60222, #51116, #35402, #22756, #36048, #13807, #9933, #34192, #26, #65809, #40947, #18005, #8087, #57904, #44298, #30948, #21801, #36259, #10975, #39031, #5110, #14420, #34547, #64682, #66119, #26881, #31495, #69243, #3916, #72932, #3876, #3840, #64247, #43836, #38479, #29544, #64495, #122, #23261, #23528, #18192, #18690, #1762, #44463, #6902, #53980, #61903, #37808, #46113, #36006, #12576, #9012, #65796, #48282, #19784, #71535, #27598, #58576, #7555, #25777, #63074, #62205, #42107, #65277, #28835, #62906, #68336, #2909, #9945, #19738, #34477, #52033, #11777, #40136, #46262, #40139, #46796, #37682, #23937, #13303, #21981, #29597, #20712, #56531, #53699, #16128, #58989, #24194, #14538, #1098, #47677, #59079, #1482, #37804, #56387, #71257, #15361, #5243, #20761, #14265, #20396, #33053, #19834, #69207, #50399, #7111, #38434, #39892, #35241, #62858, #11621, #66468, #5183, #61465, #16237, #22758, #12325, #14669, #60014, #52554, #46712, #39916, #1472, #2923, #50352, #12789, #34385, #64740, #1075, #50642, #67383, #10337, #66161, #59655, #23579, #49799, #4033, #24519, #71352, #25896, #17907, #13732, #68956, #59263, #2594, #15389, #12498, #7999, #244, #2939, #71212, #7720, #37022, #21283, #55420, #38204, #32717, #24227, #41774, #13353, #24689, #67557, #6568, #69701, #74123, #61307, #51842, #58468, #32405, #67985, #47220, #26273, #67917, #50696, #3742, #57291, #37693, #61124, #69531, #17687, #1733, #58252, #54683, #45921, #10973, #21359, #1656, #29015, #27128, #20121, #48469, #50320, #10295, #2694, #52954, #56200, #9767, #68019, #18800, #73562, #57301, #39651, #33687, #63322, #57370, #64423, #44400, #44335, #36667, #30895, #21184, #74155, #14948, #63038, #9062, #17758, #63522, #14352, #3651, #57207, #58554, #14854, #53783, #72732, #61370, #21909, #47712, #29421, #72697, #29828, #23969, #41924, #20290, #28023, #58507, #66903, #43080, #63321, #44919, #22711, #26404, #61994, #48621 ) ) ;
#45205 = CARTESIAN_POINT ( 'NONE',  ( 0.000000000000000000, -22.32062822937469804, -14.36278369418829826 ) ) ;
#45206 = EDGE_LOOP ( 'NONE', ( #45118, #46508, #62911, #31518, #58406, #27837, #23680, #2818, #29302, #56484, #6172, #34667, #16277, #62792, #37396, #6482, #45252, #48822, #41535, #60578, #343, #20047, #18569, #59468, #44694, #22076, #21422, #44763, #13678, #3349, #68487, #34938, #54433, #55577, #8156, #6864, #69185, #63109, #26915, #25776, #41259, #40603, #48198, #18508, #13800, #36875, #50551, #8109, #26356, #50630, #28776, #10211 ) ) ;
#45207 = FACE_OUTER_BOUND ( 'NONE', #31822, .T. ) ;
#45208 = CARTESIAN_POINT ( 'NONE',  ( 0.000000000000000000, 0.000000000000000000, 0.000000000000000000 ) ) ;
#45209 = EDGE_LOOP ( 'NONE', ( #35483, #53116, #31432, #10179 ) ) ;
#45210 = CARTESIAN_POINT ( 'NONE',  ( 95.00000000000000000, -207.3369185715606307, 86.94406250086714749 ) ) ;
#45211 = DIRECTION ( 'NONE',  ( -1.000000000000000000, 0.000000000000000000, -0.000000000000000000 ) ) ;
#45212 = AXIS2_PLACEMENT_3D ( 'NONE', #68839, #17326, #12049 ) ;
#45213 = ORIENTED_EDGE ( 'NONE', *, *, #29332, .F. ) ;
#45214 = CARTESIAN_POINT ( 'NONE',  ( 95.00000000000000000, -213.0599564267049857, 89.52374999999999261 ) ) ;
#45215 = ORIENTED_EDGE ( 'NONE', *, *, #69548, .T. ) ;
#45216 = CARTESIAN_POINT ( 'NONE',  ( 0.000000000000000000, -11.95096189432345390, 23.69967320028757385 ) ) ;
#45217 = VERTEX_POINT ( 'NONE', #67762 ) ;
#45218 = CARTESIAN_POINT ( 'NONE',  ( -24.94940289813038703, -237.3777120880567963, -5.500000000000000000 ) ) ;
#45219 = VERTEX_POINT ( 'NONE', #43730 ) ;
#45220 = CIRCLE ( 'NONE', #55995, 12.74999999999999822 ) ;
#45221 = ORIENTED_EDGE ( 'NONE', *, *, #66629, .F. ) ;
#45222 = CIRCLE ( 'NONE', #35595, 31.99999999999998934 ) ;
#45223 = ORIENTED_EDGE ( 'NONE', *, *, #65529, .F. ) ;
#45224 = DIRECTION ( 'NONE',  ( 1.000000000000000000, 0.000000000000000000, 0.000000000000000000 ) ) ;
#45225 = ORIENTED_EDGE ( 'NONE', *, *, #31409, .F. ) ;
#45226 = PRODUCT_DEFINITION_SHAPE ( 'NONE', 'NONE',  #23745 ) ;
#45227 = VECTOR ( 'NONE', #4507, 1000.000000000000000 ) ;
#45228 = EDGE_LOOP ( 'NONE', ( #58912, #46315, #21628, #46182 ) ) ;
#45229 = CARTESIAN_POINT ( 'NONE',  ( 93.67499999999998295, 92.29496732002878900, 87.35416666666665719 ) ) ;
#45230 = DIRECTION ( 'NONE',  ( -0.000000000000000000, -0.000000000000000000, -1.000000000000000000 ) ) ;
#45231 = DIRECTION ( 'NONE',  ( 0.000000000000000000, 0.9945218953682742891, 0.1045284632676436315 ) ) ;
#45232 = ORIENTED_EDGE ( 'NONE', *, *, #72376, .T. ) ;
#45233 = ORIENTED_EDGE ( 'NONE', *, *, #37165, .F. ) ;
#45234 = ADVANCED_FACE ( 'NONE', ( #67384 ), #98, .T. ) ;
#45235 = ORIENTED_EDGE ( 'NONE', *, *, #3118, .T. ) ;
#45236 = CARTESIAN_POINT ( 'NONE',  ( 96.15314808468748708, 91.99731107132950569, 85.62114583420046188 ) ) ;
#45237 = VERTEX_POINT ( 'NONE', #50075 ) ;
#45238 = CARTESIAN_POINT ( 'NONE',  ( 95.00000000000000000, -212.6630814284392557, 86.62656250086715204 ) ) ;
#45239 = APPLICATION_PROTOCOL_DEFINITION ( 'draft international standard', 'automotive_design', 1998, #9969 ) ;
#45240 = FACE_OUTER_BOUND ( 'NONE', #21149, .T. ) ;
#45241 = EDGE_CURVE ( 'NONE', #54986, #55937, #12060, .T. ) ;
#45242 = CIRCLE ( 'NONE', #47647, 82.00000000000000000 ) ;
#45243 = CARTESIAN_POINT ( 'NONE',  ( -93.67499999999998295, -207.7050326799711968, 80.26333333333332121 ) ) ;
#45244 = CARTESIAN_POINT ( 'NONE',  ( 10.00000000000000000, 0.000000000000000000, 0.000000000000000000 ) ) ;
#45245 = CYLINDRICAL_SURFACE ( 'NONE', #15142, 16.00000000000000000 ) ;
#45246 = CYLINDRICAL_SURFACE ( 'NONE', #31205, 37.49900000000000233 ) ;
#45247 = EDGE_CURVE ( 'NONE', #58433, #41314, #14527, .T. ) ;
#45248 = DIRECTION ( 'NONE',  ( 0.000000000000000000, 0.000000000000000000, 1.000000000000000000 ) ) ;
#45249 = EDGE_CURVE ( 'NONE', #44844, #47502, #58224, .T. ) ;
#45250 = CARTESIAN_POINT ( 'NONE',  ( -93.84685191531247028, -211.9973110713294489, 87.31447916753380412 ) ) ;
#45251 = CARTESIAN_POINT ( 'NONE',  ( -97.30629616937501680, 88.66845928578038638, 87.31447916753381833 ) ) ;
#45252 = ORIENTED_EDGE ( 'NONE', *, *, #5365, .F. ) ;
#45254 = CARTESIAN_POINT ( 'NONE',  ( -92.69370383062504004, 90.00000000000004263, 85.51531250086713953 ) ) ;
#45253 = CARTESIAN_POINT ( 'NONE',  ( 94.99999999999998579, 92.66308142843935514, 84.40406250086712703 ) ) ;
#45255 = ORIENTED_EDGE ( 'NONE', *, *, #7778, .T. ) ;
#45256 = CARTESIAN_POINT ( 'NONE',  ( 10.00000000000000000, 0.6853352020795618893, -37.58145647212453611 ) ) ;
#45257 = DIRECTION ( 'NONE',  ( 0.000000000000000000, 0.000000000000000000, 1.000000000000000000 ) ) ;
#45258 = CARTESIAN_POINT ( 'NONE',  ( 0.000000000000000000, -3.894527615418464705, 81.90746397400387480 ) ) ;
#45259 = CARTESIAN_POINT ( 'NONE',  ( 0.000000000000000000, 0.000000000000000000, 0.000000000000000000 ) ) ;
#45260 = CARTESIAN_POINT ( 'NONE',  ( -93.84685191531248449, -208.0026889286704943, 88.16114583420046813 ) ) ;
#45261 = DIRECTION ( 'NONE',  ( 1.000000000000000000, -0.000000000000000000, 0.000000000000000000 ) ) ;
#45262 = CARTESIAN_POINT ( 'NONE',  ( -7.469491406282094736, 4.756046723998911929, 52.00000000000002132 ) ) ;
#45263 = CARTESIAN_POINT ( 'NONE',  ( 12.00000000000000000, 23.49999999999999645, -1.500000000000003997 ) ) ;
#45264 = DIRECTION ( 'NONE',  ( 0.000000000000000000, 0.9510565162951544194, -0.3090169943749448422 ) ) ;
#45265 = EDGE_LOOP ( 'NONE', ( #8237, #59626, #14425, #52243 ) ) ;
#45266 = VECTOR ( 'NONE', #27364, 1000.000000000000000 ) ;
#45267 = EDGE_CURVE ( 'NONE', #63916, #38750, #38071, .T. ) ;
#45268 = ORIENTED_EDGE ( 'NONE', *, *, #20356, .T. ) ;
#45269 = EDGE_CURVE ( 'NONE', #37324, #4529, #70871, .T. ) ;
#45270 = CARTESIAN_POINT ( 'NONE',  ( -93.67500000000003979, 87.70503267997129626, 81.95666666666666345 ) ) ;
#45271 = DIRECTION ( 'NONE',  ( -0.000000000000000000, -0.000000000000000000, -1.000000000000000000 ) ) ;
#45272 = DIRECTION ( 'NONE',  ( 0.000000000000000000, 0.000000000000000000, -1.000000000000000000 ) ) ;
#45273 = CARTESIAN_POINT ( 'NONE',  ( 0.000000000000000000, 4.992566952384984269, 37.16516213103279398 ) ) ;
#45274 = FACE_OUTER_BOUND ( 'NONE', #73765, .T. ) ;
#45275 = CARTESIAN_POINT ( 'NONE',  ( -10.00000000000000000, 0.000000000000000000, 0.000000000000000000 ) ) ;
#45276 = CARTESIAN_POINT ( 'NONE',  ( 10.00000000000000000, 3.925862922256160736, 41.81611651403863306 ) ) ;
#45277 = FACE_OUTER_BOUND ( 'NONE', #47710, .T. ) ;
#45278 = CIRCLE ( 'NONE', #62060, 31.99999999999998224 ) ;
#45279 = ORIENTED_EDGE ( 'NONE', *, *, #21996, .F. ) ;
#45280 = CARTESIAN_POINT ( 'NONE',  ( -95.00000000000002842, 87.33691857156074434, 77.73656250086713726 ) ) ;
#45281 = CIRCLE ( 'NONE', #4495, 31.99999999999998224 ) ;
#45282 = FACE_OUTER_BOUND ( 'NONE', #59332, .T. ) ;
#45283 = EDGE_CURVE ( 'NONE', #44855, #32719, #11343, .T. ) ;
#45284 = EDGE_CURVE ( 'NONE', #13377, #22270, #12003, .T. ) ;
#45285 = CARTESIAN_POINT ( 'NONE',  ( 10.00000000000000000, 74.65491531819105830, 8.830959090343693418 ) ) ;
#45286 = FACE_OUTER_BOUND ( 'NONE', #29393, .T. ) ;
#45287 = VECTOR ( 'NONE', #18150, 1000.000000000000000 ) ;
#45288 = DIRECTION ( 'NONE',  ( 0.000000000000000000, 0.000000000000000000, -1.000000000000000000 ) ) ;
#45289 = CARTESIAN_POINT ( 'NONE',  ( 10.00000000000000000, -74.65491531819111515, -8.830959090343204920 ) ) ;
#45290 = FACE_OUTER_BOUND ( 'NONE', #45206, .T. ) ;
#45291 = CIRCLE ( 'NONE', #53634, 82.00000000000000000 ) ;
#45292 =( NAMED_UNIT ( * ) PLANE_ANGLE_UNIT ( ) SI_UNIT ( $, .RADIAN. ) );
#45293 = CIRCLE ( 'NONE', #22464, 42.00000000000000000 ) ;
#45294 = VECTOR ( 'NONE', #63231, 1000.000000000000000 ) ;
#45295 =( BOUNDED_CURVE ( )  B_SPLINE_CURVE ( 2, ( #41308, #29635, #64250, #42057, #13093, #46578, #7092 ),
 .UNSPECIFIED., .F., .F. ) 
 B_SPLINE_CURVE_WITH_KNOTS ( ( 3, 2, 2, 3 ),
 ( 0.8890265259358470784, 0.8960822236920598094, 0.9031379892329425285, 0.9101937466091534201 ),
 .UNSPECIFIED. ) 
 CURVE ( )  GEOMETRIC_REPRESENTATION_ITEM ( )  RATIONAL_B_SPLINE_CURVE ( ( 0.9999974258394741522, 0.8660266908770667404, 1.000000000000000000, 0.8660254037844387076, 1.000000000000000000, 0.8660254037844387076, 1.000000000000000000 ) ) 
 REPRESENTATION_ITEM ( '' )  );
#45296 = CARTESIAN_POINT ( 'NONE',  ( 97.30629616937498838, 91.33154071421968467, 76.83697916753382628 ) ) ;
#45297 = CARTESIAN_POINT ( 'NONE',  ( -93.84685191531248449, -208.0026889286704943, 79.42989583420049371 ) ) ;
#45298 = LINE ( 'NONE', #68217, #63867 ) ;
#45299 = ORIENTED_EDGE ( 'NONE', *, *, #3082, .T. ) ;
#45300 = DIRECTION ( 'NONE',  ( 0.000000000000000000, -0.5877852522924624790, -0.8090169943749553338 ) ) ;
#45301 = CARTESIAN_POINT ( 'NONE',  ( -97.64999999999996305, -209.9999999999999716, 76.03000000000000114 ) ) ;
#45302 = DIRECTION ( 'NONE',  ( -0.000000000000000000, -0.000000000000000000, -1.000000000000000000 ) ) ;
#45303 = VECTOR ( 'NONE', #60749, 1000.000000000000114 ) ;
#45304 = CARTESIAN_POINT ( 'NONE',  ( -92.69370383062505425, 88.66845928578038638, 78.00114583420049996 ) ) ;
#45305 = CARTESIAN_POINT ( 'NONE',  ( 95.00000000000000000, -212.6630814284392557, 79.00656250086713328 ) ) ;
#45306 = EDGE_LOOP ( 'NONE', ( #35999, #52795, #65235, #11731 ) ) ;
#45307 = AXIS2_PLACEMENT_3D ( 'NONE', #56498, #5739, #29378 ) ;
#45308 = CARTESIAN_POINT ( 'NONE',  ( 10.00000000000000000, 41.76106447765489094, 62.50884508063442269 ) ) ;
#45309 = ORIENTED_EDGE ( 'NONE', *, *, #30632, .T. ) ;
#45310 = LINE ( 'NONE', #16350, #29149 ) ;
#45311 = ORIENTED_EDGE ( 'NONE', *, *, #55835, .F. ) ;
#45312 = CARTESIAN_POINT ( 'NONE',  ( -2.500000000000014655, -69.70000000000001705, -204.9999999999999716 ) ) ;
#45313 = EDGE_LOOP ( 'NONE', ( #31677, #31160, #63077, #1363 ) ) ;
#45314 = VERTEX_POINT ( 'NONE', #68510 ) ;
#45315 = VERTEX_POINT ( 'NONE', #58325 ) ;
#45316 = CARTESIAN_POINT ( 'NONE',  ( 96.15314808468750130, -211.9973110713294489, 75.40822916753381833 ) ) ;
#45317 = ORIENTED_EDGE ( 'NONE', *, *, #34531, .F. ) ;
#45318 = CARTESIAN_POINT ( 'NONE',  ( 0.000000000000000000, -62.50329211542465657, 41.76937507738766442 ) ) ;
#45319 = CARTESIAN_POINT ( 'NONE',  ( -94.95306897617113862, 87.35041560265752025, 75.00000002508417651 ) ) ;
#45320 = CARTESIAN_POINT ( 'NONE',  ( 97.30629616937498838, 88.66845928578037217, 84.98614583420047097 ) ) ;
#45321 = AXIS2_PLACEMENT_3D ( 'NONE', #71682, #9279, #8916 ) ;
#45322 = PLANE ( 'NONE',  #42984 ) ;
#45323 = CARTESIAN_POINT ( 'NONE',  ( 97.64999999999997726, -211.5299782133524502, 77.56458333333333144 ) ) ;
#45324 = VECTOR ( 'NONE', #67245, 1000.000000000000114 ) ;
#45325 = ORIENTED_EDGE ( 'NONE', *, *, #13178, .T. ) ;
#45326 = VERTEX_POINT ( 'NONE', #35397 ) ;
#45327 = VERTEX_POINT ( 'NONE', #22267 ) ;
#45328 = EDGE_LOOP ( 'NONE', ( #33640, #58598, #9218, #2813 ) ) ;
#45329 = DIRECTION ( 'NONE',  ( -1.000000000000000000, -0.000000000000000000, -0.000000000000000000 ) ) ;
#45330 = DIRECTION ( 'NONE',  ( 0.000000000000000000, 0.000000000000000000, 1.000000000000000000 ) ) ;
#45331 = CIRCLE ( 'NONE', #46493, 32.00000000000000000 ) ;
#45332 = EDGE_CURVE ( 'NONE', #44183, #40306, #5366, .T. ) ;
#45333 = DIRECTION ( 'NONE',  ( -1.000000000000000000, -0.000000000000000000, -0.000000000000000000 ) ) ;
#45334 = CIRCLE ( 'NONE', #57342, 77.49900000000000944 ) ;
#45335 = CARTESIAN_POINT ( 'NONE',  ( 0.000000000000000000, 0.000000000000000000, 0.000000000000000000 ) ) ;
#45336 = DIRECTION ( 'NONE',  ( 0.000000000000000000, 0.000000000000000000, 1.000000000000000000 ) ) ;
#45337 = CARTESIAN_POINT ( 'NONE',  ( 0.000000000000000000, 35.92658777277525672, -10.74501242461245809 ) ) ;
#45339 = EDGE_LOOP ( 'NONE', ( #5571, #25135, #49101 ) ) ;
#45338 = EDGE_CURVE ( 'NONE', #55509, #69802, #28263, .T. ) ;
#45340 = CARTESIAN_POINT ( 'NONE',  ( -97.64999999999994884, -211.5299782133524502, 83.78229166840095843 ) ) ;
#45341 = VERTEX_POINT ( 'NONE', #853 ) ;
#45342 = DIRECTION ( 'NONE',  ( -1.000000000000000000, -0.000000000000000000, -0.000000000000000000 ) ) ;
#45343 = VERTEX_POINT ( 'NONE', #63617 ) ;
#45345 = CARTESIAN_POINT ( 'NONE',  ( -97.65000000000001990, 90.00000000000004263, 80.55437500173430010 ) ) ;
#45344 = CARTESIAN_POINT ( 'NONE',  ( 92.34999999999999432, 91.52997821335252127, 84.31145833506762699 ) ) ;
#45346 = ADVANCED_FACE ( 'NONE', ( #40295 ), #69237, .T. ) ;
#45347 = ORIENTED_EDGE ( 'NONE', *, *, #18672, .T. ) ;
#45348 = CARTESIAN_POINT ( 'NONE',  ( 94.99999999999998579, 87.33691857156068750, 82.97531250086716170 ) ) ;
#45349 = CARTESIAN_POINT ( 'NONE',  ( 11.99999999999999822, 51.03279382321166224, -55.19960302592011914 ) ) ;
#45350 = DIRECTION ( 'NONE',  ( 0.7950889364178796992, -0.6064928550163511956, 0.000000000000000000 ) ) ;
#45351 = CYLINDRICAL_SURFACE ( 'NONE', #44639, 82.00000000000000000 ) ;
#45352 = CYLINDRICAL_SURFACE ( 'NONE', #16241, 37.49900000000000233 ) ;
#45353 = ORIENTED_EDGE ( 'NONE', *, *, #65020, .T. ) ;
#45355 = EDGE_CURVE ( 'NONE', #59768, #59223, #7239, .T. ) ;
#45354 = DIRECTION ( 'NONE',  ( 0.000000000000000000, 0.000000000000000000, 1.000000000000000000 ) ) ;
#45356 = CARTESIAN_POINT ( 'NONE',  ( -15.70044424985254850, 0.001194404164626844313, -90.00000000000000000 ) ) ;
#45357 = DIRECTION ( 'NONE',  ( -1.000000000000000000, -0.000000000000000000, -0.000000000000000000 ) ) ;
#45358 = ORIENTED_EDGE ( 'NONE', *, *, #33153, .F. ) ;
#45359 = VECTOR ( 'NONE', #32985, 1000.000000000000000 ) ;
#45360 = ORIENTED_EDGE ( 'NONE', *, *, #12247, .F. ) ;
#45361 = EDGE_CURVE ( 'NONE', #26842, #22221, #5733, .T. ) ;
#45362 = CARTESIAN_POINT ( 'NONE',  ( -94.95306897617061281, -212.6495843973424655, 75.00000002508416230 ) ) ;
#45363 = CIRCLE ( 'NONE', #28530, 77.49899999999999523 ) ;
#45364 = ADVANCED_FACE ( 'NONE', ( #52312 ), #69607, .T. ) ;
#45365 = CARTESIAN_POINT ( 'NONE',  ( 11.99999999999999822, 46.54456581323888997, -59.03342792756214408 ) ) ;
#45366 = CARTESIAN_POINT ( 'NONE',  ( 92.69370383062498320, 90.00000000000002842, 89.80156250086714920 ) ) ;
#45367 = DIRECTION ( 'NONE',  ( 0.000000000000000000, 0.000000000000000000, 1.000000000000000000 ) ) ;
#45368 = CARTESIAN_POINT ( 'NONE',  ( -96.15314808468745866, -211.9973110713294489, 80.38239583420048007 ) ) ;
#45369 = EDGE_LOOP ( 'NONE', ( #11482, #59375, #9255, #53101 ) ) ;
#45370 = CARTESIAN_POINT ( 'NONE',  ( -92.69370383062502583, 91.33154071421968467, 87.47322916753381605 ) ) ;
#45371 = ORIENTED_EDGE ( 'NONE', *, *, #44559, .T. ) ;
#45372 = CYLINDRICAL_SURFACE ( 'NONE', #54712, 2.649999999999985700 ) ;
#45373 = ADVANCED_FACE ( 'NONE', ( #74130 ), #33630, .T. ) ;
#45374 = ADVANCED_FACE ( 'NONE', ( #39936 ), #1276, .T. ) ;
#45375 = CARTESIAN_POINT ( 'NONE',  ( -97.44941226939890555, -210.6792855350397815, 74.93153462041274793 ) ) ;
#45376 = CARTESIAN_POINT ( 'NONE',  ( 11.99999999999999822, 55.19960302592141232, -51.03279382321027668 ) ) ;
#45377 = DIRECTION ( 'NONE',  ( -1.000000000000000000, 0.000000000000000000, -0.000000000000000000 ) ) ;
#45378 = DIRECTION ( 'NONE',  ( 0.000000000000000000, 0.5224985647159500202, -0.8526401643540915121 ) ) ;
#45379 = CARTESIAN_POINT ( 'NONE',  ( 11.99999999999999822, -55.19960302592029677, -51.03279382321147750 ) ) ;
#45380 = DIRECTION ( 'NONE',  ( -0.000000000000000000, -0.000000000000000000, 1.000000000000000000 ) ) ;
#45381 = DIRECTION ( 'NONE',  ( 0.000000000000000000, 0.8910065241883655673, 0.4539904997395510233 ) ) ;
#45382 = DIRECTION ( 'NONE',  ( -1.000000000000000000, 0.000000000000000000, 0.000000000000000000 ) ) ;
#45383 = CARTESIAN_POINT ( 'NONE',  ( 0.000000000000000000, -78.73519480814971416, 22.90783923731599359 ) ) ;
#45384 = LINE ( 'NONE', #22441, #46843 ) ;
#45385 = CARTESIAN_POINT ( 'NONE',  ( 94.99999999999998579, 87.33691857156068750, 89.32531250086715602 ) ) ;
#45386 = CIRCLE ( 'NONE', #12929, 21.00000000000000000 ) ;
#45387 = CARTESIAN_POINT ( 'NONE',  ( -96.15314808468747287, -208.0026889286704943, 89.06072916753382174 ) ) ;
#45388 = LINE ( 'NONE', #29171, #61443 ) ;
#45389 = EDGE_LOOP ( 'NONE', ( #58991, #5391, #48668, #64482 ) ) ;
#45390 = DIRECTION ( 'NONE',  ( 0.000000000000000000, 0.1564344650402244852, 0.9876883405951387696 ) ) ;
#45391 = CARTESIAN_POINT ( 'NONE',  ( -92.69370383062505425, 88.66845928578038638, 79.11239583420046984 ) ) ;
#45392 = CARTESIAN_POINT ( 'NONE',  ( -92.35000000000306386, -210.0000040461925437, 77.06187486178056645 ) ) ;
#45393 = VERTEX_POINT ( 'NONE', #41048 ) ;
#45394 = CARTESIAN_POINT ( 'NONE',  ( 92.35000000000000853, -209.9999999999999716, 79.91937500173429498 ) ) ;
#45395 = CARTESIAN_POINT ( 'NONE',  ( -1.200000000000000030E-05, 16.95692799528845640, -2.500000000000000000 ) ) ;
#45396 = CARTESIAN_POINT ( 'NONE',  ( 0.000000000000000000, -17.67226234102849958, 33.17418723428301774 ) ) ;
#45397 = DIRECTION ( 'NONE',  ( -2.628368902995164490E-16, -1.000000000000000000, 0.000000000000000000 ) ) ;
#45398 = CARTESIAN_POINT ( 'NONE',  ( 97.30629616937498838, -208.6684592857803011, 74.93197916753381094 ) ) ;
#45399 = CIRCLE ( 'NONE', #53757, 37.49900000000000944 ) ;
#45400 = CONICAL_SURFACE ( 'NONE', #20148, 20.64000000000000057, 0.7853981633974482790 ) ;
#45401 = ORIENTED_EDGE ( 'NONE', *, *, #3954, .F. ) ;
#45402 = ADVANCED_FACE ( 'NONE', ( #45207 ), #11706, .T. ) ;
#45403 = ORIENTED_EDGE ( 'NONE', *, *, #57887, .F. ) ;
#45404 = VECTOR ( 'NONE', #17828, 1000.000000000000000 ) ;
#45406 = EDGE_CURVE ( 'NONE', #48817, #15890, #25270, .T. ) ;
#45405 = AXIS2_PLACEMENT_3D ( 'NONE', #31295, #25661, #54249 ) ;
#45407 = DIRECTION ( 'NONE',  ( 2.603472992746261562E-14, 2.546204323184492723E-14, -1.000000000000000000 ) ) ;
#45408 = CARTESIAN_POINT ( 'NONE',  ( 10.00000000000000000, -17.67226234102849958, 33.17418723428301774 ) ) ;
#45409 = EDGE_CURVE ( 'NONE', #9559, #37478, #29008, .T. ) ;
#45410 = CYLINDRICAL_SURFACE ( 'NONE', #17248, 16.00000000000000000 ) ;
#45411 = DIRECTION ( 'NONE',  ( 0.000000000000000000, 0.000000000000000000, 1.000000000000000000 ) ) ;
#45412 = CARTESIAN_POINT ( 'NONE',  ( 97.65000000000000568, -211.5299782133524218, 82.08895833506764461 ) ) ;
#45413 = CARTESIAN_POINT ( 'NONE',  ( 96.32499999999998863, -212.2949673200287179, 88.30666666666665776 ) ) ;
#45414 = ADVANCED_FACE ( 'NONE', ( #56854 ), #51940, .T. ) ;
#45415 = VERTEX_POINT ( 'NONE', #58697 ) ;
#45416 = ORIENTED_EDGE ( 'NONE', *, *, #8009, .T. ) ;
#45417 = CARTESIAN_POINT ( 'NONE',  ( -97.65000000000000568, 90.00003728274772641, 81.18937371225271704 ) ) ;
#45418 = ORIENTED_EDGE ( 'NONE', *, *, #578, .F. ) ;
#45419 = EDGE_LOOP ( 'NONE', ( #13298, #19488, #69630, #62830 ) ) ;
#45420 = DIRECTION ( 'NONE',  ( -0.1850432970638682395, 0.9827303690289280746, 0.000000000000000000 ) ) ;
#45421 = EDGE_CURVE ( 'NONE', #54824, #56357, #19206, .T. ) ;
#45422 = CYLINDRICAL_SURFACE ( 'NONE', #30482, 77.49899999999999523 ) ;
#45423 = ORIENTED_EDGE ( 'NONE', *, *, #34441, .T. ) ;
#45424 = DIRECTION ( 'NONE',  ( -1.000000000000000000, -0.000000000000000000, -0.000000000000000000 ) ) ;
#45425 = CARTESIAN_POINT ( 'NONE',  ( 93.67500000000001137, -212.2949673200287179, 75.58020833506763836 ) ) ;
#45426 = CARTESIAN_POINT ( 'NONE',  ( 97.64999999999997726, 88.47002178664753558, 82.00958333333332462 ) ) ;
#45427 = ORIENTED_EDGE ( 'NONE', *, *, #72462, .T. ) ;
#45428 = DIRECTION ( 'NONE',  ( -1.000000000000000000, -0.000000000000000000, -0.000000000000000000 ) ) ;
#45429 = ORIENTED_EDGE ( 'NONE', *, *, #44137, .F. ) ;
#45430 = LINE ( 'NONE', #62734, #3805 ) ;
#45431 = ORIENTED_EDGE ( 'NONE', *, *, #57494, .F. ) ;
#45432 = CARTESIAN_POINT ( 'NONE',  ( -93.67500000000003979, 92.29496732002878900, 88.59770833506763665 ) ) ;
#45433 = CARTESIAN_POINT ( 'NONE',  ( -95.00000000000002842, 87.33691857156074434, 82.34031250086714238 ) ) ;
#45434 = EDGE_CURVE ( 'NONE', #38362, #66220, #34874, .T. ) ;
#45435 = AXIS2_PLACEMENT_3D ( 'NONE', #55854, #38937, #50574 ) ;
#45436 = CARTESIAN_POINT ( 'NONE',  ( 97.30629616937498838, 91.33154071421968467, 78.58322916753381548 ) ) ;
#45437 = ORIENTED_EDGE ( 'NONE', *, *, #42616, .T. ) ;
#45438 = DIRECTION ( 'NONE',  ( 0.000000000000000000, -0.9510565162951500895, -0.3090169943749581649 ) ) ;
#45439 = CARTESIAN_POINT ( 'NONE',  ( -97.64999999999997726, -209.9999999999999716, 75.00000000000000000 ) ) ;
#45440 = CARTESIAN_POINT ( 'NONE',  ( 92.35003969675449298, 88.46999886771558863, 88.86229325377449584 ) ) ;
#45441 = CARTESIAN_POINT ( 'NONE',  ( 10.00000000000000000, 35.92658777277525672, -10.74501242461245809 ) ) ;
#45442 = VERTEX_POINT ( 'NONE', #13561 ) ;
#45443 = CARTESIAN_POINT ( 'NONE',  ( 5.000000000000000000, -59.75363087400035056, -56.15606465355021015 ) ) ;
#45444 = CARTESIAN_POINT ( 'NONE',  ( -93.84685191531248449, -208.0026889286704943, 77.36614583420046642 ) ) ;
#45445 = ORIENTED_EDGE ( 'NONE', *, *, #48775, .T. ) ;
#45446 = CIRCLE ( 'NONE', #70566, 20.99999999999999645 ) ;
#45447 = EDGE_LOOP ( 'NONE', ( #42092, #50814, #64453, #40154 ) ) ;
#45448 = AXIS2_PLACEMENT_3D ( 'NONE', #16054, #25214, #47759 ) ;
#45449 = DIRECTION ( 'NONE',  ( -0.7071067811865474617, 8.659560562354932858E-17, -0.7071067811865474617 ) ) ;
#45450 = EDGE_CURVE ( 'NONE', #60769, #6114, #3667, .T. ) ;
#45451 = EDGE_LOOP ( 'NONE', ( #4872, #29315, #23009, #45896 ) ) ;
#45452 = EDGE_CURVE ( 'NONE', #6488, #46015, #49137, .T. ) ;
#45453 = CARTESIAN_POINT ( 'NONE',  ( -7.400000000000021672, -2.546381662934748895E-13, -22.90000000000042490 ) ) ;
#45454 = CARTESIAN_POINT ( 'NONE',  ( -6.170112525937310188, 10.87104923258429068, 125.0000000000000000 ) ) ;
#45455 = ORIENTED_EDGE ( 'NONE', *, *, #33286, .T. ) ;
#45456 = CARTESIAN_POINT ( 'NONE',  ( -93.84685191531248449, -208.0026889286704943, 89.58989583420049030 ) ) ;
#45457 = EDGE_LOOP ( 'NONE', ( #63564, #63477, #60011, #73204 ) ) ;
#45458 = CARTESIAN_POINT ( 'NONE',  ( -92.35000000000003695, -208.4700217866474077, 81.48041666666665606 ) ) ;
#45459 = CARTESIAN_POINT ( 'NONE',  ( 10.00000000000000000, -26.08949754953044220, 27.05870788708222818 ) ) ;
#45460 = LINE ( 'NONE', #10861, #36944 ) ;
#45461 = DIRECTION ( 'NONE',  ( 0.000000000000000000, 0.000000000000000000, -1.000000000000000000 ) ) ;
#45462 = AXIS2_PLACEMENT_3D ( 'NONE', #17813, #13283, #41134 ) ;
#45463 = CARTESIAN_POINT ( 'NONE',  ( 12.50000000000000000, -132.5000000000000000, 40.00000000000000000 ) ) ;
#45464 = AXIS2_PLACEMENT_3D ( 'NONE', #24503, #47440, #36152 ) ;
#45465 = CARTESIAN_POINT ( 'NONE',  ( 92.35000000000000853, -209.9999999999999716, 86.26937500173430351 ) ) ;
#45467 = CIRCLE ( 'NONE', #1045, 16.00000000000000000 ) ;
#45466 = CARTESIAN_POINT ( 'NONE',  ( 96.15314808468748708, 91.99731107132950569, 86.25614583420048120 ) ) ;
#45468 = DIRECTION ( 'NONE',  ( 1.000000000000000000, 0.000000000000000000, 0.000000000000000000 ) ) ;
#45469 = DIRECTION ( 'NONE',  ( 0.000000000000000000, 0.000000000000000000, 1.000000000000000000 ) ) ;
#45470 = DIRECTION ( 'NONE',  ( -0.7273375899149793211, 0.6862798483830554463, 0.000000000000000000 ) ) ;
#45471 = AXIS2_PLACEMENT_3D ( 'NONE', #12558, #29836, #5832 ) ;
#45472 = LINE ( 'NONE', #22908, #13546 ) ;
#45473 = FACE_BOUND ( 'NONE', #6743, .T. ) ;
#45474 = CARTESIAN_POINT ( 'NONE',  ( 1.324703144935786447, 5.008684974571240289, -0.8655517945778323785 ) ) ;
#45475 = DIRECTION ( 'NONE',  ( 1.000000000000000000, 0.000000000000000000, -0.000000000000000000 ) ) ;
#45476 = COLOUR_RGB ( '', 0.31764706, 0.68627451, 0.89019608) ;
#45477 = DIRECTION ( 'NONE',  ( 0.000000000000000000, 0.9510565162951521989, 0.3090169943749515591 ) ) ;
#45478 = DIRECTION ( 'NONE',  ( 0.000000000000000000, 0.000000000000000000, -1.000000000000000000 ) ) ;
#45479 = CARTESIAN_POINT ( 'NONE',  ( 12.00000000000000000, -10.45096189432344502, -21.10159698893425784 ) ) ;
#45480 = CARTESIAN_POINT ( 'NONE',  ( 20.85212586905262100, -130.9402397935870965, 5.500000000000000000 ) ) ;
#45481 = DIRECTION ( 'NONE',  ( -1.000000000000000000, -0.000000000000000000, -0.000000000000000000 ) ) ;
#45482 = CARTESIAN_POINT ( 'NONE',  ( -93.67499999999998295, -212.2949673200287179, 83.86166666666666458 ) ) ;
#45483 = EDGE_CURVE ( 'NONE', #20649, #72017, #19566, .T. ) ;
#45484 = DIRECTION ( 'NONE',  ( -1.000000000000000000, 0.000000000000000000, 0.000000000000000000 ) ) ;
#45485 = ORIENTED_EDGE ( 'NONE', *, *, #47204, .F. ) ;
#45486 = CIRCLE ( 'NONE', #14331, 31.99999999999999645 ) ;
#45487 = DIRECTION ( 'NONE',  ( -1.000000000000000000, -0.000000000000000000, -0.000000000000000000 ) ) ;
#45488 = DIRECTION ( 'NONE',  ( 0.000000000000000000, 0.000000000000000000, 1.000000000000000000 ) ) ;
#45489 = DIRECTION ( 'NONE',  ( 0.9997280174009349762, -0.02332147558787671729, 0.000000000000000000 ) ) ;
#45490 = AXIS2_PLACEMENT_3D ( 'NONE', #41120, #70776, #70035 ) ;
#45491 = DIRECTION ( 'NONE',  ( -1.000000000000000000, -0.000000000000000000, -0.000000000000000000 ) ) ;
#45492 = CARTESIAN_POINT ( 'NONE',  ( 97.30629616937498838, -208.6684592857803011, 85.09197916753380753 ) ) ;
#45493 = CIRCLE ( 'NONE', #64693, 2.445500000000000007 ) ;
#45494 = AXIS2_PLACEMENT_3D ( 'NONE', #21041, #71426, #43993 ) ;
#45495 = ORIENTED_EDGE ( 'NONE', *, *, #6199, .T. ) ;
#45496 = ADVANCED_FACE ( 'NONE', ( #36127 ), #48517, .T. ) ;
#45497 = VERTEX_POINT ( 'NONE', #42156 ) ;
#45498 = EDGE_CURVE ( 'NONE', #11957, #52503, #65459, .T. ) ;
#45499 = EDGE_LOOP ( 'NONE', ( #50140, #53439, #50759, #23755 ) ) ;
#45500 = DIRECTION ( 'NONE',  ( 1.000000000000000000, 0.000000000000000000, 0.000000000000000000 ) ) ;
#45501 = CARTESIAN_POINT ( 'NONE',  ( 96.15314808468748708, -208.0026889286704943, 79.90614583420047268 ) ) ;
#45502 = ORIENTED_EDGE ( 'NONE', *, *, #5552, .F. ) ;
#45503 = CARTESIAN_POINT ( 'NONE',  ( 96.15314808468750130, -211.9973110713294489, 83.02822916753380866 ) ) ;
#45504 = EDGE_CURVE ( 'NONE', #62152, #36870, #30478, .T. ) ;
#45505 = EDGE_CURVE ( 'NONE', #64894, #35896, #8295, .T. ) ;
#45506 = VERTEX_POINT ( 'NONE', #53425 ) ;
#45507 = PLANE ( 'NONE',  #63541 ) ;
#45508 = VERTEX_POINT ( 'NONE', #13923 ) ;
#45509 = VERTEX_POINT ( 'NONE', #53788 ) ;
#45510 = CARTESIAN_POINT ( 'NONE',  ( -92.69370383062502583, 91.33154071421968467, 74.93197916753381094 ) ) ;
#45511 = CIRCLE ( 'NONE', #44317, 15.69999999999999929 ) ;
#45512 = FACE_OUTER_BOUND ( 'NONE', #55553, .T. ) ;
#45513 = AXIS2_PLACEMENT_3D ( 'NONE', #12466, #863, #23394 ) ;
#45514 = ORIENTED_EDGE ( 'NONE', *, *, #69412, .F. ) ;
#45515 = CARTESIAN_POINT ( 'NONE',  ( 15.69955575014744831, 0.001194404164628767254, -85.59999999999999432 ) ) ;
#45516 = CARTESIAN_POINT ( 'NONE',  ( 96.32499999999998863, -212.2949673200287179, 88.38604166840097776 ) ) ;
#45517 = CIRCLE ( 'NONE', #17857, 42.00000000000000000 ) ;
#45518 = ORIENTED_EDGE ( 'NONE', *, *, #36133, .F. ) ;
#45519 = CARTESIAN_POINT ( 'NONE',  ( 0.000000000000000000, 0.000000000000000000, 52.00000000000002132 ) ) ;
#45520 = VERTEX_POINT ( 'NONE', #71436 ) ;
#45521 = AXIS2_PLACEMENT_3D ( 'NONE', #61103, #26874, #37445 ) ;
#45522 =( BOUNDED_CURVE ( )  B_SPLINE_CURVE ( 2, ( #54128, #29687, #30430, #24803, #7882, #47733, #52636 ),
 .UNSPECIFIED., .F., .F. ) 
 B_SPLINE_CURVE_WITH_KNOTS ( ( 3, 2, 2, 3 ),
 ( 0.5208333333333332593, 0.5277777777777776791, 0.5347222222222220989, 0.5416666666666665186 ),
 .UNSPECIFIED. ) 
 CURVE ( )  GEOMETRIC_REPRESENTATION_ITEM ( )  RATIONAL_B_SPLINE_CURVE ( ( 1.000000000000002220, 0.8660254037844365982, 1.000000000000000000, 0.8660254037844387076, 1.000000000000000000, 0.8660254037844408170, 0.9999999999999978906 ) ) 
 REPRESENTATION_ITEM ( '' )  );
#45523 = DIRECTION ( 'NONE',  ( 0.000000000000000000, 0.000000000000000000, 1.000000000000000000 ) ) ;
#45524 = EDGE_CURVE ( 'NONE', #10395, #75, #48157, .T. ) ;
#45525 = ORIENTED_EDGE ( 'NONE', *, *, #52344, .F. ) ;
#45526 = ORIENTED_EDGE ( 'NONE', *, *, #48734, .F. ) ;
#45527 = ORIENTED_EDGE ( 'NONE', *, *, #17612, .F. ) ;
#45528 = LINE ( 'NONE', #34589, #69306 ) ;
#45529 = ITEM_DEFINED_TRANSFORMATION ( 'NONE', 'NONE', #11171,  #43395 ) ;
#45530 = CYLINDRICAL_SURFACE ( 'NONE', #654, 31.99999999999999289 ) ;
#45531 = ORIENTED_EDGE ( 'NONE', *, *, #36471, .T. ) ;
#45532 = ORIENTED_EDGE ( 'NONE', *, *, #42982, .T. ) ;
#45533 = EDGE_LOOP ( 'NONE', ( #42367, #7485, #12411, #41106 ) ) ;
#45534 = CARTESIAN_POINT ( 'NONE',  ( 0.000000000000000000, 41.76106447765489094, 62.50884508063442269 ) ) ;
#45535 = CARTESIAN_POINT ( 'NONE',  ( 10.00000000000000000, -65.64334221924939072, 41.19522573413710376 ) ) ;
#45537 = CARTESIAN_POINT ( 'NONE',  ( -96.15314808468752972, 91.99731107132950569, 75.72572916753382799 ) ) ;
#45536 = VECTOR ( 'NONE', #1636, 1000.000000000000114 ) ;
#45538 = EDGE_CURVE ( 'NONE', #5740, #3181, #24845, .T. ) ;
#45539 = VERTEX_POINT ( 'NONE', #7194 ) ;
#45540 = CARTESIAN_POINT ( 'NONE',  ( 92.69370383062498320, 91.33154071421968467, 75.61989583420047722 ) ) ;
#45541 = ORIENTED_EDGE ( 'NONE', *, *, #30194, .T. ) ;
#45542 = CARTESIAN_POINT ( 'NONE',  ( 97.64999999997404245, -210.0000117261773198, 82.77687459617033028 ) ) ;
#45543 = CARTESIAN_POINT ( 'NONE',  ( -92.69370383062498320, -211.3315407142195852, 86.73239583420047438 ) ) ;
#45544 = ORIENTED_EDGE ( 'NONE', *, *, #56807, .F. ) ;
#45545 = AXIS2_PLACEMENT_3D ( 'NONE', #38769, #55316, #14719 ) ;
#45546 = EDGE_CURVE ( 'NONE', #25482, #29219, #47778, .T. ) ;
#45547 = FACE_OUTER_BOUND ( 'NONE', #24663, .T. ) ;
#45548 = CARTESIAN_POINT ( 'NONE',  ( 94.20702885560676521, -212.5043059284880087, 74.98272308147871001 ) ) ;
#45549 = LINE ( 'NONE', #10949, #930 ) ;
#45550 = DIRECTION ( 'NONE',  ( -1.000000000000000000, 0.000000000000000000, 0.000000000000000000 ) ) ;
#45551 = CIRCLE ( 'NONE', #2362, 37.49900000000000233 ) ;
#45552 = VECTOR ( 'NONE', #6719, 1000.000000000000000 ) ;
#45553 = VECTOR ( 'NONE', #59295, 1000.000000000000000 ) ;
#45554 = LINE ( 'NONE', #40635, #48228 ) ;
#45555 = CARTESIAN_POINT ( 'NONE',  ( 0.000000000000000000, 51.29473840253223216, 63.97538442413444670 ) ) ;
#45556 = DIRECTION ( 'NONE',  ( 0.000000000000000000, 0.000000000000000000, 1.000000000000000000 ) ) ;
#45557 = CIRCLE ( 'NONE', #13101, 77.49899999999998101 ) ;
#45558 = CARTESIAN_POINT ( 'NONE',  ( 11.99999999999999822, 74.65491531819118620, 23.16904090965732621 ) ) ;
#45559 = CARTESIAN_POINT ( 'NONE',  ( 94.56602944578247616, -207.6412937382897894, 74.84690984288795335 ) ) ;
#45560 = CARTESIAN_POINT ( 'NONE',  ( -95.00000000000002842, 87.33691857156074434, 83.45156250086714067 ) ) ;
#45561 = CARTESIAN_POINT ( 'NONE',  ( 2.499999999999984457, -73.00000000000001421, -255.0000000000000000 ) ) ;
#45562 = CARTESIAN_POINT ( 'NONE',  ( 10.00000000000000000, -20.41045688087876897, 72.35160999960810102 ) ) ;
#45563 = ORIENTED_EDGE ( 'NONE', *, *, #20263, .T. ) ;
#45564 = CARTESIAN_POINT ( 'NONE',  ( 97.64999999999999147, 90.00000015433757028, 79.60187500750917877 ) ) ;
#45565 = FACE_OUTER_BOUND ( 'NONE', #73499, .T. ) ;
#45567 = FACE_OUTER_BOUND ( 'NONE', #9130, .T. ) ;
#45566 = VECTOR ( 'NONE', #56012, 1000.000000000000000 ) ;
#45568 = CARTESIAN_POINT ( 'NONE',  ( 5.000000000000000000, 21.40280677340421889, -36.13751322684397138 ) ) ;
#45569 = CYLINDRICAL_SURFACE ( 'NONE', #34577, 15.80000000000028315 ) ;
#45570 = LINE ( 'NONE', #52667, #50950 ) ;
#45571 = CARTESIAN_POINT ( 'NONE',  ( -97.30629616937497417, -211.3315407142195852, 80.96447916753382401 ) ) ;
#45572 = VECTOR ( 'NONE', #51493, 1000.000000000000114 ) ;
#45573 = AXIS2_PLACEMENT_3D ( 'NONE', #47409, #70314, #71424 ) ;
#45574 = DIRECTION ( 'NONE',  ( 1.000000000000000000, 0.000000000000000000, 0.000000000000000000 ) ) ;
#45575 =( REPRESENTATION_RELATIONSHIP ('NONE','NONE', #31117, #8524 ) REPRESENTATION_RELATIONSHIP_WITH_TRANSFORMATION ( #23050 )SHAPE_REPRESENTATION_RELATIONSHIP( ) );
#45576 = EDGE_CURVE ( 'NONE', #45217, #46805, #64347, .T. ) ;
#45577 = EDGE_LOOP ( 'NONE', ( #8875, #33459 ) ) ;
#45578 = CARTESIAN_POINT ( 'NONE',  ( 0.000000000000000000, -120.0000000000000000, 2.500000000000000000 ) ) ;
#45579 = CARTESIAN_POINT ( 'NONE',  ( -92.35000000000005116, 88.47002178664754979, 80.81895833506763438 ) ) ;
#45580 = LINE ( 'NONE', #33905, #4575 ) ;
#45581 = CARTESIAN_POINT ( 'NONE',  ( -26.29030328629083968, -123.6496510949466341, 5.500000000000000000 ) ) ;
#45582 = DIRECTION ( 'NONE',  ( 0.000000000000000000, 0.000000000000000000, 1.000000000000000000 ) ) ;
#45583 = EDGE_CURVE ( 'NONE', #54917, #7348, #26322, .T. ) ;
#45584 = EDGE_CURVE ( 'NONE', #26049, #17019, #18461, .T. ) ;
#45585 = FACE_OUTER_BOUND ( 'NONE', #52518, .T. ) ;
#45586 = ORIENTED_EDGE ( 'NONE', *, *, #60553, .T. ) ;
#45587 = DIRECTION ( 'NONE',  ( -1.000000000000000000, 0.000000000000000000, 0.000000000000000000 ) ) ;
#45588 = DIRECTION ( 'NONE',  ( -1.000000000000000000, -0.000000000000000000, -0.000000000000000000 ) ) ;
#45589 = ORIENTED_EDGE ( 'NONE', *, *, #44073, .T. ) ;
#45590 = CARTESIAN_POINT ( 'NONE',  ( 95.00000000000000000, -207.3369185715606307, 89.48406250086713953 ) ) ;
#45591 = CARTESIAN_POINT ( 'NONE',  ( 11.99999999999999822, -71.91182617369207719, 28.89263327155721228 ) ) ;
#45592 = VERTEX_POINT ( 'NONE', #35747 ) ;
#45593 = VECTOR ( 'NONE', #14195, 999.9999999999998863 ) ;
#45594 = DIRECTION ( 'NONE',  ( 2.603472992746261562E-14, 2.546204323184492723E-14, -1.000000000000000000 ) ) ;
#45595 = EDGE_CURVE ( 'NONE', #4573, #67765, #30111, .T. ) ;
#45596 = EDGE_LOOP ( 'NONE', ( #15821, #27196, #43212, #72864 ) ) ;
#45597 = CARTESIAN_POINT ( 'NONE',  ( -97.64998927049083477, -208.4700155919624933, 84.94645790656207396 ) ) ;
#45598 = ORIENTED_EDGE ( 'NONE', *, *, #35040, .T. ) ;
#45599 = DIRECTION ( 'NONE',  ( 0.000000000000000000, 0.000000000000000000, 1.000000000000000000 ) ) ;
#45600 = VERTEX_POINT ( 'NONE', #24482 ) ;
#45601 = DIRECTION ( 'NONE',  ( 0.000000000000000000, -0.9969173337331287410, 0.07845909572783489605 ) ) ;
#45602 = ORIENTED_EDGE ( 'NONE', *, *, #70971, .F. ) ;
#45603 = CIRCLE ( 'NONE', #26362, 77.49900000000002365 ) ;
#45604 = EDGE_LOOP ( 'NONE', ( #53543, #70820, #2425, #30007 ) ) ;
#45605 = DIRECTION ( 'NONE',  ( -1.000000000000000000, 0.000000000000000000, 0.000000000000000000 ) ) ;
#45606 = VERTEX_POINT ( 'NONE', #1960 ) ;
#45607 = EDGE_CURVE ( 'NONE', #19859, #55964, #70696, .T. ) ;
#45608 = ORIENTED_EDGE ( 'NONE', *, *, #39063, .F. ) ;
#45609 = CARTESIAN_POINT ( 'NONE',  ( 92.34999999999999432, 91.52997821335252127, 89.94708333333333883 ) ) ;
#45610 = CARTESIAN_POINT ( 'NONE',  ( 15.50000000000000000, 0.000000000000000000, -4.400000000000001243 ) ) ;
#45611 = EDGE_CURVE ( 'NONE', #56976, #24230, #68373, .T. ) ;
#45612 = LINE ( 'NONE', #17022, #46519 ) ;
#45613 = ORIENTED_EDGE ( 'NONE', *, *, #46962, .T. ) ;
#45615 = VERTEX_POINT ( 'NONE', #14675 ) ;
#45614 = AXIS2_PLACEMENT_3D ( 'NONE', #53662, #12326, #53292 ) ;
#45616 = EDGE_LOOP ( 'NONE', ( #3643, #12328, #8310, #57165 ) ) ;
#45617 = CARTESIAN_POINT ( 'NONE',  ( 97.30629616937498838, 91.33154071421968467, 83.66322916753379957 ) ) ;
#45619 = EDGE_LOOP ( 'NONE', ( #32395, #14694, #65204, #57354 ) ) ;
#45618 = EDGE_CURVE ( 'NONE', #54954, #56201, #15043, .T. ) ;
#45620 = CARTESIAN_POINT ( 'NONE',  ( 96.15314808468748708, -208.0026889286704943, 86.89114583420047211 ) ) ;
#45621 = CIRCLE ( 'NONE', #63598, 23.50000000000489919 ) ;
#45622 = AXIS2_PLACEMENT_3D ( 'NONE', #33685, #56639, #5138 ) ;
#45623 = PRODUCT_CONTEXT ( 'NONE', #33461, 'mechanical' ) ;
#45624 = CARTESIAN_POINT ( 'NONE',  ( -97.64999999999996305, -209.9999627172523446, 81.18937371225273125 ) ) ;
#45625 = CARTESIAN_POINT ( 'NONE',  ( 5.250000000000000000, -13.95926121303099343, -1.199999999999999956 ) ) ;
#45626 = CARTESIAN_POINT ( 'NONE',  ( 0.000000000000000000, 0.000000000000000000, 0.000000000000000000 ) ) ;
#45627 = CARTESIAN_POINT ( 'NONE',  ( 0.000000000000000000, 39.78640506895700213, -66.50666863321957578 ) ) ;
#45628 = DIRECTION ( 'NONE',  ( 0.9435911131814398445, -0.3311129884571295534, 0.000000000000000000 ) ) ;
#45629 = AXIS2_PLACEMENT_3D ( 'NONE', #30959, #25702, #19682 ) ;
#45630 = CYLINDRICAL_SURFACE ( 'NONE', #62326, 31.99999999999999289 ) ;
#45631 = AXIS2_PLACEMENT_3D ( 'NONE', #10506, #33429, #73655 ) ;
#45632 = CARTESIAN_POINT ( 'NONE',  ( -92.69370383062498320, -211.3315407142195852, 86.09739583420048348 ) ) ;
#45633 = CARTESIAN_POINT ( 'NONE',  ( -92.69370383062502583, 91.33154071421968467, 85.09197916753380753 ) ) ;
#45634 = EDGE_CURVE ( 'NONE', #52314, #32720, #62368, .T. ) ;
#45635 = ORIENTED_EDGE ( 'NONE', *, *, #67376, .F. ) ;
#45637 = CARTESIAN_POINT ( 'NONE',  ( -96.15314808468752972, 91.99731107132950569, 84.45697916753380241 ) ) ;
#45636 = CARTESIAN_POINT ( 'NONE',  ( 93.84685191531248449, 91.99731107132950569, 83.82197916753381151 ) ) ;
#45638 = ORIENTED_EDGE ( 'NONE', *, *, #36187, .T. ) ;
#45639 = CARTESIAN_POINT ( 'NONE',  ( 0.000000000000000000, -6.903761155838323837, 77.19088730480521576 ) ) ;
#45640 = PLANE ( 'NONE',  #70945 ) ;
#45641 = LINE ( 'NONE', #73434, #15136 ) ;
#45642 = CARTESIAN_POINT ( 'NONE',  ( 92.34999999999999432, 90.00000000000002842, 87.45999999999999375 ) ) ;
#45643 = CARTESIAN_POINT ( 'NONE',  ( -94.99999999999997158, -212.6630814284392557, 86.62656250086713783 ) ) ;
#45644 = CARTESIAN_POINT ( 'NONE',  ( -93.67499999999998295, -212.2949673200287179, 81.95666666666666345 ) ) ;
#45645 = CARTESIAN_POINT ( 'NONE',  ( -93.67500000000003979, 87.70503267997129626, 89.02104166840096866 ) ) ;
#45646 = CARTESIAN_POINT ( 'NONE',  ( 11.99999999999999822, 0.000000000000000000, 0.000000000000000000 ) ) ;
#45647 = CARTESIAN_POINT ( 'NONE',  ( -7.572224309238338336, -145.4393675041377492, 5.500000000000000000 ) ) ;
#45648 = ORIENTED_EDGE ( 'NONE', *, *, #35372, .T. ) ;
#45649 = ORIENTED_EDGE ( 'NONE', *, *, #29269, .T. ) ;
#45650 = CARTESIAN_POINT ( 'NONE',  ( -97.65000000000001990, 90.00000000000004263, 77.93499999999998806 ) ) ;
#45651 = DIRECTION ( 'NONE',  ( 0.000000000000000000, -0.6494480483301903195, 0.7604059656000251577 ) ) ;
#45652 = DIRECTION ( 'NONE',  ( 0.000000000000000000, 0.000000000000000000, 1.000000000000000000 ) ) ;
#45653 = FACE_OUTER_BOUND ( 'NONE', #61848, .T. ) ;
#45654 = CARTESIAN_POINT ( 'NONE',  ( -96.32499999999996021, -207.7050326799711968, 89.89416666666666345 ) ) ;
#45655 = CARTESIAN_POINT ( 'NONE',  ( 10.00000000000000000, 0.000000000000000000, 0.000000000000000000 ) ) ;
#45656 = DIRECTION ( 'NONE',  ( -1.000000000000000000, 0.000000000000000000, -0.000000000000000000 ) ) ;
#45657 = EDGE_LOOP ( 'NONE', ( #50934, #28542, #3993, #37274 ) ) ;
#45658 = CARTESIAN_POINT ( 'NONE',  ( -92.69370383062504004, 90.00000000000004263, 79.16531250086714522 ) ) ;
#45660 = PLANE ( 'NONE',  #21103 ) ;
#45659 = AXIS2_PLACEMENT_3D ( 'NONE', #56927, #45656, #61451 ) ;
#45661 = CARTESIAN_POINT ( 'NONE',  ( 4.999999999999999112, -40.98264845739743123, -9.188173127307734944 ) ) ;
#45662 = PLANE ( 'NONE',  #46597 ) ;
#45663 = DIRECTION ( 'NONE',  ( 0.000000000000000000, 0.6494480483301793283, 0.7604059656000345946 ) ) ;
#45664 = AXIS2_PLACEMENT_3D ( 'NONE', #32268, #8981, #31906 ) ;
#45665 = CYLINDRICAL_SURFACE ( 'NONE', #13703, 42.00000000000000000 ) ;
#45666 = DIRECTION ( 'NONE',  ( -5.778480238264233142E-17, 1.000000000000000000, -0.000000000000000000 ) ) ;
#45667 = SURFACE_STYLE_USAGE ( .BOTH. , #61835 ) ;
#45668 = CARTESIAN_POINT ( 'NONE',  ( 93.84685191531248449, 88.00268892867053694, 76.57239583420049200 ) ) ;
#45669 = EDGE_CURVE ( 'NONE', #65482, #32129, #23927, .T. ) ;
#45670 = CARTESIAN_POINT ( 'NONE',  ( -93.84685191531248449, -208.0026889286704943, 80.69989583420047552 ) ) ;
#45671 = DIRECTION ( 'NONE',  ( -2.889240119132116694E-16, 1.000000000000000000, 0.000000000000000000 ) ) ;
#45672 = AXIS2_PLACEMENT_3D ( 'NONE', #57932, #51542, #41015 ) ;
#45673 = EDGE_LOOP ( 'NONE', ( #42627, #29246, #19119, #884 ) ) ;
#45674 = CYLINDRICAL_SURFACE ( 'NONE', #23320, 37.49900000000000233 ) ;
#45675 = CARTESIAN_POINT ( 'NONE',  ( 0.000000000000000000, 68.55367621811141987, 44.99326035066079044 ) ) ;
#45676 = DIRECTION ( 'NONE',  ( -0.000000000000000000, -0.000000000000000000, -1.000000000000000000 ) ) ;
#45677 = CIRCLE ( 'NONE', #27620, 37.49900000000000233 ) ;
#45678 = EDGE_CURVE ( 'NONE', #44013, #33546, #50311, .T. ) ;
#45679 = CIRCLE ( 'NONE', #9595, 15.80000000000028315 ) ;
#45680 = EDGE_CURVE ( 'NONE', #8327, #20786, #63538, .T. ) ;
#45681 = AXIS2_PLACEMENT_3D ( 'NONE', #19937, #54176, #1233 ) ;
#45682 = DIRECTION ( 'NONE',  ( 0.000000000000000000, 0.000000000000000000, 1.000000000000000000 ) ) ;
#45683 = CARTESIAN_POINT ( 'NONE',  ( 92.69370383062501162, -209.9999999999999716, 79.48281250086714067 ) ) ;
#45684 = ORIENTED_EDGE ( 'NONE', *, *, #58545, .F. ) ;
#45685 = DIRECTION ( 'NONE',  ( -1.000000000000000000, 0.000000000000000000, 0.000000000000000000 ) ) ;
#45686 = VERTEX_POINT ( 'NONE', #21048 ) ;
#45687 = EDGE_CURVE ( 'NONE', #4546, #1094, #38730, .T. ) ;
#45688 = LINE ( 'NONE', #57697, #33923 ) ;
#45689 = ORIENTED_EDGE ( 'NONE', *, *, #71088, .F. ) ;
#45690 = LINE ( 'NONE', #49809, #28581 ) ;
#45691 = VERTEX_POINT ( 'NONE', #54531 ) ;
#45692 = ORIENTED_EDGE ( 'NONE', *, *, #69033, .T. ) ;
#45693 = ORIENTED_EDGE ( 'NONE', *, *, #21513, .T. ) ;
#45694 = CARTESIAN_POINT ( 'NONE',  ( 95.00000000000000000, -207.3369185715606307, 76.30781250086715772 ) ) ;
#45695 = ORIENTED_EDGE ( 'NONE', *, *, #41310, .F. ) ;
#45696 = CARTESIAN_POINT ( 'NONE',  ( 11.99999999999999822, 74.18225833017889670, 34.94270380257665209 ) ) ;
#45697 = ORIENTED_EDGE ( 'NONE', *, *, #66288, .T. ) ;
#45698 = CARTESIAN_POINT ( 'NONE',  ( 97.30629616937498838, 88.66845928578037217, 81.81114583420048803 ) ) ;
#45699 = EDGE_CURVE ( 'NONE', #6579, #56950, #37982, .T. ) ;
#45700 = CARTESIAN_POINT ( 'NONE',  ( 96.32499999999998863, -212.2949673200287179, 77.51166666666665606 ) ) ;
#45701 = ORIENTED_EDGE ( 'NONE', *, *, #34797, .F. ) ;
#45702 = ORIENTED_EDGE ( 'NONE', *, *, #51676, .F. ) ;
#45703 = AXIS2_PLACEMENT_3D ( 'NONE', #45844, #69136, #45093 ) ;
#45704 = ORIENTED_EDGE ( 'NONE', *, *, #68681, .F. ) ;
#45705 = VERTEX_POINT ( 'NONE', #31958 ) ;
#45706 = CARTESIAN_POINT ( 'NONE',  ( -14.87942725330654348, -141.9795960975983178, 5.500000000000000000 ) ) ;
#45707 = AXIS2_PLACEMENT_3D ( 'NONE', #10029, #55899, #37874 ) ;
#45708 = EDGE_CURVE ( 'NONE', #25161, #48419, #3422, .T. ) ;
#45709 = EDGE_CURVE ( 'NONE', #7579, #4754, #37622, .T. ) ;
#45710 =( LENGTH_UNIT ( ) NAMED_UNIT ( * ) SI_UNIT ( .MILLI., .METRE. ) );
#45711 = DIRECTION ( 'NONE',  ( -1.000000000000000000, 0.000000000000000000, 0.000000000000000000 ) ) ;
#45712 = FACE_OUTER_BOUND ( 'NONE', #3881, .T. ) ;
#45713 = DIRECTION ( 'NONE',  ( -1.000000000000000000, -0.000000000000000000, -0.000000000000000000 ) ) ;
#45714 = AXIS2_PLACEMENT_3D ( 'NONE', #27760, #28873, #29245 ) ;
#45715 = FACE_OUTER_BOUND ( 'NONE', #9871, .T. ) ;
#45716 = LINE ( 'NONE', #68639, #26382 ) ;
#45717 = CARTESIAN_POINT ( 'NONE',  ( 10.00000000000000000, 0.000000000000000000, 0.000000000000000000 ) ) ;
#45718 = ORIENTED_EDGE ( 'NONE', *, *, #8212, .T. ) ;
#45719 = CARTESIAN_POINT ( 'NONE',  ( -93.67499999999998295, -212.2949673200287179, 83.94104166840097037 ) ) ;
#45720 = ORIENTED_EDGE ( 'NONE', *, *, #43376, .F. ) ;
#45721 = CARTESIAN_POINT ( 'NONE',  ( 10.00000000000000000, -58.39081064771787766, 50.95692526931307498 ) ) ;
#45722 = EDGE_CURVE ( 'NONE', #53141, #45993, #64708, .T. ) ;
#45723 = ORIENTED_EDGE ( 'NONE', *, *, #32566, .F. ) ;
#45725 = CARTESIAN_POINT ( 'NONE',  ( -97.65000000000001990, 91.52997821335253548, 78.59645833506763779 ) ) ;
#45724 = CARTESIAN_POINT ( 'NONE',  ( 93.67499999999999716, 87.70503267997126784, 80.66020833506763665 ) ) ;
#45726 = VERTEX_POINT ( 'NONE', #71805 ) ;
#45727 = CARTESIAN_POINT ( 'NONE',  ( 92.69370383062498320, 88.66845928578037217, 81.59947916753381492 ) ) ;
#45728 = DIRECTION ( 'NONE',  ( -0.000000000000000000, -0.2079116908177653378, 0.9781476007338044676 ) ) ;
#45729 = CARTESIAN_POINT ( 'NONE',  ( 10.00000000000000000, -29.01471420065507090, -76.69515212746047439 ) ) ;
#45730 = CARTESIAN_POINT ( 'NONE',  ( 0.000000000000000000, -27.75498641678764855, 31.52238457039590358 ) ) ;
#45731 = DIRECTION ( 'NONE',  ( 0.000000000000000000, 0.000000000000000000, 1.000000000000000000 ) ) ;
#45732 = CARTESIAN_POINT ( 'NONE',  ( 94.99999999999998579, 93.05995642670504253, 87.93624999999998693 ) ) ;
#45733 = ORIENTED_EDGE ( 'NONE', *, *, #44646, .T. ) ;
#45734 = CARTESIAN_POINT ( 'NONE',  ( 11.99999999999999822, -77.16300072079641836, -27.74655509720752633 ) ) ;
#45735 = CARTESIAN_POINT ( 'NONE',  ( -92.35000677010287973, 88.47001787792684979, 82.72395806468928470 ) ) ;
#45736 = CIRCLE ( 'NONE', #55303, 31.99999999999999289 ) ;
#45737 = CARTESIAN_POINT ( 'NONE',  ( 92.34999999999999432, 90.00000000000002842, 90.00000000000000000 ) ) ;
#45738 = ORIENTED_EDGE ( 'NONE', *, *, #71639, .F. ) ;
#45739 = AXIS2_PLACEMENT_3D ( 'NONE', #13874, #65042, #7878 ) ;
#45740 = EDGE_LOOP ( 'NONE', ( #57702, #872, #29582, #43579 ) ) ;
#45741 = AXIS2_PLACEMENT_3D ( 'NONE', #7292, #29093, #30206 ) ;
#45742 = LINE ( 'NONE', #74285, #72041 ) ;
#45743 = CARTESIAN_POINT ( 'NONE',  ( 0.000000000000000000, 0.000000000000000000, 0.000000000000000000 ) ) ;
#45744 = DIRECTION ( 'NONE',  ( -1.000000000000000000, 0.000000000000000000, 0.000000000000000000 ) ) ;
#45745 =( BOUNDED_CURVE ( )  B_SPLINE_CURVE ( 2, ( #47192, #999, #35167, #17506, #23519, #11491, #40820 ),
 .UNSPECIFIED., .F., .F. ) 
 B_SPLINE_CURVE_WITH_KNOTS ( ( 3, 2, 2, 3 ),
 ( 0.8333333333333334814, 0.8402777777777779011, 0.8472222222222222099, 0.8541666666666666297 ),
 .UNSPECIFIED. ) 
 CURVE ( )  GEOMETRIC_REPRESENTATION_ITEM ( )  RATIONAL_B_SPLINE_CURVE ( ( 0.9999999999999978906, 0.8660254037844408170, 1.000000000000000000, 0.8660254037844387076, 1.000000000000000000, 0.8660254037844387076, 1.000000000000000000 ) ) 
 REPRESENTATION_ITEM ( '' )  );
#45746 = CARTESIAN_POINT ( 'NONE',  ( -92.69370383062498320, -209.9999999999999716, 80.59406250086715318 ) ) ;
#45747 = VERTEX_POINT ( 'NONE', #15409 ) ;
#45748 = EDGE_LOOP ( 'NONE', ( #64701, #69743, #9459, #51221 ) ) ;
#45749 = DIRECTION ( 'NONE',  ( 0.000000000000000000, 0.000000000000000000, 1.000000000000000000 ) ) ;
#45750 = FACE_OUTER_BOUND ( 'NONE', #34421, .T. ) ;
#45751 = SURFACE_SIDE_STYLE ('',( #74298 ) ) ;
#45752 = DIRECTION ( 'NONE',  ( 0.4279312458753000703, 0.9038112904824842087, 0.000000000000000000 ) ) ;
#45753 = LINE ( 'NONE', #62679, #62898 ) ;
#45754 = DIRECTION ( 'NONE',  ( -1.000000000000000000, -0.000000000000000000, -0.000000000000000000 ) ) ;
#45755 = CARTESIAN_POINT ( 'NONE',  ( -96.32499999999996021, -207.7050326799711968, 79.09916666666666174 ) ) ;
#45756 = CARTESIAN_POINT ( 'NONE',  ( 10.00000000000000000, -66.50666863322028632, 39.78640506895582973 ) ) ;
#45757 = DIRECTION ( 'NONE',  ( -1.000000000000000000, 5.236901059551556403E-15, 2.618450529775778123E-14 ) ) ;
#45758 = CYLINDRICAL_SURFACE ( 'NONE', #50174, 77.49899999999999523 ) ;
#45759 = CARTESIAN_POINT ( 'NONE',  ( 94.99999999999998579, 87.33691857156068750, 87.42031250086715488 ) ) ;
#45760 = CARTESIAN_POINT ( 'NONE',  ( -96.15314808468745866, -211.9973110713294489, 88.63739583420048973 ) ) ;
#45761 = DIRECTION ( 'NONE',  ( -1.000000000000000000, -0.000000000000000000, -0.000000000000000000 ) ) ;
#45762 = VERTEX_POINT ( 'NONE', #49988 ) ;
#45763 = CIRCLE ( 'NONE', #55338, 31.99999999999999289 ) ;
#45764 = CARTESIAN_POINT ( 'NONE',  ( -3.000000000000000000, -26.23277895567245821, -4.042438405570103477 ) ) ;
#45765 = CIRCLE ( 'NONE', #52977, 26.50000000000000355 ) ;
#45766 = CARTESIAN_POINT ( 'NONE',  ( -97.30629616937501680, 90.00000000000004263, 78.21281250086714465 ) ) ;
#45767 = AXIS2_PLACEMENT_3D ( 'NONE', #30630, #46461, #69386 ) ;
#45768 = EDGE_CURVE ( 'NONE', #8213, #21151, #11888, .T. ) ;
#45769 = EDGE_CURVE ( 'NONE', #19317, #21360, #35935, .T. ) ;
#45770 = CARTESIAN_POINT ( 'NONE',  ( 93.84685191531251292, -211.9973110713294489, 89.11364583420048291 ) ) ;
#45771 = ORIENTED_EDGE ( 'NONE', *, *, #12634, .F. ) ;
#45772 = EDGE_CURVE ( 'NONE', #29385, #54357, #10145, .T. ) ;
#45773 = DIRECTION ( 'NONE',  ( 0.000000000000000000, 0.07845909572784530439, -0.9969173337331279638 ) ) ;
#45774 = CARTESIAN_POINT ( 'NONE',  ( 94.99999999999998579, 86.94004357329502852, 83.17374999999999829 ) ) ;
#45775 = CARTESIAN_POINT ( 'NONE',  ( 5.000000000000000000, 26.79245525562762253, -32.34446384429941901 ) ) ;
#45776 = CIRCLE ( 'NONE', #25369, 82.00000000000000000 ) ;
#45777 = VECTOR ( 'NONE', #19347, 1000.000000000000000 ) ;
#45778 = CARTESIAN_POINT ( 'NONE',  ( 0.000000000000000000, -8.840884882374576037, -74.65374052328658649 ) ) ;
#45779 = CARTESIAN_POINT ( 'NONE',  ( 18.80329974962065265, -105.8248132807389084, -5.500000000000000000 ) ) ;
#45780 = ORIENTED_EDGE ( 'NONE', *, *, #59590, .F. ) ;
#45781 = VECTOR ( 'NONE', #12347, 1000.000000000000000 ) ;
#45782 = VERTEX_POINT ( 'NONE', #4531 ) ;
#45783 = EDGE_CURVE ( 'NONE', #53203, #22270, #21485, .T. ) ;
#45784 = CARTESIAN_POINT ( 'NONE',  ( 93.84685191531251292, -211.9973110713294489, 86.09739583420049769 ) ) ;
#45785 = EDGE_CURVE ( 'NONE', #37995, #63103, #17910, .T. ) ;
#45786 = DIRECTION ( 'NONE',  ( 0.000000000000000000, 0.000000000000000000, 1.000000000000000000 ) ) ;
#45787 = DIRECTION ( 'NONE',  ( -0.9730327541852497042, 0.2306669878475623159, 0.000000000000000000 ) ) ;
#45788 = CARTESIAN_POINT ( 'NONE',  ( -96.32499999999996021, -207.7050326799711968, 77.27354166840096639 ) ) ;
#45789 = CARTESIAN_POINT ( 'NONE',  ( -6.509281303079589520, -14.89695620656361008, -1.199999999999999956 ) ) ;
#45790 = DIRECTION ( 'NONE',  ( 0.000000000000000000, -0.3826834323650772363, -0.9238795325112919565 ) ) ;
#45791 = CARTESIAN_POINT ( 'NONE',  ( 96.32499999999998863, -207.7050326799711968, 89.15333333333333599 ) ) ;
#45792 = ORIENTED_EDGE ( 'NONE', *, *, #45023, .T. ) ;
#45793 = VERTEX_POINT ( 'NONE', #7808 ) ;
#45794 = VERTEX_POINT ( 'NONE', #24729 ) ;
#45795 = ORIENTED_EDGE ( 'NONE', *, *, #61563, .F. ) ;
#45796 = DIRECTION ( 'NONE',  ( -1.000000000000000000, -0.000000000000000000, 0.000000000000000000 ) ) ;
#45797 = EDGE_CURVE ( 'NONE', #50744, #35896, #54411, .T. ) ;
#45798 = EDGE_CURVE ( 'NONE', #70524, #26348, #43152, .T. ) ;
#45799 = DIRECTION ( 'NONE',  ( 0.000000000000000000, 0.000000000000000000, 1.000000000000000000 ) ) ;
#45800 = DIRECTION ( 'NONE',  ( 0.000000000000000000, 0.000000000000000000, 1.000000000000000000 ) ) ;
#45801 = CARTESIAN_POINT ( 'NONE',  ( 96.32499999999998863, -207.7050326799711968, 76.53270833506762472 ) ) ;
#45802 = CARTESIAN_POINT ( 'NONE',  ( 96.32499999999998863, 87.70503267997126784, 83.22666666666665947 ) ) ;
#45803 = ORIENTED_EDGE ( 'NONE', *, *, #63763, .F. ) ;
#45804 = DIRECTION ( 'NONE',  ( -1.000000000000000000, 0.000000000000000000, 0.000000000000000000 ) ) ;
#45805 = ORIENTED_EDGE ( 'NONE', *, *, #59533, .F. ) ;
#45806 = CARTESIAN_POINT ( 'NONE',  ( 0.000000000000000000, 0.000000000000000000, 0.000000000000000000 ) ) ;
#45807 = ORIENTED_EDGE ( 'NONE', *, *, #46764, .T. ) ;
#45808 = CARTESIAN_POINT ( 'NONE',  ( 97.64999999999999147, 89.99999988321010846, 84.68187499741277691 ) ) ;
#45809 = CARTESIAN_POINT ( 'NONE',  ( -97.30629616937501680, 90.00000000000004263, 80.27656250086714351 ) ) ;
#45810 = CARTESIAN_POINT ( 'NONE',  ( 94.99999999999998579, 87.33691857156068750, 79.64156250086713840 ) ) ;
#45811 = ORIENTED_EDGE ( 'NONE', *, *, #59970, .T. ) ;
#45812 = DIRECTION ( 'NONE',  ( 0.000000000000000000, 0.000000000000000000, 1.000000000000000000 ) ) ;
#45813 = DIRECTION ( 'NONE',  ( 0.000000000000000000, -0.9969173337331271867, -0.07845909572785571273 ) ) ;
#45814 = CARTESIAN_POINT ( 'NONE',  ( 94.99999999999998579, 86.94004357329502852, 88.96812500173430749 ) ) ;
#45815 = MECHANICAL_DESIGN_GEOMETRIC_PRESENTATION_REPRESENTATION (  '', ( #24175 ), #54227 ) ;
#45816 = AXIS2_PLACEMENT_3D ( 'NONE', #70009, #51984, #904 ) ;
#45817 = DIRECTION ( 'NONE',  ( 0.000000000000000000, -0.8090169943749497827, -0.5877852522924698064 ) ) ;
#45818 = ORIENTED_EDGE ( 'NONE', *, *, #23202, .F. ) ;
#45819 = CARTESIAN_POINT ( 'NONE',  ( -4.999999999999999112, -2.417244626924490269, -5.688952927922134251 ) ) ;
#45820 = VECTOR ( 'NONE', #72880, 1000.000000000000227 ) ;
#45821 = CARTESIAN_POINT ( 'NONE',  ( -92.69370383062498320, -211.3315407142195852, 79.11239583420046984 ) ) ;
#45822 = ORIENTED_EDGE ( 'NONE', *, *, #45538, .T. ) ;
#45823 = AXIS2_PLACEMENT_3D ( 'NONE', #73069, #44529, #62573 ) ;
#45824 = ORIENTED_EDGE ( 'NONE', *, *, #54155, .T. ) ;
#45825 = FACE_BOUND ( 'NONE', #59682, .T. ) ;
#45826 = AXIS2_PLACEMENT_3D ( 'NONE', #27283, #27669, #50595 ) ;
#45827 = ORIENTED_EDGE ( 'NONE', *, *, #21620, .F. ) ;
#45828 = DIRECTION ( 'NONE',  ( 0.2306669878475623159, 0.9730327541852497042, -0.000000000000000000 ) ) ;
#45829 = EDGE_LOOP ( 'NONE', ( #32076, #25804, #64961, #47836 ) ) ;
#45830 = CARTESIAN_POINT ( 'NONE',  ( -94.99999999999997158, -212.6630814284392557, 75.19656250086714522 ) ) ;
#45831 = VERTEX_POINT ( 'NONE', #70205 ) ;
#45832 = CARTESIAN_POINT ( 'NONE',  ( 97.64999999999999147, 90.00000000000002842, 88.49187500173430010 ) ) ;
#45833 = DIRECTION ( 'NONE',  ( 1.000000000000000000, 0.000000000000000000, 0.000000000000000000 ) ) ;
#45834 = DIRECTION ( 'NONE',  ( 0.000000000000000000, -1.000000000000000000, 1.181994176819165452E-15 ) ) ;
#45835 = CARTESIAN_POINT ( 'NONE',  ( 93.67500000000001137, -207.7050326799711968, 81.63916666666666799 ) ) ;
#45836 = DIRECTION ( 'NONE',  ( 0.000000000000000000, 0.000000000000000000, 1.000000000000000000 ) ) ;
#45837 = CONICAL_SURFACE ( 'NONE', #46996, 4.749999999999999112, 0.4572823821333981131 ) ;
#45838 = AXIS2_PLACEMENT_3D ( 'NONE', #53275, #48007, #47271 ) ;
#45839 = DIRECTION ( 'NONE',  ( -1.000000000000000000, 0.000000000000000000, 0.000000000000000000 ) ) ;
#45840 = CARTESIAN_POINT ( 'NONE',  ( 93.84685191531248449, 88.00268892867053694, 83.39864583420047950 ) ) ;
#45841 = LINE ( 'NONE', #5615, #19598 ) ;
#45842 = AXIS2_PLACEMENT_3D ( 'NONE', #33716, #56669, #17535 ) ;
#45843 = CARTESIAN_POINT ( 'NONE',  ( -97.65000000000009095, 88.47002178664760663, 75.44791666666667140 ) ) ;
#45844 = CARTESIAN_POINT ( 'NONE',  ( 2.500000000000029754, 73.00000000000001421, -204.9999999999999716 ) ) ;
#45845 = DIRECTION ( 'NONE',  ( -1.000000000000000000, 0.000000000000000000, -0.000000000000000000 ) ) ;
#45846 = CARTESIAN_POINT ( 'NONE',  ( 1.250000000000000000, -12.36245420541525597, -1.199999999999999956 ) ) ;
#45847 = CARTESIAN_POINT ( 'NONE',  ( 92.35000000000000853, -209.9999999999999716, 87.53937500173429953 ) ) ;
#45848 = CARTESIAN_POINT ( 'NONE',  ( 0.000000000000000000, 0.000000000000000000, 0.000000000000000000 ) ) ;
#45849 = ADVANCED_FACE ( 'NONE', ( #1841 ), #8556, .T. ) ;
#45850 = CARTESIAN_POINT ( 'NONE',  ( 11.99999999999999822, 72.35160999960817207, 20.41045688087850607 ) ) ;
#45851 = EDGE_CURVE ( 'NONE', #22210, #20975, #52745, .T. ) ;
#45852 = DIRECTION ( 'NONE',  ( 0.000000000000000000, -0.5877852522924779111, -0.8090169943749440096 ) ) ;
#45853 = CARTESIAN_POINT ( 'NONE',  ( -93.84685191531254134, 91.99731107132950569, 89.43114583420047836 ) ) ;
#45854 = CARTESIAN_POINT ( 'NONE',  ( 10.00000000000000000, 0.000000000000000000, 0.000000000000000000 ) ) ;
#45855 = EDGE_CURVE ( 'NONE', #15896, #10469, #57521, .T. ) ;
#45856 = EDGE_CURVE ( 'NONE', #69332, #51295, #48134, .T. ) ;
#45857 = CARTESIAN_POINT ( 'NONE',  ( -92.35000000000003695, 90.00000000000004263, 75.07749999999998636 ) ) ;
#45858 = PRODUCT_DEFINITION_SHAPE ( 'NONE', 'NONE',  #74356 ) ;
#45859 = EDGE_LOOP ( 'NONE', ( #18405, #4172, #57074, #220 ) ) ;
#45860 = EDGE_CURVE ( 'NONE', #19435, #13671, #60436, .T. ) ;
#45861 = CYLINDRICAL_SURFACE ( 'NONE', #62374, 42.00000000000000000 ) ;
#45862 = CARTESIAN_POINT ( 'NONE',  ( 15.00000000000000000, -4.261787119644963262, 26.19803753235780164 ) ) ;
#45863 = LINE ( 'NONE', #68787, #67008 ) ;
#45864 = DIRECTION ( 'NONE',  ( -0.000000000000000000, -1.000000000000000000, -0.000000000000000000 ) ) ;
#45865 =( GEOMETRIC_REPRESENTATION_CONTEXT ( 3 ) GLOBAL_UNCERTAINTY_ASSIGNED_CONTEXT ( ( #44461 ) ) GLOBAL_UNIT_ASSIGNED_CONTEXT ( ( #46761, #12163, #8753 ) ) REPRESENTATION_CONTEXT ( 'NONE', 'WORKASPACE' ) );
#45866 = AXIS2_PLACEMENT_3D ( 'NONE', #28503, #4, #1104 ) ;
#45867 = FACE_OUTER_BOUND ( 'NONE', #3537, .T. ) ;
#45868 = CARTESIAN_POINT ( 'NONE',  ( 93.84685191531249870, -208.0026889286704943, 84.61572916753381435 ) ) ;
#45869 = CIRCLE ( 'NONE', #6261, 12.49999999999999822 ) ;
#45870 = ORIENTED_EDGE ( 'NONE', *, *, #53153, .F. ) ;
#45871 = ORIENTED_EDGE ( 'NONE', *, *, #47435, .F. ) ;
#45872 = EDGE_CURVE ( 'NONE', #63343, #9632, #54085, .T. ) ;
#45873 = CIRCLE ( 'NONE', #66306, 20.20000000000036522 ) ;
#45874 = ADVANCED_FACE ( 'NONE', ( #71686 ), #68333, .F. ) ;
#45875 = DIRECTION ( 'NONE',  ( 0.7533909544171998318, 0.6575728627325954090, 0.000000000000000000 ) ) ;
#45876 = VERTEX_POINT ( 'NONE', #54378 ) ;
#45877 = DIRECTION ( 'NONE',  ( 1.000000000000000000, 0.000000000000000000, 0.000000000000000000 ) ) ;
#45878 = AXIS2_PLACEMENT_3D ( 'NONE', #69727, #59194, #40800 ) ;
#45879 = CARTESIAN_POINT ( 'NONE',  ( 93.84685191531249870, -208.0026889286704943, 77.47197916753380298 ) ) ;
#45880 = VERTEX_POINT ( 'NONE', #36338 ) ;
#45881 = CARTESIAN_POINT ( 'NONE',  ( 92.69370383062501162, -208.6684592857803011, 84.03364583420049883 ) ) ;
#45882 = ORIENTED_EDGE ( 'NONE', *, *, #28076, .F. ) ;
#45883 = VERTEX_POINT ( 'NONE', #8525 ) ;
#45884 = VECTOR ( 'NONE', #48210, 1000.000000000000000 ) ;
#45885 = ORIENTED_EDGE ( 'NONE', *, *, #6202, .T. ) ;
#45886 = UNCERTAINTY_MEASURE_WITH_UNIT (LENGTH_MEASURE( 1.000000000000000082E-05 ), #24003, 'distance_accuracy_value', 'NONE');
#45887 = CIRCLE ( 'NONE', #26641, 82.00000000000000000 ) ;
#45888 = EDGE_LOOP ( 'NONE', ( #28117, #41160, #20703, #71461 ) ) ;
#45889 = CARTESIAN_POINT ( 'NONE',  ( 97.64999999989935020, -209.9999769027737671, 83.41187580057901130 ) ) ;
#45890 = CARTESIAN_POINT ( 'NONE',  ( 95.00000000000000000, -213.0599564267049857, 87.06312500173430635 ) ) ;
#45891 = ORIENTED_EDGE ( 'NONE', *, *, #16152, .F. ) ;
#45892 = DIRECTION ( 'NONE',  ( 0.000000000000000000, -0.9238795325112906243, 0.3826834323650804004 ) ) ;
#45893 = ORIENTED_EDGE ( 'NONE', *, *, #2167, .T. ) ;
#45894 = CARTESIAN_POINT ( 'NONE',  ( 4.999999999999999112, -2.691295138309024892, -1.881393335304215153 ) ) ;
#45895 = ORIENTED_EDGE ( 'NONE', *, *, #14493, .F. ) ;
#45896 = ORIENTED_EDGE ( 'NONE', *, *, #59502, .T. ) ;
#45897 = ORIENTED_EDGE ( 'NONE', *, *, #73186, .T. ) ;
#45898 = CARTESIAN_POINT ( 'NONE',  ( -3.000000000000000000, 16.83928648764923253, 16.46020748918050458 ) ) ;
#45899 = CARTESIAN_POINT ( 'NONE',  ( 10.00000000000000000, 75.11764819372142199, 2.946379043147685728 ) ) ;
#45900 = ORIENTED_EDGE ( 'NONE', *, *, #24012, .F. ) ;
#45901 = VERTEX_POINT ( 'NONE', #48004 ) ;
#45902 = EDGE_LOOP ( 'NONE', ( #14145, #50916, #1985, #73690 ) ) ;
#45903 = DIRECTION ( 'NONE',  ( -1.000000000000000000, -0.000000000000000000, 0.000000000000000000 ) ) ;
#45904 = CARTESIAN_POINT ( 'NONE',  ( 96.32499999999997442, 92.29496732002878900, 81.53333333333333144 ) ) ;
#45905 = CARTESIAN_POINT ( 'NONE',  ( -92.35000000000003695, 90.00000000000004263, 89.04749999999999943 ) ) ;
#45906 = EDGE_LOOP ( 'NONE', ( #65838, #36118, #72215, #37433 ) ) ;
#45907 = CARTESIAN_POINT ( 'NONE',  ( 15.00000000000000000, 22.07842321921492612, 8.187992925817123790 ) ) ;
#45908 = ORIENTED_EDGE ( 'NONE', *, *, #30473, .T. ) ;
#45909 = LINE ( 'NONE', #1190, #57556 ) ;
#45910 = CARTESIAN_POINT ( 'NONE',  ( -93.84685191531248449, -208.0026889286704943, 87.52614583420047722 ) ) ;
#45911 = VERTEX_POINT ( 'NONE', #25800 ) ;
#45912 = CARTESIAN_POINT ( 'NONE',  ( 11.99999999999999822, 2.956366410620650420, 75.11725578898469280 ) ) ;
#45913 = CARTESIAN_POINT ( 'NONE',  ( 94.87443773336561037, -212.6467947905572089, 74.99648857272262603 ) ) ;
#45914 = CARTESIAN_POINT ( 'NONE',  ( 92.35000000000007958, 88.47002178664749295, 81.16291666666667481 ) ) ;
#45915 = CARTESIAN_POINT ( 'NONE',  ( -97.30629616937497417, -211.3315407142195852, 77.63072916753380071 ) ) ;
#45916 = ADVANCED_FACE ( 'NONE', ( #47625 ), #48730, .F. ) ;
#45917 = AXIS2_PLACEMENT_3D ( 'NONE', #43432, #43048, #65236 ) ;
#45918 = CARTESIAN_POINT ( 'NONE',  ( 0.000000000000000000, 3.925862922256160736, 41.81611651403863306 ) ) ;
#45919 = CARTESIAN_POINT ( 'NONE',  ( 0.000000000000000000, 0.000000000000000000, 0.000000000000000000 ) ) ;
#45920 = LINE ( 'NONE', #57568, #64918 ) ;
#45921 = ADVANCED_FACE ( 'NONE', ( #66044 ), #25062, .F. ) ;
#45922 = LINE ( 'NONE', #4964, #43572 ) ;
#45923 = EDGE_CURVE ( 'NONE', #27633, #32262, #19079, .T. ) ;
#45924 = CARTESIAN_POINT ( 'NONE',  ( 3.250000000000000444, -13.95926121303099343, 0.000000000000000000 ) ) ;
#45925 = CIRCLE ( 'NONE', #71108, 31.99999999999999289 ) ;
#45926 = CARTESIAN_POINT ( 'NONE',  ( -97.30629616937501680, 91.33154071421968467, 79.42989583420046529 ) ) ;
#45927 = FACE_OUTER_BOUND ( 'NONE', #34298, .T. ) ;
#45928 = DIRECTION ( 'NONE',  ( -1.000000000000000000, 0.000000000000000000, 0.000000000000000000 ) ) ;
#45929 = AXIS2_PLACEMENT_3D ( 'NONE', #38591, #43511, #37488 ) ;
#45930 = ORIENTED_EDGE ( 'NONE', *, *, #11990, .F. ) ;
#45931 = CYLINDRICAL_SURFACE ( 'NONE', #46200, 23.50000000000000355 ) ;
#45932 = EDGE_CURVE ( 'NONE', #10439, #54468, #47903, .T. ) ;
#45933 = CIRCLE ( 'NONE', #13491, 31.99999999999998579 ) ;
#45934 = DIRECTION ( 'NONE',  ( -1.000000000000000000, 0.000000000000000000, 0.000000000000000000 ) ) ;
#45935 = FACE_OUTER_BOUND ( 'NONE', #47159, .T. ) ;
#45936 = VECTOR ( 'NONE', #13166, 1000.000000000000000 ) ;
#45937 = CARTESIAN_POINT ( 'NONE',  ( 0.000000000000000000, 0.000000000000000000, -270.0000000000000000 ) ) ;
#45938 = CARTESIAN_POINT ( 'NONE',  ( -97.65000000000001990, 91.52997821335253548, 89.94708333333332462 ) ) ;
#45939 = CARTESIAN_POINT ( 'NONE',  ( 0.000000000000000000, 0.000000000000000000, -125.0000000000000000 ) ) ;
#45940 = CARTESIAN_POINT ( 'NONE',  ( -93.84685191531247028, -211.9973110713294489, 81.12322916753382174 ) ) ;
#45941 = LINE ( 'NONE', #68866, #53690 ) ;
#45942 = ORIENTED_EDGE ( 'NONE', *, *, #63766, .T. ) ;
#45943 = EDGE_CURVE ( 'NONE', #73838, #15358, #64935, .T. ) ;
#45944 = CARTESIAN_POINT ( 'NONE',  ( -95.00000000000002842, 90.00000000000004263, 90.00000000000000000 ) ) ;
#45945 = LINE ( 'NONE', #5723, #61097 ) ;
#45946 = DIRECTION ( 'NONE',  ( -1.000000000000000000, 0.000000000000000000, -0.000000000000000000 ) ) ;
#45947 = CYLINDRICAL_SURFACE ( 'NONE', #594, 31.99999999999998579 ) ;
#45948 = DIRECTION ( 'NONE',  ( -1.000000000000000000, 0.000000000000000000, 0.000000000000000000 ) ) ;
#45949 = ORIENTED_EDGE ( 'NONE', *, *, #50214, .T. ) ;
#45950 = EDGE_CURVE ( 'NONE', #61799, #7483, #13409, .T. ) ;
#45951 = DIRECTION ( 'NONE',  ( 0.3853207896976533209, -0.9227826878668545785, 0.000000000000000000 ) ) ;
#45952 = ADVANCED_FACE ( 'NONE', ( #19416 ), #44593, .F. ) ;
#45953 = CARTESIAN_POINT ( 'NONE',  ( -10.00000000000000000, 0.000000000000000000, 0.000000000000000000 ) ) ;
#45954 = ORIENTED_EDGE ( 'NONE', *, *, #41190, .F. ) ;
#45955 =( BOUNDED_CURVE ( )  B_SPLINE_CURVE ( 2, ( #269, #23161, #62272, #69021, #57739, #6245, #628 ),
 .UNSPECIFIED., .F., .F. ) 
 B_SPLINE_CURVE_WITH_KNOTS ( ( 3, 2, 2, 3 ),
 ( 0.6250000000000003331, 0.6319444444444446418, 0.6388888888888890616, 0.6458333333333334814 ),
 .UNSPECIFIED. ) 
 CURVE ( )  GEOMETRIC_REPRESENTATION_ITEM ( )  RATIONAL_B_SPLINE_CURVE ( ( 0.9999999999999935607, 0.8660254037844451469, 1.000000000000000000, 0.8660254037844387076, 1.000000000000000000, 0.8660254037844365982, 1.000000000000002220 ) ) 
 REPRESENTATION_ITEM ( '' )  );
#45956 = CARTESIAN_POINT ( 'NONE',  ( 97.30629616937498838, -208.6684592857803295, 87.47322916753380184 ) ) ;
#45957 = CARTESIAN_POINT ( 'NONE',  ( 0.000000000000000000, 0.000000000000000000, -43.79999999999998295 ) ) ;
#45958 = ADVANCED_FACE ( 'NONE', ( #49835 ), #27656, .T. ) ;
#45959 = ORIENTED_EDGE ( 'NONE', *, *, #38446, .F. ) ;
#45960 = DIRECTION ( 'NONE',  ( 0.000000000000000000, 0.000000000000000000, -1.000000000000000000 ) ) ;
#45961 = ORIENTED_EDGE ( 'NONE', *, *, #68058, .F. ) ;
#45962 = CARTESIAN_POINT ( 'NONE',  ( 0.000000000000000000, 0.000000000000000000, 20.00000000000000000 ) ) ;
#45963 = ORIENTED_EDGE ( 'NONE', *, *, #493, .T. ) ;
#45964 = FACE_OUTER_BOUND ( 'NONE', #16628, .T. ) ;
#45965 = VERTEX_POINT ( 'NONE', #26538 ) ;
#45966 = DIRECTION ( 'NONE',  ( 0.000000000000000000, 0.9723699203976773342, -0.2334453638559024213 ) ) ;
#45967 = ORIENTED_EDGE ( 'NONE', *, *, #55605, .T. ) ;
#45968 = ORIENTED_EDGE ( 'NONE', *, *, #31414, .T. ) ;
#45969 = CYLINDRICAL_SURFACE ( 'NONE', #42852, 12.75000000000000000 ) ;
#45970 = VERTEX_POINT ( 'NONE', #68259 ) ;
#45971 = VECTOR ( 'NONE', #5875, 1000.000000000000000 ) ;
#45972 = ORIENTED_EDGE ( 'NONE', *, *, #21305, .F. ) ;
#45973 = CARTESIAN_POINT ( 'NONE',  ( 11.99999999999999822, 0.000000000000000000, 0.000000000000000000 ) ) ;
#45974 = EDGE_LOOP ( 'NONE', ( #54010, #72574, #41147, #54859 ) ) ;
#45975 = EDGE_LOOP ( 'NONE', ( #27093, #63907, #47268, #54765 ) ) ;
#45976 = CARTESIAN_POINT ( 'NONE',  ( 96.15314808468748708, 88.00268892867053694, 86.04447916753380809 ) ) ;
#45977 = CIRCLE ( 'NONE', #37547, 82.00000000000000000 ) ;
#45978 = EDGE_LOOP ( 'NONE', ( #65309, #40084, #73603, #45223 ) ) ;
#45979 = CARTESIAN_POINT ( 'NONE',  ( 92.69370383062501162, -209.9999999999999716, 80.75281250086715090 ) ) ;
#45980 = VECTOR ( 'NONE', #48854, 1000.000000000000000 ) ;
#45981 = APPLICATION_PROTOCOL_DEFINITION ( 'draft international standard', 'automotive_design', 1998, #40285 ) ;
#45982 = CARTESIAN_POINT ( 'NONE',  ( 7.103376864691351012E-17, -120.0000000000000000, -64.00000000000000000 ) ) ;
#45983 = DIRECTION ( 'NONE',  ( -1.000000000000000000, 0.000000000000000000, 0.000000000000000000 ) ) ;
#45984 = DIRECTION ( 'NONE',  ( 0.000000000000000000, 0.000000000000000000, 1.000000000000000000 ) ) ;
#45985 = DIRECTION ( 'NONE',  ( 0.000000000000000000, 0.000000000000000000, 1.000000000000000000 ) ) ;
#45986 = DIRECTION ( 'NONE',  ( -1.000000000000000000, 0.000000000000000000, 0.000000000000000000 ) ) ;
#45987 = CARTESIAN_POINT ( 'NONE',  ( 92.35000000003287823, 90.00000839536618003, 84.99910573348789455 ) ) ;
#45988 = CARTESIAN_POINT ( 'NONE',  ( -94.99999999999997158, -212.6630814284392557, 85.99156250086714692 ) ) ;
#45989 = CARTESIAN_POINT ( 'NONE',  ( -93.84685191531254134, 91.99731107132950569, 83.87489583420048689 ) ) ;
#45990 = ORIENTED_EDGE ( 'NONE', *, *, #9485, .T. ) ;
#45992 = CARTESIAN_POINT ( 'NONE',  ( -97.30629616937501680, 91.33154071421968467, 84.50989583420046358 ) ) ;
#45991 = CARTESIAN_POINT ( 'NONE',  ( 94.99999999999998579, 92.66308142843935514, 85.03906250086714635 ) ) ;
#45993 = VERTEX_POINT ( 'NONE', #9987 ) ;
#45994 = CARTESIAN_POINT ( 'NONE',  ( -97.64999999999997726, 91.52997821335256390, 88.04208333333330927 ) ) ;
#45995 = CARTESIAN_POINT ( 'NONE',  ( -99.99999999999998579, -124.0000000000000142, 39.99999999999996447 ) ) ;
#45996 = DIRECTION ( 'NONE',  ( 0.9918136447140101231, -0.1276937514489694114, 0.000000000000000000 ) ) ;
#45997 = LINE ( 'NONE', #29784, #52449 ) ;
#45998 = CARTESIAN_POINT ( 'NONE',  ( -93.84685191531248449, -208.0026889286704943, 86.89114583420047211 ) ) ;
#45999 = DIRECTION ( 'NONE',  ( 0.000000000000000000, 0.8526401643540935105, -0.5224985647159466895 ) ) ;
#46000 = EDGE_CURVE ( 'NONE', #27087, #70823, #50959, .T. ) ;
#46001 = CARTESIAN_POINT ( 'NONE',  ( 11.99999999999999822, -17.28742895386137945, 75.54627589209938776 ) ) ;
#46002 = CARTESIAN_POINT ( 'NONE',  ( 0.000000000000000000, 80.28980883073758434, 16.65972982744963460 ) ) ;
#46003 = DIRECTION ( 'NONE',  ( -1.000000000000000000, -0.000000000000000000, 0.000000000000000000 ) ) ;
#46004 = ORIENTED_EDGE ( 'NONE', *, *, #32683, .T. ) ;
#46005 = ORIENTED_EDGE ( 'NONE', *, *, #73396, .F. ) ;
#46006 = ADVANCED_FACE ( 'NONE', ( #15999, #61506 ), #72395, .F. ) ;
#46007 = CARTESIAN_POINT ( 'NONE',  ( -97.65000000000001990, 91.52997821335253548, 76.61208333333333087 ) ) ;
#46008 = EDGE_CURVE ( 'NONE', #62552, #53187, #45621, .T. ) ;
#46009 = FACE_OUTER_BOUND ( 'NONE', #19808, .T. ) ;
#46010 = DIRECTION ( 'NONE',  ( -1.000000000000000000, 0.000000000000000000, 0.000000000000000000 ) ) ;
#46011 = CARTESIAN_POINT ( 'NONE',  ( 96.32499999999997442, 92.29496732002878900, 76.45333333333333314 ) ) ;
#46012 = CARTESIAN_POINT ( 'NONE',  ( -10.00000000000000000, 0.000000000000000000, 0.000000000000000000 ) ) ;
#46013 = CARTESIAN_POINT ( 'NONE',  ( 97.64999999999996305, -209.9999996502043018, 77.69687501385438111 ) ) ;
#46014 = CARTESIAN_POINT ( 'NONE',  ( 0.000000000000000000, 0.000000000000000000, 0.000000000000000000 ) ) ;
#46015 = VERTEX_POINT ( 'NONE', #55859 ) ;
#46016 = CARTESIAN_POINT ( 'NONE',  ( -95.00000000000002842, 87.33691857156074434, 77.10156250086711793 ) ) ;
#46017 = EDGE_CURVE ( 'NONE', #57811, #14148, #13176, .T. ) ;
#46018 =( GEOMETRIC_REPRESENTATION_CONTEXT ( 3 ) GLOBAL_UNCERTAINTY_ASSIGNED_CONTEXT ( ( #71605 ) ) GLOBAL_UNIT_ASSIGNED_CONTEXT ( ( #57337, #602, #40410 ) ) REPRESENTATION_CONTEXT ( 'NONE', 'WORKASPACE' ) );
#46019 = DIRECTION ( 'NONE',  ( -1.000000000000000000, 0.000000000000000000, 0.000000000000000000 ) ) ;
#46020 = FACE_OUTER_BOUND ( 'NONE', #45389, .T. ) ;
#46021 = AXIS2_PLACEMENT_3D ( 'NONE', #37168, #2245, #14965 ) ;
#46022 = CARTESIAN_POINT ( 'NONE',  ( 0.000000000000000000, 9.188173127307898369, -40.98264845739739570 ) ) ;
#46023 = DIRECTION ( 'NONE',  ( -1.000000000000000000, 0.000000000000000000, 0.000000000000000000 ) ) ;
#46024 = PLANE ( 'NONE',  #20891 ) ;
#46025 = LINE ( 'NONE', #44542, #14242 ) ;
#46026 = CIRCLE ( 'NONE', #20779, 31.99999999999998224 ) ;
#46027 = AXIS2_PLACEMENT_3D ( 'NONE', #32768, #61737, #10971 ) ;
#46028 = EDGE_CURVE ( 'NONE', #50672, #67440, #62634, .T. ) ;
#46029 = CARTESIAN_POINT ( 'NONE',  ( 93.84685191531248449, 91.99731107132950569, 76.99572916753382401 ) ) ;
#46030 = CARTESIAN_POINT ( 'NONE',  ( -96.15314808468747287, -208.0026889286704943, 78.26572916753382003 ) ) ;
#46031 = DIRECTION ( 'NONE',  ( -0.8225049752423791993, -0.5687579148473745905, 0.000000000000000000 ) ) ;
#46032 = ORIENTED_EDGE ( 'NONE', *, *, #28240, .F. ) ;
#46033 = CIRCLE ( 'NONE', #20630, 82.00000000000000000 ) ;
#46034 = DIRECTION ( 'NONE',  ( -1.000000000000000000, 0.000000000000000000, 0.000000000000000000 ) ) ;
#46035 = CARTESIAN_POINT ( 'NONE',  ( 11.99999999999999822, -75.11725578898470701, 2.956366410620372864 ) ) ;
#46036 = DIRECTION ( 'NONE',  ( 0.000000000000000000, 0.000000000000000000, 1.000000000000000000 ) ) ;
#46037 = AXIS2_PLACEMENT_3D ( 'NONE', #51451, #22905, #22149 ) ;
#46038 = CARTESIAN_POINT ( 'NONE',  ( -97.30629616937501680, 90.00000000000004263, 76.46656250086715545 ) ) ;
#46039 = CARTESIAN_POINT ( 'NONE',  ( 96.15314808468748708, -208.0026889286704943, 80.54114583420046358 ) ) ;
#46040 = ORIENTED_EDGE ( 'NONE', *, *, #58765, .F. ) ;
#46041 = ADVANCED_FACE ( 'NONE', ( #21640 ), #33280, .F. ) ;
#46042 = EDGE_CURVE ( 'NONE', #37315, #33112, #7178, .T. ) ;
#46043 = DIRECTION ( 'NONE',  ( 0.9038112904824853189, -0.4279312458752977388, 0.000000000000000000 ) ) ;
#46044 = ORIENTED_EDGE ( 'NONE', *, *, #68326, .T. ) ;
#46045 = CYLINDRICAL_SURFACE ( 'NONE', #21962, 2.649999999999985700 ) ;
#46046 = ORIENTED_EDGE ( 'NONE', *, *, #58058, .F. ) ;
#46047 = CARTESIAN_POINT ( 'NONE',  ( 10.00000000000000000, -44.99326035066006568, -68.55367621811190304 ) ) ;
#46048 = ORIENTED_EDGE ( 'NONE', *, *, #34875, .F. ) ;
#46049 = EDGE_LOOP ( 'NONE', ( #4113, #66659, #18420, #72413 ) ) ;
#46050 = ORIENTED_EDGE ( 'NONE', *, *, #38873, .T. ) ;
#46051 = ORIENTED_EDGE ( 'NONE', *, *, #72209, .T. ) ;
#46052 = CIRCLE ( 'NONE', #19569, 82.00000000000000000 ) ;
#46053 = VERTEX_POINT ( 'NONE', #4371 ) ;
#46054 = CARTESIAN_POINT ( 'NONE',  ( 93.84685191531248449, 88.00268892867053694, 83.55739583420049144 ) ) ;
#46055 = CARTESIAN_POINT ( 'NONE',  ( 10.00000000000000000, 27.75498641678742473, 31.52238457039609898 ) ) ;
#46056 = ORIENTED_EDGE ( 'NONE', *, *, #11275, .T. ) ;
#46057 = LINE ( 'NONE', #12672, #38052 ) ;
#46058 = ORIENTED_EDGE ( 'NONE', *, *, #63771, .T. ) ;
#46059 = ORIENTED_EDGE ( 'NONE', *, *, #35051, .T. ) ;
#46060 = VERTEX_POINT ( 'NONE', #22015 ) ;
#46061 = CARTESIAN_POINT ( 'NONE',  ( 0.000000000000000000, -0.8299999999999999600, -1.199999999999999956 ) ) ;
#46062 = DIRECTION ( 'NONE',  ( 0.000000000000000000, 0.000000000000000000, 1.000000000000000000 ) ) ;
#46063 = CARTESIAN_POINT ( 'NONE',  ( -96.32499999999996021, -207.7050326799711968, 85.44916666666665606 ) ) ;
#46064 = DIRECTION ( 'NONE',  ( 0.000000000000000000, 0.000000000000000000, 1.000000000000000000 ) ) ;
#46065 = LINE ( 'NONE', #32905, #12259 ) ;
#46066 = FACE_BOUND ( 'NONE', #2450, .T. ) ;
#46067 = CYLINDRICAL_SURFACE ( 'NONE', #67174, 31.99999999999998579 ) ;
#46068 = DIRECTION ( 'NONE',  ( -1.000000000000000000, -0.000000000000000000, -0.000000000000000000 ) ) ;
#46069 = ORIENTED_EDGE ( 'NONE', *, *, #34357, .F. ) ;
#46070 = CARTESIAN_POINT ( 'NONE',  ( -92.34999999999999432, -209.9999999999999716, 84.04687500173430692 ) ) ;
#46071 = ORIENTED_EDGE ( 'NONE', *, *, #59641, .F. ) ;
#46072 = DIRECTION ( 'NONE',  ( -0.000000000000000000, -0.000000000000000000, 1.000000000000000000 ) ) ;
#46073 = ORIENTED_EDGE ( 'NONE', *, *, #70656, .T. ) ;
#46075 = CARTESIAN_POINT ( 'NONE',  ( -97.65000000000001990, 91.52997821335253548, 80.50145833506765314 ) ) ;
#46074 = CARTESIAN_POINT ( 'NONE',  ( 97.64999999999997726, 91.52997821335252127, 80.92479166840098515 ) ) ;
#46076 = AXIS2_PLACEMENT_3D ( 'NONE', #52604, #19133, #53715 ) ;
#46077 = ORIENTED_EDGE ( 'NONE', *, *, #27835, .T. ) ;
#46078 = CARTESIAN_POINT ( 'NONE',  ( 97.30629616937498838, 90.00000000000002842, 79.32406250086715715 ) ) ;
#46079 = CIRCLE ( 'NONE', #446, 31.99999999999999289 ) ;
#46080 = LINE ( 'NONE', #23889, #16924 ) ;
#46081 = CARTESIAN_POINT ( 'NONE',  ( 0.000000000000000000, -0.8299999999999999600, -1.199999999999999956 ) ) ;
#46082 = EDGE_CURVE ( 'NONE', #49121, #29989, #1621, .T. ) ;
#46083 = DIRECTION ( 'NONE',  ( -1.000000000000000000, 0.000000000000000000, -0.000000000000000000 ) ) ;
#46084 = CARTESIAN_POINT ( 'NONE',  ( 0.000000000000000000, -28.89263327155796901, 71.91182617369176455 ) ) ;
#46085 = VERTEX_POINT ( 'NONE', #73134 ) ;
#46086 = LINE ( 'NONE', #57362, #45971 ) ;
#46088 = CARTESIAN_POINT ( 'NONE',  ( 5.000000000000000000, 6.074766241781102566E-16, -0.5080592402122449114 ) ) ;
#46087 = AXIS2_PLACEMENT_3D ( 'NONE', #44251, #73547, #45378 ) ;
#46089 = AXIS2_PLACEMENT_3D ( 'NONE', #34630, #6086, #46291 ) ;
#46090 = FACE_OUTER_BOUND ( 'NONE', #58453, .T. ) ;
#46091 = EDGE_LOOP ( 'NONE', ( #29459, #65935, #73586, #39296, #31805, #68285 ) ) ;
#46092 = EDGE_CURVE ( 'NONE', #40791, #15499, #64818, .T. ) ;
#46093 = ORIENTED_EDGE ( 'NONE', *, *, #68504, .F. ) ;
#46094 = EDGE_CURVE ( 'NONE', #2723, #53818, #14367, .T. ) ;
#46095 = DIRECTION ( 'NONE',  ( -0.3853207896976533764, 0.9227826878668546895, 0.000000000000000000 ) ) ;
#46096 = DIRECTION ( 'NONE',  ( -1.000000000000000000, 0.000000000000000000, 0.000000000000000000 ) ) ;
#46097 = DIRECTION ( 'NONE',  ( -1.000000000000000000, 0.000000000000000000, 0.000000000000000000 ) ) ;
#46098 = CARTESIAN_POINT ( 'NONE',  ( -92.69370383062498320, -211.3315407142195852, 76.73114583420048973 ) ) ;
#46099 = ORIENTED_EDGE ( 'NONE', *, *, #67416, .F. ) ;
#46100 = AXIS2_PLACEMENT_3D ( 'NONE', #30149, #53458, #24884 ) ;
#46101 = EDGE_CURVE ( 'NONE', #57093, #10768, #56395, .T. ) ;
#46102 = DIRECTION ( 'NONE',  ( -1.000000000000000000, -0.000000000000000000, -0.000000000000000000 ) ) ;
#46103 = CARTESIAN_POINT ( 'NONE',  ( -96.67299840329707195, -211.9834083483352174, 74.96344747200149072 ) ) ;
#46104 = CARTESIAN_POINT ( 'NONE',  ( 92.34999999999999432, 90.00000000000002842, 75.00000000000000000 ) ) ;
#46105 = CARTESIAN_POINT ( 'NONE',  ( 96.48680242707320076, 91.80467564693685745, 74.81083481226639265 ) ) ;
#46106 = DIRECTION ( 'NONE',  ( 1.000000000000000000, 0.000000000000000000, 0.000000000000000000 ) ) ;
#46107 = CARTESIAN_POINT ( 'NONE',  ( 97.64999999981932888, 89.99996905681224746, 78.33187387208513996 ) ) ;
#46108 = LINE ( 'NONE', #40096, #62560 ) ;
#46109 = DIRECTION ( 'NONE',  ( 0.5200609990132993854, 0.8541291221503275466, 0.000000000000000000 ) ) ;
#46110 = LINE ( 'NONE', #28061, #47232 ) ;
#46111 = DIRECTION ( 'NONE',  ( 0.000000000000000000, 0.000000000000000000, 1.000000000000000000 ) ) ;
#46112 = EDGE_CURVE ( 'NONE', #2456, #7432, #9626, .T. ) ;
#46113 = ADVANCED_FACE ( 'NONE', ( #4004 ), #26904, .T. ) ;
#46114 = CARTESIAN_POINT ( 'NONE',  ( 94.99999999999998579, 87.33691857156068750, 86.78531250086713555 ) ) ;
#46115 = CARTESIAN_POINT ( 'NONE',  ( 0.000000000000000000, -120.0000000000000000, -125.0000000000000000 ) ) ;
#46116 = CARTESIAN_POINT ( 'NONE',  ( 12.00000000000000000, -1.278221433540507546, -26.51162292216071492 ) ) ;
#46117 = ORIENTED_EDGE ( 'NONE', *, *, #19028, .T. ) ;
#46118 = DIRECTION ( 'NONE',  ( -1.000000000000000000, -0.000000000000000000, 0.000000000000000000 ) ) ;
#46119 = CARTESIAN_POINT ( 'NONE',  ( -97.30629616937501680, 91.33154071421968467, 79.42989583420047950 ) ) ;
#46120 = EDGE_CURVE ( 'NONE', #9070, #50612, #18228, .T. ) ;
#46121 = EDGE_CURVE ( 'NONE', #71727, #15277, #34401, .T. ) ;
#46122 = AXIS2_PLACEMENT_3D ( 'NONE', #51878, #44766, #418 ) ;
#46123 = CARTESIAN_POINT ( 'NONE',  ( 97.30629616937498838, -208.6684592857803011, 89.37822916753381719 ) ) ;
#46124 = EDGE_CURVE ( 'NONE', #57825, #11290, #40777, .T. ) ;
#46125 = ORIENTED_EDGE ( 'NONE', *, *, #54175, .F. ) ;
#46126 = AXIS2_PLACEMENT_3D ( 'NONE', #11194, #11550, #56702 ) ;
#46127 = DIRECTION ( 'NONE',  ( 1.000000000000000000, 0.000000000000000000, 0.000000000000000000 ) ) ;
#46128 = DIRECTION ( 'NONE',  ( 0.000000000000000000, -0.9135454576426056406, 0.4067366430757897722 ) ) ;
#46129 = CARTESIAN_POINT ( 'NONE',  ( 0.000000000000000000, -15.33399622253541317, 80.55351364060584274 ) ) ;
#46130 = EDGE_CURVE ( 'NONE', #36429, #49000, #52065, .T. ) ;
#46131 = CIRCLE ( 'NONE', #33992, 16.00000000000000000 ) ;
#46132 = CYLINDRICAL_SURFACE ( 'NONE', #23935, 11.59999999999999787 ) ;
#46133 = VECTOR ( 'NONE', #9762, 1000.000000000000000 ) ;
#46134 = CARTESIAN_POINT ( 'NONE',  ( 92.69370383062501162, -211.3315407142195852, 76.51947916753381662 ) ) ;
#46135 = CARTESIAN_POINT ( 'NONE',  ( -235.0000123116479926, -123.0000000000000284, -2.500000000000000000 ) ) ;
#46136 = ORIENTED_EDGE ( 'NONE', *, *, #21445, .T. ) ;
#46137 = ORIENTED_EDGE ( 'NONE', *, *, #62141, .T. ) ;
#46138 = CARTESIAN_POINT ( 'NONE',  ( 97.30629616937498838, -209.9999999999999716, 80.59406250086715318 ) ) ;
#46139 = CARTESIAN_POINT ( 'NONE',  ( 97.64999999999999147, 90.00000000000002842, 89.68250000000000455 ) ) ;
#46141 = DIRECTION ( 'NONE',  ( 0.000000000000000000, 0.000000000000000000, -1.000000000000000000 ) ) ;
#46140 = CIRCLE ( 'NONE', #36516, 77.49899999999999523 ) ;
#46142 = CARTESIAN_POINT ( 'NONE',  ( 11.99999999999999822, 46.53671651294032330, -59.03961581697353012 ) ) ;
#46143 = CARTESIAN_POINT ( 'NONE',  ( 95.00000000000000000, -213.0599564267049857, 76.82374999999998977 ) ) ;
#46144 = DIRECTION ( 'NONE',  ( 0.000000000000000000, 0.000000000000000000, -1.000000000000000000 ) ) ;
#46145 = CARTESIAN_POINT ( 'NONE',  ( 97.64999999999997726, -211.5299782133524502, 87.08958333333333712 ) ) ;
#46146 = AXIS2_PLACEMENT_3D ( 'NONE', #59111, #36163, #64015 ) ;
#46147 = ORIENTED_EDGE ( 'NONE', *, *, #1490, .T. ) ;
#46148 = ORIENTED_EDGE ( 'NONE', *, *, #15773, .F. ) ;
#46149 = ORIENTED_EDGE ( 'NONE', *, *, #70890, .T. ) ;
#46150 = ORIENTED_EDGE ( 'NONE', *, *, #8735, .F. ) ;
#46151 = DIRECTION ( 'NONE',  ( 1.000000000000000000, 0.000000000000000000, 0.000000000000000000 ) ) ;
#46152 = CARTESIAN_POINT ( 'NONE',  ( -92.69370383062502583, 88.66845928578038638, 86.25614583420048120 ) ) ;
#46153 = CYLINDRICAL_SURFACE ( 'NONE', #65344, 2.649999999999985700 ) ;
#46154 = CARTESIAN_POINT ( 'NONE',  ( 0.000000000000000000, 0.000000000000000000, 53.20000000000001705 ) ) ;
#46155 = CARTESIAN_POINT ( 'NONE',  ( 97.64999999999999147, -209.9999999999999716, 77.69687500173431260 ) ) ;
#46156 = CARTESIAN_POINT ( 'NONE',  ( 97.64999999999997726, 88.47002178664753558, 77.56458333333333144 ) ) ;
#46157 = ORIENTED_EDGE ( 'NONE', *, *, #34921, .F. ) ;
#46158 = CYLINDRICAL_SURFACE ( 'NONE', #73109, 12.49999999999999645 ) ;
#46159 = ORIENTED_EDGE ( 'NONE', *, *, #2678, .T. ) ;
#46160 = CARTESIAN_POINT ( 'NONE',  ( 7.400000000000003908, -2.398995777955595453E-13, -23.50000000000040856 ) ) ;
#46161 = VECTOR ( 'NONE', #17150, 1000.000000000000000 ) ;
#46162 = ORIENTED_EDGE ( 'NONE', *, *, #27610, .T. ) ;
#46163 = CARTESIAN_POINT ( 'NONE',  ( 95.00000000000000000, -213.0599564267049857, 88.33312500173431658 ) ) ;
#46164 =( BOUNDED_CURVE ( )  B_SPLINE_CURVE ( 2, ( #50248, #37512, #38619, #61554, #4417, #60447, #43537 ),
 .UNSPECIFIED., .F., .F. ) 
 B_SPLINE_CURVE_WITH_KNOTS ( ( 3, 2, 2, 3 ),
 ( 0.3541666666666665741, 0.3611111111111109939, 0.3680555555555554137, 0.3749999999999998335 ),
 .UNSPECIFIED. ) 
 CURVE ( )  GEOMETRIC_REPRESENTATION_ITEM ( )  RATIONAL_B_SPLINE_CURVE ( ( 1.000000000000002220, 0.8660254037844365982, 1.000000000000000000, 0.8660254037844387076, 1.000000000000000000, 0.8660254037844419273, 0.9999999999999967804 ) ) 
 REPRESENTATION_ITEM ( '' )  );
#46165 = CARTESIAN_POINT ( 'NONE',  ( -95.00000000000002842, 87.33691857156074434, 81.07031250086716057 ) ) ;
#46166 = CARTESIAN_POINT ( 'NONE',  ( 93.84685191531248449, 88.00268892867053694, 89.27239583420049485 ) ) ;
#46167 = ORIENTED_EDGE ( 'NONE', *, *, #41177, .T. ) ;
#46168 = DIRECTION ( 'NONE',  ( 0.000000000000000000, -0.7431448254773954654, 0.6691306063588569053 ) ) ;
#46169 = CARTESIAN_POINT ( 'NONE',  ( 10.00000000000000000, -31.46837873495025306, 68.27212725128265447 ) ) ;
#46170 = ADVANCED_FACE ( 'NONE', ( #63365 ), #1360, .F. ) ;
#46171 = DIRECTION ( 'NONE',  ( 0.000000000000000000, 0.8660254037844379305, -0.5000000000000012212 ) ) ;
#46172 = VERTEX_POINT ( 'NONE', #982 ) ;
#46173 = DIRECTION ( 'NONE',  ( 0.000000000000000000, 0.000000000000000000, -1.000000000000000000 ) ) ;
#46174 = CARTESIAN_POINT ( 'NONE',  ( -92.69370383062498320, -208.6684592857803011, 78.58322916753381548 ) ) ;
#46175 = CIRCLE ( 'NONE', #68975, 32.00000000000000711 ) ;
#46176 = ORIENTED_EDGE ( 'NONE', *, *, #47053, .F. ) ;
#46177 = EDGE_CURVE ( 'NONE', #40541, #48516, #18590, .T. ) ;
#46178 = VERTEX_POINT ( 'NONE', #69729 ) ;
#46179 = DIRECTION ( 'NONE',  ( -1.000000000000000000, 0.000000000000000000, 0.000000000000000000 ) ) ;
#46180 = ADVANCED_FACE ( 'NONE', ( #6941 ), #6587, .T. ) ;
#46181 = EDGE_CURVE ( 'NONE', #66145, #36593, #29974, .T. ) ;
#46182 = ORIENTED_EDGE ( 'NONE', *, *, #60467, .T. ) ;
#46183 = CARTESIAN_POINT ( 'NONE',  ( -7.572224309238338336, -145.4393675041377492, 5.500000000000000000 ) ) ;
#46184 = AXIS2_PLACEMENT_3D ( 'NONE', #52511, #30323, #18306 ) ;
#46185 = VERTEX_POINT ( 'NONE', #34782 ) ;
#46186 = CARTESIAN_POINT ( 'NONE',  ( -94.99999999999997158, -207.3369185715606307, 76.78406250086712248 ) ) ;
#46187 = ORIENTED_EDGE ( 'NONE', *, *, #61387, .F. ) ;
#46188 = VECTOR ( 'NONE', #66998, 1000.000000000000000 ) ;
#46189 = CARTESIAN_POINT ( 'NONE',  ( 0.000000000000000000, -68.55367621811112144, -44.99326035066125939 ) ) ;
#46190 = CARTESIAN_POINT ( 'NONE',  ( 11.99999999999999822, -55.38113227695745167, -54.21277698773732823 ) ) ;
#46191 = VECTOR ( 'NONE', #3094, 1000.000000000000000 ) ;
#46192 = DIRECTION ( 'NONE',  ( -1.343011723336883198E-16, 1.000000000000000000, 0.000000000000000000 ) ) ;
#46193 = ORIENTED_EDGE ( 'NONE', *, *, #48658, .F. ) ;
#46194 = CARTESIAN_POINT ( 'NONE',  ( -10.43921258969510824, -98.89258801967538659, 5.500000000000000000 ) ) ;
#46195 = VECTOR ( 'NONE', #66377, 1000.000000000000000 ) ;
#46196 = EDGE_CURVE ( 'NONE', #28846, #68067, #5490, .T. ) ;
#46197 = CARTESIAN_POINT ( 'NONE',  ( 97.30629616937498838, 90.00000000000002842, 83.61031250086713840 ) ) ;
#46198 = DIRECTION ( 'NONE',  ( 0.000000000000000000, 0.000000000000000000, 1.000000000000000000 ) ) ;
#46199 = CARTESIAN_POINT ( 'NONE',  ( 10.00000000000000000, 4.992566952385523393, -37.16516213103272293 ) ) ;
#46200 = AXIS2_PLACEMENT_3D ( 'NONE', #56469, #51920, #73726 ) ;
#46201 = CYLINDRICAL_SURFACE ( 'NONE', #61301, 2.649999999999985700 ) ;
#46202 = CARTESIAN_POINT ( 'NONE',  ( -5.000000000000000000, 2.886751345948126879, -2.079999999999992077 ) ) ;
#46203 = ADVANCED_FACE ( 'NONE', ( #69358 ), #70086, .F. ) ;
#46204 = LINE ( 'NONE', #40934, #72823 ) ;
#46205 = FACE_OUTER_BOUND ( 'NONE', #12779, .T. ) ;
#46206 = CARTESIAN_POINT ( 'NONE',  ( 10.00000000000000000, -36.72794159290288718, 65.59268652807197952 ) ) ;
#46207 = AXIS2_PLACEMENT_3D ( 'NONE', #71719, #43188, #14587 ) ;
#46208 = DIRECTION ( 'NONE',  ( -1.000000000000000000, 3.469446951953611033E-15, 0.000000000000000000 ) ) ;
#46209 = DIRECTION ( 'NONE',  ( -1.000000000000000000, 0.000000000000000000, 0.000000000000000000 ) ) ;
#46210 = CARTESIAN_POINT ( 'NONE',  ( -97.30629616937501680, 91.33154071421968467, 88.95489583420048518 ) ) ;
#46211 = EDGE_CURVE ( 'NONE', #57222, #38625, #35987, .T. ) ;
#46212 = EDGE_CURVE ( 'NONE', #33465, #10745, #63013, .T. ) ;
#46213 = DIRECTION ( 'NONE',  ( -1.000000000000000000, -0.000000000000000000, -0.000000000000000000 ) ) ;
#46214 = CARTESIAN_POINT ( 'NONE',  ( 11.99999999999999822, -55.19960302592104284, 51.03279382321070301 ) ) ;
#46215 = ORIENTED_EDGE ( 'NONE', *, *, #65602, .T. ) ;
#46216 = DIRECTION ( 'NONE',  ( -1.000000000000000000, -0.000000000000000000, 0.000000000000000000 ) ) ;
#46217 = DIRECTION ( 'NONE',  ( -1.000000000000000000, -0.000000000000000000, 0.000000000000000000 ) ) ;
#46218 = DIRECTION ( 'NONE',  ( 2.603472992746261562E-14, 2.546204323184492723E-14, -1.000000000000000000 ) ) ;
#46219 = DIRECTION ( 'NONE',  ( 0.000000000000000000, 0.07845909572784512398, -0.9969173337331279638 ) ) ;
#46220 = AXIS2_PLACEMENT_3D ( 'NONE', #5489, #67134, #51320 ) ;
#46221 = CARTESIAN_POINT ( 'NONE',  ( 97.30629616937498838, -211.3315407142195852, 84.98614583420047097 ) ) ;
#46222 = ORIENTED_EDGE ( 'NONE', *, *, #45241, .F. ) ;
#46223 = ORIENTED_EDGE ( 'NONE', *, *, #3402, .F. ) ;
#46224 = DIRECTION ( 'NONE',  ( 0.000000000000000000, 0.000000000000000000, 1.000000000000000000 ) ) ;
#46225 = VERTEX_POINT ( 'NONE', #46432 ) ;
#46226 = CARTESIAN_POINT ( 'NONE',  ( -94.99999999999997158, -206.9400435732949575, 79.76062500173429726 ) ) ;
#46227 = CARTESIAN_POINT ( 'NONE',  ( 0.000000000000000000, -51.29473840253177741, -63.97538442413482329 ) ) ;
#46228 = VECTOR ( 'NONE', #24840, 1000.000000000000000 ) ;
#46229 = ORIENTED_EDGE ( 'NONE', *, *, #69543, .T. ) ;
#46230 = VECTOR ( 'NONE', #41353, 1000.000000000000000 ) ;
#46231 = CARTESIAN_POINT ( 'NONE',  ( 92.69370383062501162, -211.3315407142195852, 83.50447916753383026 ) ) ;
#46232 = ORIENTED_EDGE ( 'NONE', *, *, #13513, .F. ) ;
#46233 = CARTESIAN_POINT ( 'NONE',  ( -97.64999999999996305, -209.9999999999999716, 88.09499999999999886 ) ) ;
#46234 = VERTEX_POINT ( 'NONE', #22775 ) ;
#46235 = AXIS2_PLACEMENT_3D ( 'NONE', #35298, #29634, #15880 ) ;
#46236 = ORIENTED_EDGE ( 'NONE', *, *, #65218, .F. ) ;
#46237 = DIRECTION ( 'NONE',  ( -1.000000000000000000, 7.571541139944063212E-15, 2.603472992745718826E-14 ) ) ;
#46238 = LINE ( 'NONE', #57523, #10048 ) ;
#46239 = CIRCLE ( 'NONE', #58254, 31.99999999999998579 ) ;
#46240 = ORIENTED_EDGE ( 'NONE', *, *, #36054, .F. ) ;
#46241 = CARTESIAN_POINT ( 'NONE',  ( 92.34999999999999432, 90.00000000000002842, 86.18999999999999773 ) ) ;
#46242 = CARTESIAN_POINT ( 'NONE',  ( 97.64999999999999147, -209.9999999999999716, 88.49187500173430010 ) ) ;
#46243 = EDGE_LOOP ( 'NONE', ( #17979, #67406, #54648, #18757 ) ) ;
#46244 = CARTESIAN_POINT ( 'NONE',  ( -10.43921258969510824, -98.89258801967538659, 5.500000000000000000 ) ) ;
#46245 = ORIENTED_EDGE ( 'NONE', *, *, #30198, .F. ) ;
#46246 = DIRECTION ( 'NONE',  ( 0.000000000000000000, 0.000000000000000000, 1.000000000000000000 ) ) ;
#46247 = EDGE_LOOP ( 'NONE', ( #15109, #72565, #12396, #17490 ) ) ;
#46248 = VECTOR ( 'NONE', #49486, 1000.000000000000000 ) ;
#46249 = EDGE_CURVE ( 'NONE', #11167, #22373, #45716, .T. ) ;
#46250 = EDGE_CURVE ( 'NONE', #35224, #14992, #17488, .T. ) ;
#46251 = ORIENTED_EDGE ( 'NONE', *, *, #62688, .F. ) ;
#46252 = VERTEX_POINT ( 'NONE', #40415 ) ;
#46253 = CARTESIAN_POINT ( 'NONE',  ( -97.65000000000001990, 90.00000000000004263, 90.00000000000000000 ) ) ;
#46254 = DIRECTION ( 'NONE',  ( 0.000000000000000000, 0.000000000000000000, 1.000000000000000000 ) ) ;
#46255 = EDGE_LOOP ( 'NONE', ( #228, #57744 ) ) ;
#46256 = ORIENTED_EDGE ( 'NONE', *, *, #59497, .T. ) ;
#46257 = EDGE_CURVE ( 'NONE', #22414, #3329, #51704, .T. ) ;
#46258 = AXIS2_PLACEMENT_3D ( 'NONE', #47210, #30636, #2502 ) ;
#46259 = EDGE_LOOP ( 'NONE', ( #66948, #20140, #28049, #51209 ) ) ;
#46260 = CARTESIAN_POINT ( 'NONE',  ( -97.65000000000001990, 90.00000000000004263, 86.18999999999999773 ) ) ;
#46261 = DIRECTION ( 'NONE',  ( 0.000000000000000000, -1.000000000000000000, 1.181994176819165452E-15 ) ) ;
#46262 = ADVANCED_FACE ( 'NONE', ( #57722 ), #46067, .T. ) ;
#46263 = CARTESIAN_POINT ( 'NONE',  ( -93.67500000000003979, 92.29496732002878900, 86.61333333333332973 ) ) ;
#46264 = EDGE_LOOP ( 'NONE', ( #6923, #31699, #13859, #47360 ) ) ;
#46265 = CARTESIAN_POINT ( 'NONE',  ( 0.000000000000000000, 0.000000000000000000, 0.000000000000000000 ) ) ;
#46266 = ORIENTED_EDGE ( 'NONE', *, *, #2890, .T. ) ;
#46267 = CARTESIAN_POINT ( 'NONE',  ( -94.99999999999997158, -209.9999999999999716, 75.00000000000000000 ) ) ;
#46268 = CARTESIAN_POINT ( 'NONE',  ( -94.99999999999997158, -207.3369185715606307, 86.94406250086714749 ) ) ;
#46270 = ORIENTED_EDGE ( 'NONE', *, *, #62650, .T. ) ;
#46269 = EDGE_CURVE ( 'NONE', #7045, #11463, #47967, .T. ) ;
#46271 = CARTESIAN_POINT ( 'NONE',  ( -94.99999999999997158, -213.0599564267049857, 79.44312500173430180 ) ) ;
#46272 = DIRECTION ( 'NONE',  ( 1.000000000000000000, 0.000000000000000000, 0.000000000000000000 ) ) ;
#46273 = DIRECTION ( 'NONE',  ( -1.000000000000000000, 0.000000000000000000, 0.000000000000000000 ) ) ;
#46274 = CARTESIAN_POINT ( 'NONE',  ( -94.99999999999997158, -207.3369185715606307, 74.87906250086713555 ) ) ;
#46275 = DIRECTION ( 'NONE',  ( 0.000000000000000000, 0.000000000000000000, 1.000000000000000000 ) ) ;
#46276 = CARTESIAN_POINT ( 'NONE',  ( 5.000000000000000000, -35.47612816024506088, -22.48208911017539435 ) ) ;
#46277 = CIRCLE ( 'NONE', #13828, 37.49900000000000233 ) ;
#46278 = CYLINDRICAL_SURFACE ( 'NONE', #8509, 16.00000000000000000 ) ;
#46279 = CARTESIAN_POINT ( 'NONE',  ( 0.000000000000000000, 0.000000000000000000, 53.20000000000001705 ) ) ;
#46280 = EDGE_CURVE ( 'NONE', #72968, #55761, #36256, .T. ) ;
#46281 = CARTESIAN_POINT ( 'NONE',  ( -4.250000000000000000, -13.95926121303099343, -1.199999999999999956 ) ) ;
#46282 = EDGE_CURVE ( 'NONE', #1736, #30220, #34760, .T. ) ;
#46283 = CARTESIAN_POINT ( 'NONE',  ( -92.69370383062502583, 88.66845928578038638, 79.11239583420046984 ) ) ;
#46284 = DIRECTION ( 'NONE',  ( -1.000000000000000000, -0.000000000000000000, -0.000000000000000000 ) ) ;
#46285 = DIRECTION ( 'NONE',  ( -1.000000000000000000, 0.000000000000000000, 0.000000000000000000 ) ) ;
#46286 = AXIS2_PLACEMENT_3D ( 'NONE', #6253, #47237, #47598 ) ;
#46287 = EDGE_LOOP ( 'NONE', ( #7665, #8624, #66759, #15993 ) ) ;
#46288 = AXIS2_PLACEMENT_3D ( 'NONE', #40067, #63026, #26918 ) ;
#46289 = DIRECTION ( 'NONE',  ( 1.000000000000000000, 0.000000000000000000, 0.000000000000000000 ) ) ;
#46291 = DIRECTION ( 'NONE',  ( 0.000000000000000000, 0.000000000000000000, 1.000000000000000000 ) ) ;
#46290 = AXIS2_PLACEMENT_3D ( 'NONE', #2234, #20210, #64249 ) ;
#46292 = DIRECTION ( 'NONE',  ( -0.000000000000000000, -0.000000000000000000, 1.000000000000000000 ) ) ;
#46293 = EDGE_CURVE ( 'NONE', #18771, #57844, #53929, .T. ) ;
#46294 = EDGE_CURVE ( 'NONE', #8967, #67395, #19132, .T. ) ;
#46295 = DIRECTION ( 'NONE',  ( 0.000000000000000000, -0.4539904997395542430, 0.8910065241883641241 ) ) ;
#46296 = DIRECTION ( 'NONE',  ( -1.000000000000000000, 0.000000000000000000, 0.000000000000000000 ) ) ;
#46297 = DIRECTION ( 'NONE',  ( -1.000000000000000000, 0.000000000000000000, -0.000000000000000000 ) ) ;
#46298 = CARTESIAN_POINT ( 'NONE',  ( -97.30629616937495996, -209.9999999999999716, 76.46656250086715545 ) ) ;
#46299 = CIRCLE ( 'NONE', #34264, 15.70000000000327312 ) ;
#46300 = DIRECTION ( 'NONE',  ( 1.000000000000000000, 0.000000000000000000, 0.000000000000000000 ) ) ;
#46301 = VECTOR ( 'NONE', #47833, 1000.000000000000000 ) ;
#46302 = ORIENTED_EDGE ( 'NONE', *, *, #20097, .F. ) ;
#46303 = CARTESIAN_POINT ( 'NONE',  ( 0.000000000000000000, 0.000000000000000000, 0.000000000000000000 ) ) ;
#46304 = CARTESIAN_POINT ( 'NONE',  ( 92.34999999999998010, -211.5299782133523934, 88.14791666666667425 ) ) ;
#46305 = FACE_OUTER_BOUND ( 'NONE', #39576, .T. ) ;
#46306 = LINE ( 'NONE', #69603, #4164 ) ;
#46307 = VECTOR ( 'NONE', #39562, 1000.000000000000000 ) ;
#46308 = FACE_OUTER_BOUND ( 'NONE', #51756, .T. ) ;
#46309 = VERTEX_POINT ( 'NONE', #13324 ) ;
#46310 = DIRECTION ( 'NONE',  ( 0.000000000000000000, 0.000000000000000000, 1.000000000000000000 ) ) ;
#46311 = DIRECTION ( 'NONE',  ( 0.000000000000000000, 0.000000000000000000, 1.000000000000000000 ) ) ;
#46312 = VERTEX_POINT ( 'NONE', #60322 ) ;
#46313 = CARTESIAN_POINT ( 'NONE',  ( 92.69370383062501162, -211.3315407142195852, 85.25072916753379104 ) ) ;
#46314 = CARTESIAN_POINT ( 'NONE',  ( 15.00000000000000000, 16.83928648764922542, -16.46020748918050458 ) ) ;
#46315 = ORIENTED_EDGE ( 'NONE', *, *, #55067, .F. ) ;
#46316 = EDGE_CURVE ( 'NONE', #13677, #28951, #48653, .T. ) ;
#46317 = CARTESIAN_POINT ( 'NONE',  ( 11.99999999999999822, 0.000000000000000000, 0.000000000000000000 ) ) ;
#46318 = EDGE_LOOP ( 'NONE', ( #22291, #37408, #63173 ) ) ;
#46319 = CARTESIAN_POINT ( 'NONE',  ( 96.32499999999998863, -212.2949673200287179, 85.21104166840096639 ) ) ;
#46320 = ORIENTED_EDGE ( 'NONE', *, *, #46885, .F. ) ;
#46321 = CARTESIAN_POINT ( 'NONE',  ( -92.69370383062502583, 88.66845928578038638, 79.90614583420048689 ) ) ;
#46322 = ORIENTED_EDGE ( 'NONE', *, *, #61640, .F. ) ;
#46323 = DIRECTION ( 'NONE',  ( -1.000000000000000000, 0.000000000000000000, 0.000000000000000000 ) ) ;
#46324 = ORIENTED_EDGE ( 'NONE', *, *, #46689, .F. ) ;
#46325 = EDGE_CURVE ( 'NONE', #36437, #14549, #2395, .T. ) ;
#46326 = ORIENTED_EDGE ( 'NONE', *, *, #35733, .T. ) ;
#46327 = LINE ( 'NONE', #507, #63250 ) ;
#46328 = EDGE_CURVE ( 'NONE', #51512, #5579, #4014, .T. ) ;
#46329 = ORIENTED_EDGE ( 'NONE', *, *, #42102, .F. ) ;
#46330 = EDGE_CURVE ( 'NONE', #7213, #68917, #5969, .T. ) ;
#46331 = EDGE_LOOP ( 'NONE', ( #12374, #18740, #65450, #63299 ) ) ;
#46332 = FACE_OUTER_BOUND ( 'NONE', #36672, .T. ) ;
#46333 = AXIS2_PLACEMENT_3D ( 'NONE', #31275, #14359, #25639 ) ;
#46334 = ORIENTED_EDGE ( 'NONE', *, *, #56396, .F. ) ;
#46335 = EDGE_CURVE ( 'NONE', #1516, #10101, #17963, .T. ) ;
#46336 = ORIENTED_EDGE ( 'NONE', *, *, #63488, .F. ) ;
#46337 = CARTESIAN_POINT ( 'NONE',  ( 97.30629616937498838, 90.00000000000002842, 84.24531250086714351 ) ) ;
#46338 = EDGE_LOOP ( 'NONE', ( #14263, #22578, #60304, #65673 ) ) ;
#46339 = CIRCLE ( 'NONE', #53525, 31.99999999999998934 ) ;
#46340 = CARTESIAN_POINT ( 'NONE',  ( 96.15314808468748708, -208.0026889286704943, 83.08114583420048405 ) ) ;
#46341 = PRODUCT_CONTEXT ( 'NONE', #57098, 'mechanical' ) ;
#46342 = DIRECTION ( 'NONE',  ( 0.000000000000000000, -0.3090169943749549453, 0.9510565162951511997 ) ) ;
#46343 = DIRECTION ( 'NONE',  ( 0.000000000000000000, 0.1564344650402244852, 0.9876883405951387696 ) ) ;
#46344 = VECTOR ( 'NONE', #29729, 1000.000000000000114 ) ;
#46345 = DIRECTION ( 'NONE',  ( -1.000000000000000000, 0.000000000000000000, 0.000000000000000000 ) ) ;
#46346 = ADVANCED_FACE ( 'NONE', ( #3188 ), #20065, .F. ) ;
#46347 = DIRECTION ( 'NONE',  ( 0.000000000000000000, 0.6691306063588570163, -0.7431448254773953543 ) ) ;
#46348 = CIRCLE ( 'NONE', #767, 26.50000000000552092 ) ;
#46349 = LINE ( 'NONE', #23056, #60060 ) ;
#46350 = CARTESIAN_POINT ( 'NONE',  ( -92.35000000000003695, 90.00000000000004263, 82.69749999999999091 ) ) ;
#46351 = CARTESIAN_POINT ( 'NONE',  ( -97.30629616937497417, -208.6684592857803011, 83.23989583420046756 ) ) ;
#46352 = CARTESIAN_POINT ( 'NONE',  ( -97.30629616937501680, 90.00000000000004263, 83.45156250086715488 ) ) ;
#46353 = ORIENTED_EDGE ( 'NONE', *, *, #43635, .T. ) ;
#46354 = CARTESIAN_POINT ( 'NONE',  ( 97.30629616937498838, 90.00000000000002842, 84.24531250086714351 ) ) ;
#46355 = CIRCLE ( 'NONE', #48758, 31.99999999999998579 ) ;
#46356 = ORIENTED_EDGE ( 'NONE', *, *, #73671, .T. ) ;
#46357 = DIRECTION ( 'NONE',  ( 2.603472992746261562E-14, 2.546204323184492723E-14, -1.000000000000000000 ) ) ;
#46358 = ADVANCED_FACE ( 'NONE', ( #47544 ), #53551, .F. ) ;
#46359 = CARTESIAN_POINT ( 'NONE',  ( 97.65000000000000568, -211.5299782133524218, 76.37395833506761278 ) ) ;
#46360 = CARTESIAN_POINT ( 'NONE',  ( 95.00000000000000000, -209.9999999999999716, 90.00000000000000000 ) ) ;
#46361 = CARTESIAN_POINT ( 'NONE',  ( 92.35000000000006537, -208.4700217866474077, 85.50208333333331723 ) ) ;
#46362 = CARTESIAN_POINT ( 'NONE',  ( -92.69370383062498320, -211.3315407142195852, 86.09739583420048348 ) ) ;
#46363 = CARTESIAN_POINT ( 'NONE',  ( 11.99999999999999822, -71.91182617369167929, -28.89263327155821059 ) ) ;
#46364 = CARTESIAN_POINT ( 'NONE',  ( 97.64999999999999147, 90.00000000000002842, 80.15749999999999886 ) ) ;
#46365 = DIRECTION ( 'NONE',  ( 1.000000000000000000, -0.000000000000000000, -0.000000000000000000 ) ) ;
#46366 = FACE_OUTER_BOUND ( 'NONE', #58710, .T. ) ;
#46367 = ORIENTED_EDGE ( 'NONE', *, *, #56017, .T. ) ;
#46368 = AXIS2_PLACEMENT_3D ( 'NONE', #127, #45588, #68511 ) ;
#46369 = ORIENTED_EDGE ( 'NONE', *, *, #45409, .T. ) ;
#46370 = CARTESIAN_POINT ( 'NONE',  ( -95.00000000000002842, 93.05995642670501411, 77.14124999999999943 ) ) ;
#46371 = EDGE_CURVE ( 'NONE', #35258, #10635, #18956, .T. ) ;
#46372 = CARTESIAN_POINT ( 'NONE',  ( 0.000000000000000000, 0.000000000000000000, -20.00000000000000000 ) ) ;
#46373 = EDGE_CURVE ( 'NONE', #58617, #35612, #66329, .T. ) ;
#46374 = CARTESIAN_POINT ( 'NONE',  ( -10.00000000000000000, 0.000000000000000000, 0.000000000000000000 ) ) ;
#46375 = CARTESIAN_POINT ( 'NONE',  ( 10.00000000000000000, -16.23288003029473359, -33.80338159004301701 ) ) ;
#46376 =( BOUNDED_CURVE ( )  B_SPLINE_CURVE ( 2, ( #22527, #50712, #22153, #52194, #5992, #39074, #68013 ),
 .UNSPECIFIED., .F., .F. ) 
 B_SPLINE_CURVE_WITH_KNOTS ( ( 3, 2, 2, 3 ),
 ( 0.2083333333333331483, 0.2152777777777775681, 0.2222222222222219323, 0.2291666666666663521 ),
 .UNSPECIFIED. ) 
 CURVE ( )  GEOMETRIC_REPRESENTATION_ITEM ( )  RATIONAL_B_SPLINE_CURVE ( ( 1.000000000000003775, 0.8660254037844349329, 1.000000000000000000, 0.8660254037844387076, 1.000000000000000000, 0.8660254037844445918, 0.9999999999999941158 ) ) 
 REPRESENTATION_ITEM ( '' )  );
#46377 = CARTESIAN_POINT ( 'NONE',  ( 92.35000000007822507, -209.9999869687480611, 79.28395951162927702 ) ) ;
#46378 = ORIENTED_EDGE ( 'NONE', *, *, #57877, .F. ) ;
#46379 = CARTESIAN_POINT ( 'NONE',  ( -93.84685191531252713, 88.00268892867056536, 78.42447916753381776 ) ) ;
#46380 = CARTESIAN_POINT ( 'NONE',  ( 0.000000000000000000, -41.81611651403859042, -3.925862922256606602 ) ) ;
#46381 = DIRECTION ( 'NONE',  ( -0.000000000000000000, -0.000000000000000000, -1.000000000000000000 ) ) ;
#46382 = CLOSED_SHELL ( 'NONE', ( #47762, #26117, #21765, #1012, #18764, #6458, #54087, #15892, #26231, #42430, #38300, #43279, #27608, #61796, #21717, #14580, #16915, #16372, #28523, #61217, #47940, #39670, #46551, #59241 ) ) ;
#46383 = DIRECTION ( 'NONE',  ( 0.000000000000000000, 0.000000000000000000, 1.000000000000000000 ) ) ;
#46384 = PLANE ( 'NONE',  #38126 ) ;
#46385 = CARTESIAN_POINT ( 'NONE',  ( 0.000000000000000000, 46.21855187248628738, 62.20884554314034887 ) ) ;
#46386 = CARTESIAN_POINT ( 'NONE',  ( -97.30629616937497417, -211.3315407142195852, 85.40947916753380298 ) ) ;
#46387 = FILL_AREA_STYLE ('',( #2040 ) ) ;
#46388 = CIRCLE ( 'NONE', #39193, 31.99999999999998934 ) ;
#46389 = CARTESIAN_POINT ( 'NONE',  ( 92.69370383062498320, 88.66845928578035796, 76.51947916753381662 ) ) ;
#46390 = CARTESIAN_POINT ( 'NONE',  ( -97.30629616937497417, -208.6684592857803295, 80.85864583420048746 ) ) ;
#46391 = LINE ( 'NONE', #34741, #39869 ) ;
#46392 = ORIENTED_EDGE ( 'NONE', *, *, #22959, .F. ) ;
#46393 = DIRECTION ( 'NONE',  ( -3.061616997868382648E-16, -1.000000000000000000, 0.000000000000000000 ) ) ;
#46394 = CARTESIAN_POINT ( 'NONE',  ( -93.67499999999998295, -207.7050326799711968, 75.18333333333332291 ) ) ;
#46395 = CARTESIAN_POINT ( 'NONE',  ( -97.64999999998390479, 89.99999393654049129, 88.17456390440148084 ) ) ;
#46396 = AXIS2_PLACEMENT_3D ( 'NONE', #32456, #21169, #27178 ) ;
#46397 = AXIS2_PLACEMENT_3D ( 'NONE', #28159, #15771, #50717 ) ;
#46398 = DIRECTION ( 'NONE',  ( 1.000000000000000000, 0.000000000000000000, 0.000000000000000000 ) ) ;
#46399 = CARTESIAN_POINT ( 'NONE',  ( 97.30629616937498838, -208.6684592857803011, 75.40822916753381833 ) ) ;
#46400 = ORIENTED_EDGE ( 'NONE', *, *, #47523, .T. ) ;
#46401 = EDGE_CURVE ( 'NONE', #18859, #13504, #39655, .T. ) ;
#46402 = VECTOR ( 'NONE', #61355, 1000.000000000000000 ) ;
#46403 = CARTESIAN_POINT ( 'NONE',  ( 10.00000000000000000, -14.67089635893658794, -73.72996012237454977 ) ) ;
#46404 = VERTEX_POINT ( 'NONE', #59196 ) ;
#46405 = CIRCLE ( 'NONE', #3059, 82.00000000000000000 ) ;
#46406 = CARTESIAN_POINT ( 'NONE',  ( -92.35000000000003695, 90.00000000000004263, 85.23749999999999716 ) ) ;
#46407 = ORIENTED_EDGE ( 'NONE', *, *, #54267, .T. ) ;
#46408 = CARTESIAN_POINT ( 'NONE',  ( -96.32500000000001705, 92.29496732002878900, 79.17854166840096752 ) ) ;
#46409 = VECTOR ( 'NONE', #28543, 1000.000000000000000 ) ;
#46410 = ORIENTED_EDGE ( 'NONE', *, *, #50074, .F. ) ;
#46411 = ORIENTED_EDGE ( 'NONE', *, *, #38041, .F. ) ;
#46412 = EDGE_CURVE ( 'NONE', #71004, #47656, #50423, .T. ) ;
#46413 = ORIENTED_EDGE ( 'NONE', *, *, #1254, .T. ) ;
#46414 = CARTESIAN_POINT ( 'NONE',  ( -92.35000000000003695, -211.5299782133524786, 77.56458333333333144 ) ) ;
#46415 = EDGE_CURVE ( 'NONE', #1159, #4950, #30976, .T. ) ;
#46416 = ORIENTED_EDGE ( 'NONE', *, *, #15604, .F. ) ;
#46417 = VERTEX_POINT ( 'NONE', #33570 ) ;
#46418 = CARTESIAN_POINT ( 'NONE',  ( 97.30629616937498838, 91.33154071421968467, 82.55197916753382970 ) ) ;
#46419 = CARTESIAN_POINT ( 'NONE',  ( 95.53230763903961531, -213.2667778271277541, 74.92222617501690252 ) ) ;
#46420 = EDGE_LOOP ( 'NONE', ( #27687, #72579, #45702, #17613 ) ) ;
#46421 = EDGE_CURVE ( 'NONE', #26602, #43461, #55254, .T. ) ;
#46422 = ORIENTED_EDGE ( 'NONE', *, *, #50910, .F. ) ;
#46423 = EDGE_CURVE ( 'NONE', #18937, #3856, #24032, .T. ) ;
#46424 = EDGE_LOOP ( 'NONE', ( #46918, #29482, #53248, #36819 ) ) ;
#46425 = ORIENTED_EDGE ( 'NONE', *, *, #67848, .F. ) ;
#46426 = CLOSED_SHELL ( 'NONE', ( #48528, #22067, #35083, #49507, #63502, #65636, #38015, #66137, #42265, #14833, #43289, #9500, #12198, #61464, #46768, #9492, #3241, #38537 ) ) ;
#46427 = CARTESIAN_POINT ( 'NONE',  ( 0.000000000000000000, -120.0000000000000000, 40.00000000000000000 ) ) ;
#46428 = CYLINDRICAL_SURFACE ( 'NONE', #25877, 77.49899999999999523 ) ;
#46429 = FACE_OUTER_BOUND ( 'NONE', #61599, .T. ) ;
#46430 = CARTESIAN_POINT ( 'NONE',  ( -93.33864827737279768, 88.39919842643631398, 74.79754476654878204 ) ) ;
#46431 = DIRECTION ( 'NONE',  ( 0.000000000000000000, 0.8090169943749445647, 0.5877852522924770229 ) ) ;
#46432 = CARTESIAN_POINT ( 'NONE',  ( 10.00000000000000000, 50.95692526931414790, -58.39081064771693974 ) ) ;
#46433 = DIRECTION ( 'NONE',  ( 0.000000000000000000, 0.3090169943749411785, 0.9510565162951556406 ) ) ;
#46434 = ORIENTED_EDGE ( 'NONE', *, *, #13218, .F. ) ;
#46435 = CARTESIAN_POINT ( 'NONE',  ( -92.34999999999999432, -211.5299782133524502, 78.27895833506762813 ) ) ;
#46436 = ORIENTED_EDGE ( 'NONE', *, *, #915, .F. ) ;
#46437 = CARTESIAN_POINT ( 'NONE',  ( -10.00000000000000000, 0.000000000000000000, 0.000000000000000000 ) ) ;
#46438 = ORIENTED_EDGE ( 'NONE', *, *, #62895, .T. ) ;
#46440 = CARTESIAN_POINT ( 'NONE',  ( -97.65000000000001990, 91.52997821335253548, 79.86645833506761960 ) ) ;
#46439 = CARTESIAN_POINT ( 'NONE',  ( 97.64999999999997726, 91.52997821335252127, 80.28979166840098003 ) ) ;
#46441 = EDGE_LOOP ( 'NONE', ( #33939, #21710 ) ) ;
#46442 = CARTESIAN_POINT ( 'NONE',  ( 92.69370383062498320, 90.00000000000002842, 80.91156250086716284 ) ) ;
#46443 = EDGE_CURVE ( 'NONE', #51420, #12142, #15548, .T. ) ;
#46444 = AXIS2_PLACEMENT_3D ( 'NONE', #61257, #32661, #55606 ) ;
#46445 = CARTESIAN_POINT ( 'NONE',  ( -92.35000000000000853, -208.4700217866474929, 82.11541666666664696 ) ) ;
#46446 = CYLINDRICAL_SURFACE ( 'NONE', #13840, 16.00000000000000000 ) ;
#46447 = CARTESIAN_POINT ( 'NONE',  ( 92.35000000007822507, -209.9999869687480611, 79.28395951162927702 ) ) ;
#46448 = AXIS2_PLACEMENT_3D ( 'NONE', #36149, #47798, #8319 ) ;
#46449 = DIRECTION ( 'NONE',  ( -1.000000000000000000, 0.000000000000000000, 0.000000000000000000 ) ) ;
#46450 = ORIENTED_EDGE ( 'NONE', *, *, #29348, .T. ) ;
#46451 = CARTESIAN_POINT ( 'NONE',  ( 10.00000000000000000, 50.23322058963347558, 64.81221759200361987 ) ) ;
#46452 = FACE_OUTER_BOUND ( 'NONE', #41628, .T. ) ;
#46453 = ORIENTED_EDGE ( 'NONE', *, *, #52786, .T. ) ;
#46454 = ORIENTED_EDGE ( 'NONE', *, *, #11523, .F. ) ;
#46455 = AXIS2_PLACEMENT_3D ( 'NONE', #5159, #39354, #50997 ) ;
#46456 = EDGE_CURVE ( 'NONE', #25992, #12200, #33197, .T. ) ;
#46457 = EDGE_CURVE ( 'NONE', #62129, #3606, #66065, .T. ) ;
#46458 = DIRECTION ( 'NONE',  ( 0.9997280174009348652, -0.02332147558787931590, 0.000000000000000000 ) ) ;
#46459 = AXIS2_PLACEMENT_3D ( 'NONE', #26664, #49593, #21024 ) ;
#46460 = CARTESIAN_POINT ( 'NONE',  ( 11.99999999999999822, 71.27951684758026829, 30.41916302227139113 ) ) ;
#46461 = DIRECTION ( 'NONE',  ( 1.000000000000000000, 0.000000000000000000, 0.000000000000000000 ) ) ;
#46462 = CARTESIAN_POINT ( 'NONE',  ( -92.69370383062498320, -211.3315407142195852, 78.63614583420049087 ) ) ;
#46463 = ADVANCED_FACE ( 'NONE', ( #73421 ), #45246, .T. ) ;
#46464 = ORIENTED_EDGE ( 'NONE', *, *, #3862, .F. ) ;
#46465 = DIRECTION ( 'NONE',  ( -1.000000000000000000, -0.000000000000000000, -0.000000000000000000 ) ) ;
#46466 = CARTESIAN_POINT ( 'NONE',  ( 0.000000000000000000, -120.0000000000000000, 2.500000000000000000 ) ) ;
#46467 = AXIS2_PLACEMENT_3D ( 'NONE', #8503, #65646, #49083 ) ;
#46468 = CYLINDRICAL_SURFACE ( 'NONE', #59808, 31.99999999999999289 ) ;
#46469 = LINE ( 'NONE', #69392, #16443 ) ;
#46470 = DIRECTION ( 'NONE',  ( 0.000000000000000000, -0.6494480483301903195, 0.7604059656000252687 ) ) ;
#46471 = DIRECTION ( 'NONE',  ( -1.000000000000000000, -0.000000000000000000, -0.000000000000000000 ) ) ;
#46472 = CARTESIAN_POINT ( 'NONE',  ( 11.99999999999999822, 0.000000000000000000, 0.000000000000000000 ) ) ;
#46473 = DIRECTION ( 'NONE',  ( 0.000000000000000000, 0.8090169943749445647, 0.5877852522924770229 ) ) ;
#46474 = DIRECTION ( 'NONE',  ( -1.000000000000000000, -0.000000000000000000, -0.000000000000000000 ) ) ;
#46475 = VECTOR ( 'NONE', #52050, 1000.000000000000114 ) ;
#46476 = CARTESIAN_POINT ( 'NONE',  ( 0.000000000000000000, 72.35432306680455383, 20.40083707023012494 ) ) ;
#46477 = CARTESIAN_POINT ( 'NONE',  ( 93.84685191531248449, 91.99731107132950569, 88.42572916753381662 ) ) ;
#46478 = DIRECTION ( 'NONE',  ( -1.000000000000000000, 0.000000000000000000, 0.000000000000000000 ) ) ;
#46479 = FACE_OUTER_BOUND ( 'NONE', #59088, .T. ) ;
#46480 = ORIENTED_EDGE ( 'NONE', *, *, #33882, .F. ) ;
#46481 = DIRECTION ( 'NONE',  ( 1.000000000000000000, -7.619177619974977057E-15, -2.612289469705706555E-14 ) ) ;
#46482 = CARTESIAN_POINT ( 'NONE',  ( -92.69370383062504004, 90.00000000000004263, 79.16531250086714522 ) ) ;
#46483 = CARTESIAN_POINT ( 'NONE',  ( 97.30629616937498838, -209.9999999999999716, 87.42031250086714067 ) ) ;
#46484 = ADVANCED_FACE ( 'NONE', ( #72668 ), #21546, .F. ) ;
#46485 = ORIENTED_EDGE ( 'NONE', *, *, #39318, .F. ) ;
#46486 = CARTESIAN_POINT ( 'NONE',  ( 96.32499999999998863, -212.2949673200287179, 80.13104166840095388 ) ) ;
#46487 = DIRECTION ( 'NONE',  ( 0.000000000000000000, 0.8090169943749446757, 0.5877852522924769119 ) ) ;
#46488 = COLOUR_RGB ( '', 0.72549020, 0.75294118, 0.79215686) ;
#46489 = ORIENTED_EDGE ( 'NONE', *, *, #40070, .T. ) ;
#46490 = DIRECTION ( 'NONE',  ( -1.000000000000000000, 0.000000000000000000, -0.000000000000000000 ) ) ;
#46491 = EDGE_CURVE ( 'NONE', #58612, #62434, #40837, .T. ) ;
#46492 = CARTESIAN_POINT ( 'NONE',  ( -3.000000000000000000, -3.948201729842038432, -23.21447184625298021 ) ) ;
#46493 = AXIS2_PLACEMENT_3D ( 'NONE', #38405, #67718, #3838 ) ;
#46494 = ORIENTED_EDGE ( 'NONE', *, *, #31579, .T. ) ;
#46495 = VECTOR ( 'NONE', #50535, 1000.000000000000000 ) ;
#46496 = EDGE_CURVE ( 'NONE', #12032, #14707, #21170, .T. ) ;
#46497 = ORIENTED_EDGE ( 'NONE', *, *, #25273, .T. ) ;
#46498 = CARTESIAN_POINT ( 'NONE',  ( 95.00000000000000000, -212.6630814284392557, 81.07031250086716057 ) ) ;
#46499 = CARTESIAN_POINT ( 'NONE',  ( 92.34999999999999432, 90.00000000000002842, 90.00000000000000000 ) ) ;
#46500 = CIRCLE ( 'NONE', #21259, 77.49899999999999523 ) ;
#46501 = DIRECTION ( 'NONE',  ( -1.000000000000000000, 0.000000000000000000, 0.000000000000000000 ) ) ;
#46502 = CARTESIAN_POINT ( 'NONE',  ( -10.90076147243505211, 0.000000000000000000, 13.71319123027096865 ) ) ;
#46503 = CARTESIAN_POINT ( 'NONE',  ( 97.64998666484400758, 91.52998591240842075, 83.46479220096851748 ) ) ;
#46504 = CARTESIAN_POINT ( 'NONE',  ( 2.499999999999984457, -73.00000000000001421, -201.6999999999999886 ) ) ;
#46505 = CARTESIAN_POINT ( 'NONE',  ( 97.64999999999999147, -209.9999999999999716, 84.60249999999999204 ) ) ;
#46506 = VERTEX_POINT ( 'NONE', #26818 ) ;
#46507 = ADVANCED_FACE ( 'NONE', ( #27565 ), #44873, .T. ) ;
#46508 = ORIENTED_EDGE ( 'NONE', *, *, #70230, .T. ) ;
#46509 = ORIENTED_EDGE ( 'NONE', *, *, #51683, .F. ) ;
#46510 = ORIENTED_EDGE ( 'NONE', *, *, #13077, .F. ) ;
#46511 = CYLINDRICAL_SURFACE ( 'NONE', #9389, 32.50000000000000000 ) ;
#46512 = VECTOR ( 'NONE', #56312, 1000.000000000000000 ) ;
#46513 =( LENGTH_UNIT ( ) NAMED_UNIT ( * ) SI_UNIT ( .MILLI., .METRE. ) );
#46514 = CARTESIAN_POINT ( 'NONE',  ( -92.69370383062502583, 91.33154071421968467, 88.26697916753381890 ) ) ;
#46515 = CARTESIAN_POINT ( 'NONE',  ( 11.99999999999999822, 68.27212725128275395, -31.46837873495001503 ) ) ;
#46516 = CARTESIAN_POINT ( 'NONE',  ( 11.99999999999999822, 79.10210256391397365, -21.60688246758502729 ) ) ;
#46517 = CARTESIAN_POINT ( 'NONE',  ( 96.32499999999998863, -207.7050326799711968, 75.89770833506763381 ) ) ;
#46518 = CARTESIAN_POINT ( 'NONE',  ( 96.32499999999997442, 92.29496732002878900, 77.08833333333332405 ) ) ;
#46519 = VECTOR ( 'NONE', #50851, 1000.000000000000114 ) ;
#46520 = ORIENTED_EDGE ( 'NONE', *, *, #7831, .T. ) ;
#46521 = CARTESIAN_POINT ( 'NONE',  ( -92.34999999999999432, -209.9999999999999716, 88.49187500173430010 ) ) ;
#46522 = ORIENTED_EDGE ( 'NONE', *, *, #2535, .T. ) ;
#46523 = PLANE ( 'NONE',  #72195 ) ;
#46524 = EDGE_CURVE ( 'NONE', #6569, #40304, #42062, .T. ) ;
#46525 = ORIENTED_EDGE ( 'NONE', *, *, #14015, .F. ) ;
#46526 = CARTESIAN_POINT ( 'NONE',  ( -95.00000000000002842, 86.94004357329504273, 88.96812500173430749 ) ) ;
#46527 = CARTESIAN_POINT ( 'NONE',  ( -92.69370383062505425, 88.66845928578038638, 80.54114583420049200 ) ) ;
#46528 = CARTESIAN_POINT ( 'NONE',  ( 92.69370383062498320, 90.00000000000002842, 75.03781250086713328 ) ) ;
#46529 = EDGE_CURVE ( 'NONE', #19930, #60050, #48570, .T. ) ;
#46530 = VERTEX_POINT ( 'NONE', #55773 ) ;
#46531 = DIRECTION ( 'NONE',  ( -0.6064928550163524168, -0.7950889364178789220, 0.000000000000000000 ) ) ;
#46532 = DIRECTION ( 'NONE',  ( 0.000000000000000000, 0.000000000000000000, 1.000000000000000000 ) ) ;
#46533 = CARTESIAN_POINT ( 'NONE',  ( 10.00000000000000000, 0.000000000000000000, 0.000000000000000000 ) ) ;
#46534 = CARTESIAN_POINT ( 'NONE',  ( -92.34999999999999432, -210.0000000198591295, 85.95187500101400246 ) ) ;
#46535 = ORIENTED_EDGE ( 'NONE', *, *, #29338, .F. ) ;
#46536 = LINE ( 'NONE', #11943, #36297 ) ;
#46537 = ADVANCED_FACE ( 'NONE', ( #3555 ), #73790, .F. ) ;
#46538 = CARTESIAN_POINT ( 'NONE',  ( -92.69370383062498320, -209.9999999999999716, 76.62531250086713897 ) ) ;
#46539 = ORIENTED_EDGE ( 'NONE', *, *, #16615, .F. ) ;
#46540 = ORIENTED_EDGE ( 'NONE', *, *, #47875, .F. ) ;
#46541 = FACE_OUTER_BOUND ( 'NONE', #9235, .T. ) ;
#46542 = ORIENTED_EDGE ( 'NONE', *, *, #67399, .F. ) ;
#46543 = ADVANCED_FACE ( 'NONE', ( #9163 ), #32085, .T. ) ;
#46544 = CARTESIAN_POINT ( 'NONE',  ( 4.999999999999999112, 0.4881033300985041512, -6.000000000000000000 ) ) ;
#46545 = FACE_OUTER_BOUND ( 'NONE', #20036, .T. ) ;
#46546 = ORIENTED_EDGE ( 'NONE', *, *, #41073, .F. ) ;
#46547 = CARTESIAN_POINT ( 'NONE',  ( -93.84685191531248449, -208.0026889286704943, 87.68489583420048916 ) ) ;
#46548 = VERTEX_POINT ( 'NONE', #15170 ) ;
#46549 = DIRECTION ( 'NONE',  ( 0.000000000000000000, 0.3826834323650841752, 0.9238795325112891810 ) ) ;
#46550 = AXIS2_PLACEMENT_3D ( 'NONE', #51403, #10825, #5202 ) ;
#46551 = ADVANCED_FACE ( 'NONE', ( #3920 ), #36, .F. ) ;
#46552 = CARTESIAN_POINT ( 'NONE',  ( -3.000000000000000000, 23.50000000000000000, 1.499999999999997780 ) ) ;
#46553 = EDGE_LOOP ( 'NONE', ( #21824, #36144, #29987, #35910 ) ) ;
#46554 = COLOUR_RGB ( '', 0.31764706, 0.68627451, 0.89019608) ;
#46555 = ORIENTED_EDGE ( 'NONE', *, *, #9275, .F. ) ;
#46556 = LINE ( 'NONE', #58201, #70249 ) ;
#46557 = AXIS2_PLACEMENT_3D ( 'NONE', #14639, #67262, #61624 ) ;
#46558 = LINE ( 'NONE', #28147, #31306 ) ;
#46559 = CARTESIAN_POINT ( 'NONE',  ( 92.69370383062498320, 91.33154071421968467, 85.14489583420045449 ) ) ;
#46560 = AXIS2_PLACEMENT_3D ( 'NONE', #52666, #30096, #6447 ) ;
#46561 = CARTESIAN_POINT ( 'NONE',  ( 0.000000000000000000, 0.000000000000000000, 0.000000000000000000 ) ) ;
#46562 = CARTESIAN_POINT ( 'NONE',  ( -97.65000000000001990, 90.00000000000004263, 89.44437500173430067 ) ) ;
#46563 = CARTESIAN_POINT ( 'NONE',  ( 0.000000000000000000, 0.000000000000000000, 0.000000000000000000 ) ) ;
#46564 = DIRECTION ( 'NONE',  ( 1.000000000000000000, 0.000000000000000000, 0.000000000000000000 ) ) ;
#46565 = CARTESIAN_POINT ( 'NONE',  ( 0.000000000000000000, 0.000000000000000000, 0.000000000000000000 ) ) ;
#46566 = CARTESIAN_POINT ( 'NONE',  ( 10.00000000000000000, 58.39081064771823293, -50.95692526931266286 ) ) ;
#46567 = LINE ( 'NONE', #24011, #56700 ) ;
#46568 = DIRECTION ( 'NONE',  ( -1.000000000000000000, 0.000000000000000000, 0.000000000000000000 ) ) ;
#46569 = DIRECTION ( 'NONE',  ( 2.603472992746261562E-14, 2.546204323184492723E-14, -1.000000000000000000 ) ) ;
#46570 = CARTESIAN_POINT ( 'NONE',  ( -97.30629616937501680, 90.00000000000004263, 89.64281250086713726 ) ) ;
#46571 = DIRECTION ( 'NONE',  ( -1.000000000000000000, -0.000000000000000000, -0.000000000000000000 ) ) ;
#46572 = AXIS2_PLACEMENT_3D ( 'NONE', #10728, #73868, #57979 ) ;
#46573 = VECTOR ( 'NONE', #72005, 1000.000000000000000 ) ;
#46574 = CIRCLE ( 'NONE', #66953, 2.445500000000000007 ) ;
#46575 = CARTESIAN_POINT ( 'NONE',  ( 13.36581099891334645, -139.3288669181958710, 2.500000000000000000 ) ) ;
#46576 = ORIENTED_EDGE ( 'NONE', *, *, #45584, .T. ) ;
#46577 = CIRCLE ( 'NONE', #9381, 77.49900000000000944 ) ;
#46578 = CARTESIAN_POINT ( 'NONE',  ( 97.65000000000000568, -208.4700217866474645, 75.84479166840098685 ) ) ;
#46579 = FACE_OUTER_BOUND ( 'NONE', #8614, .T. ) ;
#46580 = CYLINDRICAL_SURFACE ( 'NONE', #5865, 37.49900000000000233 ) ;
#46581 = CARTESIAN_POINT ( 'NONE',  ( 0.000000000000000000, 0.000000000000000000, 0.000000000000000000 ) ) ;
#46582 = EDGE_CURVE ( 'NONE', #60145, #70171, #523, .T. ) ;
#46583 = FACE_OUTER_BOUND ( 'NONE', #43954, .T. ) ;
#46584 = CARTESIAN_POINT ( 'NONE',  ( 97.30629616937498838, -208.6684592857803011, 83.82197916753382572 ) ) ;
#46585 = ADVANCED_FACE ( 'NONE', ( #12492 ), #57639, .T. ) ;
#46586 = ORIENTED_EDGE ( 'NONE', *, *, #13468, .T. ) ;
#46587 = EDGE_CURVE ( 'NONE', #5835, #14313, #19188, .T. ) ;
#46588 = VERTEX_POINT ( 'NONE', #24162 ) ;
#46589 = EDGE_LOOP ( 'NONE', ( #57287, #52626, #17667, #24359 ) ) ;
#46590 = DIRECTION ( 'NONE',  ( 0.000000000000000000, 0.000000000000000000, 1.000000000000000000 ) ) ;
#46591 = EDGE_CURVE ( 'NONE', #23135, #69158, #5405, .T. ) ;
#46592 =( BOUNDED_CURVE ( )  B_SPLINE_CURVE ( 2, ( #65423, #6782, #1558, #30077, #70287, #18790, #44715, #3384, #49952 ),
 .UNSPECIFIED., .F., .F. ) 
 B_SPLINE_CURVE_WITH_KNOTS ( ( 3, 2, 2, 2, 3 ),
 ( 0.000000000000000000, 0.007055765540882354830, 0.01411153108176470966, 0.02116729662264706449, 0.02116741234826875415 ),
 .UNSPECIFIED. ) 
 CURVE ( )  GEOMETRIC_REPRESENTATION_ITEM ( )  RATIONAL_B_SPLINE_CURVE ( ( 1.000000000000000000, 0.8660254037844387076, 1.000000000000000000, 0.8660254037844387076, 1.000000000000000000, 0.8660254037844387076, 1.000000000000000000, 0.9999978026064856307, 0.9999956052850527133 ) ) 
 REPRESENTATION_ITEM ( '' )  );
#46593 = CARTESIAN_POINT ( 'NONE',  ( 95.00000000000000000, -207.3369185715606307, 74.87906250086713555 ) ) ;
#46594 = AXIS2_PLACEMENT_3D ( 'NONE', #4455, #27738, #44291 ) ;
#46595 = ORIENTED_EDGE ( 'NONE', *, *, #57077, .T. ) ;
#46596 = CARTESIAN_POINT ( 'NONE',  ( 97.30629616937498838, -211.3315407142195852, 78.63614583420049087 ) ) ;
#46597 = AXIS2_PLACEMENT_3D ( 'NONE', #40007, #5438, #28335 ) ;
#46598 = VECTOR ( 'NONE', #7817, 1000.000000000000000 ) ;
#46599 = ORIENTED_EDGE ( 'NONE', *, *, #69208, .T. ) ;
#46600 = ORIENTED_EDGE ( 'NONE', *, *, #68832, .T. ) ;
#46601 = EDGE_LOOP ( 'NONE', ( #48784, #18317, #1520, #5277 ) ) ;
#46602 = CARTESIAN_POINT ( 'NONE',  ( 0.000000000000000000, 0.000000000000000000, 125.0000000000000000 ) ) ;
#46603 = AXIS2_PLACEMENT_3D ( 'NONE', #31653, #48222, #53122 ) ;
#46604 = FACE_OUTER_BOUND ( 'NONE', #50961, .T. ) ;
#46605 = VECTOR ( 'NONE', #14390, 1000.000000000000000 ) ;
#46606 = VERTEX_POINT ( 'NONE', #62926 ) ;
#46607 = DIRECTION ( 'NONE',  ( 0.9580045777625458836, 0.2867529058022011412, 0.000000000000000000 ) ) ;
#46608 = CARTESIAN_POINT ( 'NONE',  ( 92.35000000000000853, -209.9999999999999716, 87.53937500173429953 ) ) ;
#46609 = ORIENTED_EDGE ( 'NONE', *, *, #16809, .F. ) ;
#46610 = DIRECTION ( 'NONE',  ( -0.000000000000000000, 0.000000000000000000, 1.000000000000000000 ) ) ;
#46611 = VERTEX_POINT ( 'NONE', #894 ) ;
#46612 = FACE_OUTER_BOUND ( 'NONE', #7557, .T. ) ;
#46613 = VERTEX_POINT ( 'NONE', #63280 ) ;
#46614 = CARTESIAN_POINT ( 'NONE',  ( 93.67499999999999716, 87.70503267997126784, 86.37520833506764006 ) ) ;
#46615 = ORIENTED_EDGE ( 'NONE', *, *, #43208, .F. ) ;
#46616 = VERTEX_POINT ( 'NONE', #6140 ) ;
#46617 = DIRECTION ( 'NONE',  ( 0.000000000000000000, 0.2079116908177532363, -0.9781476007338069101 ) ) ;
#46618 = EDGE_CURVE ( 'NONE', #41791, #28195, #26431, .T. ) ;
#46619 = EDGE_CURVE ( 'NONE', #28753, #59706, #1273, .T. ) ;
#46620 = DIRECTION ( 'NONE',  ( 0.000000000000000000, 0.000000000000000000, 1.000000000000000000 ) ) ;
#46621 = ORIENTED_EDGE ( 'NONE', *, *, #23524, .F. ) ;
#46622 = AXIS2_PLACEMENT_3D ( 'NONE', #33090, #21433, #54554 ) ;
#46623 = ORIENTED_EDGE ( 'NONE', *, *, #8009, .F. ) ;
#46624 = VECTOR ( 'NONE', #8894, 1000.000000000000000 ) ;
#46625 = EDGE_LOOP ( 'NONE', ( #3143, #68061, #69690, #229 ) ) ;
#46626 = CARTESIAN_POINT ( 'NONE',  ( 94.99999999999998579, 93.05995642670504253, 79.76062500173429726 ) ) ;
#46627 = FACE_OUTER_BOUND ( 'NONE', #34219, .T. ) ;
#46628 = VECTOR ( 'NONE', #4804, 1000.000000000000000 ) ;
#46629 = CARTESIAN_POINT ( 'NONE',  ( -95.00000000000002842, 93.05995642670501411, 88.57124999999999204 ) ) ;
#46630 = ORIENTED_EDGE ( 'NONE', *, *, #41326, .T. ) ;
#46631 = EDGE_CURVE ( 'NONE', #48807, #31231, #72046, .T. ) ;
#46632 = CARTESIAN_POINT ( 'NONE',  ( 93.84685191531248449, 88.00268892867053694, 75.14364583420046984 ) ) ;
#46633 = VECTOR ( 'NONE', #37977, 1000.000000000000000 ) ;
#46634 = EDGE_LOOP ( 'NONE', ( #31325, #16748, #40121, #3572 ) ) ;
#46635 = CARTESIAN_POINT ( 'NONE',  ( -22.17439115976385366, -112.2188447712574799, -2.500000000000000000 ) ) ;
#46636 = CARTESIAN_POINT ( 'NONE',  ( -93.84685191531248449, -208.0026889286704943, 81.17614583420048291 ) ) ;
#46637 = ORIENTED_EDGE ( 'NONE', *, *, #72967, .F. ) ;
#46638 = CARTESIAN_POINT ( 'NONE',  ( 11.99999999999999822, 60.67117009219136037, 55.16347631943064300 ) ) ;
#46639 = CARTESIAN_POINT ( 'NONE',  ( 92.59666252161194677, -210.8453944377487232, 74.93511027845777051 ) ) ;
#46640 = CARTESIAN_POINT ( 'NONE',  ( 0.000000000000000000, -60.67117009219098378, -55.16347631943106933 ) ) ;
#46641 = CARTESIAN_POINT ( 'NONE',  ( -96.15314808468745866, -211.9973110713294489, 77.04864583420047097 ) ) ;
#46642 = CARTESIAN_POINT ( 'NONE',  ( 10.00000000000000000, 33.80338159004307386, -16.23288003029461279 ) ) ;
#46643 = CARTESIAN_POINT ( 'NONE',  ( 92.34999999999999432, 90.00000000000002842, 83.01499999999998636 ) ) ;
#46644 = FACE_OUTER_BOUND ( 'NONE', #67160, .T. ) ;
#46645 = LINE ( 'NONE', #63950, #57618 ) ;
#46646 = DIRECTION ( 'NONE',  ( -0.6064928550163533050, -0.7950889364178781449, 0.000000000000000000 ) ) ;
#46647 = DIRECTION ( 'NONE',  ( -1.000000000000000000, 0.000000000000000000, 0.000000000000000000 ) ) ;
#46648 = CARTESIAN_POINT ( 'NONE',  ( -92.69370383062504004, 90.00000000000004263, 77.26031250086714408 ) ) ;
#46649 = LINE ( 'NONE', #68854, #31028 ) ;
#46650 = CARTESIAN_POINT ( 'NONE',  ( -10.90076147243505211, 0.000000000000000000, 0.000000000000000000 ) ) ;
#46651 = VECTOR ( 'NONE', #48725, 1000.000000000000000 ) ;
#46652 = ORIENTED_EDGE ( 'NONE', *, *, #63511, .F. ) ;
#46653 = DIRECTION ( 'NONE',  ( 0.000000000000000000, 0.000000000000000000, 1.000000000000000000 ) ) ;
#46654 = VECTOR ( 'NONE', #47851, 1000.000000000000000 ) ;
#46655 = AXIS2_PLACEMENT_3D ( 'NONE', #840, #40651, #23723 ) ;
#46656 = DIRECTION ( 'NONE',  ( -1.000000000000000000, -0.000000000000000000, -0.000000000000000000 ) ) ;
#46657 = CARTESIAN_POINT ( 'NONE',  ( -24.50849501662245800, -109.8101191361138831, 5.500000000000000000 ) ) ;
#46659 = CIRCLE ( 'NONE', #55078, 31.99999999999998934 ) ;
#46658 = CARTESIAN_POINT ( 'NONE',  ( 0.000000000000000000, 10.30890764327501863, -81.34940948281325745 ) ) ;
#46660 = CARTESIAN_POINT ( 'NONE',  ( 6.250000000000005329, 0.000000000000000000, 0.000000000000000000 ) ) ;
#46661 = CARTESIAN_POINT ( 'NONE',  ( 1.243286885786405054E-17, -120.0000000000000000, 127.5000000000000000 ) ) ;
#46662 = CARTESIAN_POINT ( 'NONE',  ( -93.84685191531248449, -208.0026889286704943, 76.88989583420048746 ) ) ;
#46663 = CIRCLE ( 'NONE', #57506, 37.49900000000000233 ) ;
#46664 = DIRECTION ( 'NONE',  ( -1.000000000000000000, 0.000000000000000000, -0.000000000000000000 ) ) ;
#46665 = ORIENTED_EDGE ( 'NONE', *, *, #59076, .F. ) ;
#46666 = CYLINDRICAL_SURFACE ( 'NONE', #14254, 2.649999999999985700 ) ;
#46667 = CARTESIAN_POINT ( 'NONE',  ( 2.500000000000029754, 73.00000000000001421, -201.6999999999999886 ) ) ;
#46668 = DIRECTION ( 'NONE',  ( -0.000000000000000000, -0.000000000000000000, 1.000000000000000000 ) ) ;
#46669 = DIRECTION ( 'NONE',  ( 0.000000000000000000, 1.000000000000000000, -9.787530781167598712E-16 ) ) ;
#46670 = AXIS2_PLACEMENT_3D ( 'NONE', #16338, #52024, #34365 ) ;
#46671 = EDGE_CURVE ( 'NONE', #70724, #52790, #25210, .T. ) ;
#46672 = AXIS2_PLACEMENT_3D ( 'NONE', #37921, #32632, #3727 ) ;
#46673 = EDGE_CURVE ( 'NONE', #11821, #32195, #56261, .T. ) ;
#46675 = CARTESIAN_POINT ( 'NONE',  ( 50.00005079999999680, 0.000000000000000000, 0.000000000000000000 ) ) ;
#46674 = CIRCLE ( 'NONE', #23873, 31.99999999999999289 ) ;
#46676 = ORIENTED_EDGE ( 'NONE', *, *, #18535, .F. ) ;
#46677 = CIRCLE ( 'NONE', #57528, 13.71319123027096865 ) ;
#46678 = EDGE_CURVE ( 'NONE', #30123, #70981, #46349, .T. ) ;
#46679 = CARTESIAN_POINT ( 'NONE',  ( -42.50000000000000000, 0.000000000000000000, -15.77977592589476608 ) ) ;
#46680 = LINE ( 'NONE', #12820, #40354 ) ;
#46681 = ORIENTED_EDGE ( 'NONE', *, *, #35555, .T. ) ;
#46682 = AXIS2_PLACEMENT_3D ( 'NONE', #3616, #3976, #31771 ) ;
#46683 = EDGE_CURVE ( 'NONE', #66942, #50206, #28299, .T. ) ;
#46684 = CARTESIAN_POINT ( 'NONE',  ( 95.00000000000000000, -212.6630814284392557, 83.45156250086714067 ) ) ;
#46685 = CYLINDRICAL_SURFACE ( 'NONE', #15463, 12.50000000000022560 ) ;
#46686 = ORIENTED_EDGE ( 'NONE', *, *, #64256, .T. ) ;
#46687 = DIRECTION ( 'NONE',  ( -1.000000000000000000, 0.000000000000000000, 0.000000000000000000 ) ) ;
#46688 = ORIENTED_EDGE ( 'NONE', *, *, #52819, .F. ) ;
#46689 = EDGE_CURVE ( 'NONE', #64668, #65945, #6500, .T. ) ;
#46690 = CARTESIAN_POINT ( 'NONE',  ( 92.35000000003290666, -209.9999916046337205, 84.99910573348564924 ) ) ;
#46691 = ORIENTED_EDGE ( 'NONE', *, *, #70318, .F. ) ;
#46692 = CARTESIAN_POINT ( 'NONE',  ( -96.15314808468751551, 88.00268892867056536, 79.11239583420048405 ) ) ;
#46693 = ORIENTED_EDGE ( 'NONE', *, *, #49325, .F. ) ;
#46694 = VERTEX_POINT ( 'NONE', #46721 ) ;
#46695 = ORIENTED_EDGE ( 'NONE', *, *, #11068, .F. ) ;
#46696 = DIRECTION ( 'NONE',  ( 0.000000000000000000, 0.000000000000000000, 1.000000000000000000 ) ) ;
#46697 = DIRECTION ( 'NONE',  ( -1.000000000000000000, -0.000000000000000000, 0.000000000000000000 ) ) ;
#46698 = EDGE_CURVE ( 'NONE', #26852, #62900, #45677, .T. ) ;
#46699 = VECTOR ( 'NONE', #21838, 1000.000000000000000 ) ;
#46700 = EDGE_CURVE ( 'NONE', #13957, #15423, #22682, .T. ) ;
#46701 = ORIENTED_EDGE ( 'NONE', *, *, #54809, .F. ) ;
#46702 = CARTESIAN_POINT ( 'NONE',  ( -1.384174031800281979, -120.5779811845464735, 2.500000000000000000 ) ) ;
#46703 = ORIENTED_EDGE ( 'NONE', *, *, #18464, .F. ) ;
#46704 = CARTESIAN_POINT ( 'NONE',  ( 94.20702885560666573, 87.49569407151196287, 74.98272308147875265 ) ) ;
#46705 = VECTOR ( 'NONE', #73050, 1000.000000000000000 ) ;
#46706 = VECTOR ( 'NONE', #40679, 1000.000000000000000 ) ;
#46707 = ORIENTED_EDGE ( 'NONE', *, *, #9173, .F. ) ;
#46708 = VECTOR ( 'NONE', #10132, 1000.000000000000000 ) ;
#46709 = ORIENTED_EDGE ( 'NONE', *, *, #17344, .T. ) ;
#46710 = VERTEX_POINT ( 'NONE', #39971 ) ;
#46711 = CARTESIAN_POINT ( 'NONE',  ( 92.69370383062501162, -209.9999999999999716, 81.38781250086714181 ) ) ;
#46712 = ADVANCED_FACE ( 'NONE', ( #68550 ), #11383, .T. ) ;
#46713 = EDGE_CURVE ( 'NONE', #20594, #13869, #4837, .T. ) ;
#46714 = APPLICATION_PROTOCOL_DEFINITION ( 'draft international standard', 'automotive_design', 1998, #41173 ) ;
#46715 = DIRECTION ( 'NONE',  ( -1.000000000000000000, 0.000000000000000000, 0.000000000000000000 ) ) ;
#46716 = AXIS2_PLACEMENT_3D ( 'NONE', #32298, #66896, #4891 ) ;
#46717 = CARTESIAN_POINT ( 'NONE',  ( -95.00000000000002842, 86.94004357329504273, 84.44374999999999432 ) ) ;
#46718 = DIRECTION ( 'NONE',  ( 0.000000000000000000, -0.9510565162951500895, -0.3090169943749583314 ) ) ;
#46719 = AXIS2_PLACEMENT_3D ( 'NONE', #31124, #60463, #64994 ) ;
#46720 = DIRECTION ( 'NONE',  ( -1.000000000000000000, 0.000000000000000000, 0.000000000000000000 ) ) ;
#46721 = CARTESIAN_POINT ( 'NONE',  ( 10.00000000000000000, -76.69515212746036070, 29.01471420065537643 ) ) ;
#46722 = CARTESIAN_POINT ( 'NONE',  ( -96.32500000000001705, 87.70503267997129626, 82.48583333333333201 ) ) ;
#46723 = CARTESIAN_POINT ( 'NONE',  ( -92.69370383062498320, -208.6684592857803011, 85.56822916753380071 ) ) ;
#46724 = CARTESIAN_POINT ( 'NONE',  ( -96.15314808468752972, 91.99731107132950569, 80.80572916753382628 ) ) ;
#46725 = ORIENTED_EDGE ( 'NONE', *, *, #4780, .F. ) ;
#46726 = CARTESIAN_POINT ( 'NONE',  ( 92.69370383062498320, 88.66845928578037217, 85.88572916753382458 ) ) ;
#46727 = ORIENTED_EDGE ( 'NONE', *, *, #14693, .T. ) ;
#46728 = CYLINDRICAL_SURFACE ( 'NONE', #41933, 31.99999999999999289 ) ;
#46729 = DIRECTION ( 'NONE',  ( -0.4279312458753000703, -0.9038112904824842087, 0.000000000000000000 ) ) ;
#46730 = DIRECTION ( 'NONE',  ( -1.000000000000000000, -0.000000000000000000, -0.000000000000000000 ) ) ;
#46731 = CARTESIAN_POINT ( 'NONE',  ( -95.00000000000002842, 90.00000000000004263, 90.00000000000000000 ) ) ;
#46732 = AXIS2_PLACEMENT_3D ( 'NONE', #73544, #18258, #69037 ) ;
#46733 = CARTESIAN_POINT ( 'NONE',  ( -92.69370383062498320, -209.9999999999999716, 88.05531250086713158 ) ) ;
#46734 = CARTESIAN_POINT ( 'NONE',  ( -7.500000000000016875, -80.00000000000001421, -189.9999999999999147 ) ) ;
#46735 = CIRCLE ( 'NONE', #14301, 42.00000000000000000 ) ;
#46736 = LINE ( 'NONE', #70014, #39815 ) ;
#46737 = DIRECTION ( 'NONE',  ( 1.000000000000000000, 0.000000000000000000, 0.000000000000000000 ) ) ;
#46738 = CARTESIAN_POINT ( 'NONE',  ( 94.99999999999998579, 93.05995642670504253, 80.31624999999999659 ) ) ;
#46739 = ORIENTED_EDGE ( 'NONE', *, *, #32433, .T. ) ;
#46740 = AXIS2_PLACEMENT_3D ( 'NONE', #43276, #31099, #7444 ) ;
#46741 = VECTOR ( 'NONE', #48020, 1000.000000000000000 ) ;
#46742 = ORIENTED_EDGE ( 'NONE', *, *, #15275, .F. ) ;
#46743 = AXIS2_PLACEMENT_3D ( 'NONE', #67962, #32620, #45037 ) ;
#46744 = VECTOR ( 'NONE', #36484, 1000.000000000000114 ) ;
#46745 = CARTESIAN_POINT ( 'NONE',  ( -92.35000000000005116, 88.47002178664754979, 76.92958333333332632 ) ) ;
#46746 = LINE ( 'NONE', #17786, #12689 ) ;
#46747 = CARTESIAN_POINT ( 'NONE',  ( -97.30629616937501680, 91.33154071421968467, 87.04989583420048405 ) ) ;
#46748 = CARTESIAN_POINT ( 'NONE',  ( 95.00000000000000000, -206.9400435732949575, 80.95125000000000171 ) ) ;
#46749 = CARTESIAN_POINT ( 'NONE',  ( -97.65000000000003411, 90.00000000000004263, 75.00000000000000000 ) ) ;
#46750 = DIRECTION ( 'NONE',  ( 0.000000000000000000, 0.000000000000000000, 1.000000000000000000 ) ) ;
#46751 = DIRECTION ( 'NONE',  ( -1.000000000000000000, 0.000000000000000000, -0.000000000000000000 ) ) ;
#46752 = VECTOR ( 'NONE', #32973, 1000.000000000000000 ) ;
#46753 = ORIENTED_EDGE ( 'NONE', *, *, #27311, .F. ) ;
#46754 = CARTESIAN_POINT ( 'NONE',  ( -95.00000000000002842, 87.33691857156074434, 79.00656250086713328 ) ) ;
#46755 = CARTESIAN_POINT ( 'NONE',  ( 0.000000000000000000, -120.0000000000000000, -5.500000000000000000 ) ) ;
#46756 = CARTESIAN_POINT ( 'NONE',  ( 4.999999999999999112, 16.65560815589411092, 38.55633173627015253 ) ) ;
#46757 = DIRECTION ( 'NONE',  ( -1.000000000000000000, -0.000000000000000000, 0.000000000000000000 ) ) ;
#46758 = CARTESIAN_POINT ( 'NONE',  ( 12.49999999999999645, 1.530808498934191127E-15, 20.00000000000000000 ) ) ;
#46759 = CARTESIAN_POINT ( 'NONE',  ( 10.00000000000000000, -26.08949754953044220, 27.05870788708222818 ) ) ;
#46760 = CARTESIAN_POINT ( 'NONE',  ( -97.30629616937497417, -211.3315407142195852, 84.77447916753381207 ) ) ;
#46761 =( LENGTH_UNIT ( ) NAMED_UNIT ( * ) SI_UNIT ( .MILLI., .METRE. ) );
#46762 = EDGE_CURVE ( 'NONE', #26154, #20073, #3099, .T. ) ;
#46763 = DIRECTION ( 'NONE',  ( -1.000000000000000000, -0.000000000000000000, 0.000000000000000000 ) ) ;
#46764 = EDGE_CURVE ( 'NONE', #54641, #24857, #14409, .T. ) ;
#46765 = CIRCLE ( 'NONE', #34736, 77.49899999999999523 ) ;
#46766 = CARTESIAN_POINT ( 'NONE',  ( 93.84685191531248449, 88.00268892867053694, 77.20739583420048291 ) ) ;
#46767 = VECTOR ( 'NONE', #62528, 1000.000000000000000 ) ;
#46768 = ADVANCED_FACE ( 'NONE', ( #18500 ), #64383, .F. ) ;
#46769 = CARTESIAN_POINT ( 'NONE',  ( -94.99999999999997158, -212.6630814284392557, 75.99031250086716227 ) ) ;
#46770 = CARTESIAN_POINT ( 'NONE',  ( 10.00000000000000000, 15.48615015657638239, -39.04073710021328480 ) ) ;
#46771 = ORIENTED_EDGE ( 'NONE', *, *, #5513, .T. ) ;
#46772 = DIRECTION ( 'NONE',  ( 0.000000000000000000, 0.000000000000000000, 1.000000000000000000 ) ) ;
#46773 = LINE ( 'NONE', #64431, #10659 ) ;
#46774 = VECTOR ( 'NONE', #2753, 1000.000000000000000 ) ;
#46775 = CYLINDRICAL_SURFACE ( 'NONE', #36617, 2.650000000000540812 ) ;
#46776 = EDGE_CURVE ( 'NONE', #64038, #22283, #70738, .T. ) ;
#46777 = CARTESIAN_POINT ( 'NONE',  ( -93.33864827737279768, 88.39919842643631398, 74.79754476654878204 ) ) ;
#46778 = CARTESIAN_POINT ( 'NONE',  ( 97.30629616937498838, -208.6684592857803011, 77.94822916753381037 ) ) ;
#46779 = ORIENTED_EDGE ( 'NONE', *, *, #54405, .F. ) ;
#46780 = CARTESIAN_POINT ( 'NONE',  ( 4.999999999999999112, -10.41901085202107247, 40.68715046381925049 ) ) ;
#46781 = ORIENTED_EDGE ( 'NONE', *, *, #60968, .T. ) ;
#46782 = EDGE_CURVE ( 'NONE', #27645, #49121, #9697, .T. ) ;
#46783 = DIRECTION ( 'NONE',  ( 1.000000000000000000, -0.000000000000000000, 0.000000000000000000 ) ) ;
#46784 = ORIENTED_EDGE ( 'NONE', *, *, #52948, .F. ) ;
#46785 = AXIS2_PLACEMENT_3D ( 'NONE', #8992, #61249, #60872 ) ;
#46786 = CARTESIAN_POINT ( 'NONE',  ( 10.00000000000000000, -54.21277698773636899, -55.38113227695839669 ) ) ;
#46787 = AXIS2_PLACEMENT_3D ( 'NONE', #34034, #56618, #28016 ) ;
#46788 = AXIS2_PLACEMENT_3D ( 'NONE', #34420, #21662, #28041 ) ;
#46789 = ORIENTED_EDGE ( 'NONE', *, *, #31331, .F. ) ;
#46790 = EDGE_LOOP ( 'NONE', ( #67394, #35856, #28209, #27238 ) ) ;
#46791 = VECTOR ( 'NONE', #56881, 1000.000000000000000 ) ;
#46792 = ORIENTED_EDGE ( 'NONE', *, *, #49246, .F. ) ;
#46793 = CIRCLE ( 'NONE', #26388, 77.49900000000000944 ) ;
#46794 = DIRECTION ( 'NONE',  ( 0.000000000000000000, 0.000000000000000000, -1.000000000000000000 ) ) ;
#46795 = EDGE_CURVE ( 'NONE', #39724, #47808, #2377, .T. ) ;
#46796 = ADVANCED_FACE ( 'NONE', ( #7602 ), #25268, .T. ) ;
#46797 = VERTEX_POINT ( 'NONE', #64752 ) ;
#46798 = ORIENTED_EDGE ( 'NONE', *, *, #52362, .F. ) ;
#46799 = CARTESIAN_POINT ( 'NONE',  ( 92.69370383062498320, 88.66845928578037217, 82.86947916753382515 ) ) ;
#46800 = CARTESIAN_POINT ( 'NONE',  ( -92.35000000000553655, 89.99999459739531460, 81.50687481489494246 ) ) ;
#46801 = CARTESIAN_POINT ( 'NONE',  ( 10.00000000000000000, 0.000000000000000000, 0.000000000000000000 ) ) ;
#46802 = VERTEX_POINT ( 'NONE', #42556 ) ;
#46803 = VERTEX_POINT ( 'NONE', #37296 ) ;
#46804 = ORIENTED_EDGE ( 'NONE', *, *, #55860, .T. ) ;
#46805 = VERTEX_POINT ( 'NONE', #58740 ) ;
#46806 = DIRECTION ( 'NONE',  ( 0.000000000000000000, 0.3090169943749483394, -0.9510565162951534202 ) ) ;
#46807 = ORIENTED_EDGE ( 'NONE', *, *, #73894, .F. ) ;
#46808 = DIRECTION ( 'NONE',  ( 0.9873505073845697533, 0.1585527532634883052, 0.000000000000000000 ) ) ;
#46809 = DIRECTION ( 'NONE',  ( -1.000000000000000000, -0.000000000000000000, 0.000000000000000000 ) ) ;
#46810 = DIRECTION ( 'NONE',  ( -1.000000000000000000, 0.000000000000000000, 0.000000000000000000 ) ) ;
#46811 = DIRECTION ( 'NONE',  ( -1.000000000000000000, -0.000000000000000000, 0.000000000000000000 ) ) ;
#46812 = DIRECTION ( 'NONE',  ( -1.000000000000000000, 0.000000000000000000, 0.000000000000000000 ) ) ;
#46813 = DIRECTION ( 'NONE',  ( 0.7071067811865485719, 8.659560562354946417E-17, -0.7071067811865465735 ) ) ;
#46814 = CARTESIAN_POINT ( 'NONE',  ( 10.00000000000000000, 37.58145647212453611, 0.6853352020791767529 ) ) ;
#46815 = CARTESIAN_POINT ( 'NONE',  ( -92.34999999999999432, -209.9999999999999716, 77.69687500173431260 ) ) ;
#46816 = ORIENTED_EDGE ( 'NONE', *, *, #15778, .T. ) ;
#46817 = DIRECTION ( 'NONE',  ( -0.000000000000000000, 0.000000000000000000, -1.000000000000000000 ) ) ;
#46818 = ORIENTED_EDGE ( 'NONE', *, *, #62993, .T. ) ;
#46820 = CARTESIAN_POINT ( 'NONE',  ( -97.65000000000001990, 91.52997821335253548, 77.32645833506762756 ) ) ;
#46819 = CARTESIAN_POINT ( 'NONE',  ( 92.34999999999999432, 90.00000000000002842, 79.28437500173430408 ) ) ;
#46821 =( BOUNDED_CURVE ( )  B_SPLINE_CURVE ( 2, ( #31622, #30511, #30148, #24513, #36525, #53456, #36896 ),
 .UNSPECIFIED., .F., .F. ) 
 B_SPLINE_CURVE_WITH_KNOTS ( ( 3, 2, 2, 3 ),
 ( 0.2328402629031412763, 0.2398960283911786839, 0.2469517939320956812, 0.2540073681295598185 ),
 .UNSPECIFIED. ) 
 CURVE ( )  GEOMETRIC_REPRESENTATION_ITEM ( )  RATIONAL_B_SPLINE_CURVE ( ( 1.000000000000000000, 0.8660254037844387076, 1.000000000000000000, 0.8660254037844387076, 1.000000000000000000, 0.8660290370063311594, 0.9999927337532719118 ) ) 
 REPRESENTATION_ITEM ( '' )  );
#46822 = VECTOR ( 'NONE', #40628, 1000.000000000000000 ) ;
#46823 = VERTEX_POINT ( 'NONE', #8711 ) ;
#46824 = CARTESIAN_POINT ( 'NONE',  ( 97.30629616937498838, 88.66845928578037217, 79.90614583420048689 ) ) ;
#46825 = CARTESIAN_POINT ( 'NONE',  ( 10.00000000000000000, 27.74655509720669144, 77.16300072079670258 ) ) ;
#46826 = CARTESIAN_POINT ( 'NONE',  ( 92.35000000003357457, 89.99999234487445676, 78.01464417100922333 ) ) ;
#46827 = AXIS2_PLACEMENT_3D ( 'NONE', #21134, #56105, #10986 ) ;
#46828 = CARTESIAN_POINT ( 'NONE',  ( 96.32499999999998863, -212.2949673200287179, 79.49604166840096298 ) ) ;
#46829 = CARTESIAN_POINT ( 'NONE',  ( 0.000000000000000000, -0.8828120875898013420, -37.48860685352291711 ) ) ;
#46830 = CIRCLE ( 'NONE', #52835, 16.00000000000000000 ) ;
#46831 = ORIENTED_EDGE ( 'NONE', *, *, #17644, .F. ) ;
#46832 = CARTESIAN_POINT ( 'NONE',  ( 10.00000000000000000, -30.80686688397025108, 21.53537804866070715 ) ) ;
#46833 = CARTESIAN_POINT ( 'NONE',  ( 0.8179331680532997417, 5.301268757141563981, -5.826062401966623838 ) ) ;
#46834 = VERTEX_POINT ( 'NONE', #31629 ) ;
#46835 = VERTEX_POINT ( 'NONE', #54573 ) ;
#46836 = VECTOR ( 'NONE', #10093, 1000.000000000000000 ) ;
#46837 = ADVANCED_FACE ( 'NONE', ( #13237 ), #7236, .T. ) ;
#46838 = CARTESIAN_POINT ( 'NONE',  ( -0.7178748134487012988, -5.359037475107207626, -1.327869168827489732 ) ) ;
#46839 = CARTESIAN_POINT ( 'NONE',  ( 0.000000000000000000, -67.80270845531921964, 46.11716303203162681 ) ) ;
#46840 = CARTESIAN_POINT ( 'NONE',  ( -97.30629616937495996, -209.9999999999999716, 77.10156250086714635 ) ) ;
#46841 = ORIENTED_EDGE ( 'NONE', *, *, #7067, .T. ) ;
#46842 = CARTESIAN_POINT ( 'NONE',  ( 10.00000000000000000, -37.22597642581153821, -5.202137450156795850 ) ) ;
#46843 = VECTOR ( 'NONE', #6540, 1000.000000000000000 ) ;
#46844 = VECTOR ( 'NONE', #24975, 1000.000000000000227 ) ;
#46845 = VECTOR ( 'NONE', #52365, 1000.000000000000000 ) ;
#46846 = CARTESIAN_POINT ( 'NONE',  ( 0.000000000000000000, 18.89407956138362010, -75.16055320797013906 ) ) ;
#46847 = CARTESIAN_POINT ( 'NONE',  ( 92.35004149090329406, 88.46999783186332422, 85.68729332542760346 ) ) ;
#46848 = CARTESIAN_POINT ( 'NONE',  ( 0.000000000000000000, -19.89357724624986901, -12.59942793731086041 ) ) ;
#46849 = CARTESIAN_POINT ( 'NONE',  ( 11.99999999999999822, 0.000000000000000000, 0.000000000000000000 ) ) ;
#46850 = CARTESIAN_POINT ( 'NONE',  ( 0.000000000000000000, 74.65491531819118620, -8.830959090342659579 ) ) ;
#46851 = EDGE_CURVE ( 'NONE', #67331, #64618, #3703, .T. ) ;
#46852 = CARTESIAN_POINT ( 'NONE',  ( 11.99999999999999822, -2.543863470247810010, -81.96053171279903893 ) ) ;
#46853 = CIRCLE ( 'NONE', #48024, 31.99999999999998579 ) ;
#46854 = CARTESIAN_POINT ( 'NONE',  ( 96.32499999999997442, 92.29496732002878900, 86.05770833506763040 ) ) ;
#46855 = AXIS2_PLACEMENT_3D ( 'NONE', #20418, #63425, #46487 ) ;
#46856 = DIRECTION ( 'NONE',  ( -1.000000000000000000, -0.000000000000000000, -0.000000000000000000 ) ) ;
#46857 = EDGE_CURVE ( 'NONE', #31085, #34215, #28851, .T. ) ;
#46858 = DIRECTION ( 'NONE',  ( 0.000000000000000000, 0.4067366430758009854, -0.9135454576426004225 ) ) ;
#46859 = CARTESIAN_POINT ( 'NONE',  ( 96.15314808468748708, 91.99731107132950569, 87.04989583420048405 ) ) ;
#46860 = EDGE_CURVE ( 'NONE', #58339, #22472, #59113, .T. ) ;
#46861 = CARTESIAN_POINT ( 'NONE',  ( -97.30629616937497417, -208.6684592857803295, 85.93864583420051417 ) ) ;
#46862 = DIRECTION ( 'NONE',  ( -0.000000000000000000, -0.000000000000000000, 1.000000000000000000 ) ) ;
#46863 = ORIENTED_EDGE ( 'NONE', *, *, #3231, .T. ) ;
#46864 = CARTESIAN_POINT ( 'NONE',  ( -95.00000000000002842, 93.05995642670504253, 81.58624999999999261 ) ) ;
#46865 = CARTESIAN_POINT ( 'NONE',  ( -96.32499999999996021, -212.2949673200287179, 81.85083333333332689 ) ) ;
#46866 = CARTESIAN_POINT ( 'NONE',  ( -95.00000000000002842, 87.33691857156074434, 76.46656250086712703 ) ) ;
#46867 = CARTESIAN_POINT ( 'NONE',  ( 97.30629616937498838, -211.3315407142195852, 86.09739583420048348 ) ) ;
#46868 = EDGE_LOOP ( 'NONE', ( #55336, #13870 ) ) ;
#46869 = CARTESIAN_POINT ( 'NONE',  ( 97.64999999954044085, 90.00004935162768049, 87.22187670868791542 ) ) ;
#46870 = EDGE_CURVE ( 'NONE', #20705, #51673, #16899, .T. ) ;
#46871 = ORIENTED_EDGE ( 'NONE', *, *, #651, .T. ) ;
#46872 = VECTOR ( 'NONE', #60807, 1000.000000000000000 ) ;
#46874 = CIRCLE ( 'NONE', #48051, 31.99999999999998224 ) ;
#46873 = DIRECTION ( 'NONE',  ( -1.000000000000000000, 0.000000000000000000, -0.000000000000000000 ) ) ;
#46875 = CARTESIAN_POINT ( 'NONE',  ( -7.670864526094549163, -97.73662565058241114, 5.500000000000000000 ) ) ;
#46876 = ORIENTED_EDGE ( 'NONE', *, *, #61730, .F. ) ;
#46877 = EDGE_LOOP ( 'NONE', ( #71530, #39430, #38934, #18249 ) ) ;
#46878 = CARTESIAN_POINT ( 'NONE',  ( 92.69370383062501162, -208.6684592857803295, 80.85864583420048746 ) ) ;
#46879 = EDGE_CURVE ( 'NONE', #68468, #34202, #13604, .T. ) ;
#46880 = DIRECTION ( 'NONE',  ( 0.000000000000000000, -0.9510565162951500895, -0.3090169943749582204 ) ) ;
#46881 = ADVANCED_FACE ( 'NONE', ( #7965 ), #19609, .F. ) ;
#46882 = DIRECTION ( 'NONE',  ( 1.000000000000000000, 0.000000000000000000, 0.000000000000000000 ) ) ;
#46883 = CARTESIAN_POINT ( 'NONE',  ( 2.874421927457452952, -143.3717286177755739, 5.500000000000000000 ) ) ;
#46884 = CARTESIAN_POINT ( 'NONE',  ( 10.00000000000000000, 0.000000000000000000, 0.000000000000000000 ) ) ;
#46885 = EDGE_CURVE ( 'NONE', #32222, #20050, #34865, .T. ) ;
#46886 = CYLINDRICAL_SURFACE ( 'NONE', #29742, 16.00000000000000000 ) ;
#46887 = CARTESIAN_POINT ( 'NONE',  ( 97.64999999999997726, -208.4700217866474645, 85.92541666666664923 ) ) ;
#46888 = AXIS2_PLACEMENT_3D ( 'NONE', #60254, #23523, #24907 ) ;
#46889 = EDGE_LOOP ( 'NONE', ( #51027, #23317, #10252, #6519 ) ) ;
#46890 = VERTEX_POINT ( 'NONE', #72944 ) ;
#46891 = ORIENTED_EDGE ( 'NONE', *, *, #43251, .T. ) ;
#46892 = ORIENTED_EDGE ( 'NONE', *, *, #23330, .F. ) ;
#46893 = CARTESIAN_POINT ( 'NONE',  ( 26.00000000000000355, 2.994873747314852478E-16, -2.445500000000000007 ) ) ;
#46894 = AXIS2_PLACEMENT_3D ( 'NONE', #45534, #63560, #40997 ) ;
#46895 = SURFACE_STYLE_FILL_AREA ( #23959 ) ;
#46896 = CARTESIAN_POINT ( 'NONE',  ( -96.15314808468751551, 88.00268892867056536, 87.36739583420049371 ) ) ;
#46897 = DIRECTION ( 'NONE',  ( -1.000000000000000000, -0.000000000000000000, -0.000000000000000000 ) ) ;
#46898 = AXIS2_PLACEMENT_3D ( 'NONE', #52616, #34218, #22958 ) ;
#46899 = CARTESIAN_POINT ( 'NONE',  ( 96.32499999999998863, -207.7050326799711968, 78.43770833506764006 ) ) ;
#46900 = CARTESIAN_POINT ( 'NONE',  ( 96.15314808468750130, -211.9973110713294489, 87.94947916753380923 ) ) ;
#46901 = CARTESIAN_POINT ( 'NONE',  ( 92.34999999999999432, 90.00000000000002842, 78.57000000000000739 ) ) ;
#46902 = ORIENTED_EDGE ( 'NONE', *, *, #70581, .T. ) ;
#46903 = DIRECTION ( 'NONE',  ( -1.000000000000000000, 0.000000000000000000, 0.000000000000000000 ) ) ;
#46904 = ORIENTED_EDGE ( 'NONE', *, *, #31834, .F. ) ;
#46905 = CARTESIAN_POINT ( 'NONE',  ( 0.000000000000000000, 41.91543099594818500, -2.663952781846294915 ) ) ;
#46906 = ORIENTED_EDGE ( 'NONE', *, *, #20017, .F. ) ;
#46907 = CARTESIAN_POINT ( 'NONE',  ( -92.35000000000005116, 88.47002178664754979, 89.07395833506762983 ) ) ;
#46908 = CARTESIAN_POINT ( 'NONE',  ( 94.99999999999998579, 87.33691857156068750, 75.83156250086715033 ) ) ;
#46909 = VERTEX_POINT ( 'NONE', #67707 ) ;
#46910 = DIRECTION ( 'NONE',  ( -1.000000000000000000, 0.000000000000000000, 0.000000000000000000 ) ) ;
#46911 = DIRECTION ( 'NONE',  ( -1.000000000000000000, -0.000000000000000000, -0.000000000000000000 ) ) ;
#46912 = CARTESIAN_POINT ( 'NONE',  ( 92.34999999999999432, 90.00000000000002842, 84.28499999999999659 ) ) ;
#46913 = PLANE ( 'NONE',  #13274 ) ;
#46914 = VERTEX_POINT ( 'NONE', #33473 ) ;
#46915 = FACE_OUTER_BOUND ( 'NONE', #53735, .T. ) ;
#46916 = CARTESIAN_POINT ( 'NONE',  ( 100.0000000000260201, 95.00000000000001421, -65.00000000000001421 ) ) ;
#46917 = VERTEX_POINT ( 'NONE', #66236 ) ;
#46918 = ORIENTED_EDGE ( 'NONE', *, *, #39026, .F. ) ;
#46919 = CARTESIAN_POINT ( 'NONE',  ( -12.49999999999999645, 0.000000000000000000, 52.00000000000002132 ) ) ;
#46920 = LINE ( 'NONE', #65324, #3605 ) ;
#46921 = CARTESIAN_POINT ( 'NONE',  ( -93.67500000000003979, 92.29496732002878900, 75.26270833506764291 ) ) ;
#46922 = ORIENTED_EDGE ( 'NONE', *, *, #60105, .F. ) ;
#46923 = CARTESIAN_POINT ( 'NONE',  ( -92.69370383062498320, -209.9999999999999716, 89.48406250086715374 ) ) ;
#46924 = VERTEX_POINT ( 'NONE', #66951 ) ;
#46925 = DIRECTION ( 'NONE',  ( -1.000000000000000000, 0.000000000000000000, 0.000000000000000000 ) ) ;
#46926 = VERTEX_POINT ( 'NONE', #61699 ) ;
#46927 = ADVANCED_FACE ( 'NONE', ( #32367 ), #27464, .F. ) ;
#46928 = ORIENTED_EDGE ( 'NONE', *, *, #15523, .T. ) ;
#46929 = AXIS2_PLACEMENT_3D ( 'NONE', #29905, #42321, #6979 ) ;
#46930 = CARTESIAN_POINT ( 'NONE',  ( 11.99999999999999822, -62.50329211542465657, 41.76937507738766442 ) ) ;
#46931 = AXIS2_PLACEMENT_3D ( 'NONE', #6885, #58771, #46750 ) ;
#46932 = CARTESIAN_POINT ( 'NONE',  ( 96.15314808468748708, 91.99731107132950569, 80.54114583420046358 ) ) ;
#46933 = DIRECTION ( 'NONE',  ( -1.000000000000000000, 0.000000000000000000, -0.000000000000000000 ) ) ;
#46934 = DIRECTION ( 'NONE',  ( -1.000000000000000000, -0.000000000000000000, 0.000000000000000000 ) ) ;
#46935 = ADVANCED_FACE ( 'NONE', ( #73327, #4945 ), #9073, .F. ) ;
#46936 = CARTESIAN_POINT ( 'NONE',  ( -93.67500000000003979, 92.29496732002878900, 85.34333333333333371 ) ) ;
#46937 = LINE ( 'NONE', #40933, #57990 ) ;
#46938 = CARTESIAN_POINT ( 'NONE',  ( 5.999999999999999112, 81.96053171279902472, 2.543863470248677316 ) ) ;
#46939 = EDGE_CURVE ( 'NONE', #5475, #58812, #66597, .T. ) ;
#46940 = FACE_OUTER_BOUND ( 'NONE', #53000, .T. ) ;
#46941 = CARTESIAN_POINT ( 'NONE',  ( 10.00000000000000000, 40.98264845739763018, -9.188173127306866306 ) ) ;
#46942 = DIRECTION ( 'NONE',  ( 0.000000000000000000, 0.000000000000000000, 1.000000000000000000 ) ) ;
#46943 = AXIS2_PLACEMENT_3D ( 'NONE', #69931, #30811, #19903 ) ;
#46944 = EDGE_CURVE ( 'NONE', #21262, #5289, #63703, .T. ) ;
#46945 = DIRECTION ( 'NONE',  ( -1.000000000000000000, 0.000000000000000000, -0.000000000000000000 ) ) ;
#46946 = CARTESIAN_POINT ( 'NONE',  ( -96.15314808468751551, 88.00268892867056536, 85.93864583420048575 ) ) ;
#46947 = VECTOR ( 'NONE', #73527, 1000.000000000000114 ) ;
#46948 = FACE_OUTER_BOUND ( 'NONE', #12302, .T. ) ;
#46949 =( BOUNDED_CURVE ( )  B_SPLINE_CURVE ( 2, ( #66045, #60404, #31802, #43853, #50582, #56619, #74257 ),
 .UNSPECIFIED., .F., .F. ) 
 B_SPLINE_CURVE_WITH_KNOTS ( ( 3, 2, 2, 3 ),
 ( 0.3598440426548558668, 0.3668998081276851342, 0.3739555736686021037, 0.3810111478283708664 ),
 .UNSPECIFIED. ) 
 CURVE ( )  GEOMETRIC_REPRESENTATION_ITEM ( )  RATIONAL_B_SPLINE_CURVE ( ( 1.000000000000000000, 0.8660254037844387076, 1.000000000000000000, 0.8660254037844387076, 1.000000000000000000, 0.8660290377220891678, 0.9999927323218336106 ) ) 
 REPRESENTATION_ITEM ( '' )  );
#46950 = CARTESIAN_POINT ( 'NONE',  ( -94.99999999999997158, -209.9999999999999716, 90.00000000000000000 ) ) ;
#46951 = ADVANCED_FACE ( 'NONE', ( #10550 ), #9441, .T. ) ;
#46952 = ORIENTED_EDGE ( 'NONE', *, *, #20005, .T. ) ;
#46953 = CARTESIAN_POINT ( 'NONE',  ( -12.49999999999999645, 0.000000000000000000, -54.99999999999998579 ) ) ;
#46954 = CARTESIAN_POINT ( 'NONE',  ( 0.000000000000000000, 34.94270380257639630, 74.18225833017899618 ) ) ;
#46955 = ADVANCED_FACE ( 'NONE', ( #15077 ), #21447, .F. ) ;
#46956 = ADVANCED_FACE ( 'NONE', ( #21080 ), #26722, .F. ) ;
#46957 = CARTESIAN_POINT ( 'NONE',  ( 92.35000000000000853, 91.52997821335253548, 77.24708333333332178 ) ) ;
#46958 = FACE_OUTER_BOUND ( 'NONE', #58505, .T. ) ;
#46959 = CARTESIAN_POINT ( 'NONE',  ( 93.84685191531251292, -211.9973110713294489, 82.28739583420048120 ) ) ;
#46960 = ORIENTED_EDGE ( 'NONE', *, *, #50391, .T. ) ;
#46961 = VERTEX_POINT ( 'NONE', #49653 ) ;
#46962 = EDGE_CURVE ( 'NONE', #3079, #54593, #20219, .T. ) ;
#46963 = DIRECTION ( 'NONE',  ( 0.000000000000000000, -0.5224985647159560154, 0.8526401643540879594 ) ) ;
#46964 = ORIENTED_EDGE ( 'NONE', *, *, #72989, .T. ) ;
#46965 = EDGE_CURVE ( 'NONE', #21754, #44827, #44037, .T. ) ;
#46966 = FACE_OUTER_BOUND ( 'NONE', #33603, .T. ) ;
#46967 = CARTESIAN_POINT ( 'NONE',  ( 97.30629616937498838, -211.3315407142195852, 75.30239583420048177 ) ) ;
#46968 = ORIENTED_EDGE ( 'NONE', *, *, #14610, .F. ) ;
#46969 = CARTESIAN_POINT ( 'NONE',  ( 92.69370383062501162, -211.3315407142195852, 80.32947916753381890 ) ) ;
#46970 =( GEOMETRIC_REPRESENTATION_CONTEXT ( 3 ) GLOBAL_UNCERTAINTY_ASSIGNED_CONTEXT ( ( #32462 ) ) GLOBAL_UNIT_ASSIGNED_CONTEXT ( ( #17078, #68211, #56183 ) ) REPRESENTATION_CONTEXT ( 'NONE', 'WORKASPACE' ) );
#46971 = AXIS2_PLACEMENT_3D ( 'NONE', #19339, #20824, #59963 ) ;
#46972 = ORIENTED_EDGE ( 'NONE', *, *, #40513, .F. ) ;
#46973 = DIRECTION ( 'NONE',  ( 0.000000000000000000, -0.9876883405951393247, 0.1564344650402204329 ) ) ;
#46974 = EDGE_LOOP ( 'NONE', ( #33858, #54279, #31854, #10453 ) ) ;
#46975 = AXIS2_PLACEMENT_3D ( 'NONE', #3765, #32669, #13628 ) ;
#46976 = ORIENTED_EDGE ( 'NONE', *, *, #10696, .T. ) ;
#46977 = DIRECTION ( 'NONE',  ( -1.000000000000000000, -0.000000000000000000, -0.000000000000000000 ) ) ;
#46978 = AXIS2_PLACEMENT_3D ( 'NONE', #68104, #5338, #72603 ) ;
#46979 = DIRECTION ( 'NONE',  ( -1.000000000000000000, -0.000000000000000000, 0.000000000000000000 ) ) ;
#46980 = EDGE_LOOP ( 'NONE', ( #25174, #58108, #58534, #39138 ) ) ;
#46981 = DIRECTION ( 'NONE',  ( 0.000000000000000000, 0.000000000000000000, 1.000000000000000000 ) ) ;
#46982 = CARTESIAN_POINT ( 'NONE',  ( 93.67500000000001137, -207.7050326799711968, 88.06854166840095388 ) ) ;
#46983 = CARTESIAN_POINT ( 'NONE',  ( 92.34999999999999432, 91.52997821335252127, 87.40708333333333258 ) ) ;
#46984 = ORIENTED_EDGE ( 'NONE', *, *, #45872, .T. ) ;
#46985 = DIRECTION ( 'NONE',  ( 0.000000000000000000, -0.5877852522924802425, 0.8090169943749422332 ) ) ;
#46986 = DIRECTION ( 'NONE',  ( -0.000000000000000000, 0.000000000000000000, 1.000000000000000000 ) ) ;
#46987 =( REPRESENTATION_RELATIONSHIP ('NONE','NONE', #31117, #15311 ) REPRESENTATION_RELATIONSHIP_WITH_TRANSFORMATION ( #72936 )SHAPE_REPRESENTATION_RELATIONSHIP( ) );
#46988 = ORIENTED_EDGE ( 'NONE', *, *, #6484, .F. ) ;
#46989 = ORIENTED_EDGE ( 'NONE', *, *, #2890, .F. ) ;
#46990 = DIRECTION ( 'NONE',  ( 0.000000000000000000, 0.9510565162951544194, -0.3090169943749446757 ) ) ;
#46991 = VERTEX_POINT ( 'NONE', #31997 ) ;
#46992 = CARTESIAN_POINT ( 'NONE',  ( 96.32499999999998863, 87.70503267997126784, 86.48104166840096241 ) ) ;
#46993 = VERTEX_POINT ( 'NONE', #27090 ) ;
#46994 = EDGE_LOOP ( 'NONE', ( #7791, #51519, #43120, #17743 ) ) ;
#46995 = CARTESIAN_POINT ( 'NONE',  ( 10.00000000000000000, 0.000000000000000000, 0.000000000000000000 ) ) ;
#46996 = AXIS2_PLACEMENT_3D ( 'NONE', #182, #34334, #29789 ) ;
#46997 = CARTESIAN_POINT ( 'NONE',  ( -94.99999999999997158, -206.9400435732949575, 75.23624999999998408 ) ) ;
#46998 = VERTEX_POINT ( 'NONE', #33102 ) ;
#46999 = CIRCLE ( 'NONE', #56612, 20.20000000000036522 ) ;
#47000 = ORIENTED_EDGE ( 'NONE', *, *, #4199, .F. ) ;
#47001 = VERTEX_POINT ( 'NONE', #56051 ) ;
#47002 = FACE_OUTER_BOUND ( 'NONE', #41393, .T. ) ;
#47003 = AXIS2_PLACEMENT_3D ( 'NONE', #54706, #43452, #3235 ) ;
#47004 = LINE ( 'NONE', #14993, #49290 ) ;
#47005 = CARTESIAN_POINT ( 'NONE',  ( -97.65000000000001990, 91.52997821335253548, 88.04208333333332348 ) ) ;
#47006 = VERTEX_POINT ( 'NONE', #50402 ) ;
#47007 = DIRECTION ( 'NONE',  ( -1.000000000000000000, 0.000000000000000000, 0.000000000000000000 ) ) ;
#47008 = AXIS2_PLACEMENT_3D ( 'NONE', #27042, #61282, #67286 ) ;
#47009 = DIRECTION ( 'NONE',  ( 0.000000000000000000, 0.000000000000000000, 1.000000000000000000 ) ) ;
#47010 = ORIENTED_EDGE ( 'NONE', *, *, #54061, .F. ) ;
#47011 = FACE_OUTER_BOUND ( 'NONE', #65657, .T. ) ;
#47012 = CARTESIAN_POINT ( 'NONE',  ( -93.84685191531248449, -208.0026889286704943, 82.44614583420046472 ) ) ;
#47013 = ORIENTED_EDGE ( 'NONE', *, *, #3448, .F. ) ;
#47014 = DIRECTION ( 'NONE',  ( -1.000000000000000000, -1.427937372958388501E-15, 7.962523111839142123E-16 ) ) ;
#47015 = DIRECTION ( 'NONE',  ( 0.000000000000000000, 0.000000000000000000, 1.000000000000000000 ) ) ;
#47016 = PLANE ( 'NONE',  #17680 ) ;
#47017 = CARTESIAN_POINT ( 'NONE',  ( -93.84685191531248449, -208.0026889286704943, 75.46114583420047950 ) ) ;
#47018 = ADVANCED_FACE ( 'NONE', ( #21837 ), #39135, .T. ) ;
#47019 = DIRECTION ( 'NONE',  ( 0.000000000000000000, 0.000000000000000000, 1.000000000000000000 ) ) ;
#47020 = EDGE_CURVE ( 'NONE', #56774, #26992, #60103, .T. ) ;
#47021 = CARTESIAN_POINT ( 'NONE',  ( 10.00000000000000000, 21.40280677340421533, -36.13751322684397138 ) ) ;
#47022 = EDGE_CURVE ( 'NONE', #46909, #25971, #51666, .T. ) ;
#47023 = CARTESIAN_POINT ( 'NONE',  ( 2.369999999999999662, -4.750000000000000888, -5.817072295949926440E-16 ) ) ;
#47024 = EDGE_CURVE ( 'NONE', #70934, #64038, #51145, .T. ) ;
#47025 = CARTESIAN_POINT ( 'NONE',  ( 92.34999999999999432, 89.99996511148934530, 83.09437620840749616 ) ) ;
#47026 = CARTESIAN_POINT ( 'NONE',  ( 92.34999999999998010, 90.00002373248486265, 79.91937418090952860 ) ) ;
#47027 = CARTESIAN_POINT ( 'NONE',  ( -92.69370383062502583, 91.33154071421968467, 79.85322916753379729 ) ) ;
#47028 = DIRECTION ( 'NONE',  ( 0.000000000000000000, 0.000000000000000000, 1.000000000000000000 ) ) ;
#47029 = DIRECTION ( 'NONE',  ( 0.000000000000000000, 0.000000000000000000, 1.000000000000000000 ) ) ;
#47030 = EDGE_LOOP ( 'NONE', ( #38097, #21935, #4378, #23986, #17123, #29946 ) ) ;
#47031 = DIRECTION ( 'NONE',  ( 1.000000000000000000, 0.000000000000000000, 0.000000000000000000 ) ) ;
#47032 = EDGE_CURVE ( 'NONE', #23374, #32002, #1324, .T. ) ;
#47033 = STYLED_ITEM ( 'NONE', ( #18047 ), #40864 ) ;
#47034 = AXIS2_PLACEMENT_3D ( 'NONE', #63663, #58750, #30161 ) ;
#47035 = CARTESIAN_POINT ( 'NONE',  ( 95.00000000000000000, -209.9999999999999716, 90.00000000000000000 ) ) ;
#47036 = CARTESIAN_POINT ( 'NONE',  ( -10.00000000000000000, 0.000000000000000000, 0.000000000000000000 ) ) ;
#47037 = CARTESIAN_POINT ( 'NONE',  ( 13.83832728059186046, -142.6495187161941089, 5.500000000000000000 ) ) ;
#47038 = DIRECTION ( 'NONE',  ( 0.000000000000000000, 0.000000000000000000, 1.000000000000000000 ) ) ;
#47039 = CIRCLE ( 'NONE', #57873, 77.49900000000000944 ) ;
#47040 = CARTESIAN_POINT ( 'NONE',  ( -93.84685191531247028, -211.9973110713294489, 75.40822916753381833 ) ) ;
#47041 = CIRCLE ( 'NONE', #59007, 82.00000000000000000 ) ;
#47042 = CARTESIAN_POINT ( 'NONE',  ( 10.00000000000000000, 16.00000000000000000, 2.500000000000000000 ) ) ;
#47043 = EDGE_CURVE ( 'NONE', #63132, #60480, #45736, .T. ) ;
#47044 =( BOUNDED_CURVE ( )  B_SPLINE_CURVE ( 2, ( #7174, #30091, #53036, #9014, #48133, #70667, #71781 ),
 .UNSPECIFIED., .F., .F. ) 
 B_SPLINE_CURVE_WITH_KNOTS ( ( 3, 2, 2, 3 ),
 ( 0.8958333333333331483, 0.9027777777777775681, 0.9097222222222218768, 0.9166666666666662966 ),
 .UNSPECIFIED. ) 
 CURVE ( )  GEOMETRIC_REPRESENTATION_ITEM ( )  RATIONAL_B_SPLINE_CURVE ( ( 1.000000000000004219, 0.8660254037844343777, 1.000000000000000000, 0.8660254037844387076, 1.000000000000000000, 0.8660254037844451469, 0.9999999999999935607 ) ) 
 REPRESENTATION_ITEM ( '' )  );
#47045 = ORIENTED_EDGE ( 'NONE', *, *, #74190, .T. ) ;
#47046 = DIRECTION ( 'NONE',  ( -1.000000000000000000, -0.000000000000000000, 0.000000000000000000 ) ) ;
#47047 = EDGE_CURVE ( 'NONE', #12401, #54007, #57689, .T. ) ;
#47048 = CARTESIAN_POINT ( 'NONE',  ( 10.00000000000000000, -37.48860685352291711, 0.8828120875899322373 ) ) ;
#47049 = DIRECTION ( 'NONE',  ( 0.000000000000000000, -0.7071067811865389130, -0.7071067811865561215 ) ) ;
#47050 = DIRECTION ( 'NONE',  ( -1.000000000000000000, 0.000000000000000000, -0.000000000000000000 ) ) ;
#47051 = AXIS2_PLACEMENT_3D ( 'NONE', #11179, #55560, #49905 ) ;
#47052 = EDGE_CURVE ( 'NONE', #50648, #62137, #50471, .T. ) ;
#47053 = EDGE_CURVE ( 'NONE', #61582, #34691, #44479, .T. ) ;
#47054 = AXIS2_PLACEMENT_3D ( 'NONE', #64198, #17951, #58537 ) ;
#47055 = VECTOR ( 'NONE', #45671, 1000.000000000000000 ) ;
#47056 = DIRECTION ( 'NONE',  ( 0.000000000000000000, 0.000000000000000000, 1.000000000000000000 ) ) ;
#47057 = ORIENTED_EDGE ( 'NONE', *, *, #72382, .T. ) ;
#47058 = DIRECTION ( 'NONE',  ( -1.000000000000000000, -0.000000000000000000, 0.000000000000000000 ) ) ;
#47059 = ADVANCED_FACE ( 'NONE', ( #22588 ), #17683, .T. ) ;
#47060 = CYLINDRICAL_SURFACE ( 'NONE', #71566, 16.00000000000000000 ) ;
#47061 = ORIENTED_EDGE ( 'NONE', *, *, #43127, .T. ) ;
#47062 = CARTESIAN_POINT ( 'NONE',  ( 97.30629616937498838, -211.3315407142195852, 86.09739583420048348 ) ) ;
#47063 = CARTESIAN_POINT ( 'NONE',  ( 10.00000000000000000, -37.16516213103280108, 4.992566952384862589 ) ) ;
#47064 = VERTEX_POINT ( 'NONE', #28959 ) ;
#47065 = CARTESIAN_POINT ( 'NONE',  ( 93.84685191531249870, -208.0026889286704943, 89.69572916753382685 ) ) ;
#47066 = EDGE_CURVE ( 'NONE', #36714, #38565, #22218, .T. ) ;
#47067 = ORIENTED_EDGE ( 'NONE', *, *, #17720, .F. ) ;
#47068 = LINE ( 'NONE', #17011, #47856 ) ;
#47069 = VERTEX_POINT ( 'NONE', #68460 ) ;
#47070 = CARTESIAN_POINT ( 'NONE',  ( -95.00000000000002842, 87.33691857156074434, 79.16531250086715943 ) ) ;
#47071 = ORIENTED_EDGE ( 'NONE', *, *, #63511, .T. ) ;
#47072 = ORIENTED_EDGE ( 'NONE', *, *, #63180, .T. ) ;
#47073 = DIRECTION ( 'NONE',  ( -1.000000000000000000, 0.000000000000000000, -0.000000000000000000 ) ) ;
#47074 = EDGE_LOOP ( 'NONE', ( #59177, #48005, #8215, #52142 ) ) ;
#47075 = CARTESIAN_POINT ( 'NONE',  ( 0.000000000000000000, 65.64334221924909230, 41.19522573413756561 ) ) ;
#47076 = FACE_OUTER_BOUND ( 'NONE', #57900, .T. ) ;
#47077 = ORIENTED_EDGE ( 'NONE', *, *, #20697, .F. ) ;
#47078 = DIRECTION ( 'NONE',  ( -1.000000000000000000, 0.000000000000000000, 0.000000000000000000 ) ) ;
#47079 = ORIENTED_EDGE ( 'NONE', *, *, #57126, .F. ) ;
#47080 = AXIS2_PLACEMENT_3D ( 'NONE', #11524, #45017, #11892 ) ;
#47081 = DIRECTION ( 'NONE',  ( 1.000000000000000000, 1.427937372958405461E-15, 7.962523111839130290E-16 ) ) ;
#47082 = EDGE_LOOP ( 'NONE', ( #42815, #73811, #52083, #70189 ) ) ;
#47083 = STYLED_ITEM ( 'NONE', ( #28852 ), #13932 ) ;
#47084 = VECTOR ( 'NONE', #3382, 1000.000000000000000 ) ;
#47085 = ORIENTED_EDGE ( 'NONE', *, *, #35924, .F. ) ;
#47086 = ORIENTED_EDGE ( 'NONE', *, *, #24842, .T. ) ;
#47087 = CARTESIAN_POINT ( 'NONE',  ( 96.15314808468748708, -208.0026889286704943, 81.81114583420047381 ) ) ;
#47088 = SHAPE_DEFINITION_REPRESENTATION ( #31333, #8524 ) ;
#47089 = LINE ( 'NONE', #18496, #54605 ) ;
#47091 = DIRECTION ( 'NONE',  ( 0.9966891607226785466, 0.08130631524009969413, 0.000000000000000000 ) ) ;
#47090 = AXIS2_PLACEMENT_3D ( 'NONE', #57118, #6714, #52566 ) ;
#47092 = CYLINDRICAL_SURFACE ( 'NONE', #72527, 3.299999999999969624 ) ;
#47093 = DIRECTION ( 'NONE',  ( -1.000000000000000000, 3.061616997868382648E-16, 0.000000000000000000 ) ) ;
#47094 = DIRECTION ( 'NONE',  ( -1.000000000000000000, 3.061616997868382648E-16, 0.000000000000000000 ) ) ;
#47095 = DIRECTION ( 'NONE',  ( -1.000000000000000000, 0.000000000000000000, 0.000000000000000000 ) ) ;
#47096 = CARTESIAN_POINT ( 'NONE',  ( -97.30629616937497417, -211.3315407142195852, 84.61572916753380014 ) ) ;
#47097 = CARTESIAN_POINT ( 'NONE',  ( -97.30629616937501680, 88.66845928578038638, 83.50447916753383026 ) ) ;
#47098 = CIRCLE ( 'NONE', #54281, 16.00000000000000355 ) ;
#47099 = ORIENTED_EDGE ( 'NONE', *, *, #51937, .F. ) ;
#47100 = CARTESIAN_POINT ( 'NONE',  ( 92.69370383062498320, 88.66845928578037217, 82.07572916753380809 ) ) ;
#47101 = ORIENTED_EDGE ( 'NONE', *, *, #48547, .F. ) ;
#47102 = CARTESIAN_POINT ( 'NONE',  ( 12.00000000000000000, 22.07842321921492612, 8.187992925817123790 ) ) ;
#47103 = CARTESIAN_POINT ( 'NONE',  ( 18.80329974962065265, -105.8248132807389084, 5.500000000000000000 ) ) ;
#47104 = DIRECTION ( 'NONE',  ( -1.000000000000000000, 0.000000000000000000, 0.000000000000000000 ) ) ;
#47105 = CYLINDRICAL_SURFACE ( 'NONE', #758, 16.00000000000000000 ) ;
#47106 = CYLINDRICAL_SURFACE ( 'NONE', #50017, 82.00000000000000000 ) ;
#47107 = CARTESIAN_POINT ( 'NONE',  ( -96.15314808468747287, -208.0026889286704943, 86.36197916753381776 ) ) ;
#47108 = DIRECTION ( 'NONE',  ( 0.000000000000000000, 0.000000000000000000, -1.000000000000000000 ) ) ;
#47109 = EDGE_CURVE ( 'NONE', #73028, #15149, #12056, .T. ) ;
#47110 = CARTESIAN_POINT ( 'NONE',  ( 10.00000000000000000, -5.202137450156655518, 37.22597642581156663 ) ) ;
#47111 = DIRECTION ( 'NONE',  ( -0.8774505977381983346, -0.4796670183876294291, 0.000000000000000000 ) ) ;
#47112 = AXIS2_PLACEMENT_3D ( 'NONE', #46884, #18658, #24317 ) ;
#47113 = CYLINDRICAL_SURFACE ( 'NONE', #33628, 31.99999999999998579 ) ;
#47114 = VERTEX_POINT ( 'NONE', #16949 ) ;
#47115 = EDGE_CURVE ( 'NONE', #59848, #43302, #63959, .T. ) ;
#47116 = ORIENTED_EDGE ( 'NONE', *, *, #26560, .T. ) ;
#47117 = EDGE_CURVE ( 'NONE', #59210, #11931, #27677, .T. ) ;
#47118 = EDGE_CURVE ( 'NONE', #68424, #19511, #19234, .T. ) ;
#47119 = LINE ( 'NONE', #31650, #44702 ) ;
#47120 = CARTESIAN_POINT ( 'NONE',  ( -94.99999999999997158, -213.0599564267049857, 78.72875000000001933 ) ) ;
#47121 = CARTESIAN_POINT ( 'NONE',  ( -93.84685191531252713, 88.00268892867056536, 87.94947916753380923 ) ) ;
#47122 = LINE ( 'NONE', #548, #34575 ) ;
#47123 = CARTESIAN_POINT ( 'NONE',  ( 0.000000000000000000, 0.000000000000000000, 0.000000000000000000 ) ) ;
#47124 = CARTESIAN_POINT ( 'NONE',  ( 15.00000000000000000, -11.95096189432312350, 23.69967320028773372 ) ) ;
#47125 = DIRECTION ( 'NONE',  ( 0.000000000000000000, -0.8910065241883722287, 0.4539904997395382558 ) ) ;
#47126 = ORIENTED_EDGE ( 'NONE', *, *, #50123, .F. ) ;
#47127 = DIRECTION ( 'NONE',  ( -1.000000000000000000, 0.000000000000000000, 0.000000000000000000 ) ) ;
#47128 = ADVANCED_BREP_SHAPE_REPRESENTATION ( '', ( #62646, #43395 ), #61521 ) ;
#47129 = CARTESIAN_POINT ( 'NONE',  ( -235.0000123116479926, -123.0000000000000284, 2.500000000000000000 ) ) ;
#47130 = CARTESIAN_POINT ( 'NONE',  ( 0.000000000000000000, -35.91791733033525702, 68.67312586194982771 ) ) ;
#47131 = DIRECTION ( 'NONE',  ( 0.5687579148473744795, -0.8225049752423790883, 0.000000000000000000 ) ) ;
#47132 = DIRECTION ( 'NONE',  ( -1.000000000000000000, 0.000000000000000000, 0.000000000000000000 ) ) ;
#47133 = CARTESIAN_POINT ( 'NONE',  ( -97.30629616937497417, -211.3315407142195852, 86.67947916753382742 ) ) ;
#47134 = EDGE_CURVE ( 'NONE', #54372, #15642, #39514, .T. ) ;
#47135 = LINE ( 'NONE', #64424, #38917 ) ;
#47136 = DIRECTION ( 'NONE',  ( 0.000000000000000000, 0.000000000000000000, 1.000000000000000000 ) ) ;
#47137 = CARTESIAN_POINT ( 'NONE',  ( -92.69370383062498320, -208.6684592857803295, 76.83697916753382628 ) ) ;
#47138 = DIRECTION ( 'NONE',  ( -1.000000000000000000, 0.000000000000000000, 0.000000000000000000 ) ) ;
#47139 = EDGE_LOOP ( 'NONE', ( #72725, #48919, #61769, #70978 ) ) ;
#47140 =( GEOMETRIC_REPRESENTATION_CONTEXT ( 3 ) GLOBAL_UNCERTAINTY_ASSIGNED_CONTEXT ( ( #25757 ) ) GLOBAL_UNIT_ASSIGNED_CONTEXT ( ( #33274, #32541, #50954 ) ) REPRESENTATION_CONTEXT ( 'NONE', 'WORKASPACE' ) );
#47141 = DIRECTION ( 'NONE',  ( 1.000000000000000000, 0.000000000000000000, 0.000000000000000000 ) ) ;
#47142 = CARTESIAN_POINT ( 'NONE',  ( -97.64999999999996305, -209.9999999999999716, 90.00000000000000000 ) ) ;
#47143 = EDGE_CURVE ( 'NONE', #18128, #40405, #50539, .T. ) ;
#47144 = ADVANCED_FACE ( 'NONE', ( #64656 ), #14251, .F. ) ;
#47145 = CIRCLE ( 'NONE', #53147, 77.49899999999999523 ) ;
#47146 = CARTESIAN_POINT ( 'NONE',  ( -96.15314808468751551, 88.00268892867056536, 75.30239583420048177 ) ) ;
#47147 = CARTESIAN_POINT ( 'NONE',  ( 95.00000000000000000, -207.3369185715606307, 77.41906250086714181 ) ) ;
#47148 = ORIENTED_EDGE ( 'NONE', *, *, #61882, .T. ) ;
#47149 = DIRECTION ( 'NONE',  ( -1.000000000000000000, 0.000000000000000000, 0.000000000000000000 ) ) ;
#47150 = VERTEX_POINT ( 'NONE', #59388 ) ;
#47151 = VECTOR ( 'NONE', #4444, 1000.000000000000000 ) ;
#47152 = DIRECTION ( 'NONE',  ( 0.000000000000000000, 0.000000000000000000, -1.000000000000000000 ) ) ;
#47153 = ORIENTED_EDGE ( 'NONE', *, *, #16728, .F. ) ;
#47154 = VECTOR ( 'NONE', #61449, 1000.000000000000000 ) ;
#47155 = DIRECTION ( 'NONE',  ( 1.000000000000000000, 0.000000000000000000, 0.000000000000000000 ) ) ;
#47156 = AXIS2_PLACEMENT_3D ( 'NONE', #56074, #61354, #21104 ) ;
#47157 = ORIENTED_EDGE ( 'NONE', *, *, #54975, .F. ) ;
#47158 = EDGE_LOOP ( 'NONE', ( #35041, #52037, #63198, #14997 ) ) ;
#47159 = EDGE_LOOP ( 'NONE', ( #20424, #1379, #51142, #57060 ) ) ;
#47160 = CARTESIAN_POINT ( 'NONE',  ( -10.94538922500103162, 0.000000000000000000, 0.000000000000000000 ) ) ;
#47161 = ORIENTED_EDGE ( 'NONE', *, *, #892, .T. ) ;
#47162 = ORIENTED_EDGE ( 'NONE', *, *, #28162, .T. ) ;
#47163 = CARTESIAN_POINT ( 'NONE',  ( 94.99999999999998579, 92.66308142843935514, 78.84781250086714977 ) ) ;
#47164 = CARTESIAN_POINT ( 'NONE',  ( 97.64999999999999147, 90.00000000000002842, 76.34749999999999659 ) ) ;
#47165 = CYLINDRICAL_SURFACE ( 'NONE', #56075, 26.50000000000552092 ) ;
#47166 = VERTEX_POINT ( 'NONE', #13873 ) ;
#47167 = VERTEX_POINT ( 'NONE', #30792 ) ;
#47168 = VERTEX_POINT ( 'NONE', #7516 ) ;
#47169 = LINE ( 'NONE', #70078, #8274 ) ;
#47170 = VERTEX_POINT ( 'NONE', #47369 ) ;
#47171 = LINE ( 'NONE', #57717, #45114 ) ;
#47172 = CARTESIAN_POINT ( 'NONE',  ( 0.000000000000000000, -33.80338159004273280, -16.23288003029533044 ) ) ;
#47173 = CARTESIAN_POINT ( 'NONE',  ( 10.00000000000000000, 0.000000000000000000, 0.000000000000000000 ) ) ;
#47174 = CARTESIAN_POINT ( 'NONE',  ( 10.00000000000000000, -3.894527615417343824, -81.90746397400393164 ) ) ;
#47175 = DIRECTION ( 'NONE',  ( -1.000000000000000000, -0.000000000000000000, -0.000000000000000000 ) ) ;
#47176 = CARTESIAN_POINT ( 'NONE',  ( 11.99999999999999822, 0.000000000000000000, 0.000000000000000000 ) ) ;
#47177 = CARTESIAN_POINT ( 'NONE',  ( -96.32499999999996021, -212.2949673200287179, 78.75520833506763552 ) ) ;
#47178 = ORIENTED_EDGE ( 'NONE', *, *, #53632, .T. ) ;
#47179 = CARTESIAN_POINT ( 'NONE',  ( 7.103376864691351012E-17, -120.0000000000000000, -80.00000000000000000 ) ) ;
#47180 = VERTEX_POINT ( 'NONE', #69913 ) ;
#47182 = CARTESIAN_POINT ( 'NONE',  ( -96.32500000000001705, 92.29496732002878900, 75.36854166840096525 ) ) ;
#47181 = CARTESIAN_POINT ( 'NONE',  ( 96.32499999999998863, 87.70503267997126784, 80.76604166840097321 ) ) ;
#47183 = ORIENTED_EDGE ( 'NONE', *, *, #32652, .F. ) ;
#47184 = CARTESIAN_POINT ( 'NONE',  ( 92.69370383062498320, 90.00000000000002842, 79.00656250086716170 ) ) ;
#47185 = DIRECTION ( 'NONE',  ( 0.000000000000000000, -6.938893903907228378E-15, 1.000000000000000000 ) ) ;
#47186 = DIRECTION ( 'NONE',  ( 0.000000000000000000, -0.9510565162951565288, 0.3090169943749384029 ) ) ;
#47187 = EDGE_CURVE ( 'NONE', #53812, #61985, #6769, .T. ) ;
#47188 = FACE_OUTER_BOUND ( 'NONE', #3007, .T. ) ;
#47189 = CARTESIAN_POINT ( 'NONE',  ( 0.000000000000000000, 10.41901085202078292, 40.68715046381932865 ) ) ;
#47190 = AXIS2_PLACEMENT_3D ( 'NONE', #46427, #11824, #30238 ) ;
#47191 = EDGE_LOOP ( 'NONE', ( #43526, #51484, #5757, #34116 ) ) ;
#47192 = CARTESIAN_POINT ( 'NONE',  ( 92.35000000000000853, -209.9999999999999716, 77.29999999999999716 ) ) ;
#47193 = CARTESIAN_POINT ( 'NONE',  ( 11.99999999999999822, 55.20638768913760686, 51.02545421589343988 ) ) ;
#47194 = ORIENTED_EDGE ( 'NONE', *, *, #44194, .T. ) ;
#47195 = CIRCLE ( 'NONE', #14762, 37.49900000000000944 ) ;
#47196 = EDGE_CURVE ( 'NONE', #62456, #12834, #6073, .T. ) ;
#47197 = VERTEX_POINT ( 'NONE', #70271 ) ;
#47198 = EDGE_CURVE ( 'NONE', #15647, #26264, #59027, .T. ) ;
#47199 = FACE_BOUND ( 'NONE', #46441, .T. ) ;
#47200 = DIRECTION ( 'NONE',  ( -1.000000000000000000, -0.000000000000000000, -0.000000000000000000 ) ) ;
#47201 = CARTESIAN_POINT ( 'NONE',  ( 0.000000000000000000, -65.58780272294100655, 36.73666225445870737 ) ) ;
#47202 = VECTOR ( 'NONE', #46501, 1000.000000000000000 ) ;
#47203 = CARTESIAN_POINT ( 'NONE',  ( -92.69370383062498320, -209.9999999999999716, 78.05406250086716113 ) ) ;
#47204 = EDGE_CURVE ( 'NONE', #47170, #69481, #65409, .T. ) ;
#47205 = AXIS2_PLACEMENT_3D ( 'NONE', #54253, #20401, #8751 ) ;
#47206 = ORIENTED_EDGE ( 'NONE', *, *, #6288, .T. ) ;
#47207 = CARTESIAN_POINT ( 'NONE',  ( 0.000000000000000000, 0.000000000000000000, 77.49899999999999523 ) ) ;
#47208 = VECTOR ( 'NONE', #48853, 1000.000000000000114 ) ;
#47209 = VECTOR ( 'NONE', #15384, 1000.000000000000000 ) ;
#47210 = CARTESIAN_POINT ( 'NONE',  ( 0.000000000000000000, 37.22597642581158084, -5.202137450156524068 ) ) ;
#47211 = FACE_OUTER_BOUND ( 'NONE', #10475, .T. ) ;
#47212 = CARTESIAN_POINT ( 'NONE',  ( 0.000000000000000000, -27.75498641678720446, -31.52238457039628727 ) ) ;
#47213 = CARTESIAN_POINT ( 'NONE',  ( 10.00000000000000000, 0.000000000000000000, 0.000000000000000000 ) ) ;
#47214 = DIRECTION ( 'NONE',  ( -0.000000000000000000, -0.000000000000000000, -1.000000000000000000 ) ) ;
#47215 = CARTESIAN_POINT ( 'NONE',  ( 0.000000000000000000, 33.00180498840072829, -17.80606268964504935 ) ) ;
#47216 = PLANE ( 'NONE',  #14837 ) ;
#47217 = CARTESIAN_POINT ( 'NONE',  ( -97.64999999999996305, -209.9999999999999716, 78.01437500173430806 ) ) ;
#47218 = EDGE_CURVE ( 'NONE', #50757, #9891, #48062, .T. ) ;
#47219 = DIRECTION ( 'NONE',  ( 0.000000000000000000, -0.9945218953682732899, 0.1045284632676548031 ) ) ;
#47220 = ADVANCED_FACE ( 'NONE', ( #36081 ), #18777, .F. ) ;
#47221 = CARTESIAN_POINT ( 'NONE',  ( 97.30629616937498838, 88.66845928578035796, 86.89114583420048632 ) ) ;
#47222 = CARTESIAN_POINT ( 'NONE',  ( -92.69370383062498320, -208.6684592857803295, 87.63197916753381378 ) ) ;
#47223 = DIRECTION ( 'NONE',  ( -1.000000000000000000, 0.000000000000000000, -0.000000000000000000 ) ) ;
#47224 = ORIENTED_EDGE ( 'NONE', *, *, #56126, .T. ) ;
#47225 = DIRECTION ( 'NONE',  ( 1.000000000000000000, 0.000000000000000000, 0.000000000000000000 ) ) ;
#47226 = CARTESIAN_POINT ( 'NONE',  ( -94.99999999999997158, -206.9400435732949575, 82.22124999999999773 ) ) ;
#47227 = CARTESIAN_POINT ( 'NONE',  ( -93.84685191531252713, 88.00268892867056536, 75.24947916753380639 ) ) ;
#47228 = EDGE_CURVE ( 'NONE', #28732, #49041, #54080, .T. ) ;
#47229 = EDGE_CURVE ( 'NONE', #18706, #11201, #42835, .T. ) ;
#47230 = CARTESIAN_POINT ( 'NONE',  ( 95.00000000000000000, -207.3369185715606307, 88.21406250086714351 ) ) ;
#47231 = ORIENTED_EDGE ( 'NONE', *, *, #55879, .T. ) ;
#47232 = VECTOR ( 'NONE', #68680, 999.9999999999998863 ) ;
#47233 = EDGE_LOOP ( 'NONE', ( #36415, #58895, #40996, #52872 ) ) ;
#47234 = ORIENTED_EDGE ( 'NONE', *, *, #66727, .F. ) ;
#47235 = VERTEX_POINT ( 'NONE', #44161 ) ;
#47236 = DIRECTION ( 'NONE',  ( 0.000000000000000000, 0.000000000000000000, 1.000000000000000000 ) ) ;
#47237 = DIRECTION ( 'NONE',  ( -1.000000000000000000, 0.000000000000000000, 0.000000000000000000 ) ) ;
#47238 = VECTOR ( 'NONE', #13395, 1000.000000000000000 ) ;
#47239 = VERTEX_POINT ( 'NONE', #7145 ) ;
#47240 = EDGE_LOOP ( 'NONE', ( #3265, #19151, #39522, #55102 ) ) ;
#47241 = CARTESIAN_POINT ( 'NONE',  ( 93.84685191531249870, -208.0026889286704943, 82.71072916753381321 ) ) ;
#47242 = DIRECTION ( 'NONE',  ( -1.000000000000000000, 0.000000000000000000, 0.000000000000000000 ) ) ;
#47243 = CARTESIAN_POINT ( 'NONE',  ( 4.999999999999999112, -9.188173127307004862, -40.98264845739759465 ) ) ;
#47244 = CIRCLE ( 'NONE', #42416, 42.00000000000000000 ) ;
#47245 =( BOUNDED_SURFACE ( )  B_SPLINE_SURFACE ( 1, 2, ( 
 ( #2473, #31720, #55029, #14805, #43024, #26457, #25719, #59956, #32460, #49391, #59572, #49747, #72671, #20817, #43769, #3192, #26083, #9166, #65587, #8801, #21173, #54304, #48657, #49012, #43411, #25358, #65217, #13690, #71194, #3559, #65965, #20458, #37752, #14054, #36627, #42649, #66689, #60325, #8058, #31353, #72319, #60688, #71573, #20068, #57264, #44508, #67425, #45251, #15554, #22306, #17038, #67799, #28676, #16292, #5769, #15922, #38854, #68167, #38488, #16667, #39975, #61798, #39606, #33200, #62548, #56145, #11028, #56900, #62929, #50869, #27939, #10279, #33953, #4664, #27571, #50499, #5408, #168, #28302, #11387, #34321, #73425, #51239, #74171, #61426, #21934, #44876, #9906, #22685, #45633, #68552, #39233, #27182, #73793, #62162, #10649, #33575, #56532, #51616, #5034, #44123, #67048, #32826, #55776, #4293, #50110, #73045, #21551, #64386, #64756, #30155, #52727, #45989, #24165, #69648, #70362, #23059, #7242, #11743, #47097, #46352, #29403, #7605, #1638, #13241, #6143, #36169, #12495, #18871, #53099, #29048, #6503, #24522, #69281, #51980, #47457, #30518, #35433, #34690, #64020, #12859, #70002, #898, #58743, #57999, #17767, #41809, #59116, #17403, #53466, #68916, #40337, #63284, #58362, #6863, #41443, #23421, #41088, #57644, #12126, #35067, #29774, #1278, #526, #40713, #63657, #52350, #35788, #23784, #18503, #46724, #18142, #24891, #30887, #32000, #2746, #9444, #2001, #20362, #66599, #13607, #43318, #25631, #37300, #48922, #25272, #47820, #53830, #54941, #48565, #32369, #70741, #66238, #71479, #60952, #19979, #15080, #2380, #48197, #3102, #19248, #54576, #49296, #71107, #71845, #65499, #14713, #13965, #25996, #37664, #72220, #8714, #60237, #19613, #60599, #42559, #36910, #59856, #9076, #42198, #3461, #20724, #43680, #8344, #26366, #38021, #65131, #31268, #54216, #36533, #59480, #7969, #42935, #65866, #14350, #31633, #27092, #38764, #61702, #33104, #39889, #67709, #39516, #50775, #73704, #39137, #27847, #10939, #62459, #16570, #22214, #22592, #33862, #10554, #3830, #56437, #27468, #28217, #55312, #56808, #44040, #4949, #4198, #10183, #62838, #5319, #45537, #38397, #68462, #44786, #51147, #74079, #61337, #56054, #16952, #50022, #9816, #11300, #26725, #16199, #66955, #21839, #45156, #68078, #4571, #49655, #15835 ),
 ( #55683, #72949, #72583, #21082, #67335, #15451, #32732, #50405, #73331, #62074, #21452, #33476, #44413, #64660, #40249, #41360, #12040, #58278, #45905, #6772, #23334, #30066, #41719, #47371, #28962, #64300, #17685, #46629, #12771, #69558, #35699, #1183, #63563, #41001, #34233, #57549, #24082, #47005, #57178, #69194, #18058, #40623, #23695, #34981, #28583, #58646, #57916, #24433, #69916, #29685, #7148, #63932, #29320, #11658, #6418, #5682, #52263, #807, #12404, #51524, #80, #17316, #70273, #22974, #46263, #68829, #63197, #34600, #18415, #35353, #52634, #53015, #1548, #18779, #6058, #51897, #438, #36084, #30794, #7518, #14629, #3017, #71388, #13519, #36445, #36814, #37204, #59030, #71023, #13144, #30428, #53377, #19523, #2659, #37574, #1916, #24799, #59391, #7879, #71755, #54482, #42473, #65769, #60148, #8631, #47731, #43228, #48474, #20262, #59763, #31174, #70644, #66150, #19156, #54126, #25909, #13875, #48836, #65412, #42108, #65044, #25538, #53741, #2285, #25177, #48106, #14255, #8246, #19890, #42837, #31539, #67818, #21568, #72337, #3574, #5054, #3943, #26843, #32846, #38504, #10668, #22327, #15936, #56163, #32479, #21950, #49769, #4683, #60707, #9924, #72687, #21190, #45270, #20836, #44896, #67068, #38876, #26478, #61816, #44144, #33593, #14823, #27955, #9560, #16314, #15570, #27197, #39253, #50131, #62181, #27589, #61444, #44525, #37774, #38127, #50516, #73445, #9184, #55796, #73066, #4313, #67444, #10301, #32108, #56552, #33217, #50889, #73812, #55047, #49411, #43790, #66708, #15192, #61067, #55424, #68936, #17424, #6165, #24184, #68191, #51257, #58383, #16689, #5793, #56919, #74194, #22709, #58015, #63300, #63677, #23442, #12515, #914, #39622, #62569, #1295, #11052, #28699, #33970, #5426, #41107, #40733, #39993, #11407, #57659, #29423, #28321, #40356, #45650, #29796, #52751, #51636, #34715, #35451, #6880, #64039, #68571, #17061, #52369, #12144, #187, #545, #17785, #46370, #18164, #23804, #11762, #46745, #23079, #29068, #69666, #6520, #62948, #46007, #35089, #34340, #57280, #51994, #69297, #48587, #18887, #65516, #54595, #30906, #59503, #1658, #3122, #8368, #7620, #41831, #42955, #31284, #41465, #71498, #19997, #2765, #25649, #36551, #65889, #53853, #30174, #35809, #37318, #36191, #59134, #65153, #25290 ) ),
 .UNSPECIFIED., .F., .F., .F. ) 
 B_SPLINE_SURFACE_WITH_KNOTS ( ( 2, 2 ),
 ( 3, 2, 2, 2, 2, 2, 2, 2, 2, 2, 2, 2, 2, 2, 2, 2, 2, 2, 2, 2, 2, 2, 2, 2, 2, 2, 2, 2, 2, 2, 2, 2, 2, 2, 2, 2, 2, 2, 2, 2, 2, 2, 2, 2, 2, 2, 2, 2, 2, 2, 2, 2, 2, 2, 2, 2, 2, 2, 2, 2, 2, 2, 2, 2, 2, 2, 2, 2, 2, 2, 2, 2, 2, 2, 2, 2, 2, 2, 2, 2, 2, 2, 2, 2, 2, 2, 2, 2, 2, 2, 2, 2, 2, 2, 2, 2, 2, 2, 2, 2, 2, 2, 2, 2, 2, 2, 2, 2, 2, 2, 2, 2, 2, 2, 2, 2, 2, 2, 2, 2, 2, 2, 2, 2, 2, 2, 2, 2, 2, 2, 2, 2, 2, 2, 2, 2, 2, 2, 2, 2, 2, 2, 2, 3 ),
 ( 0.000000000000000000, 1.000000000000000000 ),
 ( 0.000000000000000000, 0.006944444444444444059, 0.01388888888888888812, 0.02083333333333333218, 0.02777777777777777624, 0.03472222222222222376, 0.04166666666666666435, 0.04861111111111111188, 0.05555555555555555247, 0.06250000000000000000, 0.06944444444444444753, 0.07638888888888889506, 0.08333333333333332871, 0.09027777777777777624, 0.09722222222222222376, 0.1041666666666666713, 0.1111111111111111049, 0.1180555555555555525, 0.1250000000000000000, 0.1319444444444444475, 0.1388888888888888951, 0.1458333333333333426, 0.1527777777777777901, 0.1597222222222222099, 0.1666666666666666574, 0.1736111111111111049, 0.1805555555555555525, 0.1875000000000000000, 0.1944444444444444475, 0.2013888888888888951, 0.2083333333333333426, 0.2152777777777777901, 0.2222222222222222099, 0.2291666666666666574, 0.2361111111111111049, 0.2430555555555555525, 0.2500000000000000000, 0.2569444444444444198, 0.2638888888888888951, 0.2708333333333333148, 0.2777777777777777901, 0.2847222222222222099, 0.2916666666666666852, 0.2986111111111111049, 0.3055555555555555802, 0.3125000000000000000, 0.3194444444444444198, 0.3263888888888888951, 0.3333333333333333148, 0.3402777777777777901, 0.3472222222222222099, 0.3541666666666666852, 0.3611111111111111049, 0.3680555555555555802, 0.3750000000000000000, 0.3819444444444444198, 0.3888888888888888951, 0.3958333333333333148, 0.4027777777777777901, 0.4097222222222222099, 0.4166666666666666852, 0.4236111111111111049, 0.4305555555555555802, 0.4375000000000000000, 0.4444444444444444198, 0.4513888888888888951, 0.4583333333333333148, 0.4652777777777777901, 0.4722222222222222099, 0.4791666666666666852, 0.4861111111111111049, 0.4930555555555555802, 0.5000000000000000000, 0.5069444444444444198, 0.5138888888888888395, 0.5208333333333333703, 0.5277777777777777901, 0.5347222222222222099, 0.5416666666666666297, 0.5486111111111111605, 0.5555555555555555802, 0.5625000000000000000, 0.5694444444444444198, 0.5763888888888888395, 0.5833333333333333703, 0.5902777777777777901, 0.5972222222222222099, 0.6041666666666666297, 0.6111111111111111605, 0.6180555555555555802, 0.6250000000000000000, 0.6319444444444444198, 0.6388888888888888395, 0.6458333333333333703, 0.6527777777777777901, 0.6597222222222222099, 0.6666666666666666297, 0.6736111111111111605, 0.6805555555555555802, 0.6875000000000000000, 0.6944444444444444198, 0.7013888888888888395, 0.7083333333333333703, 0.7152777777777777901, 0.7222222222222222099, 0.7291666666666666297, 0.7361111111111111605, 0.7430555555555555802, 0.7500000000000000000, 0.7569444444444444198, 0.7638888888888888395, 0.7708333333333333703, 0.7777777777777777901, 0.7847222222222222099, 0.7916666666666666297, 0.7986111111111111605, 0.8055555555555555802, 0.8125000000000000000, 0.8194444444444444198, 0.8263888888888888395, 0.8333333333333333703, 0.8402777777777777901, 0.8472222222222222099, 0.8541666666666666297, 0.8611111111111111605, 0.8680555555555555802, 0.8750000000000000000, 0.8819444444444444198, 0.8888888888888888395, 0.8958333333333333703, 0.9027777777777777901, 0.9097222222222222099, 0.9166666666666666297, 0.9236111111111111605, 0.9305555555555555802, 0.9375000000000000000, 0.9444444444444444198, 0.9513888888888888395, 0.9583333333333333703, 0.9652777777777777901, 0.9722222222222222099, 0.9791666666666666297, 0.9842226772312641092, 0.9940649040035767214 ),
 .UNSPECIFIED. ) 
 GEOMETRIC_REPRESENTATION_ITEM ( )  RATIONAL_B_SPLINE_SURFACE ( (
 ( 1.000000000000000000, 0.8660254037844387076, 1.000000000000000000, 0.8660254037844387076, 1.000000000000000000, 0.8660254037844387076, 1.000000000000000000, 0.8660254037844387076, 1.000000000000000000, 0.8660254037844387076, 1.000000000000000000, 0.8660254037844387076, 1.000000000000000000, 0.8660254037844387076, 1.000000000000000000, 0.8660254037844387076, 1.000000000000000000, 0.8660254037844387076, 1.000000000000000000, 0.8660254037844387076, 1.000000000000000000, 0.8660254037844387076, 1.000000000000000000, 0.8660254037844387076, 1.000000000000000000, 0.8660254037844387076, 1.000000000000000000, 0.8660254037844387076, 1.000000000000000000, 0.8660254037844387076, 1.000000000000000000, 0.8660254037844387076, 1.000000000000000000, 0.8660254037844387076, 1.000000000000000000, 0.8660254037844387076, 1.000000000000000000, 0.8660254037844387076, 1.000000000000000000, 0.8660254037844387076, 1.000000000000000000, 0.8660254037844387076, 1.000000000000000000, 0.8660254037844387076, 1.000000000000000000, 0.8660254037844387076, 1.000000000000000000, 0.8660254037844387076, 1.000000000000000000, 0.8660254037844387076, 1.000000000000000000, 0.8660254037844387076, 1.000000000000000000, 0.8660254037844387076, 1.000000000000000000, 0.8660254037844387076, 1.000000000000000000, 0.8660254037844387076, 1.000000000000000000, 0.8660254037844387076, 1.000000000000000000, 0.8660254037844387076, 1.000000000000000000, 0.8660254037844387076, 1.000000000000000000, 0.8660254037844387076, 1.000000000000000000, 0.8660254037844387076, 1.000000000000000000, 0.8660254037844387076, 1.000000000000000000, 0.8660254037844387076, 1.000000000000000000, 0.8660254037844387076, 1.000000000000000000, 0.8660254037844387076, 1.000000000000000000, 0.8660254037844387076, 1.000000000000000000, 0.8660254037844387076, 1.000000000000000000, 0.8660254037844387076, 1.000000000000000000, 0.8660254037844387076, 1.000000000000000000, 0.8660254037844387076, 1.000000000000000000, 0.8660254037844387076, 1.000000000000000000, 0.8660254037844387076, 1.000000000000000000, 0.8660254037844387076, 1.000000000000000000, 0.8660254037844387076, 1.000000000000000000, 0.8660254037844387076, 1.000000000000000000, 0.8660254037844387076, 1.000000000000000000, 0.8660254037844387076, 1.000000000000000000, 0.8660254037844387076, 1.000000000000000000, 0.8660254037844387076, 1.000000000000000000, 0.8660254037844387076, 1.000000000000000000, 0.8660254037844387076, 1.000000000000000000, 0.8660254037844387076, 1.000000000000000000, 0.8660254037844387076, 1.000000000000000000, 0.8660254037844387076, 1.000000000000000000, 0.8660254037844387076, 1.000000000000000000, 0.8660254037844387076, 1.000000000000000000, 0.8660254037844387076, 1.000000000000000000, 0.8660254037844387076, 1.000000000000000000, 0.8660254037844387076, 1.000000000000000000, 0.8660254037844387076, 1.000000000000000000, 0.8660254037844387076, 1.000000000000000000, 0.8660254037844387076, 1.000000000000000000, 0.8660254037844387076, 1.000000000000000000, 0.8660254037844387076, 1.000000000000000000, 0.8660254037844387076, 1.000000000000000000, 0.8660254037844387076, 1.000000000000000000, 0.8660254037844387076, 1.000000000000000000, 0.8660254037844387076, 1.000000000000000000, 0.8660254037844387076, 1.000000000000000000, 0.8660254037844387076, 1.000000000000000000, 0.8660254037844387076, 1.000000000000000000, 0.8660254037844387076, 1.000000000000000000, 0.8660254037844387076, 1.000000000000000000, 0.8660254037844387076, 1.000000000000000000, 0.8660254037844387076, 1.000000000000000000, 0.8660254037844387076, 1.000000000000000000, 0.8660254037844387076, 1.000000000000000000, 0.8660254037844387076, 1.000000000000000000, 0.8660254037844387076, 1.000000000000000000, 0.8660254037844387076, 1.000000000000000000, 0.8660254037844387076, 1.000000000000000000, 0.8660254037844387076, 1.000000000000000000, 0.8660254037844387076, 1.000000000000000000, 0.8660254037844387076, 1.000000000000000000, 0.8660254037844387076, 1.000000000000000000, 0.8660254037844387076, 1.000000000000000000, 0.8660254037844387076, 1.000000000000000000, 0.8660254037844387076, 1.000000000000000000, 0.8660254037844387076, 1.000000000000000000, 0.8660254037844387076, 1.000000000000000000, 0.8660254037844387076, 1.000000000000000000, 0.8660254037844387076, 1.000000000000000000, 0.8660254037844387076, 1.000000000000000000, 0.8660254037844387076, 1.000000000000000000, 0.8660254037844387076, 1.000000000000000000, 0.8660254037844387076, 1.000000000000000000, 0.8660254037844387076, 1.000000000000000000, 0.8660254037844387076, 1.000000000000000000, 0.8660254037844387076, 1.000000000000000000, 0.8660254037844387076, 1.000000000000000000, 0.8660254037844387076, 1.000000000000000000, 0.8660254037844387076, 1.000000000000000000, 0.8660254037844387076, 1.000000000000000000, 0.8660254037844387076, 1.000000000000000000, 0.8660254037844387076, 1.000000000000000000, 0.8660254037844387076, 1.000000000000000000, 0.8660254037844387076, 1.000000000000000000, 0.8660254037844387076, 1.000000000000000000, 0.8660254037844387076, 1.000000000000000000, 0.8660254037844387076, 1.000000000000000000, 0.8660254037844387076, 1.000000000000000000, 0.8660254037844387076, 1.000000000000000000, 0.8660254037844387076, 1.000000000000000000, 0.8660254037844387076, 1.000000000000000000, 0.8660254037844387076, 1.000000000000000000, 0.8660254037844387076, 1.000000000000000000, 0.8660254037844387076, 1.000000000000000000, 0.8660254037844387076, 1.000000000000000000, 0.8660254037844387076, 1.000000000000000000, 0.8660254037844387076, 1.000000000000000000, 0.8660254037844387076, 1.000000000000000000, 0.8660254037844387076, 1.000000000000000000, 0.8660254037844387076, 1.000000000000000000, 0.8660254037844387076, 1.000000000000000000, 0.8660254037844387076, 1.000000000000000000, 0.8660254037844387076, 1.000000000000000000, 0.8660254037844387076, 1.000000000000000000, 0.8660254037844387076, 1.000000000000000000, 0.8660254037844387076, 1.000000000000000000, 0.8660254037844387076, 1.000000000000000000, 0.8660254037844387076, 1.000000000000000000, 0.8660254037844387076, 1.000000000000000000, 0.8660254037844387076, 1.000000000000000000, 0.8660254037844387076, 1.000000000000000000, 0.8660254037844387076, 1.000000000000000000, 0.8660254037844387076, 1.000000000000000000, 0.8660254037844387076, 1.000000000000000000, 0.8660254037844387076, 1.000000000000000000, 0.9024577157650887083, 0.9469497795711399046, 0.9469497795711399046, 0.9469497795711399046),
 ( 1.000000000000000000, 0.8660254037844387076, 1.000000000000000000, 0.8660254037844387076, 1.000000000000000000, 0.8660254037844387076, 1.000000000000000000, 0.8660254037844387076, 1.000000000000000000, 0.8660254037844387076, 1.000000000000000000, 0.8660254037844387076, 1.000000000000000000, 0.8660254037844387076, 1.000000000000000000, 0.8660254037844387076, 1.000000000000000000, 0.8660254037844387076, 1.000000000000000000, 0.8660254037844387076, 1.000000000000000000, 0.8660254037844387076, 1.000000000000000000, 0.8660254037844387076, 1.000000000000000000, 0.8660254037844387076, 1.000000000000000000, 0.8660254037844387076, 1.000000000000000000, 0.8660254037844387076, 1.000000000000000000, 0.8660254037844387076, 1.000000000000000000, 0.8660254037844387076, 1.000000000000000000, 0.8660254037844387076, 1.000000000000000000, 0.8660254037844387076, 1.000000000000000000, 0.8660254037844387076, 1.000000000000000000, 0.8660254037844387076, 1.000000000000000000, 0.8660254037844387076, 1.000000000000000000, 0.8660254037844387076, 1.000000000000000000, 0.8660254037844387076, 1.000000000000000000, 0.8660254037844387076, 1.000000000000000000, 0.8660254037844387076, 1.000000000000000000, 0.8660254037844387076, 1.000000000000000000, 0.8660254037844387076, 1.000000000000000000, 0.8660254037844387076, 1.000000000000000000, 0.8660254037844387076, 1.000000000000000000, 0.8660254037844387076, 1.000000000000000000, 0.8660254037844387076, 1.000000000000000000, 0.8660254037844387076, 1.000000000000000000, 0.8660254037844387076, 1.000000000000000000, 0.8660254037844387076, 1.000000000000000000, 0.8660254037844387076, 1.000000000000000000, 0.8660254037844387076, 1.000000000000000000, 0.8660254037844387076, 1.000000000000000000, 0.8660254037844387076, 1.000000000000000000, 0.8660254037844387076, 1.000000000000000000, 0.8660254037844387076, 1.000000000000000000, 0.8660254037844387076, 1.000000000000000000, 0.8660254037844387076, 1.000000000000000000, 0.8660254037844387076, 1.000000000000000000, 0.8660254037844387076, 1.000000000000000000, 0.8660254037844387076, 1.000000000000000000, 0.8660254037844387076, 1.000000000000000000, 0.8660254037844387076, 1.000000000000000000, 0.8660254037844387076, 1.000000000000000000, 0.8660254037844387076, 1.000000000000000000, 0.8660254037844387076, 1.000000000000000000, 0.8660254037844387076, 1.000000000000000000, 0.8660254037844387076, 1.000000000000000000, 0.8660254037844387076, 1.000000000000000000, 0.8660254037844387076, 1.000000000000000000, 0.8660254037844387076, 1.000000000000000000, 0.8660254037844387076, 1.000000000000000000, 0.8660254037844387076, 1.000000000000000000, 0.8660254037844387076, 1.000000000000000000, 0.8660254037844387076, 1.000000000000000000, 0.8660254037844387076, 1.000000000000000000, 0.8660254037844387076, 1.000000000000000000, 0.8660254037844387076, 1.000000000000000000, 0.8660254037844387076, 1.000000000000000000, 0.8660254037844387076, 1.000000000000000000, 0.8660254037844387076, 1.000000000000000000, 0.8660254037844387076, 1.000000000000000000, 0.8660254037844387076, 1.000000000000000000, 0.8660254037844387076, 1.000000000000000000, 0.8660254037844387076, 1.000000000000000000, 0.8660254037844387076, 1.000000000000000000, 0.8660254037844387076, 1.000000000000000000, 0.8660254037844387076, 1.000000000000000000, 0.8660254037844387076, 1.000000000000000000, 0.8660254037844387076, 1.000000000000000000, 0.8660254037844387076, 1.000000000000000000, 0.8660254037844387076, 1.000000000000000000, 0.8660254037844387076, 1.000000000000000000, 0.8660254037844387076, 1.000000000000000000, 0.8660254037844387076, 1.000000000000000000, 0.8660254037844387076, 1.000000000000000000, 0.8660254037844387076, 1.000000000000000000, 0.8660254037844387076, 1.000000000000000000, 0.8660254037844387076, 1.000000000000000000, 0.8660254037844387076, 1.000000000000000000, 0.8660254037844387076, 1.000000000000000000, 0.8660254037844387076, 1.000000000000000000, 0.8660254037844387076, 1.000000000000000000, 0.8660254037844387076, 1.000000000000000000, 0.8660254037844387076, 1.000000000000000000, 0.8660254037844387076, 1.000000000000000000, 0.8660254037844387076, 1.000000000000000000, 0.8660254037844387076, 1.000000000000000000, 0.8660254037844387076, 1.000000000000000000, 0.8660254037844387076, 1.000000000000000000, 0.8660254037844387076, 1.000000000000000000, 0.8660254037844387076, 1.000000000000000000, 0.8660254037844387076, 1.000000000000000000, 0.8660254037844387076, 1.000000000000000000, 0.8660254037844387076, 1.000000000000000000, 0.8660254037844387076, 1.000000000000000000, 0.8660254037844387076, 1.000000000000000000, 0.8660254037844387076, 1.000000000000000000, 0.8660254037844387076, 1.000000000000000000, 0.8660254037844387076, 1.000000000000000000, 0.8660254037844387076, 1.000000000000000000, 0.8660254037844387076, 1.000000000000000000, 0.8660254037844387076, 1.000000000000000000, 0.8660254037844387076, 1.000000000000000000, 0.8660254037844387076, 1.000000000000000000, 0.8660254037844387076, 1.000000000000000000, 0.8660254037844387076, 1.000000000000000000, 0.8660254037844387076, 1.000000000000000000, 0.8660254037844387076, 1.000000000000000000, 0.8660254037844387076, 1.000000000000000000, 0.8660254037844387076, 1.000000000000000000, 0.8660254037844387076, 1.000000000000000000, 0.8660254037844387076, 1.000000000000000000, 0.8660254037844387076, 1.000000000000000000, 0.8660254037844387076, 1.000000000000000000, 0.8660254037844387076, 1.000000000000000000, 0.8660254037844387076, 1.000000000000000000, 0.8660254037844387076, 1.000000000000000000, 0.8660254037844387076, 1.000000000000000000, 0.8660254037844387076, 1.000000000000000000, 0.8660254037844387076, 1.000000000000000000, 0.8660254037844387076, 1.000000000000000000, 0.8660254037844387076, 1.000000000000000000, 0.8660254037844387076, 1.000000000000000000, 0.8660254037844387076, 1.000000000000000000, 0.8660254037844387076, 1.000000000000000000, 0.8660254037844387076, 1.000000000000000000, 0.8660254037844387076, 1.000000000000000000, 0.8660254037844387076, 1.000000000000000000, 0.8660254037844387076, 1.000000000000000000, 0.8660254037844387076, 1.000000000000000000, 0.8660254037844387076, 1.000000000000000000, 0.8660254037844387076, 1.000000000000000000, 0.8660254037844387076, 1.000000000000000000, 0.8660254037844387076, 1.000000000000000000, 0.8660254037844387076, 1.000000000000000000, 0.9024577157650887083, 0.9469497795711399046, 0.9469497795711399046, 0.9469497795711399046) ) ) 
 REPRESENTATION_ITEM ( '' )  SURFACE ( )  );
#47246 = CARTESIAN_POINT ( 'NONE',  ( 96.32499999999997442, 92.29496732002878900, 82.80333333333332746 ) ) ;
#47247 = DIRECTION ( 'NONE',  ( -1.000000000000000000, -0.000000000000000000, 0.000000000000000000 ) ) ;
#47248 = AXIS2_PLACEMENT_3D ( 'NONE', #22825, #16430, #26309 ) ;
#47249 = DIRECTION ( 'NONE',  ( -1.000000000000000000, 0.000000000000000000, -0.000000000000000000 ) ) ;
#47250 = CARTESIAN_POINT ( 'NONE',  ( 95.00000000000000000, -213.0599564267049857, 86.34874999999999545 ) ) ;
#47251 = ADVANCED_FACE ( 'NONE', ( #24797 ), #65766, .T. ) ;
#47252 = ORIENTED_EDGE ( 'NONE', *, *, #2176, .T. ) ;
#47253 = ORIENTED_EDGE ( 'NONE', *, *, #49725, .T. ) ;
#47254 = ORIENTED_EDGE ( 'NONE', *, *, #39205, .T. ) ;
#47255 = AXIS2_PLACEMENT_3D ( 'NONE', #16042, #10779, #38984 ) ;
#47256 = ORIENTED_EDGE ( 'NONE', *, *, #70319, .F. ) ;
#47258 = VECTOR ( 'NONE', #49234, 1000.000000000000000 ) ;
#47257 = CARTESIAN_POINT ( 'NONE',  ( 0.000000000000000000, -40.68715046381937128, 10.41901085202062660 ) ) ;
#47259 = CIRCLE ( 'NONE', #61646, 16.00000000000000000 ) ;
#47260 =( LENGTH_UNIT ( ) NAMED_UNIT ( * ) SI_UNIT ( .MILLI., .METRE. ) );
#47261 = CARTESIAN_POINT ( 'NONE',  ( -97.30629616937501680, 90.00000000000004263, 87.89656250086714806 ) ) ;
#47262 = LINE ( 'NONE', #13770, #14937 ) ;
#47263 = ADVANCED_FACE ( 'NONE', ( #47002 ), #41357, .F. ) ;
#47264 = DIRECTION ( 'NONE',  ( -1.000000000000000000, 0.000000000000000000, -0.000000000000000000 ) ) ;
#47265 = CARTESIAN_POINT ( 'NONE',  ( 92.69370383062501162, -209.9999999999999716, 88.37281250086715545 ) ) ;
#47266 = CARTESIAN_POINT ( 'NONE',  ( 96.32499999999998863, 87.70503267997126784, 78.78166666666666629 ) ) ;
#47267 = EDGE_CURVE ( 'NONE', #13854, #66356, #64298, .T. ) ;
#47268 = ORIENTED_EDGE ( 'NONE', *, *, #60554, .F. ) ;
#47269 = DIRECTION ( 'NONE',  ( -1.000000000000000000, -0.000000000000000000, -0.000000000000000000 ) ) ;
#47270 = EDGE_LOOP ( 'NONE', ( #32791, #59912, #41273, #61248 ) ) ;
#47271 = DIRECTION ( 'NONE',  ( 0.000000000000000000, -0.4067366430757887730, 0.9135454576426059736 ) ) ;
#47272 = ORIENTED_EDGE ( 'NONE', *, *, #5728, .T. ) ;
#47273 = CARTESIAN_POINT ( 'NONE',  ( -97.65000000000001990, 91.52997821335253548, 86.85145833506763324 ) ) ;
#47274 = CARTESIAN_POINT ( 'NONE',  ( 97.30629616937498838, 91.33154071421968467, 88.90197916753382401 ) ) ;
#47275 = VERTEX_POINT ( 'NONE', #35697 ) ;
#47276 = DIRECTION ( 'NONE',  ( -1.000000000000000000, 0.000000000000000000, -0.000000000000000000 ) ) ;
#47277 = AXIS2_PLACEMENT_3D ( 'NONE', #64747, #22498, #10462 ) ;
#47278 = ADVANCED_FACE ( 'NONE', ( #47729 ), #30064, .F. ) ;
#47279 = DIRECTION ( 'NONE',  ( -1.000000000000000000, 0.000000000000000000, 0.000000000000000000 ) ) ;
#47280 = DIRECTION ( 'NONE',  ( -0.000000000000000000, -0.000000000000000000, 1.000000000000000000 ) ) ;
#47281 = CARTESIAN_POINT ( 'NONE',  ( -92.34999999999999432, -208.4700217866474645, 86.00479166840096923 ) ) ;
#47282 = VERTEX_POINT ( 'NONE', #55878 ) ;
#47283 = PLANE ( 'NONE',  #15901 ) ;
#47284 = CARTESIAN_POINT ( 'NONE',  ( 0.000000000000000000, 56.15606465355041621, -59.75363087400017292 ) ) ;
#47285 = ORIENTED_EDGE ( 'NONE', *, *, #35315, .F. ) ;
#47286 = ORIENTED_EDGE ( 'NONE', *, *, #41239, .F. ) ;
#47287 = CARTESIAN_POINT ( 'NONE',  ( 0.000000000000000000, -68.26794271651239399, -31.47745569255214093 ) ) ;
#47288 = CYLINDRICAL_SURFACE ( 'NONE', #21596, 42.00000000000000000 ) ;
#47289 = AXIS2_PLACEMENT_3D ( 'NONE', #33392, #61996, #11221 ) ;
#47290 = CARTESIAN_POINT ( 'NONE',  ( 16.30584220631899228, -140.9432449716519784, 2.500000000000000000 ) ) ;
#47291 = ORIENTED_EDGE ( 'NONE', *, *, #802, .T. ) ;
#47292 = CARTESIAN_POINT ( 'NONE',  ( -96.15314808468747287, -208.0026889286704943, 86.52072916753382970 ) ) ;
#47293 = ORIENTED_EDGE ( 'NONE', *, *, #20877, .F. ) ;
#47294 = EDGE_CURVE ( 'NONE', #31131, #38013, #44537, .T. ) ;
#47295 = LINE ( 'NONE', #13063, #23679 ) ;
#47296 = ORIENTED_EDGE ( 'NONE', *, *, #40493, .F. ) ;
#47297 = EDGE_LOOP ( 'NONE', ( #955, #63177 ) ) ;
#47298 = CARTESIAN_POINT ( 'NONE',  ( 10.00000000000000000, 39.04073710021366139, -15.48615015657542848 ) ) ;
#47299 = CIRCLE ( 'NONE', #14870, 15.06715634359041900 ) ;
#47300 = DIRECTION ( 'NONE',  ( -1.000000000000000000, -0.000000000000000000, -0.000000000000000000 ) ) ;
#47301 = CARTESIAN_POINT ( 'NONE',  ( -10.00000000000000000, 0.000000000000000000, 0.000000000000000000 ) ) ;
#47302 = CARTESIAN_POINT ( 'NONE',  ( 97.30629616937498838, 90.00000000000002842, 81.70531250086713726 ) ) ;
#47303 = DIRECTION ( 'NONE',  ( 1.000000000000000000, -0.000000000000000000, -0.000000000000000000 ) ) ;
#47304 = CYLINDRICAL_SURFACE ( 'NONE', #43399, 1.000000000000000000 ) ;
#47305 = CARTESIAN_POINT ( 'NONE',  ( -92.35000000000000853, 91.52997821335252127, 85.29041666666665833 ) ) ;
#47306 = DIRECTION ( 'NONE',  ( -1.000000000000000000, 0.000000000000000000, -0.000000000000000000 ) ) ;
#47307 = CARTESIAN_POINT ( 'NONE',  ( 92.35000000000000853, -209.9999999999999716, 80.47499999999999432 ) ) ;
#47308 = EDGE_CURVE ( 'NONE', #8777, #67030, #19295, .T. ) ;
#47309 = DIRECTION ( 'NONE',  ( -1.000000000000000000, 0.000000000000000000, -0.000000000000000000 ) ) ;
#47310 = CARTESIAN_POINT ( 'NONE',  ( 97.64999999999999147, 90.00000000000002842, 83.96750000000000114 ) ) ;
#47311 = EDGE_CURVE ( 'NONE', #67765, #55839, #32300, .T. ) ;
#47312 = AXIS2_PLACEMENT_3D ( 'NONE', #27445, #37273, #32708 ) ;
#47313 = ADVANCED_FACE ( 'NONE', ( #71753 ), #10010, .T. ) ;
#47314 = VECTOR ( 'NONE', #7285, 1000.000000000000000 ) ;
#47315 = CYLINDRICAL_SURFACE ( 'NONE', #9593, 31.99999999999999289 ) ;
#47316 = LINE ( 'NONE', #13458, #16950 ) ;
#47317 = AXIS2_PLACEMENT_3D ( 'NONE', #67084, #38521, #29079 ) ;
#47318 = CARTESIAN_POINT ( 'NONE',  ( -93.84685191531254134, 91.99731107132950569, 84.98614583420047097 ) ) ;
#47319 = CARTESIAN_POINT ( 'NONE',  ( 10.00000000000000000, 11.30684508768339569, 76.66974797899841576 ) ) ;
#47320 = DIRECTION ( 'NONE',  ( 0.000000000000000000, 7.228014483236689653E-16, -1.000000000000000000 ) ) ;
#47321 = ORIENTED_EDGE ( 'NONE', *, *, #69027, .F. ) ;
#47322 = DIRECTION ( 'NONE',  ( -0.1045284632676436315, -0.9945218953682742891, 0.000000000000000000 ) ) ;
#47323 = DIRECTION ( 'NONE',  ( -0.000000000000000000, -0.000000000000000000, 1.000000000000000000 ) ) ;
#47324 = DIRECTION ( 'NONE',  ( 0.000000000000000000, 0.000000000000000000, 1.000000000000000000 ) ) ;
#47325 = DIRECTION ( 'NONE',  ( -1.000000000000000000, 0.000000000000000000, 0.000000000000000000 ) ) ;
#47326 = CARTESIAN_POINT ( 'NONE',  ( 93.84685191531249870, -208.0026889286704943, 82.71072916753381321 ) ) ;
#47327 = ORIENTED_EDGE ( 'NONE', *, *, #67376, .T. ) ;
#47328 = VERTEX_POINT ( 'NONE', #73900 ) ;
#47329 = CARTESIAN_POINT ( 'NONE',  ( 11.99999999999999822, -41.76937507738745836, -62.50329211542482710 ) ) ;
#47330 = ORIENTED_EDGE ( 'NONE', *, *, #49157, .T. ) ;
#47331 = CIRCLE ( 'NONE', #60547, 32.50000000000000000 ) ;
#47332 = DIRECTION ( 'NONE',  ( -1.000000000000000000, 0.000000000000000000, -0.000000000000000000 ) ) ;
#47333 = CARTESIAN_POINT ( 'NONE',  ( 95.00000000000000000, -212.6630814284392557, 75.19656250086714522 ) ) ;
#47334 = EDGE_LOOP ( 'NONE', ( #37260, #71928, #5839, #6817 ) ) ;
#47335 = CARTESIAN_POINT ( 'NONE',  ( 97.30629616937498838, -211.3315407142195852, 78.00114583420049996 ) ) ;
#47336 = ORIENTED_EDGE ( 'NONE', *, *, #39063, .T. ) ;
#47337 = CARTESIAN_POINT ( 'NONE',  ( 11.99999999999999822, -77.19088730480518734, -6.903761155838607166 ) ) ;
#47338 = ORIENTED_EDGE ( 'NONE', *, *, #60303, .F. ) ;
#47339 = ORIENTED_EDGE ( 'NONE', *, *, #33427, .T. ) ;
#47340 = CARTESIAN_POINT ( 'NONE',  ( 95.00000000000000000, -206.9400435732949575, 86.74562500173429669 ) ) ;
#47341 = VECTOR ( 'NONE', #16177, 1000.000000000000000 ) ;
#47342 =( NAMED_UNIT ( * ) PLANE_ANGLE_UNIT ( ) SI_UNIT ( $, .RADIAN. ) );
#47343 = DIRECTION ( 'NONE',  ( -1.000000000000000000, -0.000000000000000000, 0.000000000000000000 ) ) ;
#47344 = EDGE_CURVE ( 'NONE', #34327, #66429, #11130, .T. ) ;
#47345 = ORIENTED_EDGE ( 'NONE', *, *, #6562, .T. ) ;
#47346 = CARTESIAN_POINT ( 'NONE',  ( 10.00000000000000000, 77.19088730480524418, 6.903761155838049390 ) ) ;
#47347 = CARTESIAN_POINT ( 'NONE',  ( 95.00000000000000000, -213.0599564267049857, 81.98312500173430806 ) ) ;
#47348 = CARTESIAN_POINT ( 'NONE',  ( 97.30629616937497417, 89.06968786819601291, 74.84209103131392737 ) ) ;
#47349 = EDGE_CURVE ( 'NONE', #19214, #70942, #50220, .T. ) ;
#47350 = VERTEX_POINT ( 'NONE', #45356 ) ;
#47351 = DIRECTION ( 'NONE',  ( -1.000000000000000000, -0.000000000000000000, 0.000000000000000000 ) ) ;
#47352 = FACE_OUTER_BOUND ( 'NONE', #31445, .T. ) ;
#47353 = ORIENTED_EDGE ( 'NONE', *, *, #26545, .T. ) ;
#47354 = VERTEX_POINT ( 'NONE', #4391 ) ;
#47355 = FACE_OUTER_BOUND ( 'NONE', #44381, .T. ) ;
#47356 = EDGE_LOOP ( 'NONE', ( #60057, #17317, #41225, #55735 ) ) ;
#47357 = CARTESIAN_POINT ( 'NONE',  ( 93.67499999999998295, 92.29496732002878900, 86.79854166840097207 ) ) ;
#47358 = EDGE_CURVE ( 'NONE', #11199, #63551, #8515, .T. ) ;
#47359 = EDGE_CURVE ( 'NONE', #32129, #18143, #2551, .T. ) ;
#47360 = ORIENTED_EDGE ( 'NONE', *, *, #18191, .T. ) ;
#47361 = CIRCLE ( 'NONE', #66423, 11.59999999999999964 ) ;
#47362 = ORIENTED_EDGE ( 'NONE', *, *, #54598, .T. ) ;
#47363 = CARTESIAN_POINT ( 'NONE',  ( 92.34999999999995168, -211.5299782133524502, 77.98791666666667766 ) ) ;
#47364 = AXIS2_PLACEMENT_3D ( 'NONE', #72528, #49236, #37963 ) ;
#47365 = CARTESIAN_POINT ( 'NONE',  ( -92.35000000000678710, 90.00000598221780024, 82.14187520865721126 ) ) ;
#47366 = VERTEX_POINT ( 'NONE', #56638 ) ;
#47367 = EDGE_LOOP ( 'NONE', ( #37112, #43467, #45990, #39396 ) ) ;
#47368 = EDGE_LOOP ( 'NONE', ( #23129, #35297, #13222, #16473 ) ) ;
#47369 = CARTESIAN_POINT ( 'NONE',  ( 97.64999999999999147, -209.9999999999999716, 80.15749999999999886 ) ) ;
#47370 = CARTESIAN_POINT ( 'NONE',  ( 2.117611129180199558, -93.54218975225703048, -5.500000000000000000 ) ) ;
#47371 = CARTESIAN_POINT ( 'NONE',  ( -97.65000000000001990, 88.47002178664754979, 88.78291666666667936 ) ) ;
#47372 = ORIENTED_EDGE ( 'NONE', *, *, #12890, .F. ) ;
#47373 = LINE ( 'NONE', #41364, #26320 ) ;
#47374 = CIRCLE ( 'NONE', #24565, 31.99999999999998579 ) ;
#47375 = CARTESIAN_POINT ( 'NONE',  ( -3.000000000000000000, 14.60985201121704513, 18.46759930825707841 ) ) ;
#47376 = ORIENTED_EDGE ( 'NONE', *, *, #33252, .F. ) ;
#47377 = CARTESIAN_POINT ( 'NONE',  ( 94.99999999999998579, 90.00000000000002842, 90.00000000000000000 ) ) ;
#47378 = CARTESIAN_POINT ( 'NONE',  ( -93.84685191531247028, -211.9973110713294489, 82.86947916753379673 ) ) ;
#47379 = ORIENTED_EDGE ( 'NONE', *, *, #8586, .T. ) ;
#47381 = EDGE_CURVE ( 'NONE', #37554, #32596, #44980, .T. ) ;
#47380 = CARTESIAN_POINT ( 'NONE',  ( 12.13205353604972991, -140.1820037904669789, 5.500000000000000000 ) ) ;
#47382 = CARTESIAN_POINT ( 'NONE',  ( -70.53423027509626309, -217.0820393249940423, -5.500000000000000000 ) ) ;
#47383 = CARTESIAN_POINT ( 'NONE',  ( 26.00000000000000355, 0.000000000000000000, 2.445500000000000007 ) ) ;
#47384 = DIRECTION ( 'NONE',  ( 0.000000000000000000, 0.000000000000000000, -1.000000000000000000 ) ) ;
#47385 = AXIS2_PLACEMENT_3D ( 'NONE', #40903, #47280, #65316 ) ;
#47386 = CYLINDRICAL_SURFACE ( 'NONE', #24764, 16.00000000000000000 ) ;
#47387 = CARTESIAN_POINT ( 'NONE',  ( 10.00000000000000000, -27.74655509720617275, -77.16300072079690153 ) ) ;
#47388 = DIRECTION ( 'NONE',  ( -1.000000000000000000, 0.000000000000000000, 0.000000000000000000 ) ) ;
#47389 = CARTESIAN_POINT ( 'NONE',  ( 10.00000000000000000, 74.65491531819118620, -8.830959090342659579 ) ) ;
#47390 = DIRECTION ( 'NONE',  ( 0.000000000000000000, 0.3090169943749411230, 0.9510565162951555296 ) ) ;
#47391 = CARTESIAN_POINT ( 'NONE',  ( 92.34999999999999432, 90.00000000000002842, 79.91937500173429498 ) ) ;
#47392 = EDGE_CURVE ( 'NONE', #54476, #59274, #61327, .T. ) ;
#47393 = EDGE_CURVE ( 'NONE', #54089, #37730, #16777, .T. ) ;
#47394 = CARTESIAN_POINT ( 'NONE',  ( -96.15314808468751551, 88.00268892867056536, 79.58864583420047722 ) ) ;
#47395 = DIRECTION ( 'NONE',  ( 1.000000000000000000, 0.000000000000000000, 0.000000000000000000 ) ) ;
#47396 = CARTESIAN_POINT ( 'NONE',  ( 0.000000000000000000, 22.48208911017551515, -35.47612816024499693 ) ) ;
#47397 = EDGE_CURVE ( 'NONE', #31904, #44373, #20257, .T. ) ;
#47398 = DIRECTION ( 'NONE',  ( 1.000000000000000000, 0.000000000000000000, 0.000000000000000000 ) ) ;
#47399 = CARTESIAN_POINT ( 'NONE',  ( -97.64999999980585699, -210.0000198431789897, 84.36502761000342332 ) ) ;
#47400 = CARTESIAN_POINT ( 'NONE',  ( 6.000000000000000000, -16.65972982744991171, 80.28980883073752750 ) ) ;
#47401 = CIRCLE ( 'NONE', #14924, 31.99999999999998579 ) ;
#47402 = CARTESIAN_POINT ( 'NONE',  ( 96.37670920697046029, 87.70919997534038259, 75.00000000000000000 ) ) ;
#47403 = DIRECTION ( 'NONE',  ( -2.603472992746261562E-14, -2.546204323184492723E-14, 1.000000000000000000 ) ) ;
#47404 = DIRECTION ( 'NONE',  ( 1.000000000000000000, 0.000000000000000000, 0.000000000000000000 ) ) ;
#47405 = CARTESIAN_POINT ( 'NONE',  ( -97.30629616937495996, -209.9999999999999716, 75.19656250086714522 ) ) ;
#47406 = LINE ( 'NONE', #1952, #17689 ) ;
#47407 = ORIENTED_EDGE ( 'NONE', *, *, #21888, .T. ) ;
#47408 = VECTOR ( 'NONE', #61534, 1000.000000000000000 ) ;
#47409 = CARTESIAN_POINT ( 'NONE',  ( 0.000000000000000000, -73.73191006444561424, -14.66109333815538918 ) ) ;
#47410 = FACE_OUTER_BOUND ( 'NONE', #24941, .T. ) ;
#47411 = DIRECTION ( 'NONE',  ( 1.000000000000000000, 0.000000000000000000, 0.000000000000000000 ) ) ;
#47412 = CARTESIAN_POINT ( 'NONE',  ( 3.000000000000000000, -1.467624384280027838, 2.542000000000001592 ) ) ;
#47413 = AXIS2_PLACEMENT_3D ( 'NONE', #24025, #61750, #18364 ) ;
#47414 = CARTESIAN_POINT ( 'NONE',  ( -97.64999999950704535, 89.99996796756893502, 85.63541623677065218 ) ) ;
#47415 = VERTEX_POINT ( 'NONE', #62656 ) ;
#47416 = CARTESIAN_POINT ( 'NONE',  ( -10.00000000000000000, 0.000000000000000000, 0.000000000000000000 ) ) ;
#47417 = DIRECTION ( 'NONE',  ( -1.000000000000000000, 0.000000000000000000, 0.000000000000000000 ) ) ;
#47418 = ORIENTED_EDGE ( 'NONE', *, *, #65606, .T. ) ;
#47419 = EDGE_CURVE ( 'NONE', #11723, #51387, #33298, .T. ) ;
#47420 = CARTESIAN_POINT ( 'NONE',  ( 95.00000000000000000, -212.6630814284392557, 86.62656250086713783 ) ) ;
#47421 = CARTESIAN_POINT ( 'NONE',  ( 96.15314808468750130, -211.9973110713294489, 87.47322916753381605 ) ) ;
#47422 = ORIENTED_EDGE ( 'NONE', *, *, #10166, .T. ) ;
#47423 = VECTOR ( 'NONE', #6601, 1000.000000000000000 ) ;
#47424 = ADVANCED_FACE ( 'NONE', ( #43226 ), #60162, .T. ) ;
#47425 = DIRECTION ( 'NONE',  ( -1.000000000000000000, -0.000000000000000000, -0.000000000000000000 ) ) ;
#47426 = VERTEX_POINT ( 'NONE', #28406 ) ;
#47427 = DIRECTION ( 'NONE',  ( 0.000000000000000000, 0.7431448254773939111, 0.6691306063588584596 ) ) ;
#47428 = ORIENTED_EDGE ( 'NONE', *, *, #4015, .F. ) ;
#47429 = CARTESIAN_POINT ( 'NONE',  ( -95.00000000000002842, 87.33691857156074434, 82.34031250086714238 ) ) ;
#47430 = EDGE_CURVE ( 'NONE', #56810, #61359, #51341, .T. ) ;
#47431 = EDGE_LOOP ( 'NONE', ( #13631, #50848, #61780, #73525 ) ) ;
#47432 = AXIS2_PLACEMENT_3D ( 'NONE', #17073, #34350, #28712 ) ;
#47433 = ORIENTED_EDGE ( 'NONE', *, *, #59319, .F. ) ;
#47434 = CARTESIAN_POINT ( 'NONE',  ( -92.34999999999999432, -211.5299782133524218, 87.80395833506766223 ) ) ;
#47435 = EDGE_CURVE ( 'NONE', #20698, #47697, #14626, .T. ) ;
#47436 = ORIENTED_EDGE ( 'NONE', *, *, #56169, .T. ) ;
#47437 = CARTESIAN_POINT ( 'NONE',  ( 0.000000000000000000, 59.46389618802034960, -49.70050353004825894 ) ) ;
#47438 = SURFACE_STYLE_FILL_AREA ( #7583 ) ;
#47439 = VERTEX_POINT ( 'NONE', #6958 ) ;
#47440 = DIRECTION ( 'NONE',  ( -0.000000000000000000, -0.000000000000000000, 1.000000000000000000 ) ) ;
#47441 = ORIENTED_EDGE ( 'NONE', *, *, #22071, .F. ) ;
#47442 = CARTESIAN_POINT ( 'NONE',  ( 92.79788703567041352, 88.68334238502474420, 74.94590613650809985 ) ) ;
#47443 = ORIENTED_EDGE ( 'NONE', *, *, #39831, .F. ) ;
#47444 = EDGE_CURVE ( 'NONE', #29284, #63342, #49344, .T. ) ;
#47445 = EDGE_LOOP ( 'NONE', ( #68465, #55678, #58647, #3013 ) ) ;
#47446 = VERTEX_POINT ( 'NONE', #30259 ) ;
#47447 = CARTESIAN_POINT ( 'NONE',  ( 96.15314808468748708, -208.0026889286704943, 80.54114583420046358 ) ) ;
#47448 = DIRECTION ( 'NONE',  ( -1.000000000000000000, 0.000000000000000000, 0.000000000000000000 ) ) ;
#47449 = CIRCLE ( 'NONE', #642, 82.00000000000000000 ) ;
#47450 = LINE ( 'NONE', #25621, #46191 ) ;
#47451 = CARTESIAN_POINT ( 'NONE',  ( 11.99999999999999822, -26.01480285779885904, 70.53064760720306481 ) ) ;
#47452 = DIRECTION ( 'NONE',  ( -1.000000000000000000, -0.000000000000000000, 0.000000000000000000 ) ) ;
#47453 = FACE_OUTER_BOUND ( 'NONE', #33745, .T. ) ;
#47454 = CARTESIAN_POINT ( 'NONE',  ( 0.000000000000000000, 0.000000000000000000, 0.000000000000000000 ) ) ;
#47455 = CARTESIAN_POINT ( 'NONE',  ( 0.000000000000000000, 0.000000000000000000, 0.000000000000000000 ) ) ;
#47456 = CARTESIAN_POINT ( 'NONE',  ( -93.84685191531248449, -208.0026889286704943, 83.08114583420048405 ) ) ;
#47457 = CARTESIAN_POINT ( 'NONE',  ( -95.00000000000002842, 92.66308142843932671, 82.65781250086715204 ) ) ;
#47458 = ORIENTED_EDGE ( 'NONE', *, *, #62755, .T. ) ;
#47459 = EDGE_CURVE ( 'NONE', #45520, #27660, #61382, .T. ) ;
#47460 = CARTESIAN_POINT ( 'NONE',  ( 92.69370383062498320, 91.33154071421968467, 79.42989583420046529 ) ) ;
#47461 = ORIENTED_EDGE ( 'NONE', *, *, #22833, .T. ) ;
#47462 = LINE ( 'NONE', #70370, #62332 ) ;
#47464 = CIRCLE ( 'NONE', #22241, 77.49900000000000944 ) ;
#47463 = DIRECTION ( 'NONE',  ( -1.000000000000000000, -0.000000000000000000, -0.000000000000000000 ) ) ;
#47466 = EDGE_CURVE ( 'NONE', #67844, #65764, #52446, .T. ) ;
#47465 = CARTESIAN_POINT ( 'NONE',  ( -92.34999999999999432, -209.9999999999999716, 83.41187500173430180 ) ) ;
#47467 = LINE ( 'NONE', #1645, #67957 ) ;
#47468 = FACE_OUTER_BOUND ( 'NONE', #44662, .T. ) ;
#47469 = CARTESIAN_POINT ( 'NONE',  ( -92.69370383062498320, -208.6684592857803295, 83.02822916753379445 ) ) ;
#47470 = CARTESIAN_POINT ( 'NONE',  ( 10.00000000000000000, 0.000000000000000000, 0.000000000000000000 ) ) ;
#47471 = CYLINDRICAL_SURFACE ( 'NONE', #55466, 37.49900000000000233 ) ;
#47472 = DIRECTION ( 'NONE',  ( -0.000000000000000000, -0.000000000000000000, -1.000000000000000000 ) ) ;
#47473 = EDGE_CURVE ( 'NONE', #32411, #49261, #45745, .T. ) ;
#47474 = VECTOR ( 'NONE', #73564, 1000.000000000000000 ) ;
#47475 = CARTESIAN_POINT ( 'NONE',  ( 94.99999999999998579, 90.00000000000002842, 90.00000000000000000 ) ) ;
#47476 = ORIENTED_EDGE ( 'NONE', *, *, #61385, .T. ) ;
#47477 = VERTEX_POINT ( 'NONE', #29146 ) ;
#47478 = DIRECTION ( 'NONE',  ( -0.000000000000000000, -0.000000000000000000, -1.000000000000000000 ) ) ;
#47479 = DIRECTION ( 'NONE',  ( 2.603472992746261562E-14, 2.546204323184492723E-14, -1.000000000000000000 ) ) ;
#47480 = EDGE_CURVE ( 'NONE', #17553, #42918, #69745, .T. ) ;
#47481 = CARTESIAN_POINT ( 'NONE',  ( -92.69370383062504004, 90.00000000000004263, 88.05531250086713158 ) ) ;
#47482 = CARTESIAN_POINT ( 'NONE',  ( 10.00000000000000000, 40.98264845739749518, 9.188173127307441845 ) ) ;
#47483 = DIRECTION ( 'NONE',  ( 1.000000000000000000, 0.000000000000000000, 0.000000000000000000 ) ) ;
#47484 = DIRECTION ( 'NONE',  ( -1.000000000000000000, 0.000000000000000000, -0.000000000000000000 ) ) ;
#47485 = CARTESIAN_POINT ( 'NONE',  ( 0.000000000000000000, 59.46389618801964616, 49.70050353004909738 ) ) ;
#47486 =( BOUNDED_CURVE ( )  B_SPLINE_CURVE ( 2, ( #51407, #56325, #51044, #44296, #68723, #50666, #10831 ),
 .UNSPECIFIED., .F., .F. ) 
 B_SPLINE_CURVE_WITH_KNOTS ( ( 3, 2, 2, 3 ),
 ( 0.1458333333333334536, 0.1527777777777778734, 0.1597222222222222654, 0.1666666666666666852 ),
 .UNSPECIFIED. ) 
 CURVE ( )  GEOMETRIC_REPRESENTATION_ITEM ( )  RATIONAL_B_SPLINE_CURVE ( ( 0.9999999999999978906, 0.8660254037844408170, 1.000000000000000000, 0.8660254037844387076, 1.000000000000000000, 0.8660254037844381525, 1.000000000000000444 ) ) 
 REPRESENTATION_ITEM ( '' )  );
#47487 = ORIENTED_EDGE ( 'NONE', *, *, #13167, .T. ) ;
#47488 = DIRECTION ( 'NONE',  ( 0.4796670183876304283, -0.8774505977381978905, 0.000000000000000000 ) ) ;
#47489 = VECTOR ( 'NONE', #58755, 1000.000000000000000 ) ;
#47490 = EDGE_CURVE ( 'NONE', #26473, #3895, #13340, .T. ) ;
#47491 = DIRECTION ( 'NONE',  ( -1.000000000000000000, 0.000000000000000000, -0.000000000000000000 ) ) ;
#47492 = DIRECTION ( 'NONE',  ( -1.000000000000000000, -0.000000000000000000, 0.000000000000000000 ) ) ;
#47493 = CARTESIAN_POINT ( 'NONE',  ( -22.53294031248082163, -134.0273518838794757, 5.500000000000000000 ) ) ;
#47494 = AXIS2_PLACEMENT_3D ( 'NONE', #38817, #61756, #32422 ) ;
#47495 = CARTESIAN_POINT ( 'NONE',  ( 11.99999999999999822, 0.000000000000000000, 0.000000000000000000 ) ) ;
#47496 = CARTESIAN_POINT ( 'NONE',  ( -93.84685191531247028, -211.9973110713294489, 86.20322916753382003 ) ) ;
#47497 =( LENGTH_UNIT ( ) NAMED_UNIT ( * ) SI_UNIT ( .MILLI., .METRE. ) );
#47498 = DIRECTION ( 'NONE',  ( -1.000000000000000000, 0.000000000000000000, -0.000000000000000000 ) ) ;
#47499 = LINE ( 'NONE', #25672, #16621 ) ;
#47500 = CARTESIAN_POINT ( 'NONE',  ( -93.84685191531247028, -211.9973110713294489, 77.31322916753381946 ) ) ;
#47501 = DIRECTION ( 'NONE',  ( 1.000000000000000000, 0.000000000000000000, 0.000000000000000000 ) ) ;
#47502 = VERTEX_POINT ( 'NONE', #63758 ) ;
#47503 = CARTESIAN_POINT ( 'NONE',  ( -2.499999999999965361, 90.00000000000000000, -90.00000000000000000 ) ) ;
#47504 = LINE ( 'NONE', #30933, #27438 ) ;
#47505 = CARTESIAN_POINT ( 'NONE',  ( -97.64999247309856401, 88.47001744098896836, 88.22729196900364457 ) ) ;
#47506 = FACE_OUTER_BOUND ( 'NONE', #36786, .T. ) ;
#47507 = CARTESIAN_POINT ( 'NONE',  ( 92.69370383062501162, -208.6684592857803011, 78.15989583420048348 ) ) ;
#47508 = ORIENTED_EDGE ( 'NONE', *, *, #56037, .F. ) ;
#47509 = CARTESIAN_POINT ( 'NONE',  ( 5.000000000000000000, -77.16300072079641836, -27.74655509720751567 ) ) ;
#47510 = DIRECTION ( 'NONE',  ( 0.000000000000000000, 0.3826834323650904479, -0.9238795325112865164 ) ) ;
#47511 = VERTEX_POINT ( 'NONE', #6603 ) ;
#47512 = DIRECTION ( 'NONE',  ( -1.000000000000000000, 0.000000000000000000, 0.000000000000000000 ) ) ;
#47513 = VECTOR ( 'NONE', #43779, 1000.000000000000000 ) ;
#47514 = VERTEX_POINT ( 'NONE', #18606 ) ;
#47515 = EDGE_CURVE ( 'NONE', #16806, #57541, #52086, .T. ) ;
#47516 = FACE_OUTER_BOUND ( 'NONE', #70076, .T. ) ;
#47517 = EDGE_CURVE ( 'NONE', #49481, #55130, #40436, .T. ) ;
#47518 = ORIENTED_EDGE ( 'NONE', *, *, #15255, .T. ) ;
#47519 = ORIENTED_EDGE ( 'NONE', *, *, #58712, .F. ) ;
#47520 = AXIS2_PLACEMENT_3D ( 'NONE', #62287, #43883, #27302 ) ;
#47522 = ORIENTED_EDGE ( 'NONE', *, *, #48535, .F. ) ;
#47521 = EDGE_CURVE ( 'NONE', #53901, #4438, #73321, .T. ) ;
#47523 = EDGE_CURVE ( 'NONE', #21232, #74280, #64483, .T. ) ;
#47524 = DIRECTION ( 'NONE',  ( 0.000000000000000000, 0.000000000000000000, -1.000000000000000000 ) ) ;
#47525 = ORIENTED_EDGE ( 'NONE', *, *, #52508, .F. ) ;
#47526 = CIRCLE ( 'NONE', #13912, 31.99999999999998579 ) ;
#47527 = AXIS2_PLACEMENT_3D ( 'NONE', #18156, #65145, #58757 ) ;
#47528 = VERTEX_POINT ( 'NONE', #46088 ) ;
#47529 = CARTESIAN_POINT ( 'NONE',  ( 92.69370383062498320, 88.66845928578037217, 78.42447916753380355 ) ) ;
#47530 = LINE ( 'NONE', #18212, #26386 ) ;
#47531 = CARTESIAN_POINT ( 'NONE',  ( 96.32499999999998863, -207.7050326799711968, 75.81833333333332803 ) ) ;
#47532 = ORIENTED_EDGE ( 'NONE', *, *, #23089, .F. ) ;
#47533 = ORIENTED_EDGE ( 'NONE', *, *, #70589, .F. ) ;
#47534 = ORIENTED_EDGE ( 'NONE', *, *, #62909, .T. ) ;
#47535 = CARTESIAN_POINT ( 'NONE',  ( 0.000000000000000000, 46.21855187248630159, 62.20884554314034176 ) ) ;
#47536 = ORIENTED_EDGE ( 'NONE', *, *, #27639, .T. ) ;
#47537 = CARTESIAN_POINT ( 'NONE',  ( -120.0000000000000000, -119.9999999999999858, 36.50000000000000711 ) ) ;
#47538 = DIRECTION ( 'NONE',  ( -1.000000000000000000, -0.000000000000000000, 0.000000000000000000 ) ) ;
#47539 = AXIS2_PLACEMENT_3D ( 'NONE', #71068, #24483, #7927 ) ;
#47540 = DIRECTION ( 'NONE',  ( -2.603472992746261562E-14, -2.546204323184492723E-14, 1.000000000000000000 ) ) ;
#47541 = EDGE_CURVE ( 'NONE', #45606, #31921, #57363, .T. ) ;
#47542 = LINE ( 'NONE', #2086, #73480 ) ;
#47543 = DIRECTION ( 'NONE',  ( -1.000000000000000000, -0.000000000000000000, -0.000000000000000000 ) ) ;
#47544 = FACE_OUTER_BOUND ( 'NONE', #71480, .T. ) ;
#47545 = ADVANCED_FACE ( 'NONE', ( #58847 ), #7345, .T. ) ;
#47546 = CARTESIAN_POINT ( 'NONE',  ( 97.65000000000004832, 91.52997821335250705, 77.67041666666666799 ) ) ;
#47547 = CARTESIAN_POINT ( 'NONE',  ( -93.67499999999998295, -212.2949673200287179, 78.22604166840096696 ) ) ;
#47548 = DIRECTION ( 'NONE',  ( -1.000000000000000000, -0.000000000000000000, -0.000000000000000000 ) ) ;
#47550 = CARTESIAN_POINT ( 'NONE',  ( -93.67500000000003979, 92.29496732002878900, 75.89770833506763381 ) ) ;
#47549 = CARTESIAN_POINT ( 'NONE',  ( 92.34999999999999432, 90.00000000000002842, 74.83937500173429669 ) ) ;
#47551 = EDGE_LOOP ( 'NONE', ( #45613, #36002, #47079, #36419 ) ) ;
#47552 = CARTESIAN_POINT ( 'NONE',  ( 97.30629616937498838, 91.33154071421968467, 77.47197916753381719 ) ) ;
#47553 = CARTESIAN_POINT ( 'NONE',  ( 0.000000000000000000, -33.79645857604525361, 16.45098606841114730 ) ) ;
#47554 = DIRECTION ( 'NONE',  ( -1.000000000000000000, -0.000000000000000000, 0.000000000000000000 ) ) ;
#47555 = CARTESIAN_POINT ( 'NONE',  ( 0.000000000000000000, 0.000000000000000000, 0.000000000000000000 ) ) ;
#47556 = CARTESIAN_POINT ( 'NONE',  ( -92.35000000000003695, 89.99999989488615881, 86.58687499784845443 ) ) ;
#47557 = FACE_OUTER_BOUND ( 'NONE', #17737, .T. ) ;
#47558 = EDGE_LOOP ( 'NONE', ( #43770, #22828, #13778, #28648, #40355 ) ) ;
#47559 = DIRECTION ( 'NONE',  ( -0.000000000000000000, -0.000000000000000000, -1.000000000000000000 ) ) ;
#47560 = ADVANCED_FACE ( 'NONE', ( #24624 ), #70466, .F. ) ;
#47561 = ADVANCED_FACE ( 'NONE', ( #6246 ), #28787, .F. ) ;
#47562 = CARTESIAN_POINT ( 'NONE',  ( 97.64999999999997726, 90.00000000000002842, 90.00000000000000000 ) ) ;
#47563 = VERTEX_POINT ( 'NONE', #69022 ) ;
#47564 = EDGE_LOOP ( 'NONE', ( #12551, #11389, #23315, #48793 ) ) ;
#47565 = CARTESIAN_POINT ( 'NONE',  ( -93.07557990970624928, -211.8218417373838065, 75.00000000000000000 ) ) ;
#47566 = CARTESIAN_POINT ( 'NONE',  ( -3.000000000000000000, -22.67460108101783334, 6.353146135317912169 ) ) ;
#47567 = LINE ( 'NONE', #18979, #6375 ) ;
#47568 = LINE ( 'NONE', #1748, #6554 ) ;
#47569 = CARTESIAN_POINT ( 'NONE',  ( -94.99999999999997158, -207.3369185715606307, 76.94281250086714863 ) ) ;
#47570 = AXIS2_PLACEMENT_3D ( 'NONE', #44884, #74179, #61055 ) ;
#47571 = ORIENTED_EDGE ( 'NONE', *, *, #9348, .F. ) ;
#47572 = DIRECTION ( 'NONE',  ( 0.000000000000000000, 0.000000000000000000, 1.000000000000000000 ) ) ;
#47573 = DIRECTION ( 'NONE',  ( -1.000000000000000000, 0.000000000000000000, -0.000000000000000000 ) ) ;
#47574 = AXIS2_PLACEMENT_3D ( 'NONE', #5765, #28671, #45985 ) ;
#47575 = DIRECTION ( 'NONE',  ( 1.000000000000000000, -0.000000000000000000, 0.000000000000000000 ) ) ;
#47576 = CYLINDRICAL_SURFACE ( 'NONE', #65350, 31.99999999999997868 ) ;
#47577 = CYLINDRICAL_SURFACE ( 'NONE', #4881, 82.00000000000000000 ) ;
#47578 = CIRCLE ( 'NONE', #57193, 1.000000000000000000 ) ;
#47579 = CYLINDRICAL_SURFACE ( 'NONE', #20569, 2.649999999999985700 ) ;
#47580 = CARTESIAN_POINT ( 'NONE',  ( 92.34999999999999432, 91.52997821335252127, 86.21645833506764234 ) ) ;
#47581 = DIRECTION ( 'NONE',  ( -1.000000000000000000, -0.000000000000000000, 0.000000000000000000 ) ) ;
#47582 = LINE ( 'NONE', #70487, #43072 ) ;
#47583 = CIRCLE ( 'NONE', #36777, 32.00000000000000000 ) ;
#47584 = CARTESIAN_POINT ( 'NONE',  ( 96.15314808468748708, 88.00268892867053694, 82.39322916753381776 ) ) ;
#47585 = CARTESIAN_POINT ( 'NONE',  ( -97.30629616937495996, -209.9999999999999716, 86.62656250086715204 ) ) ;
#47586 = DIRECTION ( 'NONE',  ( -0.000000000000000000, 0.000000000000000000, 1.000000000000000000 ) ) ;
#47587 = ORIENTED_EDGE ( 'NONE', *, *, #73727, .F. ) ;
#47588 = CARTESIAN_POINT ( 'NONE',  ( 97.65000000000000568, -211.5299782133524218, 83.35895833506764063 ) ) ;
#47589 = CARTESIAN_POINT ( 'NONE',  ( -92.34999999999999432, -209.9999999999999716, 80.79249999999998977 ) ) ;
#47590 = CARTESIAN_POINT ( 'NONE',  ( -93.84685191531252713, 88.00268892867056536, 75.88447916753381151 ) ) ;
#47591 = AXIS2_PLACEMENT_3D ( 'NONE', #8202, #9314, #54444 ) ;
#47592 = CARTESIAN_POINT ( 'NONE',  ( 93.84685191531251292, -211.9973110713294489, 86.57364583420047666 ) ) ;
#47593 = ORIENTED_EDGE ( 'NONE', *, *, #14846, .F. ) ;
#47594 = VERTEX_POINT ( 'NONE', #46451 ) ;
#47595 = ORIENTED_EDGE ( 'NONE', *, *, #46795, .T. ) ;
#47596 = EDGE_CURVE ( 'NONE', #3278, #1800, #17386, .T. ) ;
#47597 = CARTESIAN_POINT ( 'NONE',  ( 96.32499999999998863, -212.2949673200287179, 75.60666666666665492 ) ) ;
#47598 = DIRECTION ( 'NONE',  ( 0.000000000000000000, -0.3090169943749548342, 0.9510565162951511997 ) ) ;
#47599 = EDGE_CURVE ( 'NONE', #53775, #56493, #42167, .T. ) ;
#47600 = ORIENTED_EDGE ( 'NONE', *, *, #28333, .F. ) ;
#47601 = ORIENTED_EDGE ( 'NONE', *, *, #23573, .T. ) ;
#47602 = CARTESIAN_POINT ( 'NONE',  ( 2.874421927457452952, -143.3717286177755739, 2.500000000000000000 ) ) ;
#47603 = EDGE_CURVE ( 'NONE', #54492, #9345, #14819, .T. ) ;
#47604 = CARTESIAN_POINT ( 'NONE',  ( 96.15314808468748708, -208.0026889286704943, 81.33489583420049485 ) ) ;
#47605 = CARTESIAN_POINT ( 'NONE',  ( -97.64999999999996305, -209.9999999999999716, 81.10999999999999943 ) ) ;
#47606 = CARTESIAN_POINT ( 'NONE',  ( 92.34999999999988063, 91.52997821335246442, 81.05708333333332405 ) ) ;
#47607 = DIRECTION ( 'NONE',  ( 0.000000000000000000, 0.000000000000000000, 1.000000000000000000 ) ) ;
#47608 = LINE ( 'NONE', #2893, #14671 ) ;
#47609 = EDGE_CURVE ( 'NONE', #55850, #38100, #4904, .T. ) ;
#47610 = VECTOR ( 'NONE', #35363, 1000.000000000000000 ) ;
#47611 = DIRECTION ( 'NONE',  ( -1.000000000000000000, 0.000000000000000000, 0.000000000000000000 ) ) ;
#47612 = CARTESIAN_POINT ( 'NONE',  ( 93.67500000000001137, -207.7050326799711968, 85.44916666666665606 ) ) ;
#47613 = VECTOR ( 'NONE', #53443, 1000.000000000000114 ) ;
#47614 = ORIENTED_EDGE ( 'NONE', *, *, #12632, .F. ) ;
#47615 = EDGE_LOOP ( 'NONE', ( #11323, #65830, #51049, #71735 ) ) ;
#47616 = ORIENTED_EDGE ( 'NONE', *, *, #20653, .F. ) ;
#47617 = VERTEX_POINT ( 'NONE', #71208 ) ;
#47618 = CARTESIAN_POINT ( 'NONE',  ( -97.64999999999996305, -209.9999999999999716, 90.00000000000000000 ) ) ;
#47619 =( NAMED_UNIT ( * ) PLANE_ANGLE_UNIT ( ) SI_UNIT ( $, .RADIAN. ) );
#47620 = CARTESIAN_POINT ( 'NONE',  ( -95.00000000000002842, 87.33691857156074434, 88.69031250086716511 ) ) ;
#47621 = VECTOR ( 'NONE', #6871, 1000.000000000000000 ) ;
#47622 = CARTESIAN_POINT ( 'NONE',  ( 0.000000000000000000, 27.05870788708267582, -26.08949754952995903 ) ) ;
#47623 = DIRECTION ( 'NONE',  ( -1.000000000000000000, -0.000000000000000000, -0.000000000000000000 ) ) ;
#47624 = CARTESIAN_POINT ( 'NONE',  ( 95.00000000000000000, -212.6630814284392557, 87.26156250086714294 ) ) ;
#47625 = FACE_OUTER_BOUND ( 'NONE', #3817, .T. ) ;
#47626 = EDGE_CURVE ( 'NONE', #14636, #33066, #8454, .T. ) ;
#47627 = ORIENTED_EDGE ( 'NONE', *, *, #13717, .F. ) ;
#47628 = LINE ( 'NONE', #30693, #44365 ) ;
#47629 = VERTEX_POINT ( 'NONE', #18970 ) ;
#47630 = EDGE_CURVE ( 'NONE', #29668, #67669, #37345, .T. ) ;
#47631 = FACE_OUTER_BOUND ( 'NONE', #41934, .T. ) ;
#47632 = VECTOR ( 'NONE', #25927, 1000.000000000000000 ) ;
#47633 = EDGE_LOOP ( 'NONE', ( #23339, #54738, #10757, #43393 ) ) ;
#47634 = CARTESIAN_POINT ( 'NONE',  ( -93.67500000000003979, 87.70503267997129626, 86.48104166840096241 ) ) ;
#47635 = CARTESIAN_POINT ( 'NONE',  ( 96.15314808468748708, 88.00268892867053694, 89.37822916753381719 ) ) ;
#47636 = ORIENTED_EDGE ( 'NONE', *, *, #31300, .T. ) ;
#47637 = CARTESIAN_POINT ( 'NONE',  ( 0.000000000000000000, -12.26510123303284594, 35.53030884539080603 ) ) ;
#47638 = CARTESIAN_POINT ( 'NONE',  ( -0.2999999999999964362, 0.000000000000000000, -12.80000000000000071 ) ) ;
#47639 = DIRECTION ( 'NONE',  ( 0.000000000000000000, 0.000000000000000000, 1.000000000000000000 ) ) ;
#47640 = CARTESIAN_POINT ( 'NONE',  ( -7.399999999999993250, 1.306591983238623146E-13, 13.10000000000023057 ) ) ;
#47641 = VERTEX_POINT ( 'NONE', #24991 ) ;
#47642 = CARTESIAN_POINT ( 'NONE',  ( 10.00000000000000000, -72.35160999960831418, 20.41045688087797672 ) ) ;
#47643 = EDGE_CURVE ( 'NONE', #51502, #41287, #4937, .T. ) ;
#47644 = EDGE_CURVE ( 'NONE', #2055, #41798, #15701, .T. ) ;
#47645 = CARTESIAN_POINT ( 'NONE',  ( -94.99999999999997158, -212.6630814284392557, 75.83156250086715033 ) ) ;
#47646 = ORIENTED_EDGE ( 'NONE', *, *, #28367, .F. ) ;
#47647 = AXIS2_PLACEMENT_3D ( 'NONE', #47692, #19120, #42068 ) ;
#47648 = EDGE_LOOP ( 'NONE', ( #69230, #56597, #30074, #5689 ) ) ;
#47649 = CARTESIAN_POINT ( 'NONE',  ( 0.000000000000000000, -32.34446384429989507, 26.79245525562703278 ) ) ;
#47650 = AXIS2_PLACEMENT_3D ( 'NONE', #132, #12095, #62517 ) ;
#47651 = CARTESIAN_POINT ( 'NONE',  ( -10.00000000000000000, 0.000000000000000000, 0.000000000000000000 ) ) ;
#47652 = DIRECTION ( 'NONE',  ( 1.000000000000000000, 0.000000000000000000, 0.000000000000000000 ) ) ;
#47653 = CARTESIAN_POINT ( 'NONE',  ( -97.30629616937497417, -211.3315407142195852, 86.67947916753382742 ) ) ;
#47654 = ORIENTED_EDGE ( 'NONE', *, *, #71813, .F. ) ;
#47655 = CARTESIAN_POINT ( 'NONE',  ( -96.32499999999996021, -212.2949673200287179, 82.48583333333333201 ) ) ;
#47656 = VERTEX_POINT ( 'NONE', #54315 ) ;
#47657 = ORIENTED_EDGE ( 'NONE', *, *, #73567, .T. ) ;
#47658 = CARTESIAN_POINT ( 'NONE',  ( 97.64999999999999147, 89.99999997442942856, 84.04687500080852658 ) ) ;
#47659 = CARTESIAN_POINT ( 'NONE',  ( 10.00000000000000000, -16.23288003029521320, 33.80338159004277543 ) ) ;
#47660 = CARTESIAN_POINT ( 'NONE',  ( 94.99999999999998579, 92.66308142843932671, 79.95906250086713385 ) ) ;
#47661 = FACE_OUTER_BOUND ( 'NONE', #2078, .T. ) ;
#47662 = CARTESIAN_POINT ( 'NONE',  ( 10.00000000000000000, 79.10210256391367523, 21.60688246758613218 ) ) ;
#47663 = CARTESIAN_POINT ( 'NONE',  ( -95.00000000000002842, 93.05995642670504253, 80.95125000000000171 ) ) ;
#47664 = DIRECTION ( 'NONE',  ( 1.000000000000000000, 0.000000000000000000, 0.000000000000000000 ) ) ;
#47665 = CARTESIAN_POINT ( 'NONE',  ( 0.000000000000000000, 0.000000000000000000, -6.000000000000000000 ) ) ;
#47666 = DIRECTION ( 'NONE',  ( -0.000000000000000000, 0.000000000000000000, -1.000000000000000000 ) ) ;
#47667 = DIRECTION ( 'NONE',  ( -1.000000000000000000, -1.390371824233641368E-16, 0.000000000000000000 ) ) ;
#47668 = AXIS2_PLACEMENT_3D ( 'NONE', #17978, #6699, #22517 ) ;
#47669 = CARTESIAN_POINT ( 'NONE',  ( 92.35000000000000853, -210.0000359324574788, 85.63437624451400154 ) ) ;
#47670 = CIRCLE ( 'NONE', #30808, 77.49899999999999523 ) ;
#47671 = CARTESIAN_POINT ( 'NONE',  ( 11.99999999999999822, 76.66974797899837313, 11.30684508768366747 ) ) ;
#47672 = ORIENTED_EDGE ( 'NONE', *, *, #23285, .T. ) ;
#47673 = CARTESIAN_POINT ( 'NONE',  ( -97.30629616937501680, 90.00000000000004263, 85.83281250086714920 ) ) ;
#47674 = DIRECTION ( 'NONE',  ( -1.000000000000000000, 0.000000000000000000, -0.000000000000000000 ) ) ;
#47675 = CIRCLE ( 'NONE', #44084, 32.00000000000000000 ) ;
#47676 = ADVANCED_FACE ( 'NONE', ( #26470 ), #36639, .F. ) ;
#47677 = ADVANCED_FACE ( 'NONE', ( #2105 ), #47927, .T. ) ;
#47678 = DIRECTION ( 'NONE',  ( 1.000000000000000000, -0.000000000000000000, -0.000000000000000000 ) ) ;
#47679 = EDGE_CURVE ( 'NONE', #12399, #17939, #31735, .T. ) ;
#47680 = VERTEX_POINT ( 'NONE', #54678 ) ;
#47681 =( BOUNDED_CURVE ( )  B_SPLINE_CURVE ( 2, ( #55716, #56475, #67743, #54971, #4232, #27509, #21121, #50443, #49687, #73365, #4980 ),
 .UNSPECIFIED., .F., .F. ) 
 B_SPLINE_CURVE_WITH_KNOTS ( ( 3, 2, 2, 2, 2, 3 ),
 ( 0.04233441017594471306, 0.04233459324529428858, 0.04939035878617635544, 0.05644612432705840843, 0.06350188986794047530, 0.06350193517735297499 ),
 .UNSPECIFIED. ) 
 CURVE ( )  GEOMETRIC_REPRESENTATION_ITEM ( )  RATIONAL_B_SPLINE_CURVE ( ( 0.9999930479532868066, 0.9999965238864518824, 1.000000000000000000, 0.8660254037844387076, 1.000000000000000000, 0.8660254037844387076, 1.000000000000000000, 0.8660254037844387076, 1.000000000000000000, 0.9999991396666727539, 0.9999982793443948914 ) ) 
 REPRESENTATION_ITEM ( '' )  );
#47682 = CYLINDRICAL_SURFACE ( 'NONE', #22245, 82.00000000000000000 ) ;
#47683 = CARTESIAN_POINT ( 'NONE',  ( 50.00005079999999680, 0.000000000000000000, 21.00000000000000000 ) ) ;
#47684 = DIRECTION ( 'NONE',  ( 0.000000000000000000, 0.000000000000000000, 1.000000000000000000 ) ) ;
#47685 = EDGE_CURVE ( 'NONE', #30100, #18341, #10927, .T. ) ;
#47686 = CYLINDRICAL_SURFACE ( 'NONE', #41610, 77.49899999999999523 ) ;
#47687 = CARTESIAN_POINT ( 'NONE',  ( 92.69370383062501162, -211.3315407142195852, 80.96447916753382401 ) ) ;
#47688 = AXIS2_PLACEMENT_3D ( 'NONE', #43476, #54363, #31421 ) ;
#47689 = EDGE_CURVE ( 'NONE', #968, #19228, #49405, .T. ) ;
#47690 = ORIENTED_EDGE ( 'NONE', *, *, #16842, .F. ) ;
#47691 = ORIENTED_EDGE ( 'NONE', *, *, #35296, .T. ) ;
#47692 = CARTESIAN_POINT ( 'NONE',  ( 0.000000000000000000, 0.000000000000000000, 0.000000000000000000 ) ) ;
#47693 = ORIENTED_EDGE ( 'NONE', *, *, #13143, .F. ) ;
#47694 = DIRECTION ( 'NONE',  ( 0.000000000000000000, 0.000000000000000000, 1.000000000000000000 ) ) ;
#47695 = CARTESIAN_POINT ( 'NONE',  ( 95.00000000000000000, -207.3369185715606307, 76.14906250086716000 ) ) ;
#47696 = ADVANCED_FACE ( 'NONE', ( #30620 ), #19715, .T. ) ;
#47697 = VERTEX_POINT ( 'NONE', #59585 ) ;
#47698 = CARTESIAN_POINT ( 'NONE',  ( 92.69370383062501162, -211.3315407142195852, 80.96447916753382401 ) ) ;
#47699 = ORIENTED_EDGE ( 'NONE', *, *, #42954, .F. ) ;
#47700 = CARTESIAN_POINT ( 'NONE',  ( 0.000000000000000000, 0.000000000000000000, 0.000000000000000000 ) ) ;
#47701 = ORIENTED_EDGE ( 'NONE', *, *, #54061, .T. ) ;
#47702 = ORIENTED_EDGE ( 'NONE', *, *, #50042, .T. ) ;
#47703 = PLANE ( 'NONE',  #66980 ) ;
#47704 = CARTESIAN_POINT ( 'NONE',  ( 12.00000000000000000, 18.84667830672605859, 18.68964196561243085 ) ) ;
#47705 = ORIENTED_EDGE ( 'NONE', *, *, #69333, .F. ) ;
#47706 = DIRECTION ( 'NONE',  ( 1.000000000000000000, 0.000000000000000000, 0.000000000000000000 ) ) ;
#47707 = CARTESIAN_POINT ( 'NONE',  ( 95.00000000000000000, -213.0599564267049857, 82.61812500173428475 ) ) ;
#47708 = CARTESIAN_POINT ( 'NONE',  ( 94.99999999999998579, 93.05995642670504253, 87.93625000000000114 ) ) ;
#47709 = EDGE_CURVE ( 'NONE', #13922, #9966, #6176, .T. ) ;
#47710 = EDGE_LOOP ( 'NONE', ( #56606, #29805, #25442, #49777 ) ) ;
#47711 = DIRECTION ( 'NONE',  ( 0.000000000000000000, -1.065814103640131346E-14, -1.000000000000000000 ) ) ;
#47712 = ADVANCED_FACE ( 'NONE', ( #11044 ), #67061, .F. ) ;
#47713 = LINE ( 'NONE', #31524, #24890 ) ;
#47714 = VERTEX_POINT ( 'NONE', #73059 ) ;
#47715 = VERTEX_POINT ( 'NONE', #44521 ) ;
#47716 = CARTESIAN_POINT ( 'NONE',  ( -93.84685191531254134, 91.99731107132950569, 88.95489583420049939 ) ) ;
#47717 = CARTESIAN_POINT ( 'NONE',  ( 92.69370383062498320, 90.00000000000002842, 85.83281250086714920 ) ) ;
#47718 = VERTEX_POINT ( 'NONE', #49763 ) ;
#47720 = CARTESIAN_POINT ( 'NONE',  ( 96.32499999999997442, 92.29496732002878900, 85.42270833506762528 ) ) ;
#47719 = AXIS2_PLACEMENT_3D ( 'NONE', #35344, #17306, #29311 ) ;
#47721 = ORIENTED_EDGE ( 'NONE', *, *, #17726, .F. ) ;
#47722 = DIRECTION ( 'NONE',  ( -1.000000000000000000, 0.000000000000000000, 0.000000000000000000 ) ) ;
#47723 = LINE ( 'NONE', #60415, #36610 ) ;
#47724 = EDGE_LOOP ( 'NONE', ( #57974, #4846, #43196, #14112 ) ) ;
#47725 = ORIENTED_EDGE ( 'NONE', *, *, #48790, .T. ) ;
#47726 = AXIS2_PLACEMENT_3D ( 'NONE', #19721, #13348, #59977 ) ;
#47727 = ORIENTED_EDGE ( 'NONE', *, *, #51700, .F. ) ;
#47728 = VECTOR ( 'NONE', #13635, 1000.000000000000000 ) ;
#47729 = FACE_OUTER_BOUND ( 'NONE', #38414, .T. ) ;
#47730 = DIRECTION ( 'NONE',  ( -0.8541291221503275466, 0.5200609990132993854, 0.000000000000000000 ) ) ;
#47731 = CARTESIAN_POINT ( 'NONE',  ( -95.00000000000002842, 86.94004357329504273, 84.44375000000000853 ) ) ;
#47732 = VERTEX_POINT ( 'NONE', #4309 ) ;
#47733 = CARTESIAN_POINT ( 'NONE',  ( 92.35000000000000853, 88.47002178664752137, 81.79791666666665151 ) ) ;
#47734 = FACE_OUTER_BOUND ( 'NONE', #71074, .T. ) ;
#47735 = EDGE_LOOP ( 'NONE', ( #71470, #50981 ) ) ;
#47736 = DIRECTION ( 'NONE',  ( -1.000000000000000000, 5.236901059551556403E-15, 2.618450529775778123E-14 ) ) ;
#47737 = CARTESIAN_POINT ( 'NONE',  ( -92.69370383062498320, -208.6684592857803011, 83.02822916753379445 ) ) ;
#47738 = ORIENTED_EDGE ( 'NONE', *, *, #49410, .T. ) ;
#47739 = DIRECTION ( 'NONE',  ( -1.000000000000000000, -0.000000000000000000, 0.000000000000000000 ) ) ;
#47740 = DIRECTION ( 'NONE',  ( 0.000000000000000000, -0.8910065241883723397, 0.4539904997395382003 ) ) ;
#47741 = CARTESIAN_POINT ( 'NONE',  ( 6.377742925735834234, -145.7647898336707897, -2.500000000000000000 ) ) ;
#47742 = CARTESIAN_POINT ( 'NONE',  ( 0.000000000000000000, 0.000000000000000000, 0.000000000000000000 ) ) ;
#47743 = CARTESIAN_POINT ( 'NONE',  ( 0.000000000000000000, -41.91543099594816368, -2.663952781846588014 ) ) ;
#47744 = AXIS2_PLACEMENT_3D ( 'NONE', #66117, #2978, #2624 ) ;
#47745 =( NAMED_UNIT ( * ) SI_UNIT ( $, .STERADIAN. ) SOLID_ANGLE_UNIT ( ) );
#47746 = DIRECTION ( 'NONE',  ( -1.000000000000000000, 0.000000000000000000, -0.000000000000000000 ) ) ;
#47747 = CARTESIAN_POINT ( 'NONE',  ( 96.66135172262730180, -211.6008015735635865, 74.79754476654878204 ) ) ;
#47748 = CARTESIAN_POINT ( 'NONE',  ( 92.35000000046503033, 89.99996900126896548, 83.09538598081184091 ) ) ;
#47749 = DIRECTION ( 'NONE',  ( 0.000000000000000000, -0.000000000000000000, -1.000000000000000000 ) ) ;
#47750 = EDGE_CURVE ( 'NONE', #70108, #36401, #59019, .T. ) ;
#47751 = CARTESIAN_POINT ( 'NONE',  ( -95.00000000000002842, 87.33691857156074434, 75.83156250086715033 ) ) ;
#47752 = DIRECTION ( 'NONE',  ( -1.000000000000000000, 0.000000000000000000, 0.000000000000000000 ) ) ;
#47753 = FACE_OUTER_BOUND ( 'NONE', #15559, .T. ) ;
#47754 = AXIS2_PLACEMENT_3D ( 'NONE', #50065, #10227, #17356 ) ;
#47755 = DIRECTION ( 'NONE',  ( -1.000000000000000000, 0.000000000000000000, 0.000000000000000000 ) ) ;
#47756 = DIRECTION ( 'NONE',  ( 0.6064928550163524168, 0.7950889364178788110, 0.000000000000000000 ) ) ;
#47757 = CARTESIAN_POINT ( 'NONE',  ( 10.00000000000000000, -5.256550761632340141, -77.32052557432847095 ) ) ;
#47758 = LINE ( 'NONE', #65442, #13096 ) ;
#47759 = DIRECTION ( 'NONE',  ( 0.000000000000000000, 0.000000000000000000, 1.000000000000000000 ) ) ;
#47760 = CARTESIAN_POINT ( 'NONE',  ( 97.65000000002650893, -209.9999999999999432, -74.99999999999356248 ) ) ;
#47761 = CARTESIAN_POINT ( 'NONE',  ( -96.32499999999996021, -207.7050326799711968, 87.98916666666666231 ) ) ;
#47762 = ADVANCED_FACE ( 'NONE', ( #55789 ), #22319, .F. ) ;
#47763 = EDGE_CURVE ( 'NONE', #42920, #37316, #3937, .T. ) ;
#47764 = DIRECTION ( 'NONE',  ( 0.000000000000000000, 0.000000000000000000, 1.000000000000000000 ) ) ;
#47765 = VERTEX_POINT ( 'NONE', #27193 ) ;
#47766 = AXIS2_PLACEMENT_3D ( 'NONE', #18666, #67680, #28850 ) ;
#47767 = DIRECTION ( 'NONE',  ( 0.000000000000000000, 0.9238795325112851842, 0.3826834323650937786 ) ) ;
#47768 = CARTESIAN_POINT ( 'NONE',  ( -21.33958957442910886, -129.9559990355020034, 2.500000000000000000 ) ) ;
#47769 = CARTESIAN_POINT ( 'NONE',  ( 0.000000000000000000, 0.000000000000000000, 0.000000000000000000 ) ) ;
#47770 = CIRCLE ( 'NONE', #56156, 4.999999999999997335 ) ;
#47771 = EDGE_CURVE ( 'NONE', #45794, #52132, #72682, .T. ) ;
#47772 = DIRECTION ( 'NONE',  ( 0.000000000000000000, 0.000000000000000000, 1.000000000000000000 ) ) ;
#47773 = EDGE_CURVE ( 'NONE', #18341, #44376, #31365, .T. ) ;
#47774 = AXIS2_PLACEMENT_3D ( 'NONE', #34717, #189, #39995 ) ;
#47775 = AXIS2_PLACEMENT_3D ( 'NONE', #45191, #10970, #15868 ) ;
#47776 = DIRECTION ( 'NONE',  ( 0.000000000000000000, 0.000000000000000000, 1.000000000000000000 ) ) ;
#47777 = ORIENTED_EDGE ( 'NONE', *, *, #49535, .F. ) ;
#47778 = LINE ( 'NONE', #64713, #38302 ) ;
#47779 = DIRECTION ( 'NONE',  ( -1.000000000000000000, 0.000000000000000000, -0.000000000000000000 ) ) ;
#47780 = ORIENTED_EDGE ( 'NONE', *, *, #58055, .T. ) ;
#47781 = CARTESIAN_POINT ( 'NONE',  ( 97.30629616937498838, -211.3315407142195852, 85.46239583420044994 ) ) ;
#47782 = CARTESIAN_POINT ( 'NONE',  ( 96.15314808468748708, -208.0026889286704943, 89.58989583420049030 ) ) ;
#47783 = ADVANCED_FACE ( 'NONE', ( #44890 ), #4676, .F. ) ;
#47784 = ORIENTED_EDGE ( 'NONE', *, *, #73019, .T. ) ;
#47785 = CARTESIAN_POINT ( 'NONE',  ( 93.84685191531249870, -208.0026889286704943, 88.42572916753381662 ) ) ;
#47786 = EDGE_LOOP ( 'NONE', ( #10147, #15513, #58052, #15362 ) ) ;
#47787 = FACE_OUTER_BOUND ( 'NONE', #9799, .T. ) ;
#47788 = ORIENTED_EDGE ( 'NONE', *, *, #25652, .T. ) ;
#47789 = CARTESIAN_POINT ( 'NONE',  ( -97.30629616937501680, 91.33154071421968467, 80.22364583420048234 ) ) ;
#47790 = VECTOR ( 'NONE', #8122, 1000.000000000000000 ) ;
#47791 = ORIENTED_EDGE ( 'NONE', *, *, #14358, .T. ) ;
#47792 = ORIENTED_EDGE ( 'NONE', *, *, #74005, .T. ) ;
#47793 = VECTOR ( 'NONE', #17956, 1000.000000000000000 ) ;
#47794 = LINE ( 'NONE', #25599, #58034 ) ;
#47795 = AXIS2_PLACEMENT_3D ( 'NONE', #27150, #3891, #21146 ) ;
#47796 = ORIENTED_EDGE ( 'NONE', *, *, #53048, .F. ) ;
#47797 = FACE_OUTER_BOUND ( 'NONE', #23022, .T. ) ;
#47798 = DIRECTION ( 'NONE',  ( -1.000000000000000000, -0.000000000000000000, 0.000000000000000000 ) ) ;
#47799 = AXIS2_PLACEMENT_3D ( 'NONE', #60179, #62300, #9018 ) ;
#47800 = EDGE_CURVE ( 'NONE', #19857, #54641, #15188, .T. ) ;
#47801 = ORIENTED_EDGE ( 'NONE', *, *, #47020, .T. ) ;
#47802 = DIRECTION ( 'NONE',  ( 0.000000000000000000, 0.8090169943749446757, 0.5877852522924769119 ) ) ;
#47803 = VERTEX_POINT ( 'NONE', #26836 ) ;
#47804 = VECTOR ( 'NONE', #42977, 1000.000000000000114 ) ;
#47805 = CARTESIAN_POINT ( 'NONE',  ( 97.64999999999449187, -210.0000054026048701, 81.50687481489494246 ) ) ;
#47806 = EDGE_CURVE ( 'NONE', #44570, #57845, #38122, .T. ) ;
#47807 = VERTEX_POINT ( 'NONE', #67810 ) ;
#47808 = VERTEX_POINT ( 'NONE', #73806 ) ;
#47809 = VERTEX_POINT ( 'NONE', #38869 ) ;
#47810 = CARTESIAN_POINT ( 'NONE',  ( 97.30629616937498838, -209.9999999999999716, 78.53031250086714010 ) ) ;
#47811 = CARTESIAN_POINT ( 'NONE',  ( -96.32500000000001705, 92.29496732002878900, 83.54416666666666913 ) ) ;
#47812 = DIRECTION ( 'NONE',  ( -1.000000000000000000, -0.000000000000000000, -0.000000000000000000 ) ) ;
#47813 = ORIENTED_EDGE ( 'NONE', *, *, #42799, .T. ) ;
#47814 = CARTESIAN_POINT ( 'NONE',  ( -93.67499999999998295, -212.2949673200287179, 78.86104166840097207 ) ) ;
#47815 = CARTESIAN_POINT ( 'NONE',  ( 10.00000000000000000, 0.000000000000000000, 0.000000000000000000 ) ) ;
#47816 = DIRECTION ( 'NONE',  ( 0.000000000000000000, 0.000000000000000000, 1.000000000000000000 ) ) ;
#47817 = DIRECTION ( 'NONE',  ( 0.000000000000000000, 0.000000000000000000, 1.000000000000000000 ) ) ;
#47818 = CARTESIAN_POINT ( 'NONE',  ( 10.00000000000000000, 78.73519480814954363, 22.90783923731657978 ) ) ;
#47819 = CARTESIAN_POINT ( 'NONE',  ( -97.30629616937497417, -211.3315407142195852, 80.17072916753379275 ) ) ;
#47820 = CARTESIAN_POINT ( 'NONE',  ( -92.69370383062504004, 90.00000000000004263, 79.95906250086714806 ) ) ;
#47821 = ORIENTED_EDGE ( 'NONE', *, *, #74077, .F. ) ;
#47822 = CARTESIAN_POINT ( 'NONE',  ( 94.99999999999998579, 92.66308142843935514, 81.86406250086714920 ) ) ;
#47823 = ORIENTED_EDGE ( 'NONE', *, *, #18727, .T. ) ;
#47824 = CARTESIAN_POINT ( 'NONE',  ( 6.938893903907228378E-15, 0.000000000000000000, 0.000000000000000000 ) ) ;
#47825 = CARTESIAN_POINT ( 'NONE',  ( 11.99999999999999822, 54.21277698773752007, -55.38113227695726692 ) ) ;
#47826 = CARTESIAN_POINT ( 'NONE',  ( 11.99999999999999822, 0.000000000000000000, 0.000000000000000000 ) ) ;
#47827 = DIRECTION ( 'NONE',  ( 0.000000000000000000, -0.3090169943749460635, -0.9510565162951539753 ) ) ;
#47828 = DIRECTION ( 'NONE',  ( -1.000000000000000000, 0.000000000000000000, -0.000000000000000000 ) ) ;
#47829 = CARTESIAN_POINT ( 'NONE',  ( -93.84685191531248449, -208.0026889286704943, 81.81114583420047381 ) ) ;
#47830 = COLOUR_RGB ( '', 0.72549020, 0.75294118, 0.79215686) ;
#47831 = VECTOR ( 'NONE', #66367, 1000.000000000000000 ) ;
#47832 = CARTESIAN_POINT ( 'NONE',  ( 10.00000000000000000, 0.000000000000000000, 0.000000000000000000 ) ) ;
#47833 = DIRECTION ( 'NONE',  ( -1.000000000000000000, 0.000000000000000000, -0.000000000000000000 ) ) ;
#47834 = CARTESIAN_POINT ( 'NONE',  ( 10.00000000000000000, 6.903761155837774943, 77.19088730480525840 ) ) ;
#47835 = ORIENTED_EDGE ( 'NONE', *, *, #69928, .T. ) ;
#47836 = ORIENTED_EDGE ( 'NONE', *, *, #66287, .T. ) ;
#47837 = DIRECTION ( 'NONE',  ( 0.02332147558787931590, 0.9997280174009348652, 0.000000000000000000 ) ) ;
#47838 = CIRCLE ( 'NONE', #53852, 31.99999999999998579 ) ;
#47839 = DIRECTION ( 'NONE',  ( 0.000000000000000000, 0.9945218953682742891, 0.1045284632676436315 ) ) ;
#47840 = CARTESIAN_POINT ( 'NONE',  ( 10.00000000000000000, 62.20884554314086046, -46.21855187248561236 ) ) ;
#47841 = CARTESIAN_POINT ( 'NONE',  ( -93.84685191531252713, 88.00268892867056536, 84.13947916753380696 ) ) ;
#47842 = CARTESIAN_POINT ( 'NONE',  ( 22.51310757741980240, -113.2613067136482101, 2.500000000000000000 ) ) ;
#47843 = DIRECTION ( 'NONE',  ( -2.628368902995175337E-16, -1.000000000000000000, 0.000000000000000000 ) ) ;
#47844 = PLANE ( 'NONE',  #42212 ) ;
#47845 = CARTESIAN_POINT ( 'NONE',  ( 11.99999999999999822, -65.64334221924882229, -41.19522573413803457 ) ) ;
#47846 = EDGE_LOOP ( 'NONE', ( #30212, #74264, #30610, #5824 ) ) ;
#47847 = CARTESIAN_POINT ( 'NONE',  ( -95.00000000000002842, 92.66308142843932671, 75.51406250086714067 ) ) ;
#47848 = AXIS2_PLACEMENT_3D ( 'NONE', #6189, #11431, #40020 ) ;
#47849 = DIRECTION ( 'NONE',  ( 0.000000000000000000, -0.2334453638559125521, 0.9723699203976750027 ) ) ;
#47850 = VECTOR ( 'NONE', #50006, 1000.000000000000000 ) ;
#47851 = DIRECTION ( 'NONE',  ( -1.000000000000000000, 0.000000000000000000, 0.000000000000000000 ) ) ;
#47852 = CARTESIAN_POINT ( 'NONE',  ( -10.90473778262209414, 0.000000000000000000, -13.71319123046128752 ) ) ;
#47853 = CARTESIAN_POINT ( 'NONE',  ( -92.69370383062498320, -211.3315407142195852, 87.52614583420049144 ) ) ;
#47854 = SURFACE_SIDE_STYLE ('',( #57679 ) ) ;
#47855 = EDGE_CURVE ( 'NONE', #15277, #48910, #43784, .T. ) ;
#47856 = VECTOR ( 'NONE', #35037, 1000.000000000000000 ) ;
#47857 = CIRCLE ( 'NONE', #38247, 31.99999999999999289 ) ;
#47858 = EDGE_CURVE ( 'NONE', #12105, #31980, #69785, .T. ) ;
#47859 = DIRECTION ( 'NONE',  ( -1.000000000000000000, -0.000000000000000000, -0.000000000000000000 ) ) ;
#47860 = AXIS2_PLACEMENT_3D ( 'NONE', #15401, #53779, #42888 ) ;
#47861 = CARTESIAN_POINT ( 'NONE',  ( 10.00000000000000000, 0.000000000000000000, 0.000000000000000000 ) ) ;
#47862 = CARTESIAN_POINT ( 'NONE',  ( -96.15314808468747287, -208.0026889286704943, 77.63072916753381492 ) ) ;
#47863 = CARTESIAN_POINT ( 'NONE',  ( 96.32499999999997442, 92.29496732002878900, 88.51833333333333087 ) ) ;
#47864 = ORIENTED_EDGE ( 'NONE', *, *, #35733, .F. ) ;
#47865 = EDGE_CURVE ( 'NONE', #53435, #49109, #67377, .T. ) ;
#47866 = CYLINDRICAL_SURFACE ( 'NONE', #66568, 2.649999999999985700 ) ;
#47867 = DIRECTION ( 'NONE',  ( -1.000000000000000000, -0.000000000000000000, -0.000000000000000000 ) ) ;
#47868 = DIRECTION ( 'NONE',  ( 0.000000000000000000, -0.7604059656000228262, -0.6494480483301932061 ) ) ;
#47869 = DIRECTION ( 'NONE',  ( -0.000000000000000000, 0.000000000000000000, -1.000000000000000000 ) ) ;
#47870 = CARTESIAN_POINT ( 'NONE',  ( 92.69370383062501162, -211.3315407142195852, 87.31447916753381833 ) ) ;
#47871 = EDGE_LOOP ( 'NONE', ( #6328, #42936, #39513, #59167 ) ) ;
#47872 = AXIS2_PLACEMENT_3D ( 'NONE', #7757, #36319, #70896 ) ;
#47873 = DIRECTION ( 'NONE',  ( 1.000000000000000000, 0.000000000000000000, 0.000000000000000000 ) ) ;
#47874 = CYLINDRICAL_SURFACE ( 'NONE', #66705, 31.99999999999998579 ) ;
#47875 = EDGE_CURVE ( 'NONE', #40595, #50481, #28315, .T. ) ;
#47876 = ORIENTED_EDGE ( 'NONE', *, *, #3514, .F. ) ;
#47877 = DIRECTION ( 'NONE',  ( -1.000000000000000000, 3.061616997868382648E-16, 0.000000000000000000 ) ) ;
#47878 = EDGE_CURVE ( 'NONE', #72116, #9910, #33212, .T. ) ;
#47879 = ORIENTED_EDGE ( 'NONE', *, *, #3675, .F. ) ;
#47880 = CIRCLE ( 'NONE', #11802, 16.00000000000000000 ) ;
#47881 = VECTOR ( 'NONE', #50721, 1000.000000000000000 ) ;
#47882 = CARTESIAN_POINT ( 'NONE',  ( 10.00000000000000000, -31.47745569255189224, 68.26794271651249346 ) ) ;
#47883 = EDGE_CURVE ( 'NONE', #48585, #36787, #3803, .T. ) ;
#47884 = CIRCLE ( 'NONE', #10643, 16.00000000000000355 ) ;
#47885 = VERTEX_POINT ( 'NONE', #73438 ) ;
#47886 = ORIENTED_EDGE ( 'NONE', *, *, #17510, .F. ) ;
#47887 = AXIS2_PLACEMENT_3D ( 'NONE', #69956, #18455, #35739 ) ;
#47888 = ORIENTED_EDGE ( 'NONE', *, *, #8772, .T. ) ;
#47889 = DIRECTION ( 'NONE',  ( -1.000000000000000000, 0.000000000000000000, -0.000000000000000000 ) ) ;
#47890 = EDGE_CURVE ( 'NONE', #66514, #19617, #55415, .T. ) ;
#47891 = VERTEX_POINT ( 'NONE', #12509 ) ;
#47892 = ORIENTED_EDGE ( 'NONE', *, *, #15688, .F. ) ;
#47893 = CARTESIAN_POINT ( 'NONE',  ( 97.30629616937498838, 90.00000000000002842, 79.32406250086715715 ) ) ;
#47894 = CARTESIAN_POINT ( 'NONE',  ( -97.65000000000001990, 88.47002178664754979, 81.24229166840096639 ) ) ;
#47895 = CARTESIAN_POINT ( 'NONE',  ( -7.001685179585692254, -14.98378029539707512, 0.000000000000000000 ) ) ;
#47896 = AXIS2_PLACEMENT_3D ( 'NONE', #38410, #32749, #50037 ) ;
#47897 = ORIENTED_EDGE ( 'NONE', *, *, #54100, .T. ) ;
#47899 = ORIENTED_EDGE ( 'NONE', *, *, #61147, .F. ) ;
#47898 = VECTOR ( 'NONE', #52265, 1000.000000000000114 ) ;
#47900 = ORIENTED_EDGE ( 'NONE', *, *, #48225, .T. ) ;
#47901 = CARTESIAN_POINT ( 'NONE',  ( 10.00000000000000000, 80.55351364060609853, -15.33399622253395478 ) ) ;
#47902 = VERTEX_POINT ( 'NONE', #40724 ) ;
#47903 = CIRCLE ( 'NONE', #25097, 16.00000000000000355 ) ;
#47904 = CARTESIAN_POINT ( 'NONE',  ( 0.09268126076924407264, 0.8248091802970087816, 42.00000000000001421 ) ) ;
#47905 = CARTESIAN_POINT ( 'NONE',  ( 10.00000000000000000, 0.000000000000000000, 0.000000000000000000 ) ) ;
#47906 = CARTESIAN_POINT ( 'NONE',  ( -97.45337789172094745, 90.48452257634338025, 74.90854212414870972 ) ) ;
#47907 = LINE ( 'NONE', #17486, #41091 ) ;
#47908 = CARTESIAN_POINT ( 'NONE',  ( 10.00000000000000000, -50.23322058963299241, -64.81221759200398935 ) ) ;
#47909 = DIRECTION ( 'NONE',  ( 0.000000000000000000, -0.4999999999999913403, -0.8660254037844435926 ) ) ;
#47910 = AXIS2_PLACEMENT_3D ( 'NONE', #31510, #36049, #64627 ) ;
#47911 = DIRECTION ( 'NONE',  ( -1.000000000000000000, 0.000000000000000000, 0.000000000000000000 ) ) ;
#47912 = CIRCLE ( 'NONE', #40672, 42.00000000000000000 ) ;
#47913 = CARTESIAN_POINT ( 'NONE',  ( -97.64999999999996305, -209.9999999999999716, 79.91937500173429498 ) ) ;
#47914 = DIRECTION ( 'NONE',  ( 0.000000000000000000, 0.000000000000000000, 1.000000000000000000 ) ) ;
#47916 = CARTESIAN_POINT ( 'NONE',  ( -92.35000000000005116, 88.47002178664754979, 77.64395833506762301 ) ) ;
#47915 = CARTESIAN_POINT ( 'NONE',  ( 97.64999999999997726, 91.52997821335252127, 77.11479166840095445 ) ) ;
#47917 = AXIS2_PLACEMENT_3D ( 'NONE', #29458, #22362, #68225 ) ;
#47918 =( BOUNDED_CURVE ( )  B_SPLINE_CURVE ( 2, ( #1299, #24188, #6169, #6524, #46011, #7265, #40359 ),
 .UNSPECIFIED., .F., .F. ) 
 B_SPLINE_CURVE_WITH_KNOTS ( ( 3, 2, 2, 3 ),
 ( 0.8749999999999997780, 0.8819444444444441977, 0.8888888888888886175, 0.8958333333333331483 ),
 .UNSPECIFIED. ) 
 CURVE ( )  GEOMETRIC_REPRESENTATION_ITEM ( )  RATIONAL_B_SPLINE_CURVE ( ( 1.000000000000004219, 0.8660254037844343777, 1.000000000000000000, 0.8660254037844387076, 1.000000000000000000, 0.8660254037844430375, 0.9999999999999956701 ) ) 
 REPRESENTATION_ITEM ( '' )  );
#47919 = ORIENTED_EDGE ( 'NONE', *, *, #25572, .T. ) ;
#47920 = CARTESIAN_POINT ( 'NONE',  ( 93.84685191531248449, 91.99731107132950569, 75.09072916753380866 ) ) ;
#47921 = DIRECTION ( 'NONE',  ( -1.000000000000000000, 0.000000000000000000, 0.000000000000000000 ) ) ;
#47922 = DIRECTION ( 'NONE',  ( 1.000000000000000000, 0.000000000000000000, 0.000000000000000000 ) ) ;
#47923 = CYLINDRICAL_SURFACE ( 'NONE', #41986, 37.49900000000000233 ) ;
#47924 = CARTESIAN_POINT ( 'NONE',  ( -97.64999999999996305, -209.9999999999999716, 90.00000000000000000 ) ) ;
#47925 = CARTESIAN_POINT ( 'NONE',  ( 12.00000000000000000, -18.13022148937263012, -15.02647892043543898 ) ) ;
#47926 = ORIENTED_EDGE ( 'NONE', *, *, #54069, .F. ) ;
#47927 = CYLINDRICAL_SURFACE ( 'NONE', #12099, 31.99999999999998579 ) ;
#47928 = CARTESIAN_POINT ( 'NONE',  ( 10.00000000000000000, 6.903761155838878061, -77.19088730480517313 ) ) ;
#47929 = ORIENTED_EDGE ( 'NONE', *, *, #41326, .F. ) ;
#47930 = ORIENTED_EDGE ( 'NONE', *, *, #5362, .F. ) ;
#47931 = VECTOR ( 'NONE', #4568, 1000.000000000000000 ) ;
#47932 = FACE_OUTER_BOUND ( 'NONE', #44472, .T. ) ;
#47933 = CARTESIAN_POINT ( 'NONE',  ( 92.35000000000000853, -208.4700217866474645, 88.12145833506765769 ) ) ;
#47934 = CARTESIAN_POINT ( 'NONE',  ( -3.000000000000000000, -26.23277895567251505, 4.042438405569750870 ) ) ;
#47935 = DIRECTION ( 'NONE',  ( -0.9038112904824853189, 0.4279312458752976833, 0.000000000000000000 ) ) ;
#47936 = DIRECTION ( 'NONE',  ( -2.603472992746261562E-14, -2.546204323184492723E-14, 1.000000000000000000 ) ) ;
#47937 = COLOUR_RGB ( '', 0.66274510, 0.83137255, 0.94901961) ;
#47938 = VERTEX_POINT ( 'NONE', #58756 ) ;
#47939 = AXIS2_PLACEMENT_3D ( 'NONE', #8417, #14782, #36977 ) ;
#47940 = ADVANCED_FACE ( 'NONE', ( #51629 ), #45837, .T. ) ;
#47942 = CARTESIAN_POINT ( 'NONE',  ( 0.000000000000000000, -46.53671651293991118, 59.03961581697383565 ) ) ;
#47941 = CIRCLE ( 'NONE', #30062, 31.99999999999999645 ) ;
#47943 = CARTESIAN_POINT ( 'NONE',  ( 5.999999999999999112, -77.16300072079681627, 27.74655509720641433 ) ) ;
#47944 = AXIS2_PLACEMENT_3D ( 'NONE', #15769, #9379, #4138 ) ;
#47945 = EDGE_CURVE ( 'NONE', #44992, #4927, #17779, .T. ) ;
#47946 = CARTESIAN_POINT ( 'NONE',  ( 5.000000000000000000, -27.75498641678764855, 31.52238457039590358 ) ) ;
#47947 = CARTESIAN_POINT ( 'NONE',  ( 11.99999999999999822, -12.93880638057260946, -76.41127070299286572 ) ) ;
#47948 = ADVANCED_FACE ( 'NONE', ( #6875 ), #43424, .T. ) ;
#47949 = CIRCLE ( 'NONE', #23910, 77.49899999999999523 ) ;
#47950 = DIRECTION ( 'NONE',  ( -0.000000000000000000, -0.000000000000000000, 1.000000000000000000 ) ) ;
#47951 = DIRECTION ( 'NONE',  ( 0.000000000000000000, 0.000000000000000000, 1.000000000000000000 ) ) ;
#47952 = DIRECTION ( 'NONE',  ( -1.000000000000000000, 0.000000000000000000, 0.000000000000000000 ) ) ;
#47953 = CARTESIAN_POINT ( 'NONE',  ( -97.64999999999996305, -209.9999907079536854, 84.99937468035446386 ) ) ;
#47954 = EDGE_CURVE ( 'NONE', #47807, #48711, #48168, .T. ) ;
#47955 = CARTESIAN_POINT ( 'NONE',  ( -97.64999999999996305, -208.4700217866474645, 77.96145833506763267 ) ) ;
#47956 = CARTESIAN_POINT ( 'NONE',  ( -92.34999999999999432, -209.9999999999999716, 90.00000000000000000 ) ) ;
#47957 = EDGE_CURVE ( 'NONE', #2572, #26602, #55416, .T. ) ;
#47958 = CARTESIAN_POINT ( 'NONE',  ( 97.30629616937498838, 91.33154071421968467, 83.18697916753382060 ) ) ;
#47959 = CARTESIAN_POINT ( 'NONE',  ( -94.99999999999997158, -212.6630814284392557, 87.42031250086715488 ) ) ;
#47960 = CARTESIAN_POINT ( 'NONE',  ( 94.99999999999998579, 93.05995642670504253, 79.12562500173429214 ) ) ;
#47961 = AXIS2_PLACEMENT_3D ( 'NONE', #22508, #44708, #34151 ) ;
#47962 = ORIENTED_EDGE ( 'NONE', *, *, #48708, .F. ) ;
#47963 = EDGE_CURVE ( 'NONE', #16250, #51073, #12109, .T. ) ;
#47964 = CARTESIAN_POINT ( 'NONE',  ( 0.000000000000000000, 0.000000000000000000, 0.000000000000000000 ) ) ;
#47965 = CARTESIAN_POINT ( 'NONE',  ( -97.64999999999996305, -209.9999999999999716, 82.37999999999999545 ) ) ;
#47966 = CARTESIAN_POINT ( 'NONE',  ( -97.30629616937501680, 90.00000000000004263, 76.94281250086713442 ) ) ;
#47967 = CIRCLE ( 'NONE', #1214, 31.99999999999998579 ) ;
#47968 = AXIS2_PLACEMENT_3D ( 'NONE', #68727, #45428, #61970 ) ;
#47969 = VECTOR ( 'NONE', #15904, 1000.000000000000000 ) ;
#47970 = CIRCLE ( 'NONE', #15551, 37.49900000000000233 ) ;
#47971 = CARTESIAN_POINT ( 'NONE',  ( 96.15314808468750130, -211.9973110713294489, 87.94947916753380923 ) ) ;
#47972 = VERTEX_POINT ( 'NONE', #17052 ) ;
#47973 = CARTESIAN_POINT ( 'NONE',  ( 0.000000000000000000, 0.000000000000000000, 0.000000000000000000 ) ) ;
#47974 = VERTEX_POINT ( 'NONE', #46364 ) ;
#47975 = EDGE_CURVE ( 'NONE', #66404, #32719, #2603, .T. ) ;
#47976 = ORIENTED_EDGE ( 'NONE', *, *, #10303, .T. ) ;
#47977 = CARTESIAN_POINT ( 'NONE',  ( 96.32499999999998863, -207.7050326799711968, 84.07333333333333769 ) ) ;
#47978 = ADVANCED_FACE ( 'NONE', ( #39988 ), #18155, .F. ) ;
#47979 = EDGE_CURVE ( 'NONE', #70065, #53287, #9793, .T. ) ;
#47980 = CARTESIAN_POINT ( 'NONE',  ( -10.00000000000000000, 0.000000000000000000, 0.000000000000000000 ) ) ;
#47981 = ORIENTED_EDGE ( 'NONE', *, *, #16413, .T. ) ;
#47982 = CARTESIAN_POINT ( 'NONE',  ( 11.99999999999999822, 2.543863470249544623, -81.96053171279901051 ) ) ;
#47983 = CARTESIAN_POINT ( 'NONE',  ( 95.00000000000000000, -212.6630814284392557, 77.26031250086714408 ) ) ;
#47984 = DIRECTION ( 'NONE',  ( -0.000000000000000000, -0.000000000000000000, 1.000000000000000000 ) ) ;
#47985 = EDGE_CURVE ( 'NONE', #36972, #44773, #17417, .T. ) ;
#47986 = CARTESIAN_POINT ( 'NONE',  ( 24.95699195200416654, -110.9640411295978595, 5.500000000000000000 ) ) ;
#47987 = LINE ( 'NONE', #8120, #47238 ) ;
#47988 = CARTESIAN_POINT ( 'NONE',  ( -10.00000000000000000, 0.000000000000000000, 0.000000000000000000 ) ) ;
#47989 = AXIS2_PLACEMENT_3D ( 'NONE', #3749, #60514, #38313 ) ;
#47990 = DIRECTION ( 'NONE',  ( -1.000000000000000000, 0.000000000000000000, 0.000000000000000000 ) ) ;
#47991 = CARTESIAN_POINT ( 'NONE',  ( 96.32499999999998863, -207.7050326799711968, 84.07333333333333769 ) ) ;
#47992 = VECTOR ( 'NONE', #67760, 1000.000000000000000 ) ;
#47993 = ORIENTED_EDGE ( 'NONE', *, *, #26329, .F. ) ;
#47994 = ORIENTED_EDGE ( 'NONE', *, *, #30205, .T. ) ;
#47995 = AXIS2_PLACEMENT_3D ( 'NONE', #15198, #47936, #31376 ) ;
#47996 = ORIENTED_EDGE ( 'NONE', *, *, #4803, .F. ) ;
#47997 = ORIENTED_EDGE ( 'NONE', *, *, #44913, .T. ) ;
#47998 = DIRECTION ( 'NONE',  ( -1.000000000000000000, 0.000000000000000000, 0.000000000000000000 ) ) ;
#47999 = SURFACE_SIDE_STYLE ('',( #46895 ) ) ;
#48000 = CARTESIAN_POINT ( 'NONE',  ( -96.15314808468752972, 91.99731107132950569, 83.34572916753383254 ) ) ;
#48001 = FACE_OUTER_BOUND ( 'NONE', #631, .T. ) ;
#48002 = AXIS2_PLACEMENT_3D ( 'NONE', #4817, #26962, #61195 ) ;
#48003 = CARTESIAN_POINT ( 'NONE',  ( 0.000000000000000000, 75.11764819372149304, 29.05362095685338275 ) ) ;
#48004 = CARTESIAN_POINT ( 'NONE',  ( -21.67772167707813935, -110.8034581014852762, -5.500000000000000000 ) ) ;
#48005 = ORIENTED_EDGE ( 'NONE', *, *, #51599, .F. ) ;
#48006 = ORIENTED_EDGE ( 'NONE', *, *, #19005, .F. ) ;
#48007 = DIRECTION ( 'NONE',  ( -1.000000000000000000, 0.000000000000000000, 0.000000000000000000 ) ) ;
#48008 = EDGE_LOOP ( 'NONE', ( #30874, #59587, #63335, #58888 ) ) ;
#48009 = CARTESIAN_POINT ( 'NONE',  ( -97.65000000000001990, 91.52997821335253548, 85.58145833506763722 ) ) ;
#48010 = CARTESIAN_POINT ( 'NONE',  ( 97.30629616937498838, 88.66845928578037217, 85.62114583420047609 ) ) ;
#48011 = LINE ( 'NONE', #66424, #49030 ) ;
#48012 = LINE ( 'NONE', #31075, #7382 ) ;
#48013 = DIRECTION ( 'NONE',  ( 1.000000000000000000, 0.000000000000000000, 0.000000000000000000 ) ) ;
#48014 = DIRECTION ( 'NONE',  ( 0.000000000000000000, 0.9876883405951382144, -0.1564344650402276493 ) ) ;
#48015 = VERTEX_POINT ( 'NONE', #64400 ) ;
#48016 = CARTESIAN_POINT ( 'NONE',  ( 15.00000000000000000, -23.29833615347104470, 3.418703333116808629 ) ) ;
#48017 = AXIS2_PLACEMENT_3D ( 'NONE', #49878, #14563, #60812 ) ;
#48018 = AXIS2_PLACEMENT_3D ( 'NONE', #10276, #38851, #10646 ) ;
#48020 = DIRECTION ( 'NONE',  ( -1.000000000000000000, 0.000000000000000000, -0.000000000000000000 ) ) ;
#48019 = CIRCLE ( 'NONE', #71996, 37.49900000000000944 ) ;
#48021 = ORIENTED_EDGE ( 'NONE', *, *, #23857, .T. ) ;
#48022 = EDGE_LOOP ( 'NONE', ( #21434, #31778, #72478, #22650, #66863 ) ) ;
#48023 = CARTESIAN_POINT ( 'NONE',  ( 94.99999999999998579, 86.94004357329502852, 78.80812500173429669 ) ) ;
#48024 = AXIS2_PLACEMENT_3D ( 'NONE', #30503, #53447, #65846 ) ;
#48025 = CARTESIAN_POINT ( 'NONE',  ( 5.000000000000000000, 1.947085426416884202, -5.800379292880308846 ) ) ;
#48026 = CARTESIAN_POINT ( 'NONE',  ( 10.00000000000000000, -16.65972982744878195, -80.28980883073774066 ) ) ;
#48027 = CARTESIAN_POINT ( 'NONE',  ( -96.15314808468745866, -211.9973110713294489, 88.00239583420048461 ) ) ;
#48028 = ORIENTED_EDGE ( 'NONE', *, *, #27922, .F. ) ;
#48029 = SURFACE_STYLE_USAGE ( .BOTH. , #35624 ) ;
#48030 = VERTEX_POINT ( 'NONE', #40350 ) ;
#48031 = VERTEX_POINT ( 'NONE', #29062 ) ;
#48032 = DIRECTION ( 'NONE',  ( 1.000000000000000000, 0.000000000000000000, 0.000000000000000000 ) ) ;
#48033 = EDGE_CURVE ( 'NONE', #72759, #63788, #51989, .T. ) ;
#48034 = FILL_AREA_STYLE_COLOUR ( '', #46554 ) ;
#48035 = CARTESIAN_POINT ( 'NONE',  ( 97.30629616937498838, 90.00000000000002842, 81.07031250086714635 ) ) ;
#48036 = DIRECTION ( 'NONE',  ( 0.000000000000000000, 0.000000000000000000, 1.000000000000000000 ) ) ;
#48037 = CARTESIAN_POINT ( 'NONE',  ( -92.35000000000003695, 89.99999990163421160, 80.23687499810812085 ) ) ;
#48038 = CARTESIAN_POINT ( 'NONE',  ( 6.000000000000000000, 81.34940948281337114, 10.30890764327411446 ) ) ;
#48039 = DIRECTION ( 'NONE',  ( -1.000000000000000000, 0.000000000000000000, 0.000000000000000000 ) ) ;
#48040 = ADVANCED_FACE ( 'NONE', ( #6514 ), #23435, .T. ) ;
#48042 = EDGE_CURVE ( 'NONE', #21068, #45442, #51826, .T. ) ;
#48041 = FACE_OUTER_BOUND ( 'NONE', #14602, .T. ) ;
#48043 = FACE_OUTER_BOUND ( 'NONE', #1339, .T. ) ;
#48044 = CARTESIAN_POINT ( 'NONE',  ( 0.000000000000000000, 0.000000000000000000, 0.000000000000000000 ) ) ;
#48045 = AXIS2_PLACEMENT_3D ( 'NONE', #26081, #9164, #72317 ) ;
#48046 = CARTESIAN_POINT ( 'NONE',  ( 92.35000000000000853, -209.9999999999999716, 90.00000000000000000 ) ) ;
#48047 = CARTESIAN_POINT ( 'NONE',  ( 10.00000000000000000, 0.000000000000000000, 0.000000000000000000 ) ) ;
#48048 = ORIENTED_EDGE ( 'NONE', *, *, #37615, .T. ) ;
#48049 = AXIS2_PLACEMENT_3D ( 'NONE', #68943, #18170, #57665 ) ;
#48050 = CARTESIAN_POINT ( 'NONE',  ( -97.30629616937501680, 88.66845928578038638, 87.79072916753379729 ) ) ;
#48051 = AXIS2_PLACEMENT_3D ( 'NONE', #45379, #73548, #22056 ) ;
#48052 = DIRECTION ( 'NONE',  ( 0.000000000000000000, 0.9510565162951523099, 0.3090169943749514481 ) ) ;
#48053 = AXIS2_PLACEMENT_3D ( 'NONE', #43588, #2648, #20635 ) ;
#48054 = EDGE_CURVE ( 'NONE', #11355, #11947, #46736, .T. ) ;
#48055 = DIRECTION ( 'NONE',  ( -1.000000000000000000, 0.000000000000000000, 0.000000000000000000 ) ) ;
#48056 = EDGE_CURVE ( 'NONE', #50841, #71000, #57780, .T. ) ;
#48057 = ORIENTED_EDGE ( 'NONE', *, *, #62688, .T. ) ;
#48058 = CARTESIAN_POINT ( 'NONE',  ( 119.3426274441929280, -132.5434155921172419, 5.500000000000000000 ) ) ;
#48059 = CARTESIAN_POINT ( 'NONE',  ( 5.999999999999999112, 68.55367621811141987, 44.99326035066079044 ) ) ;
#48060 = DIRECTION ( 'NONE',  ( 0.000000000000000000, 0.000000000000000000, 1.000000000000000000 ) ) ;
#48061 = VECTOR ( 'NONE', #65515, 1000.000000000000000 ) ;
#48062 = CIRCLE ( 'NONE', #67281, 32.00000000000000000 ) ;
#48063 = EDGE_CURVE ( 'NONE', #55509, #21370, #19391, .T. ) ;
#48064 = EDGE_CURVE ( 'NONE', #71124, #29550, #43322, .T. ) ;
#48065 = CARTESIAN_POINT ( 'NONE',  ( 95.00000000000000000, -207.3369185715606307, 82.02281250086714692 ) ) ;
#48066 = ORIENTED_EDGE ( 'NONE', *, *, #22169, .F. ) ;
#48067 = VECTOR ( 'NONE', #574, 1000.000000000000000 ) ;
#48068 = ORIENTED_EDGE ( 'NONE', *, *, #12166, .T. ) ;
#48069 = VECTOR ( 'NONE', #45951, 1000.000000000000114 ) ;
#48070 = CARTESIAN_POINT ( 'NONE',  ( 0.000000000000000000, -75.11725578898470701, 2.956366410620372864 ) ) ;
#48071 = VERTEX_POINT ( 'NONE', #25643 ) ;
#48072 = CARTESIAN_POINT ( 'NONE',  ( 12.00000000000000000, -22.67460108101782268, -6.353146135317906840 ) ) ;
#48073 = LINE ( 'NONE', #42436, #72390 ) ;
#48074 = ORIENTED_EDGE ( 'NONE', *, *, #41544, .T. ) ;
#48075 = CARTESIAN_POINT ( 'NONE',  ( 96.15314808468750130, -211.9973110713294489, 81.12322916753382174 ) ) ;
#48076 = ORIENTED_EDGE ( 'NONE', *, *, #47466, .F. ) ;
#48077 = CARTESIAN_POINT ( 'NONE',  ( 10.00000000000000000, -35.91791733033426226, -68.67312586195033930 ) ) ;
#48078 = ORIENTED_EDGE ( 'NONE', *, *, #54685, .T. ) ;
#48079 = ORIENTED_EDGE ( 'NONE', *, *, #40057, .T. ) ;
#48080 = DIRECTION ( 'NONE',  ( 0.000000000000000000, 0.5877852522924685852, 0.8090169943749508930 ) ) ;
#48081 = SURFACE_STYLE_USAGE ( .BOTH. , #35324 ) ;
#48082 = FACE_OUTER_BOUND ( 'NONE', #68731, .T. ) ;
#48083 = ORIENTED_EDGE ( 'NONE', *, *, #24701, .T. ) ;
#48084 = LINE ( 'NONE', #31890, #38980 ) ;
#48085 = CARTESIAN_POINT ( 'NONE',  ( 96.32499999999998863, -212.2949673200287179, 83.30604166840096525 ) ) ;
#48086 = CARTESIAN_POINT ( 'NONE',  ( 97.64999999999997726, 88.47002178664753558, 83.91458333333333997 ) ) ;
#48087 = EDGE_LOOP ( 'NONE', ( #18837, #40614 ) ) ;
#48088 = DIRECTION ( 'NONE',  ( -1.000000000000000000, 0.000000000000000000, -0.000000000000000000 ) ) ;
#48089 = DIRECTION ( 'NONE',  ( -1.000000000000000000, 0.000000000000000000, 0.000000000000000000 ) ) ;
#48090 = ORIENTED_EDGE ( 'NONE', *, *, #71051, .T. ) ;
#48091 = ORIENTED_EDGE ( 'NONE', *, *, #65602, .F. ) ;
#48092 = CARTESIAN_POINT ( 'NONE',  ( -93.84685191531252713, 88.00268892867056536, 87.47322916753381605 ) ) ;
#48093 = CARTESIAN_POINT ( 'NONE',  ( 96.15314808468748708, 91.99731107132950569, 82.44614583420046472 ) ) ;
#48094 = VERTEX_POINT ( 'NONE', #54229 ) ;
#48095 = CARTESIAN_POINT ( 'NONE',  ( 97.64999999999997726, 91.52997821335252127, 85.36979166840096411 ) ) ;
#48096 = VECTOR ( 'NONE', #65894, 1000.000000000000000 ) ;
#48097 = VERTEX_POINT ( 'NONE', #14362 ) ;
#48098 = CARTESIAN_POINT ( 'NONE',  ( 97.64999999954044085, -209.9999506483753180, 87.22187670868780174 ) ) ;
#48099 = VECTOR ( 'NONE', #56660, 1000.000000000000000 ) ;
#48100 = ORIENTED_EDGE ( 'NONE', *, *, #10612, .F. ) ;
#48101 = EDGE_LOOP ( 'NONE', ( #55392, #66716, #14036, #32261 ) ) ;
#48102 = CIRCLE ( 'NONE', #33662, 2.541999999999999815 ) ;
#48103 = ORIENTED_EDGE ( 'NONE', *, *, #21831, .F. ) ;
#48104 = CARTESIAN_POINT ( 'NONE',  ( 10.00000000000000000, 22.74946021919133088, 29.81001611431016229 ) ) ;
#48105 = DIRECTION ( 'NONE',  ( 0.000000000000000000, 0.000000000000000000, -1.000000000000000000 ) ) ;
#48106 = CARTESIAN_POINT ( 'NONE',  ( -92.35000000000005116, 91.52997821335253548, 83.38541666666667140 ) ) ;
#48107 = ORIENTED_EDGE ( 'NONE', *, *, #57574, .F. ) ;
#48108 = LINE ( 'NONE', #19158, #7109 ) ;
#48109 = FACE_OUTER_BOUND ( 'NONE', #65861, .T. ) ;
#48110 = ORIENTED_EDGE ( 'NONE', *, *, #38553, .F. ) ;
#48111 = DIRECTION ( 'NONE',  ( 0.000000000000000000, 0.000000000000000000, 1.000000000000000000 ) ) ;
#48112 = CARTESIAN_POINT ( 'NONE',  ( -93.84685191531247028, -211.9973110713294489, 83.50447916753381605 ) ) ;
#48113 = ORIENTED_EDGE ( 'NONE', *, *, #49695, .T. ) ;
#48114 = DIRECTION ( 'NONE',  ( -0.000000000000000000, -0.000000000000000000, -1.000000000000000000 ) ) ;
#48115 = CARTESIAN_POINT ( 'NONE',  ( 0.000000000000000000, 35.47612816024523852, 22.48208911017513145 ) ) ;
#48116 = FACE_OUTER_BOUND ( 'NONE', #406, .T. ) ;
#48117 = CARTESIAN_POINT ( 'NONE',  ( 12.00000000000000000, -10.45096189432344502, -21.10159698893425073 ) ) ;
#48118 = PRODUCT_RELATED_PRODUCT_CATEGORY ( 'part', '', ( #72776 ) ) ;
#48119 = EDGE_CURVE ( 'NONE', #11255, #12875, #30530, .T. ) ;
#48120 = VECTOR ( 'NONE', #50334, 1000.000000000000000 ) ;
#48121 = DIRECTION ( 'NONE',  ( 0.000000000000000000, -0.000000000000000000, 1.000000000000000000 ) ) ;
#48122 = AXIS2_PLACEMENT_3D ( 'NONE', #67995, #62754, #4483 ) ;
#48123 = EDGE_CURVE ( 'NONE', #19678, #6105, #33792, .T. ) ;
#48124 = DIRECTION ( 'NONE',  ( 0.000000000000000000, 0.000000000000000000, 1.000000000000000000 ) ) ;
#48125 = DIRECTION ( 'NONE',  ( -1.000000000000000000, -0.000000000000000000, 0.000000000000000000 ) ) ;
#48126 = CARTESIAN_POINT ( 'NONE',  ( 97.30629616937497417, -209.9999999999998863, 74.79348190356849102 ) ) ;
#48127 = AXIS2_PLACEMENT_3D ( 'NONE', #48047, #31112, #36021 ) ;
#48128 = DIRECTION ( 'NONE',  ( -0.000000000000000000, -0.000000000000000000, 1.000000000000000000 ) ) ;
#48130 = ADVANCED_FACE ( 'NONE', ( #18882 ), #37312, .T. ) ;
#48129 = CARTESIAN_POINT ( 'NONE',  ( 0.000000000000000000, 62.50329211542494789, -41.76937507738723099 ) ) ;
#48131 = CARTESIAN_POINT ( 'NONE',  ( -97.30629616937501680, 90.00000000000004263, 89.80156250086714920 ) ) ;
#48132 = CARTESIAN_POINT ( 'NONE',  ( 1.560000000000000053, -1.732050807568877859, -1.752539433813135784E-17 ) ) ;
#48133 = CARTESIAN_POINT ( 'NONE',  ( 93.67499999999999716, 87.70503267997126784, 76.13583333333333769 ) ) ;
#48134 =( BOUNDED_CURVE ( )  B_SPLINE_CURVE ( 2, ( #14178, #48765, #64583, #2210, #19081, #13069, #31472 ),
 .UNSPECIFIED., .F., .F. ) 
 B_SPLINE_CURVE_WITH_KNOTS ( ( 3, 2, 2, 3 ),
 ( 0.2083333333333331483, 0.2152777777777775681, 0.2222222222222219323, 0.2291666666666663521 ),
 .UNSPECIFIED. ) 
 CURVE ( )  GEOMETRIC_REPRESENTATION_ITEM ( )  RATIONAL_B_SPLINE_CURVE ( ( 1.000000000000003775, 0.8660254037844349329, 1.000000000000000000, 0.8660254037844387076, 1.000000000000000000, 0.8660254037844445918, 0.9999999999999941158 ) ) 
 REPRESENTATION_ITEM ( '' )  );
#48135 = FACE_OUTER_BOUND ( 'NONE', #37392, .T. ) ;
#48136 = EDGE_CURVE ( 'NONE', #69025, #62465, #65510, .T. ) ;
#48137 = UNCERTAINTY_MEASURE_WITH_UNIT (LENGTH_MEASURE( 1.000000000000000082E-05 ), #12455, 'distance_accuracy_value', 'NONE');
#48138 = DIRECTION ( 'NONE',  ( -1.000000000000000000, -0.000000000000000000, -0.000000000000000000 ) ) ;
#48139 = DIRECTION ( 'NONE',  ( 0.000000000000000000, 0.8910065241883690090, -0.4539904997395446395 ) ) ;
#48140 = DIRECTION ( 'NONE',  ( -1.000000000000000000, 0.000000000000000000, -0.000000000000000000 ) ) ;
#48141 = LINE ( 'NONE', #53409, #57501 ) ;
#48142 = CARTESIAN_POINT ( 'NONE',  ( 11.99999999999999822, -72.35432306680469594, -20.40083707022958848 ) ) ;
#48143 = CARTESIAN_POINT ( 'NONE',  ( 10.00000000000000000, -27.13269053701078448, -25.88420570971428702 ) ) ;
#48144 = CARTESIAN_POINT ( 'NONE',  ( -94.99999999999997158, -206.9400435732949575, 89.20624999999999716 ) ) ;
#48145 = EDGE_CURVE ( 'NONE', #39502, #70850, #14725, .T. ) ;
#48146 = DIRECTION ( 'NONE',  ( -1.000000000000000000, -0.000000000000000000, 0.000000000000000000 ) ) ;
#48147 = EDGE_CURVE ( 'NONE', #33344, #19604, #37676, .T. ) ;
#48148 = VERTEX_POINT ( 'NONE', #42210 ) ;
#48149 = DIRECTION ( 'NONE',  ( 1.000000000000000000, 0.000000000000000000, 0.000000000000000000 ) ) ;
#48150 = LINE ( 'NONE', #15034, #37056 ) ;
#48151 = CARTESIAN_POINT ( 'NONE',  ( 0.3000000000000016542, 0.000000000000000000, 0.000000000000000000 ) ) ;
#48152 = FACE_OUTER_BOUND ( 'NONE', #62271, .T. ) ;
#48153 = VECTOR ( 'NONE', #8925, 1000.000000000000000 ) ;
#48154 = AXIS2_PLACEMENT_3D ( 'NONE', #32467, #73051, #44515 ) ;
#48155 = VECTOR ( 'NONE', #73071, 1000.000000000000000 ) ;
#48156 = ORIENTED_EDGE ( 'NONE', *, *, #3249, .F. ) ;
#48157 = LINE ( 'NONE', #36863, #7116 ) ;
#48158 = CARTESIAN_POINT ( 'NONE',  ( -97.65000000000001990, 90.00000000000004263, 90.00000000000000000 ) ) ;
#48159 = ORIENTED_EDGE ( 'NONE', *, *, #28774, .T. ) ;
#48160 = CARTESIAN_POINT ( 'NONE',  ( 92.69370383062501162, -208.6684592857803295, 81.33489583420048064 ) ) ;
#48161 = CARTESIAN_POINT ( 'NONE',  ( 93.84685191531251292, -211.9973110713294489, 87.36739583420049371 ) ) ;
#48162 = ORIENTED_EDGE ( 'NONE', *, *, #62213, .F. ) ;
#48163 = CARTESIAN_POINT ( 'NONE',  ( 95.00000000000000000, -207.3369185715606307, 89.64281250086715147 ) ) ;
#48164 = VECTOR ( 'NONE', #45089, 999.9999999999998863 ) ;
#48165 = ORIENTED_EDGE ( 'NONE', *, *, #18160, .T. ) ;
#48166 = CARTESIAN_POINT ( 'NONE',  ( 0.000000000000000000, 0.000000000000000000, 0.000000000000000000 ) ) ;
#48167 = VERTEX_POINT ( 'NONE', #48932 ) ;
#48168 = CIRCLE ( 'NONE', #54187, 77.49900000000002365 ) ;
#48169 = CARTESIAN_POINT ( 'NONE',  ( -96.15314808468751551, 88.00268892867056536, 77.84239583420048803 ) ) ;
#48170 = ORIENTED_EDGE ( 'NONE', *, *, #16066, .F. ) ;
#48171 = ORIENTED_EDGE ( 'NONE', *, *, #40825, .F. ) ;
#48172 = DIRECTION ( 'NONE',  ( -0.000000000000000000, -0.000000000000000000, -1.000000000000000000 ) ) ;
#48173 = ORIENTED_EDGE ( 'NONE', *, *, #16722, .F. ) ;
#48174 = DIRECTION ( 'NONE',  ( -0.000000000000000000, -0.6691306063588569053, -0.7431448254773954654 ) ) ;
#48175 = DIRECTION ( 'NONE',  ( -1.000000000000000000, -0.000000000000000000, 0.000000000000000000 ) ) ;
#48176 = ORIENTED_EDGE ( 'NONE', *, *, #48297, .T. ) ;
#48177 = DIRECTION ( 'NONE',  ( -1.000000000000000000, 0.000000000000000000, 0.000000000000000000 ) ) ;
#48178 = VERTEX_POINT ( 'NONE', #1650 ) ;
#48179 = DIRECTION ( 'NONE',  ( -1.000000000000000000, -0.000000000000000000, 0.000000000000000000 ) ) ;
#48180 = VERTEX_POINT ( 'NONE', #71859 ) ;
#48181 = ADVANCED_FACE ( 'NONE', ( #24902 ), #47471, .T. ) ;
#48182 = ORIENTED_EDGE ( 'NONE', *, *, #37118, .T. ) ;
#48183 = ORIENTED_EDGE ( 'NONE', *, *, #51590, .F. ) ;
#48184 = CARTESIAN_POINT ( 'NONE',  ( 93.84685191531251292, -211.9973110713294489, 79.58864583420047722 ) ) ;
#48185 = DIRECTION ( 'NONE',  ( 0.6862798483830554463, 0.7273375899149793211, -0.000000000000000000 ) ) ;
#48186 = CONTEXT_DEPENDENT_SHAPE_REPRESENTATION ( #13379, #41066 ) ;
#48187 = CARTESIAN_POINT ( 'NONE',  ( -92.35000000000003695, 90.00000000000004263, 82.06250000000000000 ) ) ;
#48188 = VERTEX_POINT ( 'NONE', #59492 ) ;
#48189 = CARTESIAN_POINT ( 'NONE',  ( -92.34999999999998010, -209.9999733970677482, 78.96687592183791082 ) ) ;
#48190 = LINE ( 'NONE', #24885, #41375 ) ;
#48191 = CARTESIAN_POINT ( 'NONE',  ( 0.000000000000000000, -39.04073710021356192, 15.48615015657568073 ) ) ;
#48192 = EDGE_CURVE ( 'NONE', #21370, #49839, #41823, .T. ) ;
#48193 = CARTESIAN_POINT ( 'NONE',  ( 11.99999999999999822, 66.50666863322055633, -39.78640506895536078 ) ) ;
#48194 = DIRECTION ( 'NONE',  ( -1.000000000000000000, 0.000000000000000000, -0.000000000000000000 ) ) ;
#48195 = CARTESIAN_POINT ( 'NONE',  ( -92.69370383062498320, -209.9999999999999716, 79.80031250086713612 ) ) ;
#48196 = EDGE_CURVE ( 'NONE', #32752, #12079, #36182, .T. ) ;
#48197 = CARTESIAN_POINT ( 'NONE',  ( -92.69370383062504004, 90.00000000000004263, 79.32406250086715715 ) ) ;
#48198 = ORIENTED_EDGE ( 'NONE', *, *, #29535, .F. ) ;
#48199 = CARTESIAN_POINT ( 'NONE',  ( 97.30629616937498838, 90.00000000000002842, 81.70531250086713726 ) ) ;
#48200 = VERTEX_POINT ( 'NONE', #70752 ) ;
#48201 = CARTESIAN_POINT ( 'NONE',  ( 96.32499999999997442, 92.29496732002878900, 78.43770833506764006 ) ) ;
#48202 = DIRECTION ( 'NONE',  ( 0.7585478161175716050, 0.6516173805718067369, 0.000000000000000000 ) ) ;
#48203 = CARTESIAN_POINT ( 'NONE',  ( -97.64999999953492704, -210.0000309987302956, 83.09538598079114990 ) ) ;
#48204 = CARTESIAN_POINT ( 'NONE',  ( 6.000000000000003553, 0.000000000000000000, -3.250000000000001332 ) ) ;
#48205 = CARTESIAN_POINT ( 'NONE',  ( -10.00000000000000000, 0.000000000000000000, 0.000000000000000000 ) ) ;
#48206 = CARTESIAN_POINT ( 'NONE',  ( -97.30629616937495996, -209.9999999999999716, 83.29281250086714294 ) ) ;
#48207 = EDGE_CURVE ( 'NONE', #48805, #29886, #7983, .T. ) ;
#48208 = AXIS2_PLACEMENT_3D ( 'NONE', #20106, #20495, #43064 ) ;
#48209 = AXIS2_PLACEMENT_3D ( 'NONE', #29782, #53107, #58005 ) ;
#48210 = DIRECTION ( 'NONE',  ( -0.000000000000000000, -0.000000000000000000, -1.000000000000000000 ) ) ;
#48211 = DIRECTION ( 'NONE',  ( 1.000000000000000000, 0.000000000000000000, -0.000000000000000000 ) ) ;
#48212 = CIRCLE ( 'NONE', #15790, 15.80000000000028315 ) ;
#48213 = CARTESIAN_POINT ( 'NONE',  ( -5.000000000000000000, -2.886751345948133540, -6.000000000000000000 ) ) ;
#48214 = ORIENTED_EDGE ( 'NONE', *, *, #4766, .T. ) ;
#48215 = AXIS2_PLACEMENT_3D ( 'NONE', #12148, #41836, #35094 ) ;
#48216 = ORIENTED_EDGE ( 'NONE', *, *, #31381, .F. ) ;
#48217 = CARTESIAN_POINT ( 'NONE',  ( 5.000000000000000000, 71.21200624218795383, 40.65526001592638039 ) ) ;
#48218 = CARTESIAN_POINT ( 'NONE',  ( 10.00000000000000000, -73.44644590900078640, 24.73286445877676343 ) ) ;
#48219 = CARTESIAN_POINT ( 'NONE',  ( 10.00000000000000000, 77.19088730480524418, 6.903761155838049390 ) ) ;
#48220 = CIRCLE ( 'NONE', #52994, 16.00000000000000000 ) ;
#48221 = CARTESIAN_POINT ( 'NONE',  ( -92.69370383062504004, 90.00000000000004263, 86.15031250086714465 ) ) ;
#48222 = DIRECTION ( 'NONE',  ( -1.000000000000000000, 0.000000000000000000, 0.000000000000000000 ) ) ;
#48223 = CYLINDRICAL_SURFACE ( 'NONE', #58999, 12.49999999999999822 ) ;
#48224 = CARTESIAN_POINT ( 'NONE',  ( -2.499999999999970690, 73.00000000000001421, -204.9999999999999716 ) ) ;
#48225 = EDGE_CURVE ( 'NONE', #47275, #36497, #25283, .T. ) ;
#48226 = EDGE_LOOP ( 'NONE', ( #64920, #33150, #28660, #69363 ) ) ;
#48227 = CARTESIAN_POINT ( 'NONE',  ( -93.84685191531254134, 91.99731107132950569, 75.46114583420047950 ) ) ;
#48228 = VECTOR ( 'NONE', #41013, 1000.000000000000000 ) ;
#48229 = DIRECTION ( 'NONE',  ( -1.000000000000000000, 0.000000000000000000, 0.000000000000000000 ) ) ;
#48230 = AXIS2_PLACEMENT_3D ( 'NONE', #50673, #73601, #11202 ) ;
#48231 = LINE ( 'NONE', #59515, #21403 ) ;
#48232 = DIRECTION ( 'NONE',  ( 1.000000000000000000, -0.000000000000000000, -0.000000000000000000 ) ) ;
#48233 = DIRECTION ( 'NONE',  ( 0.000000000000000000, 0.000000000000000000, -1.000000000000000000 ) ) ;
#48234 = DIRECTION ( 'NONE',  ( 0.000000000000000000, 0.8090169943749486725, -0.5877852522924713607 ) ) ;
#48235 = CARTESIAN_POINT ( 'NONE',  ( -97.30629616937497417, -208.6684592857803011, 82.76364583420048859 ) ) ;
#48236 = SURFACE_STYLE_FILL_AREA ( #60634 ) ;
#48237 = EDGE_CURVE ( 'NONE', #30123, #69332, #52959, .T. ) ;
#48238 = CARTESIAN_POINT ( 'NONE',  ( 7.893099573151324044, -11.68370571044642503, -1.199999999999999956 ) ) ;
#48239 = EDGE_CURVE ( 'NONE', #4854, #42442, #3859, .T. ) ;
#48240 = EDGE_CURVE ( 'NONE', #57167, #25433, #21466, .T. ) ;
#48241 = DIRECTION ( 'NONE',  ( 0.000000000000000000, 0.000000000000000000, 1.000000000000000000 ) ) ;
#48242 = CARTESIAN_POINT ( 'NONE',  ( -97.30629616937497417, -208.6684592857803295, 75.77864583420048916 ) ) ;
#48243 = CARTESIAN_POINT ( 'NONE',  ( 0.000000000000000000, 0.000000000000000000, 0.000000000000000000 ) ) ;
#48244 = VERTEX_POINT ( 'NONE', #32011 ) ;
#48245 = DIRECTION ( 'NONE',  ( -0.000000000000000000, -0.000000000000000000, 1.000000000000000000 ) ) ;
#48246 = LINE ( 'NONE', #35478, #69480 ) ;
#48247 = CARTESIAN_POINT ( 'NONE',  ( 95.00000000000000000, -206.9400435732949575, 79.68124999999999147 ) ) ;
#48248 = CARTESIAN_POINT ( 'NONE',  ( 0.000000000000000000, 0.000000000000000000, 0.000000000000000000 ) ) ;
#48249 = CARTESIAN_POINT ( 'NONE',  ( 92.69370383062501162, -208.6684592857803011, 74.98489583420048632 ) ) ;
#48250 = ORIENTED_EDGE ( 'NONE', *, *, #13986, .T. ) ;
#48251 = CYLINDRICAL_SURFACE ( 'NONE', #55260, 82.00000000000000000 ) ;
#48252 = CARTESIAN_POINT ( 'NONE',  ( 0.000000000000000000, -10.30890764327323161, -81.34940948281348483 ) ) ;
#48253 = VERTEX_POINT ( 'NONE', #27860 ) ;
#48254 = DIRECTION ( 'NONE',  ( 0.000000000000000000, 6.938893903907228378E-16, 1.000000000000000000 ) ) ;
#48255 = ORIENTED_EDGE ( 'NONE', *, *, #16187, .T. ) ;
#48256 = CIRCLE ( 'NONE', #69870, 82.00000000000000000 ) ;
#48257 = CYLINDRICAL_SURFACE ( 'NONE', #23822, 31.99999999999998579 ) ;
#48258 = ORIENTED_EDGE ( 'NONE', *, *, #54821, .T. ) ;
#48259 = VERTEX_POINT ( 'NONE', #66967 ) ;
#48260 = ORIENTED_EDGE ( 'NONE', *, *, #14015, .T. ) ;
#48261 = CARTESIAN_POINT ( 'NONE',  ( 0.000000000000000000, 0.000000000000000000, 0.000000000000000000 ) ) ;
#48262 = VECTOR ( 'NONE', #47384, 1000.000000000000000 ) ;
#48263 = EDGE_LOOP ( 'NONE', ( #68519, #28180, #57469, #13194 ) ) ;
#48264 = VECTOR ( 'NONE', #14891, 1000.000000000000000 ) ;
#48265 = ORIENTED_EDGE ( 'NONE', *, *, #24759, .F. ) ;
#48266 = CARTESIAN_POINT ( 'NONE',  ( 96.15314808468748708, 88.00268892867053694, 79.85322916753381151 ) ) ;
#48267 = CARTESIAN_POINT ( 'NONE',  ( 0.000000000000000000, 37.22597642581158084, 10.79786254984347593 ) ) ;
#48268 = DIRECTION ( 'NONE',  ( -1.000000000000000000, -0.000000000000000000, 0.000000000000000000 ) ) ;
#48269 = VERTEX_POINT ( 'NONE', #62089 ) ;
#48270 = ORIENTED_EDGE ( 'NONE', *, *, #55183, .F. ) ;
#48271 = ADVANCED_FACE ( 'NONE', ( #72963 ), #26740, .T. ) ;
#48272 = ORIENTED_EDGE ( 'NONE', *, *, #28181, .T. ) ;
#48273 = CYLINDRICAL_SURFACE ( 'NONE', #21459, 31.99999999999997868 ) ;
#48274 = CIRCLE ( 'NONE', #48333, 31.99999999999998224 ) ;
#48275 = ORIENTED_EDGE ( 'NONE', *, *, #41680, .F. ) ;
#48276 = CIRCLE ( 'NONE', #5096, 31.99999999999998579 ) ;
#48277 = DIRECTION ( 'NONE',  ( -0.3731444310164280243, 0.9277732662679100128, 1.592504622367969680E-16 ) ) ;
#48278 = DIRECTION ( 'NONE',  ( -1.000000000000000000, -0.000000000000000000, -0.000000000000000000 ) ) ;
#48279 = FACE_OUTER_BOUND ( 'NONE', #54184, .T. ) ;
#48280 = LINE ( 'NONE', #55023, #67770 ) ;
#48281 = CARTESIAN_POINT ( 'NONE',  ( -94.99999999999997158, -206.9400435732949575, 84.20562500173429044 ) ) ;
#48282 = ADVANCED_FACE ( 'NONE', ( #4959 ), #38408, .T. ) ;
#48283 = CARTESIAN_POINT ( 'NONE',  ( 5.000000000000002665, 39.47590169984944453, -71.87247863392373404 ) ) ;
#48284 = CARTESIAN_POINT ( 'NONE',  ( 10.00000000000000000, 73.73191006444551476, 14.66109333815590254 ) ) ;
#48285 = CARTESIAN_POINT ( 'NONE',  ( -93.67499999999998295, -207.7050326799711968, 74.62770833506762358 ) ) ;
#48286 = EDGE_CURVE ( 'NONE', #68809, #38655, #16584, .T. ) ;
#48287 = DIRECTION ( 'NONE',  ( -1.000000000000000000, -0.000000000000000000, 0.000000000000000000 ) ) ;
#48289 = CARTESIAN_POINT ( 'NONE',  ( -93.67500000000003979, 87.70503267997129626, 75.05104166840095559 ) ) ;
#48288 = CARTESIAN_POINT ( 'NONE',  ( 97.64999999999997726, 91.52997821335252127, 75.20979166840096752 ) ) ;
#48290 = VERTEX_POINT ( 'NONE', #9088 ) ;
#48291 = CARTESIAN_POINT ( 'NONE',  ( 92.69370383062498320, 91.33154071421968467, 75.77864583420048916 ) ) ;
#48292 = DIRECTION ( 'NONE',  ( -1.000000000000000000, 0.000000000000000000, 0.000000000000000000 ) ) ;
#48293 = DIRECTION ( 'NONE',  ( -0.5687579148473752566, 0.8225049752423786442, 0.000000000000000000 ) ) ;
#48294 = LINE ( 'NONE', #30255, #56381 ) ;
#48295 = CARTESIAN_POINT ( 'NONE',  ( 93.67500000000001137, -212.2949673200287179, 77.48520833506763950 ) ) ;
#48296 = DIRECTION ( 'NONE',  ( -1.000000000000000000, -0.000000000000000000, -0.000000000000000000 ) ) ;
#48297 = EDGE_CURVE ( 'NONE', #65655, #39425, #61348, .T. ) ;
#48298 = ORIENTED_EDGE ( 'NONE', *, *, #7576, .F. ) ;
#48299 = CARTESIAN_POINT ( 'NONE',  ( 11.99999999999999822, -65.59268652807183742, -36.72794159290312166 ) ) ;
#48300 = DIRECTION ( 'NONE',  ( -1.000000000000000000, -0.000000000000000000, 0.000000000000000000 ) ) ;
#48301 = ORIENTED_EDGE ( 'NONE', *, *, #51638, .T. ) ;
#48302 = VERTEX_POINT ( 'NONE', #73343 ) ;
#48303 = DIRECTION ( 'NONE',  ( 0.000000000000000000, 0.000000000000000000, -1.000000000000000000 ) ) ;
#48304 = CARTESIAN_POINT ( 'NONE',  ( 97.65000000000003411, -208.4700217866474929, 82.75041666666666629 ) ) ;
#48305 = LINE ( 'NONE', #38132, #43559 ) ;
#48306 = CYLINDRICAL_SURFACE ( 'NONE', #5155, 32.00000000000000000 ) ;
#48307 = DIRECTION ( 'NONE',  ( 0.000000000000000000, 0.000000000000000000, -1.000000000000000000 ) ) ;
#48308 = CARTESIAN_POINT ( 'NONE',  ( -10.00000000000000000, 0.000000000000000000, 0.000000000000000000 ) ) ;
#48309 = EDGE_CURVE ( 'NONE', #48877, #23492, #8623, .T. ) ;
#48310 = ORIENTED_EDGE ( 'NONE', *, *, #1685, .F. ) ;
#48311 =( GEOMETRIC_REPRESENTATION_CONTEXT ( 3 ) GLOBAL_UNCERTAINTY_ASSIGNED_CONTEXT ( ( #60177 ) ) GLOBAL_UNIT_ASSIGNED_CONTEXT ( ( #35673, #70248, #32250 ) ) REPRESENTATION_CONTEXT ( 'NONE', 'WORKASPACE' ) );
#48312 = DIRECTION ( 'NONE',  ( -1.000000000000000000, 0.000000000000000000, 0.000000000000000000 ) ) ;
#48313 = CARTESIAN_POINT ( 'NONE',  ( 0.000000000000000000, 75.54627589209970040, -17.28742895386005785 ) ) ;
#48314 = AXIS2_PLACEMENT_3D ( 'NONE', #979, #52062, #23141 ) ;
#48315 = FACE_OUTER_BOUND ( 'NONE', #50458, .T. ) ;
#48316 = DIRECTION ( 'NONE',  ( -1.000000000000000000, -0.000000000000000000, -0.000000000000000000 ) ) ;
#48317 = CARTESIAN_POINT ( 'NONE',  ( 5.000000000000002665, 3.894527615417891830, 81.90746397400390322 ) ) ;
#48318 = DIRECTION ( 'NONE',  ( -1.000000000000000000, 0.000000000000000000, 0.000000000000000000 ) ) ;
#48319 = PRODUCT_DEFINITION_CONTEXT ( 'detailed design', #44574, 'design' ) ;
#48320 = CARTESIAN_POINT ( 'NONE',  ( 0.000000000000000000, 0.000000000000000000, 0.000000000000000000 ) ) ;
#48321 = DIRECTION ( 'NONE',  ( 0.000000000000000000, 0.000000000000000000, 1.000000000000000000 ) ) ;
#48322 = PLANE ( 'NONE',  #69402 ) ;
#48323 = EDGE_CURVE ( 'NONE', #47697, #49297, #49307, .T. ) ;
#48324 = EDGE_CURVE ( 'NONE', #11454, #73113, #68093, .T. ) ;
#48325 = VECTOR ( 'NONE', #13049, 1000.000000000000114 ) ;
#48326 = CARTESIAN_POINT ( 'NONE',  ( 92.69370383062498320, 90.00000000000002842, 84.08656250086716000 ) ) ;
#48327 = CARTESIAN_POINT ( 'NONE',  ( -93.84685191531248449, -208.0026889286704943, 86.41489583420049314 ) ) ;
#48328 = CARTESIAN_POINT ( 'NONE',  ( 95.00000000000000000, -213.0599564267049857, 83.88812500173429498 ) ) ;
#48329 = ORIENTED_EDGE ( 'NONE', *, *, #60635, .F. ) ;
#48330 = DIRECTION ( 'NONE',  ( 1.000000000000000000, 0.000000000000000000, -0.000000000000000000 ) ) ;
#48331 = CARTESIAN_POINT ( 'NONE',  ( -97.64999999999994884, -211.5299782133524502, 81.79791666666666572 ) ) ;
#48332 = CARTESIAN_POINT ( 'NONE',  ( -97.30629616937501680, 91.33154071421968467, 77.52489583420046415 ) ) ;
#48333 = AXIS2_PLACEMENT_3D ( 'NONE', #10434, #61579, #16452 ) ;
#48334 = CIRCLE ( 'NONE', #3913, 82.00000000000000000 ) ;
#48335 = CARTESIAN_POINT ( 'NONE',  ( 97.30629616937498838, -209.9999999999999716, 84.88031250086713442 ) ) ;
#48336 = VERTEX_POINT ( 'NONE', #72592 ) ;
#48337 = LINE ( 'NONE', #395, #59839 ) ;
#48338 = ORIENTED_EDGE ( 'NONE', *, *, #12080, .F. ) ;
#48339 = EDGE_LOOP ( 'NONE', ( #45455, #52057, #63557, #58061 ) ) ;
#48340 = CARTESIAN_POINT ( 'NONE',  ( 97.64999999999992042, -208.4700217866474361, 84.02041666666666231 ) ) ;
#48341 = ORIENTED_EDGE ( 'NONE', *, *, #37770, .F. ) ;
#48342 = CYLINDRICAL_SURFACE ( 'NONE', #39631, 31.99999999999998579 ) ;
#48343 = CARTESIAN_POINT ( 'NONE',  ( 97.30629616937498838, -209.9999999999999716, 79.32406250086715715 ) ) ;
#48344 = DIRECTION ( 'NONE',  ( -1.000000000000000000, -0.000000000000000000, -0.000000000000000000 ) ) ;
#48345 = DIRECTION ( 'NONE',  ( 1.000000000000000000, -0.000000000000000000, 0.000000000000000000 ) ) ;
#48346 = EDGE_CURVE ( 'NONE', #13386, #31034, #25417, .T. ) ;
#48347 = CARTESIAN_POINT ( 'NONE',  ( 0.000000000000000000, 0.000000000000000000, 0.000000000000000000 ) ) ;
#48348 =( BOUNDED_CURVE ( )  B_SPLINE_CURVE ( 2, ( #34914, #40548, #11235, #17985, #6352, #45843, #45092 ),
 .UNSPECIFIED., .F., .F. ) 
 B_SPLINE_CURVE_WITH_KNOTS ( ( 3, 2, 2, 3 ),
 ( 0.9374999999999995559, 0.9444444444444441977, 0.9513888888888889506, 0.9583333333333337034 ),
 .UNSPECIFIED. ) 
 CURVE ( )  GEOMETRIC_REPRESENTATION_ITEM ( )  RATIONAL_B_SPLINE_CURVE ( ( 1.000000000000008660, 0.8660254037844301589, 1.000000000000000000, 0.8660254037844387076, 1.000000000000000000, 0.8660254037844322683, 1.000000000000006439 ) ) 
 REPRESENTATION_ITEM ( '' )  );
#48349 = DIRECTION ( 'NONE',  ( 0.000000000000000000, 0.000000000000000000, 1.000000000000000000 ) ) ;
#48350 = CYLINDRICAL_SURFACE ( 'NONE', #63385, 16.00000000000000000 ) ;
#48351 = CARTESIAN_POINT ( 'NONE',  ( 95.00000000000000000, -213.0599564267049857, 80.63375000000000625 ) ) ;
#48352 = EDGE_CURVE ( 'NONE', #73475, #49826, #19449, .T. ) ;
#48353 = ORIENTED_EDGE ( 'NONE', *, *, #63526, .T. ) ;
#48354 = ORIENTED_EDGE ( 'NONE', *, *, #14767, .T. ) ;
#48355 = ORIENTED_EDGE ( 'NONE', *, *, #6202, .F. ) ;
#48356 = ORIENTED_EDGE ( 'NONE', *, *, #23770, .F. ) ;
#48357 = CARTESIAN_POINT ( 'NONE',  ( 0.000000000000000000, 0.000000000000000000, 0.000000000000000000 ) ) ;
#48358 = EDGE_CURVE ( 'NONE', #65292, #64440, #27103, .T. ) ;
#48359 = AXIS2_PLACEMENT_3D ( 'NONE', #36620, #66326, #54657 ) ;
#48360 = FILL_AREA_STYLE_COLOUR ( '', #69929 ) ;
#48361 = CARTESIAN_POINT ( 'NONE',  ( -97.30629616937501680, 91.33154071421968467, 82.76364583420048859 ) ) ;
#48362 = CARTESIAN_POINT ( 'NONE',  ( 94.99999999999998579, 86.94004357329502852, 88.33312500173431658 ) ) ;
#48363 = CARTESIAN_POINT ( 'NONE',  ( 100.0000000000260343, -214.9999999999999716, -64.99999999999350564 ) ) ;
#48364 = EDGE_CURVE ( 'NONE', #4011, #6866, #56067, .T. ) ;
#48365 = CARTESIAN_POINT ( 'NONE',  ( 92.34999999999999432, 91.52997821335252127, 75.34208333333333485 ) ) ;
#48366 = ORIENTED_EDGE ( 'NONE', *, *, #57155, .F. ) ;
#48367 = CARTESIAN_POINT ( 'NONE',  ( -93.67499999999998295, -207.7050326799711968, 84.78770833506763438 ) ) ;
#48368 = ORIENTED_EDGE ( 'NONE', *, *, #39247, .F. ) ;
#48369 = CARTESIAN_POINT ( 'NONE',  ( 23.49916127795269460, -121.5130826919798039, 5.500000000000000000 ) ) ;
#48370 = ORIENTED_EDGE ( 'NONE', *, *, #16647, .F. ) ;
#48371 = CARTESIAN_POINT ( 'NONE',  ( -92.35000000000003695, 90.00000000000004263, 85.95187500173430806 ) ) ;
#48372 = CIRCLE ( 'NONE', #24338, 31.99999999999998934 ) ;
#48373 = CARTESIAN_POINT ( 'NONE',  ( 94.99999999999998579, 92.66308142843935514, 86.46781250086716852 ) ) ;
#48374 = CARTESIAN_POINT ( 'NONE',  ( -92.34999999999999432, -209.9999999999999716, 80.15749999999999886 ) ) ;
#48375 = CARTESIAN_POINT ( 'NONE',  ( -92.35000000000003695, 89.99999997442942856, 84.04687500080852658 ) ) ;
#48376 = CYLINDRICAL_SURFACE ( 'NONE', #69016, 2.649999999999985700 ) ;
#48377 = EDGE_CURVE ( 'NONE', #47617, #69188, #36247, .T. ) ;
#48378 = LINE ( 'NONE', #28403, #4883 ) ;
#48379 = ORIENTED_EDGE ( 'NONE', *, *, #29121, .F. ) ;
#48380 = CARTESIAN_POINT ( 'NONE',  ( 1.443735181952766844, -4.939961795957303003, -5.918341802876224911 ) ) ;
#48381 = AXIS2_PLACEMENT_3D ( 'NONE', #7169, #25197, #51641 ) ;
#48382 = LINE ( 'NONE', #46916, #57583 ) ;
#48383 = VERTEX_POINT ( 'NONE', #50787 ) ;
#48384 = ORIENTED_EDGE ( 'NONE', *, *, #65606, .F. ) ;
#48385 = CARTESIAN_POINT ( 'NONE',  ( 97.64999999999999147, 90.00000000000002842, 78.96687500173429441 ) ) ;
#48386 = CARTESIAN_POINT ( 'NONE',  ( 0.000000000000000000, 20.85821328998756385, -10.92862929874494959 ) ) ;
#48387 = ADVANCED_FACE ( 'NONE', ( #9456 ), #33119, .T. ) ;
#48388 = FACE_OUTER_BOUND ( 'NONE', #68816, .T. ) ;
#48389 = CARTESIAN_POINT ( 'NONE',  ( -92.69370383062498320, -211.3315407142195852, 83.08114583420048405 ) ) ;
#48390 = ORIENTED_EDGE ( 'NONE', *, *, #71770, .F. ) ;
#48391 = CARTESIAN_POINT ( 'NONE',  ( -92.35000000000002274, -211.5299782133524786, 82.64458333333332973 ) ) ;
#48392 = ADVANCED_FACE ( 'NONE', ( #38777 ), #61714, .F. ) ;
#48393 = ORIENTED_EDGE ( 'NONE', *, *, #70005, .T. ) ;
#48394 = EDGE_LOOP ( 'NONE', ( #67706, #11213, #29574, #69974 ) ) ;
#48395 = LINE ( 'NONE', #70946, #42645 ) ;
#48396 = EDGE_CURVE ( 'NONE', #30113, #62276, #28228, .T. ) ;
#48397 = EDGE_CURVE ( 'NONE', #62137, #13883, #69205, .T. ) ;
#48398 = CARTESIAN_POINT ( 'NONE',  ( 92.69370383062498320, 88.66845928578037217, 88.58447916753382856 ) ) ;
#48399 = DIRECTION ( 'NONE',  ( -1.000000000000000000, 0.000000000000000000, 0.000000000000000000 ) ) ;
#48400 = CARTESIAN_POINT ( 'NONE',  ( 96.15314808468748708, 88.00268892867053694, 81.59947916753381492 ) ) ;
#48401 = DIRECTION ( 'NONE',  ( -1.000000000000000000, -0.000000000000000000, 0.000000000000000000 ) ) ;
#48402 = CARTESIAN_POINT ( 'NONE',  ( -96.32500000000001705, 92.29496732002878900, 80.44854166840097776 ) ) ;
#48403 = DIRECTION ( 'NONE',  ( -1.000000000000000000, -0.000000000000000000, -0.000000000000000000 ) ) ;
#48404 = CARTESIAN_POINT ( 'NONE',  ( 0.000000000000000000, -36.72794159290197769, -65.59268652807249111 ) ) ;
#48405 = DIRECTION ( 'NONE',  ( -2.603472992746261562E-14, -2.546204323184492723E-14, 1.000000000000000000 ) ) ;
#48406 = DIRECTION ( 'NONE',  ( -0.000000000000000000, -0.000000000000000000, 1.000000000000000000 ) ) ;
#48407 = ADVANCED_FACE ( 'NONE', ( #6432 ), #22985, .T. ) ;
#48408 = APPLICATION_CONTEXT ( 'automotive_design' ) ;
#48409 = CARTESIAN_POINT ( 'NONE',  ( 4.999999999999999112, 40.98264845739749518, 9.188173127307448951 ) ) ;
#48410 = PRODUCT_DEFINITION_CONTEXT ( 'detailed design', #59957, 'design' ) ;
#48411 = EDGE_CURVE ( 'NONE', #22350, #51185, #45554, .T. ) ;
#48412 = AXIS2_PLACEMENT_3D ( 'NONE', #34777, #53178, #6222 ) ;
#48413 = DIRECTION ( 'NONE',  ( 0.000000000000000000, 0.000000000000000000, -1.000000000000000000 ) ) ;
#48414 = ORIENTED_EDGE ( 'NONE', *, *, #24809, .T. ) ;
#48415 = CARTESIAN_POINT ( 'NONE',  ( -92.69370383062505425, 91.33154071421968467, 86.83822916753381094 ) ) ;
#48416 = DIRECTION ( 'NONE',  ( -1.000000000000000000, -0.000000000000000000, -0.000000000000000000 ) ) ;
#48417 = VECTOR ( 'NONE', #35314, 1000.000000000000000 ) ;
#48418 = DIRECTION ( 'NONE',  ( 0.000000000000000000, 0.1045284632676449221, -0.9945218953682741780 ) ) ;
#48419 = VERTEX_POINT ( 'NONE', #16965 ) ;
#48420 = VECTOR ( 'NONE', #60387, 1000.000000000000000 ) ;
#48421 = CARTESIAN_POINT ( 'NONE',  ( 0.000000000000000000, 58.39081064771751528, 50.95692526931350841 ) ) ;
#48423 = CARTESIAN_POINT ( 'NONE',  ( -3.000000000000000000, -0.9646360437375307573, 23.52805723605590060 ) ) ;
#48422 = AXIS2_PLACEMENT_3D ( 'NONE', #1582, #36852, #47404 ) ;
#48424 = DIRECTION ( 'NONE',  ( -1.000000000000000000, 0.000000000000000000, -0.000000000000000000 ) ) ;
#48425 = CIRCLE ( 'NONE', #49599, 82.00000000000000000 ) ;
#48426 = VECTOR ( 'NONE', #1575, 1000.000000000000000 ) ;
#48427 = AXIS2_PLACEMENT_3D ( 'NONE', #71693, #43535, #66448 ) ;
#48428 = CARTESIAN_POINT ( 'NONE',  ( 97.30629616937498838, -211.3315407142195852, 80.54114583420049200 ) ) ;
#48429 = ORIENTED_EDGE ( 'NONE', *, *, #41261, .T. ) ;
#48430 = ORIENTED_EDGE ( 'NONE', *, *, #8309, .T. ) ;
#48431 = FACE_OUTER_BOUND ( 'NONE', #41889, .T. ) ;
#48432 = ORIENTED_EDGE ( 'NONE', *, *, #41832, .T. ) ;
#48433 = CARTESIAN_POINT ( 'NONE',  ( 0.000000000000000000, 77.16300072079698680, -27.74655509720590985 ) ) ;
#48434 = FACE_OUTER_BOUND ( 'NONE', #41755, .T. ) ;
#48435 = ORIENTED_EDGE ( 'NONE', *, *, #12711, .F. ) ;
#48436 = CARTESIAN_POINT ( 'NONE',  ( 96.15314808468750130, -211.9973110713294489, 76.67822916753381435 ) ) ;
#48437 = EDGE_LOOP ( 'NONE', ( #53166, #34603, #67103, #10555 ) ) ;
#48438 = EDGE_CURVE ( 'NONE', #73701, #1246, #15807, .T. ) ;
#48439 = CARTESIAN_POINT ( 'NONE',  ( 15.00000000000000000, -14.54903810567644484, 22.19967320028775504 ) ) ;
#48440 = VERTEX_POINT ( 'NONE', #12422 ) ;
#48441 = VERTEX_POINT ( 'NONE', #45918 ) ;
#48442 = DIRECTION ( 'NONE',  ( 0.000000000000000000, 0.000000000000000000, -1.000000000000000000 ) ) ;
#48443 = EDGE_CURVE ( 'NONE', #28069, #11579, #57847, .T. ) ;
#48444 = CARTESIAN_POINT ( 'NONE',  ( -3.000000000000000000, -23.29833615347109443, 3.418703333116492438 ) ) ;
#48445 = ORIENTED_EDGE ( 'NONE', *, *, #24460, .T. ) ;
#48446 = CARTESIAN_POINT ( 'NONE',  ( 0.000000000000000000, -31.52238457039619490, 27.75498641678731104 ) ) ;
#48447 = CARTESIAN_POINT ( 'NONE',  ( 95.00000000000000000, -206.9400435732949575, 84.20562500173429044 ) ) ;
#48448 = EDGE_CURVE ( 'NONE', #10067, #54928, #29064, .T. ) ;
#48449 = CARTESIAN_POINT ( 'NONE',  ( 94.99999999999998579, 93.05995642670504253, 84.76125000000000398 ) ) ;
#48450 = EDGE_CURVE ( 'NONE', #48097, #53076, #61486, .T. ) ;
#48451 = VERTEX_POINT ( 'NONE', #23706 ) ;
#48452 = DIRECTION ( 'NONE',  ( -1.000000000000000000, -0.000000000000000000, 0.000000000000000000 ) ) ;
#48453 = LINE ( 'NONE', #65026, #57314 ) ;
#48454 = AXIS2_PLACEMENT_3D ( 'NONE', #7366, #53227, #15214 ) ;
#48455 = ORIENTED_EDGE ( 'NONE', *, *, #28881, .F. ) ;
#48456 = ORIENTED_EDGE ( 'NONE', *, *, #55243, .T. ) ;
#48457 = CARTESIAN_POINT ( 'NONE',  ( -97.30629616937501680, 91.33154071421968467, 86.57364583420047666 ) ) ;
#48458 = CARTESIAN_POINT ( 'NONE',  ( 92.69370383062498320, 90.00000000000002842, 80.11781250086713158 ) ) ;
#48459 = VERTEX_POINT ( 'NONE', #46642 ) ;
#48460 = CARTESIAN_POINT ( 'NONE',  ( 96.32499999999998863, 87.70503267997126784, 82.67104166840096013 ) ) ;
#48461 = AXIS2_PLACEMENT_3D ( 'NONE', #3138, #10590, #37703 ) ;
#48462 = FACE_OUTER_BOUND ( 'NONE', #46287, .T. ) ;
#48463 = CARTESIAN_POINT ( 'NONE',  ( 11.41210121379328335, -99.40233154247455616, 5.500000000000000000 ) ) ;
#48464 = EDGE_LOOP ( 'NONE', ( #54394, #64617, #42253, #46407 ) ) ;
#48465 = CARTESIAN_POINT ( 'NONE',  ( 97.64999999999999147, -209.9999999999999716, 78.25249999999999773 ) ) ;
#48466 = ORIENTED_EDGE ( 'NONE', *, *, #1133, .T. ) ;
#48467 = AXIS2_PLACEMENT_3D ( 'NONE', #8869, #31784, #42349 ) ;
#48468 = ORIENTED_EDGE ( 'NONE', *, *, #23285, .F. ) ;
#48469 = ADVANCED_FACE ( 'NONE', ( #62472 ), #62852, .F. ) ;
#48470 = ORIENTED_EDGE ( 'NONE', *, *, #59584, .T. ) ;
#48471 = DIRECTION ( 'NONE',  ( 0.000000000000000000, 0.000000000000000000, -1.000000000000000000 ) ) ;
#48472 = CARTESIAN_POINT ( 'NONE',  ( 0.000000000000000000, 0.000000000000000000, 0.000000000000000000 ) ) ;
#48473 = EDGE_CURVE ( 'NONE', #63672, #37478, #38677, .T. ) ;
#48474 = CARTESIAN_POINT ( 'NONE',  ( -97.65000000000001990, 88.47002178664754979, 84.33791666666667197 ) ) ;
#48475 = EDGE_LOOP ( 'NONE', ( #34849, #67564, #18048, #73948 ) ) ;
#48476 = CYLINDRICAL_SURFACE ( 'NONE', #5964, 31.99999999999998579 ) ;
#48477 = VECTOR ( 'NONE', #37638, 1000.000000000000000 ) ;
#48478 = FACE_OUTER_BOUND ( 'NONE', #45306, .T. ) ;
#48479 = VERTEX_POINT ( 'NONE', #11313 ) ;
#48480 = CARTESIAN_POINT ( 'NONE',  ( 97.64999999999994884, -211.5299782133524786, 85.18458333333332178 ) ) ;
#48481 = CARTESIAN_POINT ( 'NONE',  ( -92.69370383062498320, -211.3315407142195852, 79.74739583420047495 ) ) ;
#48482 = ORIENTED_EDGE ( 'NONE', *, *, #68133, .T. ) ;
#48483 = LINE ( 'NONE', #71398, #26611 ) ;
#48484 = DIRECTION ( 'NONE',  ( -1.000000000000000000, 0.000000000000000000, 0.000000000000000000 ) ) ;
#48485 = CARTESIAN_POINT ( 'NONE',  ( 0.000000000000000000, 2.543863470249533965, -81.96053171279901051 ) ) ;
#48486 = CARTESIAN_POINT ( 'NONE',  ( 15.00000000000000000, -23.29833615347104470, 3.418703333116808629 ) ) ;
#48487 = DIRECTION ( 'NONE',  ( 0.000000000000000000, 0.000000000000000000, 1.000000000000000000 ) ) ;
#48488 = VECTOR ( 'NONE', #39355, 1000.000000000000000 ) ;
#48489 = ADVANCED_FACE ( 'NONE', ( #17330 ), #452, .F. ) ;
#48491 = EDGE_CURVE ( 'NONE', #55710, #69920, #2651, .T. ) ;
#48490 = AXIS2_PLACEMENT_3D ( 'NONE', #42499, #42137, #54156 ) ;
#48492 = CYLINDRICAL_SURFACE ( 'NONE', #46943, 31.99999999999998579 ) ;
#48493 = CARTESIAN_POINT ( 'NONE',  ( -10.00000000000000000, 0.000000000000000000, 0.000000000000000000 ) ) ;
#48494 = CARTESIAN_POINT ( 'NONE',  ( 0.000000000000000000, -26.23277895567251505, 4.042438405569750870 ) ) ;
#48495 = FACE_OUTER_BOUND ( 'NONE', #58996, .T. ) ;
#48496 = CARTESIAN_POINT ( 'NONE',  ( -97.64998927488629477, -208.4700155945002393, 86.85145790673762178 ) ) ;
#48497 = CARTESIAN_POINT ( 'NONE',  ( -93.84685191531252713, 88.00268892867056536, 75.24947916753380639 ) ) ;
#48498 = CARTESIAN_POINT ( 'NONE',  ( 0.000000000000000000, -71.87247863392384772, -39.47590169984923136 ) ) ;
#48499 = CARTESIAN_POINT ( 'NONE',  ( -1.250000000000000444, -16.78109714094927085, -1.199999999999999956 ) ) ;
#48500 = FACE_OUTER_BOUND ( 'NONE', #5686, .T. ) ;
#48501 = DIRECTION ( 'NONE',  ( -0.9580045777625459946, -0.2867529058022011412, 0.000000000000000000 ) ) ;
#48502 = AXIS2_PLACEMENT_3D ( 'NONE', #41081, #45983, #46343 ) ;
#48503 = DIRECTION ( 'NONE',  ( -1.000000000000000000, 0.000000000000000000, -0.000000000000000000 ) ) ;
#48504 = DIRECTION ( 'NONE',  ( -0.9227826878668540234, -0.3853207896976547642, 0.000000000000000000 ) ) ;
#48505 = DIRECTION ( 'NONE',  ( 0.000000000000000000, 0.000000000000000000, 1.000000000000000000 ) ) ;
#48506 = CARTESIAN_POINT ( 'NONE',  ( 96.32499999999998863, -212.2949673200287179, 78.78166666666666629 ) ) ;
#48507 = DIRECTION ( 'NONE',  ( -1.000000000000000000, -0.000000000000000000, 0.000000000000000000 ) ) ;
#48508 = CARTESIAN_POINT ( 'NONE',  ( -93.67499999999998295, -207.7050326799711968, 86.61333333333332973 ) ) ;
#48509 = DIRECTION ( 'NONE',  ( -1.000000000000000000, -0.000000000000000000, -0.000000000000000000 ) ) ;
#48510 = VECTOR ( 'NONE', #27685, 1000.000000000000000 ) ;
#48511 = VERTEX_POINT ( 'NONE', #34245 ) ;
#48512 = CARTESIAN_POINT ( 'NONE',  ( 97.64999999999999147, 90.00000000000002842, 84.60249999999999204 ) ) ;
#48513 = CARTESIAN_POINT ( 'NONE',  ( 0.000000000000000000, -71.91182617369207719, 28.89263327155721228 ) ) ;
#48514 =( NAMED_UNIT ( * ) PLANE_ANGLE_UNIT ( ) SI_UNIT ( $, .RADIAN. ) );
#48515 = CARTESIAN_POINT ( 'NONE',  ( -97.64999999999999147, 91.52997821335250705, 84.86708333333332632 ) ) ;
#48516 = VERTEX_POINT ( 'NONE', #5695 ) ;
#48517 = CYLINDRICAL_SURFACE ( 'NONE', #20312, 82.00000000000000000 ) ;
#48518 = DIRECTION ( 'NONE',  ( -1.000000000000000000, -0.000000000000000000, -0.000000000000000000 ) ) ;
#48519 = ORIENTED_EDGE ( 'NONE', *, *, #52548, .F. ) ;
#48520 = AXIS2_PLACEMENT_3D ( 'NONE', #14224, #72477, #71730 ) ;
#48521 = CARTESIAN_POINT ( 'NONE',  ( 97.30629616937498838, -208.6684592857803295, 81.12322916753380753 ) ) ;
#48522 = DIRECTION ( 'NONE',  ( -1.000000000000000000, 0.000000000000000000, 0.000000000000000000 ) ) ;
#48523 = AXIS2_PLACEMENT_3D ( 'NONE', #27136, #21500, #67374 ) ;
#48524 = ORIENTED_EDGE ( 'NONE', *, *, #29965, .T. ) ;
#48525 = EDGE_CURVE ( 'NONE', #14207, #1863, #33835, .T. ) ;
#48526 = CARTESIAN_POINT ( 'NONE',  ( -95.00000000000002842, 93.05995642670504253, 79.68124999999999147 ) ) ;
#48527 = ORIENTED_EDGE ( 'NONE', *, *, #4168, .T. ) ;
#48528 = ADVANCED_FACE ( 'NONE', ( #4447 ), #72466, .T. ) ;
#48529 = VECTOR ( 'NONE', #1757, 1000.000000000000000 ) ;
#48530 = CYLINDRICAL_SURFACE ( 'NONE', #51454, 82.00000000000000000 ) ;
#48531 = ORIENTED_EDGE ( 'NONE', *, *, #1588, .T. ) ;
#48532 = AXIS2_PLACEMENT_3D ( 'NONE', #27036, #49969, #21393 ) ;
#48533 = CARTESIAN_POINT ( 'NONE',  ( -92.69370383062502583, 91.33154071421968467, 77.47197916753381719 ) ) ;
#48534 = ORIENTED_EDGE ( 'NONE', *, *, #3410, .T. ) ;
#48535 = EDGE_CURVE ( 'NONE', #29646, #20333, #73208, .T. ) ;
#48536 = ORIENTED_EDGE ( 'NONE', *, *, #10951, .T. ) ;
#48537 = FACE_OUTER_BOUND ( 'NONE', #18504, .T. ) ;
#48538 = ORIENTED_EDGE ( 'NONE', *, *, #32016, .T. ) ;
#48539 = CARTESIAN_POINT ( 'NONE',  ( 92.34999999999999432, 91.52997821335252127, 88.12145833506765769 ) ) ;
#48540 = LINE ( 'NONE', #53808, #47613 ) ;
#48541 = EDGE_CURVE ( 'NONE', #67107, #49091, #50633, .T. ) ;
#48542 = ORIENTED_EDGE ( 'NONE', *, *, #5280, .T. ) ;
#48543 = CYLINDRICAL_SURFACE ( 'NONE', #23815, 31.99999999999998579 ) ;
#48544 = CIRCLE ( 'NONE', #58212, 16.00000000000000000 ) ;
#48545 = ORIENTED_EDGE ( 'NONE', *, *, #21884, .F. ) ;
#48546 = DIRECTION ( 'NONE',  ( 0.000000000000000000, 0.000000000000000000, 1.000000000000000000 ) ) ;
#48547 = EDGE_CURVE ( 'NONE', #68891, #19238, #1475, .T. ) ;
#48548 = ORIENTED_EDGE ( 'NONE', *, *, #4513, .F. ) ;
#48549 = CIRCLE ( 'NONE', #16146, 77.49900000000002365 ) ;
#48550 = ORIENTED_EDGE ( 'NONE', *, *, #45722, .F. ) ;
#48551 = ORIENTED_EDGE ( 'NONE', *, *, #54236, .T. ) ;
#48552 = CARTESIAN_POINT ( 'NONE',  ( 92.69370383062501162, -208.6684592857803011, 77.52489583420046415 ) ) ;
#48553 = DIRECTION ( 'NONE',  ( -1.000000000000000000, 0.000000000000000000, 0.000000000000000000 ) ) ;
#48554 = CARTESIAN_POINT ( 'NONE',  ( 0.000000000000000000, -37.58145647212455032, 0.6853352020789044152 ) ) ;
#48555 = ORIENTED_EDGE ( 'NONE', *, *, #21311, .T. ) ;
#48556 = DIRECTION ( 'NONE',  ( 0.000000000000000000, 0.000000000000000000, 1.000000000000000000 ) ) ;
#48557 = ORIENTED_EDGE ( 'NONE', *, *, #31672, .T. ) ;
#48558 = CARTESIAN_POINT ( 'NONE',  ( -96.32500000000001705, 87.70503267997129626, 80.58083333333331666 ) ) ;
#48559 = CARTESIAN_POINT ( 'NONE',  ( 10.00000000000000000, 0.000000000000000000, 0.000000000000000000 ) ) ;
#48560 = ORIENTED_EDGE ( 'NONE', *, *, #23621, .F. ) ;
#48561 = CARTESIAN_POINT ( 'NONE',  ( 0.000000000000000000, 0.000000000000000000, 40.00000000000000000 ) ) ;
#48562 = DIRECTION ( 'NONE',  ( 0.000000000000000000, -0.1564344650402381687, 0.9876883405951365491 ) ) ;
#48563 = CARTESIAN_POINT ( 'NONE',  ( -97.30629616937495996, -209.9999999999999716, 82.65781250086713783 ) ) ;
#48564 = EDGE_CURVE ( 'NONE', #64009, #43683, #21714, .T. ) ;
#48565 = CARTESIAN_POINT ( 'NONE',  ( -95.00000000000002842, 87.33691857156074434, 79.80031250086715033 ) ) ;
#48566 = EDGE_CURVE ( 'NONE', #67235, #73160, #53056, .T. ) ;
#48567 = ORIENTED_EDGE ( 'NONE', *, *, #13580, .T. ) ;
#48568 = AXIS2_PLACEMENT_3D ( 'NONE', #35538, #6969, #34812 ) ;
#48569 = CARTESIAN_POINT ( 'NONE',  ( 96.15314808468748708, 91.99731107132950569, 81.17614583420048291 ) ) ;
#48570 =( BOUNDED_CURVE ( )  B_SPLINE_CURVE ( 2, ( #32457, #20814, #50866, #60684, #50107, #49386, #4290 ),
 .UNSPECIFIED., .F., .F. ) 
 B_SPLINE_CURVE_WITH_KNOTS ( ( 3, 2, 2, 3 ),
 ( 0.4583333333333335924, 0.4652777777777780122, 0.4722222222222224319, 0.4791666666666668517 ),
 .UNSPECIFIED. ) 
 CURVE ( )  GEOMETRIC_REPRESENTATION_ITEM ( )  RATIONAL_B_SPLINE_CURVE ( ( 0.9999999999999946709, 0.8660254037844440367, 1.000000000000000000, 0.8660254037844387076, 1.000000000000000000, 0.8660254037844354880, 1.000000000000003109 ) ) 
 REPRESENTATION_ITEM ( '' )  );
#48571 = EDGE_LOOP ( 'NONE', ( #16312, #34195 ) ) ;
#48572 = DIRECTION ( 'NONE',  ( 1.000000000000000000, 0.000000000000000000, 0.000000000000000000 ) ) ;
#48573 = DIRECTION ( 'NONE',  ( 0.000000000000000000, 0.8660254037844370423, -0.5000000000000029976 ) ) ;
#48574 = CARTESIAN_POINT ( 'NONE',  ( -92.35000000000000853, -209.9999884513869119, 83.41187540116098376 ) ) ;
#48575 = DIRECTION ( 'NONE',  ( -1.000000000000000000, -0.000000000000000000, -0.000000000000000000 ) ) ;
#48576 = CARTESIAN_POINT ( 'NONE',  ( 11.99999999999999822, 40.65526001592611749, 71.21200624218811015 ) ) ;
#48577 = CARTESIAN_POINT ( 'NONE',  ( -97.30629616937497417, -208.6684592857803295, 82.60489583420049087 ) ) ;
#48578 = CARTESIAN_POINT ( 'NONE',  ( 0.000000000000000000, 0.000000000000000000, 0.000000000000000000 ) ) ;
#48579 = CARTESIAN_POINT ( 'NONE',  ( -3.000000000000000000, -20.55727247249726020, -16.78983467731313084 ) ) ;
#48580 = CARTESIAN_POINT ( 'NONE',  ( 10.00000000000000000, -20.41045688087772092, -72.35160999960838524 ) ) ;
#48581 = EDGE_LOOP ( 'NONE', ( #27843, #67127, #9895, #14522 ) ) ;
#48582 = ADVANCED_FACE ( 'NONE', ( #33353 ), #38266, .T. ) ;
#48583 = EDGE_CURVE ( 'NONE', #43856, #70465, #48274, .T. ) ;
#48584 = AXIS2_PLACEMENT_3D ( 'NONE', #27742, #17208, #45800 ) ;
#48585 = VERTEX_POINT ( 'NONE', #50653 ) ;
#48586 = DIRECTION ( 'NONE',  ( 0.000000000000000000, -0.3090169943749548342, 0.9510565162951511997 ) ) ;
#48587 = CARTESIAN_POINT ( 'NONE',  ( -92.35000000000005116, 88.47002178664754979, 76.29458333333333542 ) ) ;
#48588 = DIRECTION ( 'NONE',  ( 1.000000000000000000, 0.000000000000000000, 0.000000000000000000 ) ) ;
#48589 = CARTESIAN_POINT ( 'NONE',  ( -92.69370383062502583, 91.33154071421968467, 84.29822916753380468 ) ) ;
#48590 = DIRECTION ( 'NONE',  ( -1.000000000000000000, -0.000000000000000000, 0.000000000000000000 ) ) ;
#48591 = DIRECTION ( 'NONE',  ( 0.000000000000000000, 0.000000000000000000, 1.000000000000000000 ) ) ;
#48592 = DIRECTION ( 'NONE',  ( 0.000000000000000000, 0.000000000000000000, 1.000000000000000000 ) ) ;
#48593 = CIRCLE ( 'NONE', #16166, 82.00000000000000000 ) ;
#48594 = ORIENTED_EDGE ( 'NONE', *, *, #44035, .F. ) ;
#48595 = AXIS2_PLACEMENT_3D ( 'NONE', #13954, #59847, #8335 ) ;
#48596 = CARTESIAN_POINT ( 'NONE',  ( -92.69370383062502583, 91.33154071421968467, 76.67822916753378593 ) ) ;
#48597 = FACE_OUTER_BOUND ( 'NONE', #11809, .T. ) ;
#48598 = CARTESIAN_POINT ( 'NONE',  ( 90.00000000000000000, 85.00000000000002842, 90.00000000000000000 ) ) ;
#48599 = DIRECTION ( 'NONE',  ( 1.000000000000000000, 1.343011723336883198E-16, 0.000000000000000000 ) ) ;
#48600 = CARTESIAN_POINT ( 'NONE',  ( 95.00000000000000000, -206.9400435732949575, 84.76125000000000398 ) ) ;
#48601 = DIRECTION ( 'NONE',  ( -1.000000000000000000, -0.000000000000000000, -0.000000000000000000 ) ) ;
#48602 = CARTESIAN_POINT ( 'NONE',  ( -92.69370383062498320, -211.3315407142195852, 83.08114583420048405 ) ) ;
#48603 = FILL_AREA_STYLE_COLOUR ( '', #61470 ) ;
#48604 = DIRECTION ( 'NONE',  ( -1.000000000000000000, 0.000000000000000000, 0.000000000000000000 ) ) ;
#48605 = VECTOR ( 'NONE', #23777, 1000.000000000000000 ) ;
#48606 = LINE ( 'NONE', #19651, #62311 ) ;
#48607 = VECTOR ( 'NONE', #7425, 1000.000000000000000 ) ;
#48608 = FACE_OUTER_BOUND ( 'NONE', #64561, .T. ) ;
#48609 = DIRECTION ( 'NONE',  ( -1.000000000000000000, -0.000000000000000000, -0.000000000000000000 ) ) ;
#48610 = ORIENTED_EDGE ( 'NONE', *, *, #60886, .F. ) ;
#48611 = CARTESIAN_POINT ( 'NONE',  ( -3.000000000000000000, -4.261787119644969479, -26.19803753235780519 ) ) ;
#48612 = CARTESIAN_POINT ( 'NONE',  ( 96.32499999999998863, -207.7050326799711968, 79.62833333333333030 ) ) ;
#48613 = ADVANCED_FACE ( 'NONE', ( #39016 ), #3714, .T. ) ;
#48614 = DIRECTION ( 'NONE',  ( -0.000000000000000000, -0.000000000000000000, 1.000000000000000000 ) ) ;
#48615 = CARTESIAN_POINT ( 'NONE',  ( 96.15314808468748708, -208.0026889286704943, 89.58989583420049030 ) ) ;
#48616 = ORIENTED_EDGE ( 'NONE', *, *, #27471, .F. ) ;
#48617 = ADVANCED_FACE ( 'NONE', ( #73579 ), #10063, .T. ) ;
#48618 = LINE ( 'NONE', #2435, #27623 ) ;
#48619 = FACE_OUTER_BOUND ( 'NONE', #52177, .T. ) ;
#48620 = EDGE_LOOP ( 'NONE', ( #619, #72483, #24422, #58746 ) ) ;
#48621 = ADVANCED_FACE ( 'NONE', ( #73953 ), #67956, .F. ) ;
#48622 = FACE_OUTER_BOUND ( 'NONE', #7829, .T. ) ;
#48623 = ORIENTED_EDGE ( 'NONE', *, *, #17470, .T. ) ;
#48624 = EDGE_CURVE ( 'NONE', #1062, #71384, #45933, .T. ) ;
#48625 = DIRECTION ( 'NONE',  ( 1.000000000000000000, -0.000000000000000000, -0.000000000000000000 ) ) ;
#48626 = VECTOR ( 'NONE', #32165, 1000.000000000000000 ) ;
#48627 = VERTEX_POINT ( 'NONE', #45033 ) ;
#48628 = EDGE_CURVE ( 'NONE', #63730, #7618, #62331, .T. ) ;
#48629 = ORIENTED_EDGE ( 'NONE', *, *, #59921, .F. ) ;
#48630 = ORIENTED_EDGE ( 'NONE', *, *, #42886, .T. ) ;
#48631 = ORIENTED_EDGE ( 'NONE', *, *, #3699, .T. ) ;
#48632 = CARTESIAN_POINT ( 'NONE',  ( -3.000000000000000000, 6.762365576493643893, -25.66652317338391853 ) ) ;
#48633 = ORIENTED_EDGE ( 'NONE', *, *, #34559, .F. ) ;
#48634 = ORIENTED_EDGE ( 'NONE', *, *, #51424, .F. ) ;
#48635 = CARTESIAN_POINT ( 'NONE',  ( 97.30629616937498838, 88.66845928578037217, 80.54114583420049200 ) ) ;
#48636 = VECTOR ( 'NONE', #44843, 1000.000000000000000 ) ;
#48637 = DIRECTION ( 'NONE',  ( -1.000000000000000000, 0.000000000000000000, 0.000000000000000000 ) ) ;
#48638 = ADVANCED_FACE ( 'NONE', ( #10816 ), #56687, .T. ) ;
#48640 = CARTESIAN_POINT ( 'NONE',  ( 0.000000000000000000, 27.74655509720669500, 77.16300072079670258 ) ) ;
#48639 = AXIS2_PLACEMENT_3D ( 'NONE', #56800, #69552, #69187 ) ;
#48641 = ORIENTED_EDGE ( 'NONE', *, *, #56601, .F. ) ;
#48642 = VERTEX_POINT ( 'NONE', #68335 ) ;
#48643 = ORIENTED_EDGE ( 'NONE', *, *, #41952, .F. ) ;
#48644 = DIRECTION ( 'NONE',  ( 1.000000000000000000, 0.000000000000000000, 0.000000000000000000 ) ) ;
#48645 = ORIENTED_EDGE ( 'NONE', *, *, #42018, .F. ) ;
#48646 = AXIS2_PLACEMENT_3D ( 'NONE', #57040, #5550, #68696 ) ;
#48647 = DIRECTION ( 'NONE',  ( 5.336177323473924868E-17, -3.796704924751176257E-16, -0.9999999999999998890 ) ) ;
#48648 = CARTESIAN_POINT ( 'NONE',  ( -17.26469406256017791, -140.1601175325492648, 5.500000000000000000 ) ) ;
#48649 = DIRECTION ( 'NONE',  ( -1.000000000000000000, -0.000000000000000000, 0.000000000000000000 ) ) ;
#48650 = CARTESIAN_POINT ( 'NONE',  ( 92.34999999999998010, 89.99999071025125374, 78.01437532303467037 ) ) ;
#48651 = DIRECTION ( 'NONE',  ( -1.000000000000000000, 0.000000000000000000, 0.000000000000000000 ) ) ;
#48652 = AXIS2_PLACEMENT_3D ( 'NONE', #65332, #31096, #8554 ) ;
#48653 = LINE ( 'NONE', #31350, #61173 ) ;
#48654 = CARTESIAN_POINT ( 'NONE',  ( 15.00000000000000000, -19.89357724624986545, 12.59942793731086219 ) ) ;
#48655 = CARTESIAN_POINT ( 'NONE',  ( -92.34999999999999432, -209.9999999999999716, 76.42687500173430237 ) ) ;
#48656 = EDGE_CURVE ( 'NONE', #11931, #62260, #16829, .T. ) ;
#48657 = CARTESIAN_POINT ( 'NONE',  ( -96.15314808468751551, 88.00268892867056536, 88.63739583420048973 ) ) ;
#48658 = EDGE_CURVE ( 'NONE', #49261, #4256, #9257, .T. ) ;
#48660 = CARTESIAN_POINT ( 'NONE',  ( -92.69370383062502583, 88.66845928578038638, 88.00239583420047040 ) ) ;
#48659 = CARTESIAN_POINT ( 'NONE',  ( 97.64999999999997726, 88.47002178664753558, 75.10395833506764518 ) ) ;
#48661 = VERTEX_POINT ( 'NONE', #18294 ) ;
#48662 = CARTESIAN_POINT ( 'NONE',  ( 97.30629616937498838, 88.66845928578037217, 76.09614583420048461 ) ) ;
#48663 = CARTESIAN_POINT ( 'NONE',  ( 10.00000000000000000, -17.28742895386139722, 75.54627589209937355 ) ) ;
#48664 = DIRECTION ( 'NONE',  ( 0.000000000000000000, -0.8910065241883722287, 0.4539904997395383113 ) ) ;
#48665 = DIRECTION ( 'NONE',  ( -1.000000000000000000, 0.000000000000000000, -0.000000000000000000 ) ) ;
#48666 = CARTESIAN_POINT ( 'NONE',  ( -93.67500000000003979, 92.29496732002878900, 78.43770833506764006 ) ) ;
#48667 = DIRECTION ( 'NONE',  ( 0.000000000000000000, 0.000000000000000000, -1.000000000000000000 ) ) ;
#48668 = ORIENTED_EDGE ( 'NONE', *, *, #2446, .T. ) ;
#48669 = DIRECTION ( 'NONE',  ( -1.000000000000000000, 0.000000000000000000, 0.000000000000000000 ) ) ;
#48670 = FACE_BOUND ( 'NONE', #46255, .T. ) ;
#48671 = VERTEX_POINT ( 'NONE', #34110 ) ;
#48672 = ORIENTED_EDGE ( 'NONE', *, *, #22530, .F. ) ;
#48673 = DIRECTION ( 'NONE',  ( 1.000000000000000000, 0.000000000000000000, -0.000000000000000000 ) ) ;
#48674 = DIRECTION ( 'NONE',  ( 0.000000000000000000, -0.3090169943749461745, 0.9510565162951539753 ) ) ;
#48675 = CARTESIAN_POINT ( 'NONE',  ( -93.67500000000003979, 92.29496732002878900, 86.05770833506763040 ) ) ;
#48676 = LINE ( 'NONE', #60711, #41103 ) ;
#48677 = CARTESIAN_POINT ( 'NONE',  ( -93.67500000000003979, 87.70503267997129626, 76.32104166840096582 ) ) ;
#48678 = CARTESIAN_POINT ( 'NONE',  ( 10.00000000000000000, 40.68715046381944234, -10.41901085202036192 ) ) ;
#48679 = ORIENTED_EDGE ( 'NONE', *, *, #10073, .F. ) ;
#48680 = DIRECTION ( 'NONE',  ( -1.000000000000000000, -0.000000000000000000, -0.000000000000000000 ) ) ;
#48681 = CIRCLE ( 'NONE', #10245, 82.00000000000000000 ) ;
#48682 = CARTESIAN_POINT ( 'NONE',  ( 12.00000000000000000, 23.59884966291521735, -12.14883922797262805 ) ) ;
#48683 = CARTESIAN_POINT ( 'NONE',  ( -92.35000000000003695, 90.00000000000004263, 78.88750000000000284 ) ) ;
#48684 = PLANE ( 'NONE',  #30860 ) ;
#48685 = FACE_OUTER_BOUND ( 'NONE', #64078, .T. ) ;
#48686 = CARTESIAN_POINT ( 'NONE',  ( -8.000000000000019540, -1.798221273588296393E-13, -15.80000000000029026 ) ) ;
#48687 = CARTESIAN_POINT ( 'NONE',  ( 11.99999999999999822, -41.76106447765443619, -62.50884508063471401 ) ) ;
#48688 = LINE ( 'NONE', #43449, #3417 ) ;
#48689 = ADVANCED_FACE ( 'NONE', ( #35583 ), #64178, .T. ) ;
#48690 = CARTESIAN_POINT ( 'NONE',  ( 94.99999999999998579, 92.66308142843932671, 85.19781250086714408 ) ) ;
#48691 = CARTESIAN_POINT ( 'NONE',  ( -97.30629616937497417, -208.6684592857803295, 82.76364583420048859 ) ) ;
#48692 = CARTESIAN_POINT ( 'NONE',  ( 0.000000000000000000, -18.13022148937243472, -15.02647892043568767 ) ) ;
#48693 = ORIENTED_EDGE ( 'NONE', *, *, #74004, .T. ) ;
#48694 = CARTESIAN_POINT ( 'NONE',  ( 22.30499999999999972, 0.000000000000000000, 0.000000000000000000 ) ) ;
#48695 = CARTESIAN_POINT ( 'NONE',  ( -92.34999999999999432, -208.4700217866474645, 79.57541666666665492 ) ) ;
#48696 = FACE_OUTER_BOUND ( 'NONE', #13344, .T. ) ;
#48697 = AXIS2_PLACEMENT_3D ( 'NONE', #11825, #18223, #40411 ) ;
#48698 = EDGE_CURVE ( 'NONE', #55747, #1142, #17929, .T. ) ;
#48699 = CARTESIAN_POINT ( 'NONE',  ( 92.69370383062501162, -211.3315407142195852, 85.25072916753379104 ) ) ;
#48700 = ORIENTED_EDGE ( 'NONE', *, *, #27209, .F. ) ;
#48701 = EDGE_CURVE ( 'NONE', #3672, #26361, #55526, .T. ) ;
#48702 = AXIS2_PLACEMENT_3D ( 'NONE', #22328, #45271, #33595 ) ;
#48703 = FACE_OUTER_BOUND ( 'NONE', #5655, .T. ) ;
#48704 = ORIENTED_EDGE ( 'NONE', *, *, #30678, .F. ) ;
#48705 = VECTOR ( 'NONE', #47111, 1000.000000000000114 ) ;
#48706 = ORIENTED_EDGE ( 'NONE', *, *, #33971, .T. ) ;
#48707 = EDGE_CURVE ( 'NONE', #50093, #53901, #40875, .T. ) ;
#48708 = EDGE_CURVE ( 'NONE', #16263, #1076, #69886, .T. ) ;
#48709 = CARTESIAN_POINT ( 'NONE',  ( 12.00000000000000000, 16.61724383029361718, -20.69703378468927113 ) ) ;
#48710 = VECTOR ( 'NONE', #30943, 1000.000000000000000 ) ;
#48711 = VERTEX_POINT ( 'NONE', #29936 ) ;
#48712 = CARTESIAN_POINT ( 'NONE',  ( 5.000000000000002665, 16.65972982745046238, -80.28980883073738539 ) ) ;
#48713 = CARTESIAN_POINT ( 'NONE',  ( 95.00000000000000000, -212.6630814284392557, 77.89531250086714920 ) ) ;
#48714 = DIRECTION ( 'NONE',  ( -1.000000000000000000, 0.000000000000000000, 0.000000000000000000 ) ) ;
#48715 = PLANE ( 'NONE',  #28027 ) ;
#48716 = CYLINDRICAL_SURFACE ( 'NONE', #43652, 31.99999999999999289 ) ;
#48717 = FACE_OUTER_BOUND ( 'NONE', #53369, .T. ) ;
#48718 = EDGE_CURVE ( 'NONE', #19226, #72116, #27877, .T. ) ;
#48719 = DIRECTION ( 'NONE',  ( -1.000000000000000000, -0.000000000000000000, -0.000000000000000000 ) ) ;
#48720 = CARTESIAN_POINT ( 'NONE',  ( 92.35000000000002274, -208.4700217866474645, 79.78708333333332803 ) ) ;
#48721 = VERTEX_POINT ( 'NONE', #29560 ) ;
#48722 = ORIENTED_EDGE ( 'NONE', *, *, #13483, .T. ) ;
#48723 = EDGE_LOOP ( 'NONE', ( #9433, #25164, #51591, #28878, #41065, #36686, #73428, #40315, #17952, #9461, #25780, #62832, #70202, #7514, #53683, #56973 ) ) ;
#48724 = ORIENTED_EDGE ( 'NONE', *, *, #26313, .F. ) ;
#48725 = DIRECTION ( 'NONE',  ( -3.035766082959412415E-16, -1.000000000000000000, -0.000000000000000000 ) ) ;
#48726 =( NAMED_UNIT ( * ) SI_UNIT ( $, .STERADIAN. ) SOLID_ANGLE_UNIT ( ) );
#48727 = CARTESIAN_POINT ( 'NONE',  ( -93.84685191531252713, 88.00268892867056536, 82.39322916753381776 ) ) ;
#48728 = CARTESIAN_POINT ( 'NONE',  ( -97.65000000002672209, -209.9999999999999147, -74.99999999999342037 ) ) ;
#48729 = CARTESIAN_POINT ( 'NONE',  ( 12.00000000000000000, 5.835314593368777558, 22.81335362449846471 ) ) ;
#48730 = CYLINDRICAL_SURFACE ( 'NONE', #9474, 2.649999999999999467 ) ;
#48731 = DIRECTION ( 'NONE',  ( 1.000000000000000000, 0.000000000000000000, -0.000000000000000000 ) ) ;
#48732 = VERTEX_POINT ( 'NONE', #40492 ) ;
#48733 = CARTESIAN_POINT ( 'NONE',  ( -96.32499999999996021, -207.7050326799711968, 86.16354166840096696 ) ) ;
#48735 = ORIENTED_EDGE ( 'NONE', *, *, #67461, .F. ) ;
#48734 = EDGE_CURVE ( 'NONE', #21818, #42186, #65146, .T. ) ;
#48736 = CARTESIAN_POINT ( 'NONE',  ( -7.500000000000011546, -62.04836822995428491, -189.9999999999999147 ) ) ;
#48737 = ORIENTED_EDGE ( 'NONE', *, *, #61876, .F. ) ;
#48738 = CARTESIAN_POINT ( 'NONE',  ( -92.35000000000005116, 91.52997821335253548, 87.90979166840095615 ) ) ;
#48740 = EDGE_CURVE ( 'NONE', #39808, #14784, #30293, .T. ) ;
#48739 = VERTEX_POINT ( 'NONE', #52499 ) ;
#48741 = CARTESIAN_POINT ( 'NONE',  ( 92.69370383062498320, 90.00000000000002842, 85.99156250086716113 ) ) ;
#48742 = VECTOR ( 'NONE', #52735, 1000.000000000000114 ) ;
#48743 = CARTESIAN_POINT ( 'NONE',  ( 0.1219594728601484379, -121.4950337410840149, 2.500000000000000000 ) ) ;
#48744 = CARTESIAN_POINT ( 'NONE',  ( -96.32500000000001705, 87.70503267997129626, 83.83520833506763381 ) ) ;
#48745 = DIRECTION ( 'NONE',  ( 1.000000000000000000, 0.000000000000000000, -0.000000000000000000 ) ) ;
#48746 = CARTESIAN_POINT ( 'NONE',  ( 11.99999999999999822, 81.90746397400387480, 3.894527615418187150 ) ) ;
#48747 = ORIENTED_EDGE ( 'NONE', *, *, #58584, .T. ) ;
#48748 = DIRECTION ( 'NONE',  ( -1.000000000000000000, 0.000000000000000000, 0.000000000000000000 ) ) ;
#48749 = CYLINDRICAL_SURFACE ( 'NONE', #10774, 12.49999999999999645 ) ;
#48750 = ORIENTED_EDGE ( 'NONE', *, *, #64934, .T. ) ;
#48751 = AXIS2_PLACEMENT_3D ( 'NONE', #28260, #11341, #22636 ) ;
#48752 = ORIENTED_EDGE ( 'NONE', *, *, #65869, .F. ) ;
#48754 = CARTESIAN_POINT ( 'NONE',  ( 97.65000000000000568, 88.47002178664752137, 78.91395833506763324 ) ) ;
#48753 = VECTOR ( 'NONE', #61455, 1000.000000000000000 ) ;
#48755 = PRODUCT ( 'key', 'key', '', ( #66680 ) ) ;
#48756 = FACE_OUTER_BOUND ( 'NONE', #8073, .T. ) ;
#48757 = VECTOR ( 'NONE', #62482, 1000.000000000000000 ) ;
#48758 = AXIS2_PLACEMENT_3D ( 'NONE', #52647, #34995, #69206 ) ;
#48759 = CARTESIAN_POINT ( 'NONE',  ( 11.99999999999999822, 0.000000000000000000, 0.000000000000000000 ) ) ;
#48760 = CARTESIAN_POINT ( 'NONE',  ( -93.84685191531247028, -211.9973110713294489, 84.93322916753382401 ) ) ;
#48761 = ORIENTED_EDGE ( 'NONE', *, *, #12246, .F. ) ;
#48762 = CARTESIAN_POINT ( 'NONE',  ( 5.000000000000000000, 40.65526001592713357, -71.21200624218752750 ) ) ;
#48763 = ORIENTED_EDGE ( 'NONE', *, *, #57459, .T. ) ;
#48764 = CARTESIAN_POINT ( 'NONE',  ( 0.000000000000000000, -8.830959090341869100, -74.65491531819127147 ) ) ;
#48765 = CARTESIAN_POINT ( 'NONE',  ( 92.34999999999995168, 91.52997821335250705, 86.77208333333334167 ) ) ;
#48766 = AXIS2_PLACEMENT_3D ( 'NONE', #66915, #65460, #43277 ) ;
#48767 = CARTESIAN_POINT ( 'NONE',  ( -93.67499999999998295, -212.2949673200287179, 76.32104166840096582 ) ) ;
#48768 = CARTESIAN_POINT ( 'NONE',  ( 92.69370383062498320, 91.33154071421968467, 78.15989583420048348 ) ) ;
#48769 = DIRECTION ( 'NONE',  ( -1.000000000000000000, -0.000000000000000000, -0.000000000000000000 ) ) ;
#48770 = CARTESIAN_POINT ( 'NONE',  ( 12.00000000000000000, 23.49999999999999645, 1.499999999999995337 ) ) ;
#48771 = DIRECTION ( 'NONE',  ( 0.000000000000000000, 0.8910065241883688980, -0.4539904997395447506 ) ) ;
#48772 = DIRECTION ( 'NONE',  ( 0.000000000000000000, 0.1564344650402242354, 0.9876883405951387696 ) ) ;
#48773 = CARTESIAN_POINT ( 'NONE',  ( 11.99999999999999822, -24.73286445877655382, -73.44644590900085745 ) ) ;
#48774 = DIRECTION ( 'NONE',  ( 0.000000000000000000, 0.000000000000000000, 1.000000000000000000 ) ) ;
#48775 = EDGE_CURVE ( 'NONE', #20377, #19673, #42333, .T. ) ;
#48776 = DIRECTION ( 'NONE',  ( -1.000000000000000000, 0.000000000000000000, 0.000000000000000000 ) ) ;
#48777 = CARTESIAN_POINT ( 'NONE',  ( 96.32499999999997442, 92.29496732002878900, 89.15333333333333599 ) ) ;
#48778 = ORIENTED_EDGE ( 'NONE', *, *, #28357, .F. ) ;
#48779 = CARTESIAN_POINT ( 'NONE',  ( -97.30629616937501680, 88.66845928578038638, 82.07572916753382231 ) ) ;
#48780 = CARTESIAN_POINT ( 'NONE',  ( -2.499999999999970690, 73.00000000000001421, -255.0000000000000000 ) ) ;
#48781 = EDGE_CURVE ( 'NONE', #17154, #30036, #23946, .T. ) ;
#48782 = ADVANCED_FACE ( 'NONE', ( #34476 ), #41234, .T. ) ;
#48783 = DIRECTION ( 'NONE',  ( 0.000000000000000000, -0.9510565162951565288, 0.3090169943749382919 ) ) ;
#48784 = ORIENTED_EDGE ( 'NONE', *, *, #41191, .T. ) ;
#48785 =( BOUNDED_CURVE ( )  B_SPLINE_CURVE ( 2, ( #6420, #18060, #34983, #29322, #62461, #10556, #11303 ),
 .UNSPECIFIED., .F., .F. ) 
 B_SPLINE_CURVE_WITH_KNOTS ( ( 3, 2, 2, 3 ),
 ( 0.000000000000000000, 0.006944444444444406762, 0.01388888888888881352, 0.02083333333333322115 ),
 .UNSPECIFIED. ) 
 CURVE ( )  GEOMETRIC_REPRESENTATION_ITEM ( )  RATIONAL_B_SPLINE_CURVE ( ( 1.000000000000000000, 0.8660254037844387076, 1.000000000000000000, 0.8660254037844387076, 1.000000000000000000, 0.8660254037844408170, 0.9999999999999978906 ) ) 
 REPRESENTATION_ITEM ( '' )  );
#48786 = FACE_OUTER_BOUND ( 'NONE', #38502, .T. ) ;
#48787 = DIRECTION ( 'NONE',  ( 0.000000000000000000, 0.000000000000000000, 1.000000000000000000 ) ) ;
#48788 = VECTOR ( 'NONE', #10948, 1000.000000000000000 ) ;
#48789 = FACE_OUTER_BOUND ( 'NONE', #67389, .T. ) ;
#48790 = EDGE_CURVE ( 'NONE', #51135, #62092, #11539, .T. ) ;
#48791 = CARTESIAN_POINT ( 'NONE',  ( 96.15314808468750130, -211.9973110713294489, 79.21822916753382060 ) ) ;
#48792 = AXIS2_PLACEMENT_3D ( 'NONE', #69997, #47093, #69642 ) ;
#48793 = ORIENTED_EDGE ( 'NONE', *, *, #33635, .T. ) ;
#48794 = CIRCLE ( 'NONE', #38017, 31.99999999999999645 ) ;
#48795 = ORIENTED_EDGE ( 'NONE', *, *, #7877, .T. ) ;
#48796 = DIRECTION ( 'NONE',  ( 1.000000000000000000, 0.000000000000000000, 0.000000000000000000 ) ) ;
#48797 = AXIS2_PLACEMENT_3D ( 'NONE', #13896, #47749, #59412 ) ;
#48798 = EDGE_CURVE ( 'NONE', #55390, #26258, #25070, .T. ) ;
#48799 = CARTESIAN_POINT ( 'NONE',  ( -2.499999999999970690, 73.00000000000001421, -204.9999999999999716 ) ) ;
#48800 = CARTESIAN_POINT ( 'NONE',  ( 10.00000000000000000, -30.84782396557233142, 21.32104025579104345 ) ) ;
#48802 = ORIENTED_EDGE ( 'NONE', *, *, #29628, .F. ) ;
#48801 = ADVANCED_FACE ( 'NONE', ( #23569 ), #69431, .T. ) ;
#48803 = CARTESIAN_POINT ( 'NONE',  ( 5.000000000000000000, 27.75498641678786527, -31.52238457039571173 ) ) ;
#48804 = CARTESIAN_POINT ( 'NONE',  ( 93.84685191531251292, -211.9973110713294489, 75.30239583420048177 ) ) ;
#48805 = VERTEX_POINT ( 'NONE', #58904 ) ;
#48806 = LINE ( 'NONE', #13112, #62373 ) ;
#48807 = VERTEX_POINT ( 'NONE', #53255 ) ;
#48808 = ADVANCED_FACE ( 'NONE', ( #49087 ), #19767, .T. ) ;
#48809 = ORIENTED_EDGE ( 'NONE', *, *, #39201, .T. ) ;
#48810 = CARTESIAN_POINT ( 'NONE',  ( -97.64996285368241047, -208.4700003402110156, 82.40645685155115530 ) ) ;
#48811 = AXIS2_PLACEMENT_3D ( 'NONE', #70980, #65367, #20606 ) ;
#48812 = CARTESIAN_POINT ( 'NONE',  ( -93.67500000000003979, 92.29496732002878900, 89.23270833506762756 ) ) ;
#48813 = VERTEX_POINT ( 'NONE', #43479 ) ;
#48814 = LINE ( 'NONE', #37555, #71358 ) ;
#48815 = CARTESIAN_POINT ( 'NONE',  ( 96.32499999999998863, -207.7050326799711968, 82.88270833506763324 ) ) ;
#48816 = CARTESIAN_POINT ( 'NONE',  ( 92.34999999999999432, 91.52997821335252127, 86.13708333333332234 ) ) ;
#48817 = VERTEX_POINT ( 'NONE', #65649 ) ;
#48818 = DIRECTION ( 'NONE',  ( 1.000000000000000000, 0.000000000000000000, 0.000000000000000000 ) ) ;
#48819 = EDGE_CURVE ( 'NONE', #67020, #14528, #8506, .T. ) ;
#48820 = CARTESIAN_POINT ( 'NONE',  ( 11.99999999999999822, 35.91791733033570466, -68.67312586194960033 ) ) ;
#48821 = ORIENTED_EDGE ( 'NONE', *, *, #62696, .T. ) ;
#48822 = ORIENTED_EDGE ( 'NONE', *, *, #74092, .F. ) ;
#48823 = CARTESIAN_POINT ( 'NONE',  ( -96.15314808468752972, 91.99731107132950569, 89.06072916753382174 ) ) ;
#48824 = CARTESIAN_POINT ( 'NONE',  ( 94.99999999999998579, 92.66308142843935514, 81.86406250086714920 ) ) ;
#48825 = ORIENTED_EDGE ( 'NONE', *, *, #28423, .T. ) ;
#48826 = CARTESIAN_POINT ( 'NONE',  ( 93.67499999999998295, 92.29496732002878900, 81.08354166840096866 ) ) ;
#48827 = DIRECTION ( 'NONE',  ( -0.9918136447140101231, 0.1276937514489694114, 0.000000000000000000 ) ) ;
#48828 = EDGE_LOOP ( 'NONE', ( #55080, #901, #25063, #12950, #26969 ) ) ;
#48829 = DIRECTION ( 'NONE',  ( 1.000000000000000000, 1.427937372958405461E-15, 7.962523111839130290E-16 ) ) ;
#48830 = ORIENTED_EDGE ( 'NONE', *, *, #58324, .T. ) ;
#48831 = VECTOR ( 'NONE', #5957, 1000.000000000000000 ) ;
#48832 = EDGE_LOOP ( 'NONE', ( #71756, #10298, #52484, #8609 ) ) ;
#48833 = ORIENTED_EDGE ( 'NONE', *, *, #28573, .F. ) ;
#48834 = CARTESIAN_POINT ( 'NONE',  ( -95.00000000000002842, 86.94004357329504273, 82.61812500173428475 ) ) ;
#48835 = DIRECTION ( 'NONE',  ( 1.000000000000000000, 0.000000000000000000, 0.000000000000000000 ) ) ;
#48836 = CARTESIAN_POINT ( 'NONE',  ( -95.00000000000002842, 86.94004357329504273, 83.80875000000000341 ) ) ;
#48837 = ORIENTED_EDGE ( 'NONE', *, *, #70496, .T. ) ;
#48838 = DIRECTION ( 'NONE',  ( -0.000000000000000000, -0.000000000000000000, 1.000000000000000000 ) ) ;
#48839 = CARTESIAN_POINT ( 'NONE',  ( 97.64999999999997726, 91.52997821335252127, 88.54479166840097548 ) ) ;
#48840 = ORIENTED_EDGE ( 'NONE', *, *, #37207, .T. ) ;
#48841 = DIRECTION ( 'NONE',  ( -0.000000000000000000, -0.000000000000000000, 1.000000000000000000 ) ) ;
#48842 = CARTESIAN_POINT ( 'NONE',  ( -92.69370383062498320, -208.6684592857803011, 77.94822916753381037 ) ) ;
#48843 = ORIENTED_EDGE ( 'NONE', *, *, #3587, .F. ) ;
#48844 = FACE_OUTER_BOUND ( 'NONE', #29389, .T. ) ;
#48845 = AXIS2_PLACEMENT_3D ( 'NONE', #47382, #54495, #54135 ) ;
#48846 = DIRECTION ( 'NONE',  ( 0.000000000000000000, 0.000000000000000000, 1.000000000000000000 ) ) ;
#48847 = DIRECTION ( 'NONE',  ( -0.9435911131814395114, 0.3311129884571304971, 0.000000000000000000 ) ) ;
#48848 = FACE_OUTER_BOUND ( 'NONE', #1627, .T. ) ;
#48849 = AXIS2_PLACEMENT_3D ( 'NONE', #25602, #25250, #2720 ) ;
#48850 = CARTESIAN_POINT ( 'NONE',  ( -3.000000000000000000, -23.29833615347104825, -3.418703333116803744 ) ) ;
#48851 = VECTOR ( 'NONE', #7834, 1000.000000000000000 ) ;
#48852 = CARTESIAN_POINT ( 'NONE',  ( 92.69370383062498320, 91.33154071421968467, 89.58989583420047609 ) ) ;
#48853 = DIRECTION ( 'NONE',  ( 0.6516173805718079581, -0.7585478161175704948, 0.000000000000000000 ) ) ;
#48854 = DIRECTION ( 'NONE',  ( -1.000000000000000000, 0.000000000000000000, 0.000000000000000000 ) ) ;
#48855 = CARTESIAN_POINT ( 'NONE',  ( -94.99999999999997158, -206.9400435732949575, 86.74562500173429669 ) ) ;
#48856 = CARTESIAN_POINT ( 'NONE',  ( -95.00000000000002842, 92.66308142843932671, 76.14906250086716000 ) ) ;
#48857 = CYLINDRICAL_SURFACE ( 'NONE', #52665, 2.649999999999999467 ) ;
#48858 = CARTESIAN_POINT ( 'NONE',  ( -100.0000000000260485, 95.00000000000001421, -75.00000000000000000 ) ) ;
#48859 = CIRCLE ( 'NONE', #20034, 31.99999999999998934 ) ;
#48860 = AXIS2_PLACEMENT_3D ( 'NONE', #65448, #47764, #71057 ) ;
#48861 = CARTESIAN_POINT ( 'NONE',  ( 0.000000000000000000, 80.55351364060611274, -15.33399622253397609 ) ) ;
#48862 = DIRECTION ( 'NONE',  ( -0.000000000000000000, -0.000000000000000000, 1.000000000000000000 ) ) ;
#48863 = EDGE_CURVE ( 'NONE', #28639, #73949, #12553, .T. ) ;
#48864 = EDGE_CURVE ( 'NONE', #42164, #8127, #13760, .T. ) ;
#48865 = UNCERTAINTY_MEASURE_WITH_UNIT (LENGTH_MEASURE( 1.000000000000000082E-05 ), #23668, 'distance_accuracy_value', 'NONE');
#48866 = CARTESIAN_POINT ( 'NONE',  ( 4.999999999999999112, -3.925862922256468046, 41.81611651403860463 ) ) ;
#48867 = LINE ( 'NONE', #72165, #27404 ) ;
#48868 = CARTESIAN_POINT ( 'NONE',  ( 96.66734480923263106, 87.91120745868266795, 75.00000000000000000 ) ) ;
#48869 = ADVANCED_FACE ( 'NONE', ( #31426 ), #2161, .T. ) ;
#48870 = AXIS2_PLACEMENT_3D ( 'NONE', #55185, #54814, #3340 ) ;
#48871 = LINE ( 'NONE', #47760, #56861 ) ;
#48872 = CARTESIAN_POINT ( 'NONE',  ( -97.64999999999994884, -211.5299782133524502, 87.51291666666666913 ) ) ;
#48873 = EDGE_CURVE ( 'NONE', #13281, #10460, #47608, .T. ) ;
#48874 = AXIS2_PLACEMENT_3D ( 'NONE', #50833, #73762, #39570 ) ;
#48875 = LINE ( 'NONE', #50356, #12167 ) ;
#48876 = EDGE_CURVE ( 'NONE', #47477, #19038, #70901, .T. ) ;
#48877 = VERTEX_POINT ( 'NONE', #59637 ) ;
#48878 = CARTESIAN_POINT ( 'NONE',  ( -97.30629616937495996, -209.9999999999999716, 89.80156250086714920 ) ) ;
#48879 = FACE_OUTER_BOUND ( 'NONE', #24154, .T. ) ;
#48880 = FACE_OUTER_BOUND ( 'NONE', #56520, .T. ) ;
#48881 = CARTESIAN_POINT ( 'NONE',  ( 0.000000000000000000, -49.70050353004846500, -59.46389618802017907 ) ) ;
#48882 = ORIENTED_EDGE ( 'NONE', *, *, #35255, .F. ) ;
#48883 = DIRECTION ( 'NONE',  ( -1.000000000000000000, -0.000000000000000000, -0.000000000000000000 ) ) ;
#48884 = CARTESIAN_POINT ( 'NONE',  ( 0.000000000000000000, 0.000000000000000000, 0.000000000000000000 ) ) ;
#48885 = ORIENTED_EDGE ( 'NONE', *, *, #26976, .T. ) ;
#48886 = CARTESIAN_POINT ( 'NONE',  ( 92.69370383062501162, -209.9999999999999716, 83.29281250086714294 ) ) ;
#48887 = ORIENTED_EDGE ( 'NONE', *, *, #46325, .F. ) ;
#48888 = CARTESIAN_POINT ( 'NONE',  ( 97.30629616937498838, -211.3315407142195852, 87.52614583420049144 ) ) ;
#48889 = ORIENTED_EDGE ( 'NONE', *, *, #43666, .T. ) ;
#48890 = CARTESIAN_POINT ( 'NONE',  ( -93.67499999999998295, -212.2949673200287179, 80.68666666666665321 ) ) ;
#48891 = VERTEX_POINT ( 'NONE', #72011 ) ;
#48892 = EDGE_CURVE ( 'NONE', #18118, #59010, #7398, .T. ) ;
#48893 = EDGE_CURVE ( 'NONE', #73125, #30694, #66319, .T. ) ;
#48894 = CARTESIAN_POINT ( 'NONE',  ( -95.00000000000002842, 92.66308142843932671, 78.84781250086714977 ) ) ;
#48895 = ORIENTED_EDGE ( 'NONE', *, *, #22866, .F. ) ;
#48896 = AXIS2_PLACEMENT_3D ( 'NONE', #66965, #54949, #61346 ) ;
#48897 = EDGE_LOOP ( 'NONE', ( #21285, #77, #14633, #66143 ) ) ;
#48898 = CYLINDRICAL_SURFACE ( 'NONE', #58095, 31.99999999999998579 ) ;
#48899 = AXIS2_PLACEMENT_3D ( 'NONE', #30554, #57676, #41847 ) ;
#48900 = VERTEX_POINT ( 'NONE', #30675 ) ;
#48901 = CARTESIAN_POINT ( 'NONE',  ( 0.000000000000000000, 3.894527615417885169, 81.90746397400390322 ) ) ;
#48902 = DIRECTION ( 'NONE',  ( 0.000000000000000000, -0.3826834323650774028, -0.9238795325112919565 ) ) ;
#48903 = ORIENTED_EDGE ( 'NONE', *, *, #16970, .F. ) ;
#48904 = DIRECTION ( 'NONE',  ( 0.000000000000000000, 0.000000000000000000, 1.000000000000000000 ) ) ;
#48905 = ADVANCED_FACE ( 'NONE', ( #48717 ), #3256, .F. ) ;
#48906 = ORIENTED_EDGE ( 'NONE', *, *, #51009, .T. ) ;
#48907 = DIRECTION ( 'NONE',  ( -1.000000000000000000, -0.000000000000000000, 0.000000000000000000 ) ) ;
#48908 = ORIENTED_EDGE ( 'NONE', *, *, #35488, .T. ) ;
#48909 = EDGE_LOOP ( 'NONE', ( #6597, #9545, #37931, #63536 ) ) ;
#48910 = VERTEX_POINT ( 'NONE', #64914 ) ;
#48911 = CARTESIAN_POINT ( 'NONE',  ( 93.84685191531251292, -211.9973110713294489, 78.95364583420047211 ) ) ;
#48912 = CARTESIAN_POINT ( 'NONE',  ( 0.000000000000000000, -41.76937507738831812, 62.50329211542423025 ) ) ;
#48913 = ITEM_DEFINED_TRANSFORMATION ( 'NONE', 'NONE', #8814,  #43395 ) ;
#48914 = CARTESIAN_POINT ( 'NONE',  ( -95.00000000000002842, 90.00000000000004263, 90.00000000000000000 ) ) ;
#48915 = VERTEX_POINT ( 'NONE', #43101 ) ;
#48916 = VECTOR ( 'NONE', #60114, 1000.000000000000000 ) ;
#48917 = ORIENTED_EDGE ( 'NONE', *, *, #1963, .F. ) ;
#48918 = LINE ( 'NONE', #67612, #26964 ) ;
#48919 = ORIENTED_EDGE ( 'NONE', *, *, #33415, .F. ) ;
#48920 = DIRECTION ( 'NONE',  ( -0.7071067811865474617, 0.000000000000000000, 0.7071067811865474617 ) ) ;
#48921 = DIRECTION ( 'NONE',  ( 1.000000000000000000, -0.000000000000000000, -0.000000000000000000 ) ) ;
#48922 = CARTESIAN_POINT ( 'NONE',  ( -93.84685191531254134, 91.99731107132950569, 80.06489583420048461 ) ) ;
#48923 = ORIENTED_EDGE ( 'NONE', *, *, #74332, .T. ) ;
#48924 = CARTESIAN_POINT ( 'NONE',  ( 97.30629616937498838, 88.66845928578037217, 77.20739583420046870 ) ) ;
#48925 = ORIENTED_EDGE ( 'NONE', *, *, #5001, .F. ) ;
#48926 = DIRECTION ( 'NONE',  ( 0.000000000000000000, 0.2079116908177532086, -0.9781476007338069101 ) ) ;
#48927 = CARTESIAN_POINT ( 'NONE',  ( -96.15314808468745866, -211.9973110713294489, 88.47864583420047779 ) ) ;
#48928 = DIRECTION ( 'NONE',  ( 0.000000000000000000, 0.000000000000000000, 1.000000000000000000 ) ) ;
#48929 = FACE_OUTER_BOUND ( 'NONE', #64083, .T. ) ;
#48930 = DIRECTION ( 'NONE',  ( -1.000000000000000000, 0.000000000000000000, -0.000000000000000000 ) ) ;
#48931 = CARTESIAN_POINT ( 'NONE',  ( -96.15314808468745866, -211.9973110713294489, 83.39864583420047950 ) ) ;
#48932 = CARTESIAN_POINT ( 'NONE',  ( 26.09152095774781799, -124.8716048804687375, -2.500000000000000444 ) ) ;
#48933 = CARTESIAN_POINT ( 'NONE',  ( 0.000000000000000000, 70.53064760720278059, 26.01480285779964774 ) ) ;
#48934 = DIRECTION ( 'NONE',  ( 0.000000000000000000, 0.000000000000000000, 1.000000000000000000 ) ) ;
#48935 = ORIENTED_EDGE ( 'NONE', *, *, #18386, .T. ) ;
#48936 = ORIENTED_EDGE ( 'NONE', *, *, #72184, .F. ) ;
#48937 = CARTESIAN_POINT ( 'NONE',  ( 10.00000000000000000, 0.000000000000000000, 0.000000000000000000 ) ) ;
#48938 = CYLINDRICAL_SURFACE ( 'NONE', #9897, 15.80000000000028315 ) ;
#48939 = CARTESIAN_POINT ( 'NONE',  ( 10.00000000000000000, 37.22597642581158084, 10.79786254984347593 ) ) ;
#48940 = CARTESIAN_POINT ( 'NONE',  ( -92.69370383062502583, 88.66845928578038638, 86.09739583420048348 ) ) ;
#48941 = CARTESIAN_POINT ( 'NONE',  ( 10.00000000000000000, 0.000000000000000000, 0.000000000000000000 ) ) ;
#48942 = CARTESIAN_POINT ( 'NONE',  ( 0.000000000000000000, -120.0000000000000000, 125.0000000000000000 ) ) ;
#48943 = DIRECTION ( 'NONE',  ( -1.000000000000000000, -0.000000000000000000, -0.000000000000000000 ) ) ;
#48944 = CIRCLE ( 'NONE', #42961, 77.49899999999999523 ) ;
#48945 = ORIENTED_EDGE ( 'NONE', *, *, #57563, .T. ) ;
#48946 = CYLINDRICAL_SURFACE ( 'NONE', #51253, 3.299999999999997158 ) ;
#48947 = DIRECTION ( 'NONE',  ( 1.000000000000000000, 0.000000000000000000, 0.000000000000000000 ) ) ;
#48948 = CARTESIAN_POINT ( 'NONE',  ( 15.00000000000000000, 5.835314593368777558, 22.81335362449846471 ) ) ;
#48949 = CIRCLE ( 'NONE', #6935, 82.00000000000000000 ) ;
#48950 = ADVANCED_FACE ( 'NONE', ( #19402 ), #42350, .F. ) ;
#48951 = LINE ( 'NONE', #66272, #14115 ) ;
#48952 = DIRECTION ( 'NONE',  ( 1.000000000000000000, 0.000000000000000000, -0.000000000000000000 ) ) ;
#48953 = CARTESIAN_POINT ( 'NONE',  ( 97.64999999999999147, 90.00000000000002842, 86.50750000000000739 ) ) ;
#48954 = CARTESIAN_POINT ( 'NONE',  ( -93.84685191531248449, -208.0026889286704943, 81.96989583420048575 ) ) ;
#48955 = VECTOR ( 'NONE', #33512, 1000.000000000000000 ) ;
#48956 =( LENGTH_UNIT ( ) NAMED_UNIT ( * ) SI_UNIT ( .MILLI., .METRE. ) );
#48957 = EDGE_CURVE ( 'NONE', #63727, #44099, #6330, .T. ) ;
#48958 = CARTESIAN_POINT ( 'NONE',  ( 11.99999999999999822, 0.000000000000000000, 0.000000000000000000 ) ) ;
#48959 = EDGE_CURVE ( 'NONE', #6553, #44444, #63906, .T. ) ;
#48960 = FACE_OUTER_BOUND ( 'NONE', #26700, .T. ) ;
#48961 = CYLINDRICAL_SURFACE ( 'NONE', #28620, 82.00000000000000000 ) ;
#48962 = CARTESIAN_POINT ( 'NONE',  ( 0.000000000000000000, 0.000000000000000000, 0.000000000000000000 ) ) ;
#48963 = ORIENTED_EDGE ( 'NONE', *, *, #56177, .F. ) ;
#48964 = CARTESIAN_POINT ( 'NONE',  ( -97.64999999999996305, -211.5299782133524218, 81.87729166840097150 ) ) ;
#48965 = CARTESIAN_POINT ( 'NONE',  ( 11.99999999999999822, 0.000000000000000000, 0.000000000000000000 ) ) ;
#48966 = CARTESIAN_POINT ( 'NONE',  ( -10.00000000000000000, 0.000000000000000000, 0.000000000000000000 ) ) ;
#48967 = CONICAL_SURFACE ( 'NONE', #68205, 2.449999999999998845, 0.9599310885968813656 ) ;
#48968 = AXIS2_PLACEMENT_3D ( 'NONE', #52915, #1083, #69819 ) ;
#48969 = CARTESIAN_POINT ( 'NONE',  ( -95.00000000000002842, 90.00000000000004263, 90.00000000000000000 ) ) ;
#48970 = EDGE_CURVE ( 'NONE', #37974, #5960, #39919, .T. ) ;
#48971 = ORIENTED_EDGE ( 'NONE', *, *, #4147, .F. ) ;
#48972 = AXIS2_PLACEMENT_3D ( 'NONE', #33609, #73827, #22339 ) ;
#48973 = EDGE_CURVE ( 'NONE', #72829, #71534, #48676, .T. ) ;
#48974 = DIRECTION ( 'NONE',  ( -1.000000000000000000, 0.000000000000000000, 0.000000000000000000 ) ) ;
#48975 =( NAMED_UNIT ( * ) SI_UNIT ( $, .STERADIAN. ) SOLID_ANGLE_UNIT ( ) );
#48976 = EDGE_LOOP ( 'NONE', ( #40054, #16948, #31499, #36507 ) ) ;
#48977 = COLOUR_RGB ( '', 0.09019608, 0.27058824, 0.51372549) ;
#48978 = CARTESIAN_POINT ( 'NONE',  ( -10.00000000000000000, 0.000000000000000000, 0.000000000000000000 ) ) ;
#48979 = ORIENTED_EDGE ( 'NONE', *, *, #45201, .F. ) ;
#48980 = ORIENTED_EDGE ( 'NONE', *, *, #3818, .T. ) ;
#48981 = LINE ( 'NONE', #66660, #40621 ) ;
#48982 = ADVANCED_FACE ( 'NONE', ( #2850 ), #70856, .F. ) ;
#48983 = ADVANCED_FACE ( 'NONE', ( #37779 ), #31003, .T. ) ;
#48984 = ORIENTED_EDGE ( 'NONE', *, *, #51513, .F. ) ;
#48985 = ORIENTED_EDGE ( 'NONE', *, *, #7997, .T. ) ;
#48986 = ORIENTED_EDGE ( 'NONE', *, *, #15284, .F. ) ;
#48987 = VERTEX_POINT ( 'NONE', #14461 ) ;
#48988 = CARTESIAN_POINT ( 'NONE',  ( 0.000000000000000000, -0.8261519478436571973, 77.49459641780886443 ) ) ;
#48989 = VERTEX_POINT ( 'NONE', #3214 ) ;
#48990 = ORIENTED_EDGE ( 'NONE', *, *, #63152, .T. ) ;
#48991 =( BOUNDED_CURVE ( )  B_SPLINE_CURVE ( 2, ( #41901, #14050, #30602, #55025, #25715, #48281, #13323, #3554, #18955 ),
 .UNSPECIFIED., .F., .F. ) 
 B_SPLINE_CURVE_WITH_KNOTS ( ( 3, 2, 2, 2, 3 ),
 ( 0.3386766260354857061, 0.3386767459640170341, 0.3457325115049341147, 0.3527882770458510842, 0.3598440426548558668 ),
 .UNSPECIFIED. ) 
 CURVE ( )  GEOMETRIC_REPRESENTATION_ITEM ( )  RATIONAL_B_SPLINE_CURVE ( ( 0.9999954456810212777, 0.9999977228018045450, 1.000000000000000000, 0.8660254037844387076, 1.000000000000000000, 0.8660254037844387076, 1.000000000000000000, 0.8660254037844387076, 1.000000000000000000 ) ) 
 REPRESENTATION_ITEM ( '' )  );
#48992 = CARTESIAN_POINT ( 'NONE',  ( 92.69370383062498320, 88.66845928578037217, 75.88447916753382572 ) ) ;
#48993 = LINE ( 'NONE', #20438, #29980 ) ;
#48994 = CARTESIAN_POINT ( 'NONE',  ( -97.65000000000000568, 89.99999348150292633, 88.17437522718661569 ) ) ;
#48995 = ORIENTED_EDGE ( 'NONE', *, *, #29176, .T. ) ;
#48996 = AXIS2_PLACEMENT_3D ( 'NONE', #51005, #34447, #5903 ) ;
#48997 = EDGE_LOOP ( 'NONE', ( #47296, #9604, #47897, #14304 ) ) ;
#48998 = ORIENTED_EDGE ( 'NONE', *, *, #28930, .F. ) ;
#48999 = DIRECTION ( 'NONE',  ( -0.000000000000000000, -0.000000000000000000, 1.000000000000000000 ) ) ;
#49000 = VERTEX_POINT ( 'NONE', #20093 ) ;
#49001 = CARTESIAN_POINT ( 'NONE',  ( 95.00000000000000000, -207.3369185715606307, 89.48406250086713953 ) ) ;
#49002 = DIRECTION ( 'NONE',  ( 1.000000000000000222, 2.775557561562891351E-17, 0.000000000000000000 ) ) ;
#49003 = CARTESIAN_POINT ( 'NONE',  ( 11.99999999999999822, -36.72794159290197769, -65.59268652807249111 ) ) ;
#49004 = AXIS2_PLACEMENT_3D ( 'NONE', #25654, #48590, #53856 ) ;
#49005 = DIRECTION ( 'NONE',  ( -1.000000000000000000, -0.000000000000000000, 0.000000000000000000 ) ) ;
#49006 = DIRECTION ( 'NONE',  ( 0.000000000000000000, 0.000000000000000000, -1.000000000000000000 ) ) ;
#49007 = CIRCLE ( 'NONE', #14182, 77.49899999999999523 ) ;
#49008 = DIRECTION ( 'NONE',  ( 0.000000000000000000, 0.8910065241883691201, -0.4539904997395446951 ) ) ;
#49009 = DIRECTION ( 'NONE',  ( -6.951859121168206841E-17, 1.000000000000000000, 0.000000000000000000 ) ) ;
#49010 = DIRECTION ( 'NONE',  ( -1.000000000000000000, -0.000000000000000000, -0.000000000000000000 ) ) ;
#49011 = CARTESIAN_POINT ( 'NONE',  ( -92.34999999999999432, -209.9999999999999716, 75.15687500173430635 ) ) ;
#49012 = CARTESIAN_POINT ( 'NONE',  ( -97.30629616937501680, 88.66845928578038638, 88.58447916753382856 ) ) ;
#49013 = ORIENTED_EDGE ( 'NONE', *, *, #65529, .T. ) ;
#49014 = UNCERTAINTY_MEASURE_WITH_UNIT (LENGTH_MEASURE( 1.000000000000000082E-05 ), #5073, 'distance_accuracy_value', 'NONE');
#49016 = CARTESIAN_POINT ( 'NONE',  ( -96.15314808468751551, 88.00268892867056536, 87.84364583420047268 ) ) ;
#49015 = CARTESIAN_POINT ( 'NONE',  ( 92.34999999999999432, 90.00000000000002842, 76.74437500173429783 ) ) ;
#49017 = ORIENTED_EDGE ( 'NONE', *, *, #18926, .F. ) ;
#49018 = CARTESIAN_POINT ( 'NONE',  ( 94.99999999999998579, 87.33691857156068750, 75.99031250086716227 ) ) ;
#49019 = DIRECTION ( 'NONE',  ( -1.000000000000000000, -0.000000000000000000, -0.000000000000000000 ) ) ;
#49020 = FACE_OUTER_BOUND ( 'NONE', #22667, .T. ) ;
#49021 = DIRECTION ( 'NONE',  ( -1.000000000000000000, 0.000000000000000000, 0.000000000000000000 ) ) ;
#49022 = CARTESIAN_POINT ( 'NONE',  ( -97.64998056384376923, 91.52998943482256777, 78.59645755884378104 ) ) ;
#49023 = CARTESIAN_POINT ( 'NONE',  ( -97.65000000000007674, 91.52997821335250705, 89.31208333333333371 ) ) ;
#49024 = AXIS2_PLACEMENT_3D ( 'NONE', #33624, #47867, #29450 ) ;
#49025 = CARTESIAN_POINT ( 'NONE',  ( -94.99999999999997158, -213.0599564267049857, 87.61874999999999147 ) ) ;
#49026 = DIRECTION ( 'NONE',  ( 0.000000000000000000, 0.000000000000000000, 1.000000000000000000 ) ) ;
#49027 = ORIENTED_EDGE ( 'NONE', *, *, #69684, .F. ) ;
#49028 = AXIS2_PLACEMENT_3D ( 'NONE', #19591, #59462, #70718 ) ;
#49029 = ORIENTED_EDGE ( 'NONE', *, *, #9985, .T. ) ;
#49030 = VECTOR ( 'NONE', #65676, 1000.000000000000000 ) ;
#49031 = VECTOR ( 'NONE', #55744, 1000.000000000000000 ) ;
#49032 = AXIS2_PLACEMENT_3D ( 'NONE', #36209, #1315, #53508 ) ;
#49033 = CARTESIAN_POINT ( 'NONE',  ( -97.64999999969889188, -209.9999754409357422, 87.53856274002470172 ) ) ;
#49034 = DIRECTION ( 'NONE',  ( -1.000000000000000000, 0.000000000000000000, 0.000000000000000000 ) ) ;
#49035 = DIRECTION ( 'NONE',  ( 0.000000000000000000, -0.3090169943749349613, -0.9510565162951576390 ) ) ;
#49036 = EDGE_CURVE ( 'NONE', #14738, #33943, #43051, .T. ) ;
#49037 = DIRECTION ( 'NONE',  ( -1.000000000000000000, 3.061616997868382648E-16, 0.000000000000000000 ) ) ;
#49038 = CARTESIAN_POINT ( 'NONE',  ( 10.00000000000000000, 0.000000000000000000, 0.000000000000000000 ) ) ;
#49039 = DIRECTION ( 'NONE',  ( 0.000000000000000000, 0.000000000000000000, -1.000000000000000000 ) ) ;
#49040 = AXIS2_PLACEMENT_3D ( 'NONE', #44361, #74035, #22546 ) ;
#49041 = VERTEX_POINT ( 'NONE', #70473 ) ;
#49042 = PRODUCT_DEFINITION ( 'UNKNOWN', '', #15990, #48319 ) ;
#49043 = CARTESIAN_POINT ( 'NONE',  ( -93.84685191531254134, 91.99731107132950569, 82.44614583420046472 ) ) ;
#49044 = ADVANCED_FACE ( 'NONE', ( #66353 ), #37027, .T. ) ;
#49045 = DIRECTION ( 'NONE',  ( 1.000000000000000000, -0.000000000000000000, 0.000000000000000000 ) ) ;
#49046 = FACE_OUTER_BOUND ( 'NONE', #54045, .T. ) ;
#49047 = DIRECTION ( 'NONE',  ( -2.603472992746261562E-14, -2.546204323184492723E-14, 1.000000000000000000 ) ) ;
#49048 = ADVANCED_FACE ( 'NONE', ( #71964 ), #48306, .T. ) ;
#49049 = DIRECTION ( 'NONE',  ( 0.000000000000000000, 0.9238795325112851842, 0.3826834323650937786 ) ) ;
#49050 = CARTESIAN_POINT ( 'NONE',  ( 95.00000000002597744, 90.00000000000007105, -75.00000000000000000 ) ) ;
#49051 = DIRECTION ( 'NONE',  ( -1.000000000000000000, 0.000000000000000000, 0.000000000000000000 ) ) ;
#49052 = DIRECTION ( 'NONE',  ( 0.000000000000000000, 0.000000000000000000, 1.000000000000000000 ) ) ;
#49053 = CARTESIAN_POINT ( 'NONE',  ( -3.000000000000000000, 6.762365576493310826, 25.66652317338401090 ) ) ;
#49054 = CARTESIAN_POINT ( 'NONE',  ( 11.99999999999999822, -51.03279382321048985, -55.19960302592120627 ) ) ;
#49055 = EDGE_CURVE ( 'NONE', #24686, #35768, #7545, .T. ) ;
#49056 = EDGE_CURVE ( 'NONE', #39717, #32702, #31512, .T. ) ;
#49057 = AXIS2_PLACEMENT_3D ( 'NONE', #43776, #38114, #41094 ) ;
#49058 = CARTESIAN_POINT ( 'NONE',  ( 92.69370383062498320, 91.33154071421968467, 82.76364583420048859 ) ) ;
#49059 = CIRCLE ( 'NONE', #22619, 37.49900000000001654 ) ;
#49060 = CARTESIAN_POINT ( 'NONE',  ( -97.30629616937497417, -208.6684592857803295, 83.39864583420049371 ) ) ;
#49061 = DIRECTION ( 'NONE',  ( -1.000000000000000000, -0.000000000000000000, -0.000000000000000000 ) ) ;
#49062 = VERTEX_POINT ( 'NONE', #59979 ) ;
#49063 = CARTESIAN_POINT ( 'NONE',  ( 10.00000000000000000, 0.000000000000000000, 0.000000000000000000 ) ) ;
#49064 = CARTESIAN_POINT ( 'NONE',  ( -93.67499999999998295, -207.7050326799711968, 77.08833333333332405 ) ) ;
#49065 = DIRECTION ( 'NONE',  ( -1.000000000000000000, 0.000000000000000000, 0.000000000000000000 ) ) ;
#49066 = AXIS2_PLACEMENT_3D ( 'NONE', #45561, #29343, #34621 ) ;
#49067 = VECTOR ( 'NONE', #37248, 1000.000000000000000 ) ;
#49069 = EDGE_CURVE ( 'NONE', #20728, #49481, #31744, .T. ) ;
#49068 = CARTESIAN_POINT ( 'NONE',  ( 95.00000000000000000, -207.3369185715606307, 82.49906250086714010 ) ) ;
#49070 = ORIENTED_EDGE ( 'NONE', *, *, #65266, .F. ) ;
#49071 = EDGE_CURVE ( 'NONE', #4157, #7707, #47567, .T. ) ;
#49072 =( NAMED_UNIT ( * ) SI_UNIT ( $, .STERADIAN. ) SOLID_ANGLE_UNIT ( ) );
#49073 = ORIENTED_EDGE ( 'NONE', *, *, #42439, .F. ) ;
#49074 = DIRECTION ( 'NONE',  ( 0.000000000000000000, 0.000000000000000000, 1.000000000000000000 ) ) ;
#49075 = ORIENTED_EDGE ( 'NONE', *, *, #9417, .F. ) ;
#49076 = CIRCLE ( 'NONE', #1267, 82.00000000000000000 ) ;
#49077 = AXIS2_PLACEMENT_3D ( 'NONE', #66285, #59907, #55355 ) ;
#49078 = CYLINDRICAL_SURFACE ( 'NONE', #73119, 77.49899999999999523 ) ;
#49079 = AXIS2_PLACEMENT_3D ( 'NONE', #14608, #61232, #27360 ) ;
#49080 = ORIENTED_EDGE ( 'NONE', *, *, #14163, .F. ) ;
#49081 = CIRCLE ( 'NONE', #22635, 16.00000000000000000 ) ;
#49082 = CARTESIAN_POINT ( 'NONE',  ( 97.30629616937498838, -208.6684592857803295, 76.83697916753382628 ) ) ;
#49083 = DIRECTION ( 'NONE',  ( 0.000000000000000000, 0.000000000000000000, 1.000000000000000000 ) ) ;
#49084 = LINE ( 'NONE', #9228, #59220 ) ;
#49085 = AXIS2_PLACEMENT_3D ( 'NONE', #70887, #60008, #8492 ) ;
#49086 = DIRECTION ( 'NONE',  ( -1.000000000000000000, 0.000000000000000000, -0.000000000000000000 ) ) ;
#49087 = FACE_OUTER_BOUND ( 'NONE', #39799, .T. ) ;
#49088 = LINE ( 'NONE', #31427, #11719 ) ;
#49089 = CARTESIAN_POINT ( 'NONE',  ( 97.64999999999997726, -208.4700217866474645, 80.84541666666666515 ) ) ;
#49090 = ORIENTED_EDGE ( 'NONE', *, *, #7575, .F. ) ;
#49091 = VERTEX_POINT ( 'NONE', #41930 ) ;
#49092 = ORIENTED_EDGE ( 'NONE', *, *, #54847, .F. ) ;
#49093 = ORIENTED_EDGE ( 'NONE', *, *, #21437, .F. ) ;
#49094 = DIRECTION ( 'NONE',  ( 0.000000000000000000, 0.000000000000000000, -1.000000000000000000 ) ) ;
#49095 =( LENGTH_UNIT ( ) NAMED_UNIT ( * ) SI_UNIT ( .MILLI., .METRE. ) );
#49096 = CARTESIAN_POINT ( 'NONE',  ( -92.69370383062502583, 88.66845928578038638, 84.35114583420049428 ) ) ;
#49097 = CARTESIAN_POINT ( 'NONE',  ( -92.35000000000678710, 90.00000598221780024, 82.14187520865721126 ) ) ;
#49098 = CARTESIAN_POINT ( 'NONE',  ( -10.00000000000000000, 0.000000000000000000, 0.000000000000000000 ) ) ;
#49099 = CARTESIAN_POINT ( 'NONE',  ( 93.67499999999998295, 92.29496732002878900, 75.28916666666665947 ) ) ;
#49100 = LINE ( 'NONE', #21254, #64433 ) ;
#49101 = ORIENTED_EDGE ( 'NONE', *, *, #53507, .F. ) ;
#49102 = AXIS2_PLACEMENT_3D ( 'NONE', #6141, #29772, #24520 ) ;
#49103 = CARTESIAN_POINT ( 'NONE',  ( -94.99999999999997158, -206.9400435732949575, 86.11062500173430578 ) ) ;
#49104 = ORIENTED_EDGE ( 'NONE', *, *, #14410, .F. ) ;
#49105 = CARTESIAN_POINT ( 'NONE',  ( -2.500000000000017319, -80.00000000000001421, -189.9999999999999147 ) ) ;
#49106 = ORIENTED_EDGE ( 'NONE', *, *, #56873, .T. ) ;
#49107 = CARTESIAN_POINT ( 'NONE',  ( -95.00000000000002842, 86.94004357329504273, 83.88812500173429498 ) ) ;
#49108 = MECHANICAL_DESIGN_GEOMETRIC_PRESENTATION_REPRESENTATION (  '', ( #35908 ), #26299 ) ;
#49109 = VERTEX_POINT ( 'NONE', #64869 ) ;
#49110 = CARTESIAN_POINT ( 'NONE',  ( 97.30629616937498838, 88.66845928578037217, 88.16114583420048234 ) ) ;
#49111 = CARTESIAN_POINT ( 'NONE',  ( 10.00000000000000000, 4.992566952385523393, -37.16516213103272293 ) ) ;
#49113 = EDGE_CURVE ( 'NONE', #39397, #6687, #43569, .T. ) ;
#49112 = CARTESIAN_POINT ( 'NONE',  ( -34.02017708624680381, -109.8571428571428470, 2.500000000000000000 ) ) ;
#49114 = CIRCLE ( 'NONE', #27483, 82.00000000000000000 ) ;
#49115 = DIRECTION ( 'NONE',  ( 0.7273375899149802093, -0.6862798483830544471, 0.000000000000000000 ) ) ;
#49116 = CARTESIAN_POINT ( 'NONE',  ( 5.999999999999999112, 55.16347631943042984, 60.67117009219155932 ) ) ;
#49117 = CARTESIAN_POINT ( 'NONE',  ( 10.00000000000000000, 63.97538442413500093, -51.29473840253157135 ) ) ;
#49118 = VERTEX_POINT ( 'NONE', #36280 ) ;
#49119 = CARTESIAN_POINT ( 'NONE',  ( 10.00000000000000000, 75.11764819372149304, -2.946379043146603482 ) ) ;
#49120 = DIRECTION ( 'NONE',  ( -0.000000000000000000, -0.5000000000000004441, 0.8660254037844383745 ) ) ;
#49121 = VERTEX_POINT ( 'NONE', #59218 ) ;
#49122 = VECTOR ( 'NONE', #69493, 1000.000000000000000 ) ;
#49123 = EDGE_LOOP ( 'NONE', ( #18707, #69347, #31132, #50474 ) ) ;
#49124 = EDGE_CURVE ( 'NONE', #27817, #10962, #18328, .T. ) ;
#49125 = DIRECTION ( 'NONE',  ( -1.000000000000000000, 0.000000000000000000, 0.000000000000000000 ) ) ;
#49126 = ADVANCED_FACE ( 'NONE', ( #54324 ), #36650, .F. ) ;
#49127 = CARTESIAN_POINT ( 'NONE',  ( 0.000000000000000000, 16.83928648764923253, 16.46020748918050458 ) ) ;
#49128 = CYLINDRICAL_SURFACE ( 'NONE', #29285, 77.49899999999999523 ) ;
#49129 = CARTESIAN_POINT ( 'NONE',  ( -94.99999999999997158, -212.6630814284392557, 84.88031250086714863 ) ) ;
#49130 = ORIENTED_EDGE ( 'NONE', *, *, #20978, .F. ) ;
#49131 = CARTESIAN_POINT ( 'NONE',  ( 10.00000000000000000, -28.89263327155693517, -71.91182617369219088 ) ) ;
#49132 = ORIENTED_EDGE ( 'NONE', *, *, #44760, .F. ) ;
#49133 = AXIS2_PLACEMENT_3D ( 'NONE', #61546, #72065, #20575 ) ;
#49134 = EDGE_CURVE ( 'NONE', #31970, #57738, #19724, .T. ) ;
#49135 = AXIS2_PLACEMENT_3D ( 'NONE', #15748, #26272, #4118 ) ;
#49136 = CARTESIAN_POINT ( 'NONE',  ( 0.000000000000000000, -0.8299999999999999600, -1.199999999999999956 ) ) ;
#49137 = CIRCLE ( 'NONE', #58760, 42.00000000000000000 ) ;
#49138 = VECTOR ( 'NONE', #42747, 1000.000000000000000 ) ;
#49139 = DIRECTION ( 'NONE',  ( 0.000000000000000000, 0.000000000000000000, 1.000000000000000000 ) ) ;
#49140 = CARTESIAN_POINT ( 'NONE',  ( -97.64999999999996305, -209.9999999999999716, 76.10937500173430692 ) ) ;
#49141 = CARTESIAN_POINT ( 'NONE',  ( 97.30629616937498838, 90.00000000000002842, 79.16531250086714522 ) ) ;
#49142 = DIRECTION ( 'NONE',  ( -1.000000000000000000, -0.000000000000000000, -0.000000000000000000 ) ) ;
#49143 = CARTESIAN_POINT ( 'NONE',  ( 10.00000000000000000, 35.95386929396256903, -10.96151621346501237 ) ) ;
#49144 = DIRECTION ( 'NONE',  ( 1.000000000000000000, 0.000000000000000000, 0.000000000000000000 ) ) ;
#49145 = CIRCLE ( 'NONE', #32326, 42.00000000000000000 ) ;
#49146 = CARTESIAN_POINT ( 'NONE',  ( 93.09104985768151153, 91.56137061862943938, 74.88237134757152091 ) ) ;
#49147 = VECTOR ( 'NONE', #10137, 1000.000000000000114 ) ;
#49148 = DIRECTION ( 'NONE',  ( 1.000000000000000000, 0.000000000000000000, -0.000000000000000000 ) ) ;
#49149 = CARTESIAN_POINT ( 'NONE',  ( 15.00000000000000000, 0.000000000000000000, 0.000000000000000000 ) ) ;
#49150 = EDGE_CURVE ( 'NONE', #61762, #20511, #45977, .T. ) ;
#49151 = CARTESIAN_POINT ( 'NONE',  ( 1.560000000000000053, 1.732050807568878747, 7.017607234860990640E-28 ) ) ;
#49152 = CARTESIAN_POINT ( 'NONE',  ( 97.64999999999990621, 91.52997821335254969, 89.10041666666667481 ) ) ;
#49153 = ORIENTED_EDGE ( 'NONE', *, *, #44564, .T. ) ;
#49154 = CARTESIAN_POINT ( 'NONE',  ( -96.15314808468751551, 88.00268892867056536, 81.49364583420047836 ) ) ;
#49155 = CARTESIAN_POINT ( 'NONE',  ( 15.00000000000000000, -26.23277895567245466, 4.042438405570107918 ) ) ;
#49157 = EDGE_CURVE ( 'NONE', #55565, #11405, #72691, .T. ) ;
#49156 = DIRECTION ( 'NONE',  ( -1.000000000000000000, -0.000000000000000000, -0.000000000000000000 ) ) ;
#49158 = EDGE_CURVE ( 'NONE', #48440, #7925, #27202, .T. ) ;
#49159 = ORIENTED_EDGE ( 'NONE', *, *, #50, .T. ) ;
#49161 = DIRECTION ( 'NONE',  ( -0.000000000000000000, 0.5000000000000004441, 0.8660254037844383745 ) ) ;
#49160 = CIRCLE ( 'NONE', #7156, 16.00000000000000000 ) ;
#49162 = EDGE_CURVE ( 'NONE', #15980, #70981, #16955, .T. ) ;
#49163 = CARTESIAN_POINT ( 'NONE',  ( 97.65000000000003411, 91.52997821335250705, 85.29041666666665833 ) ) ;
#49164 = DIRECTION ( 'NONE',  ( -0.000000000000000000, -0.000000000000000000, -1.000000000000000000 ) ) ;
#49165 = AXIS2_PLACEMENT_3D ( 'NONE', #38244, #15691, #14945 ) ;
#49166 = LINE ( 'NONE', #72091, #7912 ) ;
#49167 = CARTESIAN_POINT ( 'NONE',  ( 92.69370383062501162, -208.6684592857803011, 78.95364583420048632 ) ) ;
#49168 = AXIS2_PLACEMENT_3D ( 'NONE', #28451, #21316, #20958 ) ;
#49169 = VERTEX_POINT ( 'NONE', #72342 ) ;
#49170 = VERTEX_POINT ( 'NONE', #22332 ) ;
#49171 = CARTESIAN_POINT ( 'NONE',  ( 0.000000000000000000, -28.89263327155693517, -71.91182617369219088 ) ) ;
#49172 = DIRECTION ( 'NONE',  ( -1.000000000000000000, -0.000000000000000000, -0.000000000000000000 ) ) ;
#49173 = LINE ( 'NONE', #20608, #23206 ) ;
#49174 = CARTESIAN_POINT ( 'NONE',  ( 15.00000000000000000, -19.89357724625003598, -12.59942793731059041 ) ) ;
#49175 = CARTESIAN_POINT ( 'NONE',  ( 92.69370383062501162, -211.3315407142195852, 77.15447916753382174 ) ) ;
#49176 = AXIS2_PLACEMENT_3D ( 'NONE', #54772, #54403, #42754 ) ;
#49177 = ORIENTED_EDGE ( 'NONE', *, *, #39161, .T. ) ;
#49178 = CARTESIAN_POINT ( 'NONE',  ( 10.00000000000000000, 0.000000000000000000, 0.000000000000000000 ) ) ;
#49179 = ORIENTED_EDGE ( 'NONE', *, *, #50823, .F. ) ;
#49180 = EDGE_LOOP ( 'NONE', ( #21597, #27520, #66500, #39123 ) ) ;
#49181 = CARTESIAN_POINT ( 'NONE',  ( 10.00000000000000000, -27.75498641678720446, -31.52238457039628727 ) ) ;
#49182 = AXIS2_PLACEMENT_3D ( 'NONE', #64104, #11471, #11829 ) ;
#49183 = CIRCLE ( 'NONE', #44434, 82.00000000000000000 ) ;
#49184 = DIRECTION ( 'NONE',  ( -1.000000000000000000, 0.000000000000000000, -0.000000000000000000 ) ) ;
#49185 = AXIS2_PLACEMENT_3D ( 'NONE', #59184, #41886, #58431 ) ;
#49186 = EDGE_LOOP ( 'NONE', ( #587, #19320, #73413, #15445 ) ) ;
#49187 = DIRECTION ( 'NONE',  ( 0.000000000000000000, -0.5877852522924625900, -0.8090169943749551118 ) ) ;
#49188 = CARTESIAN_POINT ( 'NONE',  ( 95.00000000000000000, -213.0599564267049857, 78.80812500173429669 ) ) ;
#49189 = CARTESIAN_POINT ( 'NONE',  ( 97.64999999999999147, 90.00000000000002842, 85.23749999999999716 ) ) ;
#49190 = ORIENTED_EDGE ( 'NONE', *, *, #45797, .T. ) ;
#49191 = DIRECTION ( 'NONE',  ( -0.000000000000000000, 0.8090169943749504489, -0.5877852522924689183 ) ) ;
#49192 = DIRECTION ( 'NONE',  ( -0.000000000000000000, -0.000000000000000000, -1.000000000000000000 ) ) ;
#49193 = ORIENTED_EDGE ( 'NONE', *, *, #59971, .F. ) ;
#49194 = CARTESIAN_POINT ( 'NONE',  ( -92.69370383062505425, 88.66845928578038638, 88.16114583420048234 ) ) ;
#49195 = CARTESIAN_POINT ( 'NONE',  ( 97.30629616937498838, 90.00000000000002842, 82.34031250086714238 ) ) ;
#49196 = ORIENTED_EDGE ( 'NONE', *, *, #26415, .F. ) ;
#49197 = EDGE_CURVE ( 'NONE', #63730, #36680, #19551, .T. ) ;
#49198 = DIRECTION ( 'NONE',  ( -1.000000000000000000, 0.000000000000000000, 0.000000000000000000 ) ) ;
#49199 = ORIENTED_EDGE ( 'NONE', *, *, #52726, .T. ) ;
#49200 = CARTESIAN_POINT ( 'NONE',  ( 3.000000000000000000, 1.467624384280025174, -2.542000000000001592 ) ) ;
#49201 = ORIENTED_EDGE ( 'NONE', *, *, #51278, .T. ) ;
#49202 = EDGE_LOOP ( 'NONE', ( #72398, #27351, #30856, #51881 ) ) ;
#49203 = ORIENTED_EDGE ( 'NONE', *, *, #9829, .T. ) ;
#49204 = EDGE_CURVE ( 'NONE', #1611, #1093, #38509, .T. ) ;
#49205 = FACE_OUTER_BOUND ( 'NONE', #66762, .T. ) ;
#49206 = EDGE_CURVE ( 'NONE', #71846, #62877, #4689, .T. ) ;
#49207 = ORIENTED_EDGE ( 'NONE', *, *, #24508, .T. ) ;
#49208 =( BOUNDED_CURVE ( )  B_SPLINE_CURVE ( 2, ( #9950, #32872, #55821, #44552, #52392, #69320, #40761, #13282, #63328, #64430, #35111 ),
 .UNSPECIFIED., .F., .F. ) 
 B_SPLINE_CURVE_WITH_KNOTS ( ( 3, 2, 2, 2, 2, 3 ),
 ( 0.4233457466685772164, 0.4233459324529421641, 0.4304016979938243836, 0.4374574635347066587, 0.4445132290755888782, 0.4445132602971387792 ),
 .UNSPECIFIED. ) 
 CURVE ( )  GEOMETRIC_REPRESENTATION_ITEM ( )  RATIONAL_B_SPLINE_CURVE ( ( 0.9999929448534692344, 0.9999964723338481409, 1.000000000000000000, 0.8660254037844387076, 1.000000000000000000, 0.8660254037844387076, 1.000000000000000000, 0.8660254037844387076, 1.000000000000000000, 0.9999994071664494166, 0.9999988143381453032 ) ) 
 REPRESENTATION_ITEM ( '' )  );
#49209 = CARTESIAN_POINT ( 'NONE',  ( 11.99999999999999822, -75.54627589209931671, -17.28742895386162814 ) ) ;
#49210 = ORIENTED_EDGE ( 'NONE', *, *, #64926, .F. ) ;
#49211 = CARTESIAN_POINT ( 'NONE',  ( 11.99999999999999822, -74.65491531819124305, 8.830959090342128448 ) ) ;
#49212 = CARTESIAN_POINT ( 'NONE',  ( -97.30629616937497417, -208.6684592857803011, 78.79489583420047438 ) ) ;
#49213 = ORIENTED_EDGE ( 'NONE', *, *, #49716, .T. ) ;
#49214 = AXIS2_PLACEMENT_3D ( 'NONE', #2826, #60323, #38486 ) ;
#49215 = CARTESIAN_POINT ( 'NONE',  ( 0.000000000000000000, 0.000000000000000000, 0.000000000000000000 ) ) ;
#49216 = DIRECTION ( 'NONE',  ( -0.000000000000000000, 0.5000000000000019984, 0.8660254037844374864 ) ) ;
#49217 = CARTESIAN_POINT ( 'NONE',  ( 8.000000000000000000, -1.281981485932089404E-13, -13.10000000000022879 ) ) ;
#49218 = CARTESIAN_POINT ( 'NONE',  ( 10.00000000000000000, 37.22597642581158084, -5.202137450156524068 ) ) ;
#49219 = EDGE_CURVE ( 'NONE', #73384, #20377, #50137, .T. ) ;
#49220 = AXIS2_PLACEMENT_3D ( 'NONE', #73072, #73820, #44532 ) ;
#49221 = DIRECTION ( 'NONE',  ( 0.000000000000000000, 0.000000000000000000, 1.000000000000000000 ) ) ;
#49222 = DIRECTION ( 'NONE',  ( -1.000000000000000000, 0.000000000000000000, 0.000000000000000000 ) ) ;
#49224 = CARTESIAN_POINT ( 'NONE',  ( 92.69370383062498320, 88.66845928578035796, 87.79072916753379729 ) ) ;
#49223 = CIRCLE ( 'NONE', #50456, 31.99999999999999289 ) ;
#49225 = FACE_OUTER_BOUND ( 'NONE', #7422, .T. ) ;
#49226 = LINE ( 'NONE', #27400, #18157 ) ;
#49227 = CARTESIAN_POINT ( 'NONE',  ( 95.73997229764715655, -212.5681771730651235, 75.00000000000000000 ) ) ;
#49228 = DIRECTION ( 'NONE',  ( -1.000000000000000000, 0.000000000000000000, 0.000000000000000000 ) ) ;
#49229 = FACE_OUTER_BOUND ( 'NONE', #39285, .T. ) ;
#49230 = DIRECTION ( 'NONE',  ( 0.000000000000000000, 0.000000000000000000, 1.000000000000000000 ) ) ;
#49231 = EDGE_CURVE ( 'NONE', #14688, #66971, #55816, .T. ) ;
#49232 = LINE ( 'NONE', #26298, #10327 ) ;
#49233 = EDGE_CURVE ( 'NONE', #42280, #18118, #30343, .T. ) ;
#49234 = DIRECTION ( 'NONE',  ( -1.000000000000000000, 0.000000000000000000, 0.000000000000000000 ) ) ;
#49235 = CIRCLE ( 'NONE', #3658, 3.299999999999983391 ) ;
#49236 = DIRECTION ( 'NONE',  ( -1.000000000000000000, -0.000000000000000000, -0.000000000000000000 ) ) ;
#49238 = CARTESIAN_POINT ( 'NONE',  ( 92.69370383062498320, 88.66845928578035796, 89.21947916753381946 ) ) ;
#49237 = AXIS2_PLACEMENT_3D ( 'NONE', #67045, #61423, #22303 ) ;
#49239 = AXIS2_PLACEMENT_3D ( 'NONE', #14069, #65979, #20084 ) ;
#49240 = FACE_OUTER_BOUND ( 'NONE', #58425, .T. ) ;
#49241 = LINE ( 'NONE', #5544, #64061 ) ;
#49242 = CARTESIAN_POINT ( 'NONE',  ( -97.64999999999994884, -208.4700217866474645, 87.40708333333333258 ) ) ;
#49243 = VECTOR ( 'NONE', #21071, 1000.000000000000000 ) ;
#49244 = AXIS2_PLACEMENT_3D ( 'NONE', #70322, #31225, #59077 ) ;
#49245 = DIRECTION ( 'NONE',  ( -1.000000000000000000, 0.000000000000000000, 0.000000000000000000 ) ) ;
#49246 = EDGE_CURVE ( 'NONE', #71442, #3546, #57942, .T. ) ;
#49247 = EDGE_CURVE ( 'NONE', #30413, #33465, #59172, .T. ) ;
#49248 = ORIENTED_EDGE ( 'NONE', *, *, #55925, .T. ) ;
#49249 = DIRECTION ( 'NONE',  ( -1.000000000000000000, -0.000000000000000000, 0.000000000000000000 ) ) ;
#49250 = CARTESIAN_POINT ( 'NONE',  ( 10.00000000000000000, 0.000000000000000000, 0.000000000000000000 ) ) ;
#49251 = FACE_OUTER_BOUND ( 'NONE', #58464, .T. ) ;
#49252 = CARTESIAN_POINT ( 'NONE',  ( 11.99999999999999822, 77.49459641780886443, 0.8261519478433866359 ) ) ;
#49253 = VECTOR ( 'NONE', #35295, 1000.000000000000000 ) ;
#49254 = ORIENTED_EDGE ( 'NONE', *, *, #56650, .F. ) ;
#49255 = ORIENTED_EDGE ( 'NONE', *, *, #47643, .T. ) ;
#49256 = CARTESIAN_POINT ( 'NONE',  ( 0.000000000000000000, 0.000000000000000000, 0.000000000000000000 ) ) ;
#49257 = DIRECTION ( 'NONE',  ( 0.5687579148473743684, -0.8225049752423791993, 0.000000000000000000 ) ) ;
#49258 = ORIENTED_EDGE ( 'NONE', *, *, #64197, .F. ) ;
#49259 = CARTESIAN_POINT ( 'NONE',  ( 93.84685191531249870, -208.0026889286704943, 81.91697916753381037 ) ) ;
#49260 = CARTESIAN_POINT ( 'NONE',  ( 97.30629616937498838, -209.9999999999999716, 83.76906250086716454 ) ) ;
#49261 = VERTEX_POINT ( 'NONE', #67074 ) ;
#49262 = B_SPLINE_CURVE_WITH_KNOTS ( 'NONE', 3,
 ( #49967, #71784, #72888, #14650 ),
 .UNSPECIFIED., .F., .F.,
 ( 4, 4 ),
 ( 2.380735200807732181E-07, 0.002921158011986708155 ),
 .UNSPECIFIED. ) ;
#49263 = CARTESIAN_POINT ( 'NONE',  ( 95.00000000000000000, -212.6630814284392557, 88.05531250086716000 ) ) ;
#49264 = CIRCLE ( 'NONE', #72079, 31.99999999999998579 ) ;
#49265 = ORIENTED_EDGE ( 'NONE', *, *, #45634, .F. ) ;
#49266 = CARTESIAN_POINT ( 'NONE',  ( 4.999999999999999112, -9.188173127307004862, -40.98264845739759465 ) ) ;
#49267 = EDGE_LOOP ( 'NONE', ( #24351, #44406, #28892, #62109 ) ) ;
#49268 = CIRCLE ( 'NONE', #61305, 77.49900000000000944 ) ;
#49269 = CARTESIAN_POINT ( 'NONE',  ( -97.30629616937501680, 88.66845928578038638, 76.51947916753381662 ) ) ;
#49270 = ORIENTED_EDGE ( 'NONE', *, *, #70110, .F. ) ;
#49271 = ORIENTED_EDGE ( 'NONE', *, *, #67204, .F. ) ;
#49272 = VECTOR ( 'NONE', #25816, 1000.000000000000000 ) ;
#49273 = DIRECTION ( 'NONE',  ( -1.000000000000000000, 0.000000000000000000, -0.000000000000000000 ) ) ;
#49274 = ORIENTED_EDGE ( 'NONE', *, *, #13057, .F. ) ;
#49275 = LINE ( 'NONE', #37275, #18521 ) ;
#49276 = FACE_OUTER_BOUND ( 'NONE', #9520, .T. ) ;
#49277 = ORIENTED_EDGE ( 'NONE', *, *, #13560, .F. ) ;
#49278 = CARTESIAN_POINT ( 'NONE',  ( -3.000000000000000000, -13.04903810567647682, -19.60159698893442481 ) ) ;
#49279 = EDGE_LOOP ( 'NONE', ( #38473, #65303 ) ) ;
#49280 = CARTESIAN_POINT ( 'NONE',  ( 0.000000000000000000, -81.50828551894234408, 8.966570791700407383 ) ) ;
#49281 = ORIENTED_EDGE ( 'NONE', *, *, #11316, .T. ) ;
#49282 = ADVANCED_FACE ( 'NONE', ( #56168 ), #73450, .T. ) ;
#49283 = ORIENTED_EDGE ( 'NONE', *, *, #71170, .F. ) ;
#49284 = ORIENTED_EDGE ( 'NONE', *, *, #36061, .F. ) ;
#49285 = CARTESIAN_POINT ( 'NONE',  ( 93.84685191531251292, -211.9973110713294489, 77.68364583420047609 ) ) ;
#49286 = ITEM_DEFINED_TRANSFORMATION ( 'NONE', 'NONE', #62823,  #43395 ) ;
#49287 = DIRECTION ( 'NONE',  ( 1.000000000000000000, 0.000000000000000000, 0.000000000000000000 ) ) ;
#49289 = EDGE_CURVE ( 'NONE', #47641, #32707, #44901, .T. ) ;
#49288 = ORIENTED_EDGE ( 'NONE', *, *, #30390, .F. ) ;
#49290 = VECTOR ( 'NONE', #13518, 1000.000000000000000 ) ;
#49291 = ORIENTED_EDGE ( 'NONE', *, *, #74193, .F. ) ;
#49292 = VERTEX_POINT ( 'NONE', #56558 ) ;
#49293 = CARTESIAN_POINT ( 'NONE',  ( -2.500000000000015543, -73.00000000000001421, -204.9999999999999716 ) ) ;
#49294 = ADVANCED_FACE ( 'NONE', ( #3947 ), #50894, .T. ) ;
#49295 = DIRECTION ( 'NONE',  ( -1.000000000000000000, 0.000000000000000000, 0.000000000000000000 ) ) ;
#49296 = CARTESIAN_POINT ( 'NONE',  ( -96.15314808468751551, 88.00268892867056536, 79.11239583420048405 ) ) ;
#49297 = VERTEX_POINT ( 'NONE', #49415 ) ;
#49298 = CARTESIAN_POINT ( 'NONE',  ( 92.69370383062498320, 90.00000000000002842, 78.21281250086714465 ) ) ;
#49299 = ORIENTED_EDGE ( 'NONE', *, *, #3921, .F. ) ;
#49300 = CYLINDRICAL_SURFACE ( 'NONE', #74335, 2.649999999999985700 ) ;
#49301 = CARTESIAN_POINT ( 'NONE',  ( -97.30629616937495996, -209.9999999999999716, 89.64281250086713726 ) ) ;
#49302 = DIRECTION ( 'NONE',  ( 0.000000000000000000, -0.9723699203976740035, -0.2334453638559160216 ) ) ;
#49303 = FACE_BOUND ( 'NONE', #46331, .T. ) ;
#49304 = DIRECTION ( 'NONE',  ( -0.000000000000000000, -0.000000000000000000, -1.000000000000000000 ) ) ;
#49305 = CARTESIAN_POINT ( 'NONE',  ( -92.69370383062498320, -209.9999999999999716, 79.80031250086713612 ) ) ;
#49306 = EDGE_CURVE ( 'NONE', #59102, #17492, #25509, .T. ) ;
#49307 = LINE ( 'NONE', #60963, #18219 ) ;
#49308 = DIRECTION ( 'NONE',  ( 0.000000000000000000, 0.5877852522924742473, -0.8090169943749465631 ) ) ;
#49309 = LINE ( 'NONE', #60250, #62361 ) ;
#49310 = ORIENTED_EDGE ( 'NONE', *, *, #19832, .F. ) ;
#49311 = ORIENTED_EDGE ( 'NONE', *, *, #9782, .T. ) ;
#49312 = PLANE ( 'NONE',  #7283 ) ;
#49313 = DIRECTION ( 'NONE',  ( -1.000000000000000000, -0.000000000000000000, 0.000000000000000000 ) ) ;
#49314 = CARTESIAN_POINT ( 'NONE',  ( -95.00000000000002842, 86.94004357329504273, 84.52312500173428589 ) ) ;
#49315 = CARTESIAN_POINT ( 'NONE',  ( -97.30629616937501680, 91.33154071421968467, 86.41489583420047893 ) ) ;
#49316 = DIRECTION ( 'NONE',  ( -1.000000000000000000, -0.000000000000000000, -0.000000000000000000 ) ) ;
#49317 = DIRECTION ( 'NONE',  ( -1.000000000000000000, -0.000000000000000000, 0.000000000000000000 ) ) ;
#49318 = EDGE_CURVE ( 'NONE', #18969, #26720, #69943, .T. ) ;
#49319 = ORIENTED_EDGE ( 'NONE', *, *, #65258, .T. ) ;
#49320 = EDGE_CURVE ( 'NONE', #69188, #11199, #71166, .T. ) ;
#49321 = CARTESIAN_POINT ( 'NONE',  ( 0.000000000000000000, 8.830959090343430518, -74.65491531819107252 ) ) ;
#49322 = CIRCLE ( 'NONE', #38546, 31.99999999999998934 ) ;
#49323 = AXIS2_PLACEMENT_3D ( 'NONE', #67432, #21179, #44131 ) ;
#49324 = AXIS2_PLACEMENT_3D ( 'NONE', #50138, #67450, #15942 ) ;
#49325 = EDGE_CURVE ( 'NONE', #50470, #22556, #23174, .T. ) ;
#49327 = EDGE_CURVE ( 'NONE', #53848, #27808, #15966, .T. ) ;
#49326 = DIRECTION ( 'NONE',  ( 0.000000000000000000, 0.000000000000000000, -1.000000000000000000 ) ) ;
#49328 = DIRECTION ( 'NONE',  ( 0.000000000000000000, 0.000000000000000000, 1.000000000000000000 ) ) ;
#49329 = DIRECTION ( 'NONE',  ( -1.000000000000000000, 0.000000000000000000, 0.000000000000000000 ) ) ;
#49330 = CARTESIAN_POINT ( 'NONE',  ( -2.744988726042923766, 4.188682711992889551, -0.5083873451168725577 ) ) ;
#49331 = CARTESIAN_POINT ( 'NONE',  ( -95.00000000000002842, 93.05995642670504253, 87.30124999999999602 ) ) ;
#49332 = CARTESIAN_POINT ( 'NONE',  ( -96.15314808468745866, -211.9973110713294489, 83.55739583420049144 ) ) ;
#49333 = CARTESIAN_POINT ( 'NONE',  ( 2.874421927457452952, -143.3717286177755739, -2.500000000000000000 ) ) ;
#49334 = EDGE_CURVE ( 'NONE', #15908, #39621, #42126, .T. ) ;
#49335 = DIRECTION ( 'NONE',  ( 1.000000000000000000, -0.000000000000000000, -0.000000000000000000 ) ) ;
#49336 = DIRECTION ( 'NONE',  ( 2.603472992746261562E-14, 2.546204323184492723E-14, -1.000000000000000000 ) ) ;
#49337 = DIRECTION ( 'NONE',  ( -0.08130631524009862554, 0.9966891607226787686, 0.000000000000000000 ) ) ;
#49338 = VECTOR ( 'NONE', #41734, 1000.000000000000000 ) ;
#49339 = VERTEX_POINT ( 'NONE', #19541 ) ;
#49340 = EDGE_CURVE ( 'NONE', #17937, #71124, #63513, .T. ) ;
#49341 = DIRECTION ( 'NONE',  ( 0.000000000000000000, 0.000000000000000000, 1.000000000000000000 ) ) ;
#49342 = FACE_OUTER_BOUND ( 'NONE', #868, .T. ) ;
#49343 = DIRECTION ( 'NONE',  ( 1.000000000000000000, 1.427937372958388501E-15, -7.962523111839142123E-16 ) ) ;
#49344 = CIRCLE ( 'NONE', #63759, 82.00000000000000000 ) ;
#49345 = AXIS2_PLACEMENT_3D ( 'NONE', #21362, #45072, #44320 ) ;
#49346 = AXIS2_PLACEMENT_3D ( 'NONE', #6003, #68773, #10884 ) ;
#49347 =( BOUNDED_CURVE ( )  B_SPLINE_CURVE ( 2, ( #56053, #73703, #16567, #51522, #9815, #4197, #44411 ),
 .UNSPECIFIED., .F., .F. ) 
 B_SPLINE_CURVE_WITH_KNOTS ( ( 3, 2, 2, 3 ),
 ( 0.08333333333333288462, 0.09027777777777759582, 0.09722222222222230703, 0.1041666666666670182 ),
 .UNSPECIFIED. ) 
 CURVE ( )  GEOMETRIC_REPRESENTATION_ITEM ( )  RATIONAL_B_SPLINE_CURVE ( ( 1.000000000000008660, 0.8660254037844301589, 1.000000000000000000, 0.8660254037844387076, 1.000000000000000000, 0.8660254037844320463, 1.000000000000006661 ) ) 
 REPRESENTATION_ITEM ( '' )  );
#49348 = DIRECTION ( 'NONE',  ( 1.000000000000000000, -0.000000000000000000, -0.000000000000000000 ) ) ;
#49349 = ORIENTED_EDGE ( 'NONE', *, *, #61366, .T. ) ;
#49350 = DIRECTION ( 'NONE',  ( 0.000000000000000000, -0.1564344650402380854, 0.9876883405951365491 ) ) ;
#49351 = DIRECTION ( 'NONE',  ( 0.8774505977381978905, 0.4796670183876304283, 0.000000000000000000 ) ) ;
#49352 = ORIENTED_EDGE ( 'NONE', *, *, #13982, .T. ) ;
#49353 = DIRECTION ( 'NONE',  ( -0.1276937514489679404, -0.9918136447140103451, 0.000000000000000000 ) ) ;
#49354 = CARTESIAN_POINT ( 'NONE',  ( -92.35002849301773153, -208.4700053361959817, 87.27479280632964276 ) ) ;
#49355 = VERTEX_POINT ( 'NONE', #68940 ) ;
#49356 = CARTESIAN_POINT ( 'NONE',  ( 10.00000000000000000, -68.55367621811110723, -44.99326035066125939 ) ) ;
#49357 = ORIENTED_EDGE ( 'NONE', *, *, #61870, .F. ) ;
#49358 = CARTESIAN_POINT ( 'NONE',  ( 0.000000000000000000, 50.95692526931328104, 58.39081064771769292 ) ) ;
#49359 = ORIENTED_EDGE ( 'NONE', *, *, #62108, .T. ) ;
#49360 = EDGE_LOOP ( 'NONE', ( #33642, #18209, #67328, #45197 ) ) ;
#49361 = ORIENTED_EDGE ( 'NONE', *, *, #58078, .F. ) ;
#49362 = ORIENTED_EDGE ( 'NONE', *, *, #15505, .F. ) ;
#49363 = LINE ( 'NONE', #65564, #13095 ) ;
#49364 = ORIENTED_EDGE ( 'NONE', *, *, #23625, .F. ) ;
#49365 = PRODUCT ( 'socket button head screw_iso_ISO 7380 - M5 x 20 - 20N', 'socket button head screw_iso_ISO 7380 - M5 x 20 - 20N', '', ( #44868 ) ) ;
#49366 = ORIENTED_EDGE ( 'NONE', *, *, #20263, .F. ) ;
#49367 = CARTESIAN_POINT ( 'NONE',  ( 93.84685191531248449, 91.99731107132950569, 77.63072916753381492 ) ) ;
#49368 = DIRECTION ( 'NONE',  ( 1.000000000000000000, 0.000000000000000000, 0.000000000000000000 ) ) ;
#49369 = DIRECTION ( 'NONE',  ( 0.000000000000000000, 0.000000000000000000, -1.000000000000000000 ) ) ;
#49370 = ORIENTED_EDGE ( 'NONE', *, *, #10291, .F. ) ;
#49371 = ORIENTED_EDGE ( 'NONE', *, *, #52550, .F. ) ;
#49372 = COLOUR_RGB ( '', 0.09019608, 0.27058824, 0.51372549) ;
#49373 = EDGE_CURVE ( 'NONE', #49572, #53174, #17855, .T. ) ;
#49374 = ORIENTED_EDGE ( 'NONE', *, *, #70041, .F. ) ;
#49375 = CARTESIAN_POINT ( 'NONE',  ( 92.69370383062498320, 88.66845928578037217, 87.15572916753380639 ) ) ;
#49376 = AXIS2_PLACEMENT_3D ( 'NONE', #27787, #68764, #5250 ) ;
#49377 = ORIENTED_EDGE ( 'NONE', *, *, #37367, .T. ) ;
#49378 = CARTESIAN_POINT ( 'NONE',  ( 93.84685191531249870, -208.0026889286704943, 89.53697916753381492 ) ) ;
#49379 = DIRECTION ( 'NONE',  ( 1.000000000000000000, 0.000000000000000000, 0.000000000000000000 ) ) ;
#49380 = LINE ( 'NONE', #67792, #8978 ) ;
#49381 = EDGE_CURVE ( 'NONE', #59117, #44464, #33942, .T. ) ;
#49383 = DIRECTION ( 'NONE',  ( 0.000000000000000000, 0.000000000000000000, 1.000000000000000000 ) ) ;
#49382 = VECTOR ( 'NONE', #53491, 1000.000000000000000 ) ;
#49384 = CARTESIAN_POINT ( 'NONE',  ( -7.500000000000016875, -80.00000000000001421, -269.9999999999999432 ) ) ;
#49385 = CARTESIAN_POINT ( 'NONE',  ( -6.170112525937322623, 10.87104923258428180, -54.99999999999998579 ) ) ;
#49386 = CARTESIAN_POINT ( 'NONE',  ( -92.34999999999995168, -208.4700217866474929, 82.75041666666666629 ) ) ;
#49387 = ADVANCED_FACE ( 'NONE', ( #57283 ), #63304, .T. ) ;
#49388 = FACE_OUTER_BOUND ( 'NONE', #65601, .T. ) ;
#49389 = EDGE_CURVE ( 'NONE', #43677, #54048, #62954, .T. ) ;
#49390 = CARTESIAN_POINT ( 'NONE',  ( -92.34999999999999432, -208.4700217866474645, 77.11479166840095445 ) ) ;
#49391 = CARTESIAN_POINT ( 'NONE',  ( -95.00000000000002842, 87.33691857156074434, 89.32531250086715602 ) ) ;
#49392 = CIRCLE ( 'NONE', #32590, 77.49899999999998101 ) ;
#49393 = VERTEX_POINT ( 'NONE', #11411 ) ;
#49394 =( REPRESENTATION_RELATIONSHIP ('NONE','NONE', #31117, #23457 ) REPRESENTATION_RELATIONSHIP_WITH_TRANSFORMATION ( #4938 )SHAPE_REPRESENTATION_RELATIONSHIP( ) );
#49396 = CARTESIAN_POINT ( 'NONE',  ( -96.15314808468752972, 91.99731107132950569, 86.99697916753380866 ) ) ;
#49395 = CARTESIAN_POINT ( 'NONE',  ( 93.84685191531248449, 88.00268892867053694, 89.11364583420048291 ) ) ;
#49397 = ORIENTED_EDGE ( 'NONE', *, *, #33768, .T. ) ;
#49398 = FACE_OUTER_BOUND ( 'NONE', #50380, .T. ) ;
#49399 = CARTESIAN_POINT ( 'NONE',  ( 10.00000000000000000, -62.50884508063453637, 41.76106447765467777 ) ) ;
#49400 = CARTESIAN_POINT ( 'NONE',  ( -94.99999999999997158, -209.9999999999999716, 90.00000000000000000 ) ) ;
#49401 = DIRECTION ( 'NONE',  ( 0.000000000000000000, 0.3090169943749580539, -0.9510565162951500895 ) ) ;
#49402 = LINE ( 'NONE', #73054, #61479 ) ;
#49403 = CARTESIAN_POINT ( 'NONE',  ( 10.00000000000000000, 36.88895765772642932, -6.736453364083163642 ) ) ;
#49404 = CARTESIAN_POINT ( 'NONE',  ( 0.000000000000000000, 41.76937507738875155, -62.50329211542393892 ) ) ;
#49405 = CIRCLE ( 'NONE', #29002, 32.00000000000000000 ) ;
#49406 = DIRECTION ( 'NONE',  ( 0.000000000000000000, 0.000000000000000000, -1.000000000000000000 ) ) ;
#49407 = ORIENTED_EDGE ( 'NONE', *, *, #9855, .T. ) ;
#49408 = VERTEX_POINT ( 'NONE', #34344 ) ;
#49409 = AXIS2_PLACEMENT_3D ( 'NONE', #53596, #47223, #1768 ) ;
#49410 = EDGE_CURVE ( 'NONE', #23556, #2800, #40360, .T. ) ;
#49411 = CARTESIAN_POINT ( 'NONE',  ( -95.00000000000002842, 86.94004357329504273, 79.99874999999998693 ) ) ;
#49412 = DIRECTION ( 'NONE',  ( -1.000000000000000000, -0.000000000000000000, -0.000000000000000000 ) ) ;
#49413 = DIRECTION ( 'NONE',  ( -0.000000000000000000, -0.000000000000000000, -1.000000000000000000 ) ) ;
#49414 = DIRECTION ( 'NONE',  ( 1.000000000000000000, 0.000000000000000000, 0.000000000000000000 ) ) ;
#49415 = CARTESIAN_POINT ( 'NONE',  ( 12.69589495141918611, -96.69089767102708777, -5.500000000000000000 ) ) ;
#49416 = CARTESIAN_POINT ( 'NONE',  ( -97.65000000000003411, 90.00001272927832474, 76.10937456147250657 ) ) ;
#49417 = DIRECTION ( 'NONE',  ( 0.000000000000000000, 0.000000000000000000, 1.000000000000000000 ) ) ;
#49418 = ORIENTED_EDGE ( 'NONE', *, *, #11159, .F. ) ;
#49419 = CARTESIAN_POINT ( 'NONE',  ( -97.30629616937501680, 88.66845928578038638, 82.07572916753380809 ) ) ;
#49420 = FACE_OUTER_BOUND ( 'NONE', #16913, .T. ) ;
#49421 = ADVANCED_FACE ( 'NONE', ( #11766 ), #5797, .T. ) ;
#49422 = EDGE_CURVE ( 'NONE', #43013, #55201, #12317, .T. ) ;
#49423 = DIRECTION ( 'NONE',  ( 1.000000000000000000, 0.000000000000000000, 0.000000000000000000 ) ) ;
#49424 = LINE ( 'NONE', #71228, #6987 ) ;
#49425 = CARTESIAN_POINT ( 'NONE',  ( 4.999999999999999112, -41.91543099594816368, -2.663952781846588014 ) ) ;
#49426 = CARTESIAN_POINT ( 'NONE',  ( 10.00000000000000000, 73.95703589263975175, 23.16143007188454206 ) ) ;
#49427 = CARTESIAN_POINT ( 'NONE',  ( 97.65000000000000568, -208.4700217866474645, 80.28979166840095161 ) ) ;
#49428 = DIRECTION ( 'NONE',  ( 0.000000000000000000, 0.000000000000000000, 1.000000000000000000 ) ) ;
#49429 = DIRECTION ( 'NONE',  ( -1.000000000000000000, 0.000000000000000000, 0.000000000000000000 ) ) ;
#49430 = CARTESIAN_POINT ( 'NONE',  ( 92.69370383062498320, 88.66845928578035796, 79.05947916753382287 ) ) ;
#49431 = CARTESIAN_POINT ( 'NONE',  ( -93.84685191531248449, -208.0026889286704943, 83.87489583420048689 ) ) ;
#49432 = DIRECTION ( 'NONE',  ( 1.000000000000000000, -0.000000000000000000, -0.000000000000000000 ) ) ;
#49433 = ORIENTED_EDGE ( 'NONE', *, *, #59076, .T. ) ;
#49434 =( GEOMETRIC_REPRESENTATION_CONTEXT ( 3 ) GLOBAL_UNCERTAINTY_ASSIGNED_CONTEXT ( ( #27138 ) ) GLOBAL_UNIT_ASSIGNED_CONTEXT ( ( #37042, #8475, #42594 ) ) REPRESENTATION_CONTEXT ( 'NONE', 'WORKASPACE' ) );
#49435 = CARTESIAN_POINT ( 'NONE',  ( 0.000000000000000000, 0.000000000000000000, -80.00000000000000000 ) ) ;
#49436 = AXIS2_PLACEMENT_3D ( 'NONE', #36092, #47739, #25547 ) ;
#49437 = CARTESIAN_POINT ( 'NONE',  ( -92.34999999999999432, -209.9999999999999716, 76.98250000000000171 ) ) ;
#49438 = DIRECTION ( 'NONE',  ( 0.000000000000000000, -0.8910065241883626808, -0.4539904997395569075 ) ) ;
#49439 = CIRCLE ( 'NONE', #27807, 77.49900000000000944 ) ;
#49440 = CARTESIAN_POINT ( 'NONE',  ( 96.15314808468750130, -211.9973110713294489, 84.77447916753381207 ) ) ;
#49441 = ORIENTED_EDGE ( 'NONE', *, *, #31473, .F. ) ;
#49442 = AXIS2_PLACEMENT_3D ( 'NONE', #59042, #36827, #71035 ) ;
#49443 = DIRECTION ( 'NONE',  ( -1.000000000000000000, -0.000000000000000000, -0.000000000000000000 ) ) ;
#49444 = ORIENTED_EDGE ( 'NONE', *, *, #42018, .T. ) ;
#49445 = CIRCLE ( 'NONE', #71058, 82.00000000000000000 ) ;
#49446 =( BOUNDED_CURVE ( )  B_SPLINE_CURVE ( 2, ( #44674, #33357, #9321, #55193, #20974, #56317, #3717 ),
 .UNSPECIFIED., .F., .F. ) 
 B_SPLINE_CURVE_WITH_KNOTS ( ( 3, 2, 2, 3 ),
 ( 0.1250000000000002220, 0.1319444444444446418, 0.1388888888888890338, 0.1458333333333334536 ),
 .UNSPECIFIED. ) 
 CURVE ( )  GEOMETRIC_REPRESENTATION_ITEM ( )  RATIONAL_B_SPLINE_CURVE ( ( 0.9999999999999956701, 0.8660254037844430375, 1.000000000000000000, 0.8660254037844387076, 1.000000000000000000, 0.8660254037844365982, 1.000000000000002220 ) ) 
 REPRESENTATION_ITEM ( '' )  );
#49447 = CARTESIAN_POINT ( 'NONE',  ( -3.000000000000000000, 20.85821328998741109, 10.92862929874522315 ) ) ;
#49448 = VERTEX_POINT ( 'NONE', #57663 ) ;
#49449 = VECTOR ( 'NONE', #72234, 1000.000000000000000 ) ;
#49450 = LINE ( 'NONE', #43089, #2340 ) ;
#49451 = AXIS2_PLACEMENT_3D ( 'NONE', #17493, #40421, #16004 ) ;
#49452 = VECTOR ( 'NONE', #30565, 1000.000000000000000 ) ;
#49453 = CARTESIAN_POINT ( 'NONE',  ( 92.69370383062501162, -208.6684592857803295, 77.04864583420048518 ) ) ;
#49454 = CARTESIAN_POINT ( 'NONE',  ( -94.99999999999997158, -209.9999999999999716, 90.00000000000000000 ) ) ;
#49455 = FACE_OUTER_BOUND ( 'NONE', #23255, .T. ) ;
#49456 = CARTESIAN_POINT ( 'NONE',  ( -0.9515373497862389396, -96.47140937769621871, 5.500000000000000000 ) ) ;
#49457 = CARTESIAN_POINT ( 'NONE',  ( 96.15314808468748708, 88.00268892867053694, 87.47322916753381605 ) ) ;
#49458 = CARTESIAN_POINT ( 'NONE',  ( -97.64999999960629395, 90.00002930740643592, 76.74344264317980446 ) ) ;
#49459 = CARTESIAN_POINT ( 'NONE',  ( 96.32499999999998863, -207.7050326799711968, 82.80333333333332746 ) ) ;
#49460 = EDGE_CURVE ( 'NONE', #41863, #4461, #70292, .T. ) ;
#49461 = ORIENTED_EDGE ( 'NONE', *, *, #35209, .F. ) ;
#49462 = ORIENTED_EDGE ( 'NONE', *, *, #24786, .T. ) ;
#49463 = EDGE_CURVE ( 'NONE', #28195, #16108, #24821, .T. ) ;
#49464 = ORIENTED_EDGE ( 'NONE', *, *, #57955, .F. ) ;
#49465 = EDGE_LOOP ( 'NONE', ( #37194, #35577, #58476, #48629 ) ) ;
#49466 = CARTESIAN_POINT ( 'NONE',  ( 10.00000000000000000, 0.000000000000000000, -2.500000000000000000 ) ) ;
#49467 = CARTESIAN_POINT ( 'NONE',  ( -92.69370383062504004, 90.00000000000004263, 83.76906250086716454 ) ) ;
#49468 = EDGE_CURVE ( 'NONE', #29598, #29474, #1932, .T. ) ;
#49469 = CARTESIAN_POINT ( 'NONE',  ( -92.35000000000005116, 88.47002178664754979, 82.08895833506764461 ) ) ;
#49470 = DIRECTION ( 'NONE',  ( 1.000000000000000000, 0.000000000000000000, 0.000000000000000000 ) ) ;
#49471 = CARTESIAN_POINT ( 'NONE',  ( 2.184357737007946383E-12, -120.0000000000000000, -48.99999999999997158 ) ) ;
#49472 = DIRECTION ( 'NONE',  ( 0.000000000000000000, 0.4539904997395478037, -0.8910065241883673437 ) ) ;
#49474 = VERTEX_POINT ( 'NONE', #71774 ) ;
#49473 = ADVANCED_FACE ( 'NONE', ( #27026 ), #3391, .T. ) ;
#49475 = CARTESIAN_POINT ( 'NONE',  ( -94.99999999999997158, -206.9400435732949575, 87.38062500173430180 ) ) ;
#49476 = ORIENTED_EDGE ( 'NONE', *, *, #67295, .F. ) ;
#49477 = FACE_OUTER_BOUND ( 'NONE', #14990, .T. ) ;
#49478 = ORIENTED_EDGE ( 'NONE', *, *, #22776, .F. ) ;
#49479 = CARTESIAN_POINT ( 'NONE',  ( -95.00000000000002842, 93.05995642670501411, 82.30062500173428930 ) ) ;
#49480 = ADVANCED_FACE ( 'NONE', ( #37953 ), #60166, .T. ) ;
#49481 = VERTEX_POINT ( 'NONE', #48494 ) ;
#49482 = CARTESIAN_POINT ( 'NONE',  ( 93.84685191531248449, 88.00268892867053694, 87.36739583420049371 ) ) ;
#49483 = CARTESIAN_POINT ( 'NONE',  ( 10.00000000000000000, -51.03279382321048985, -55.19960302592120627 ) ) ;
#49484 = DIRECTION ( 'NONE',  ( 0.000000000000000000, 0.000000000000000000, 1.000000000000000000 ) ) ;
#49485 = FACE_OUTER_BOUND ( 'NONE', #43209, .T. ) ;
#49486 = DIRECTION ( 'NONE',  ( -0.000000000000000000, 0.8090169943749504489, -0.5877852522924689183 ) ) ;
#49487 = AXIS2_PLACEMENT_3D ( 'NONE', #39436, #23998, #51821 ) ;
#49488 = DIRECTION ( 'NONE',  ( 0.000000000000000000, -0.8090169943749403458, -0.5877852522924830181 ) ) ;
#49489 = VERTEX_POINT ( 'NONE', #25555 ) ;
#49490 = DIRECTION ( 'NONE',  ( 0.000000000000000000, -0.07845909572783053842, -0.9969173337331290741 ) ) ;
#49491 = VERTEX_POINT ( 'NONE', #49590 ) ;
#49492 = VECTOR ( 'NONE', #63504, 1000.000000000000000 ) ;
#49493 = ORIENTED_EDGE ( 'NONE', *, *, #43810, .F. ) ;
#49494 = EDGE_CURVE ( 'NONE', #12380, #72968, #21920, .T. ) ;
#49495 = AXIS2_PLACEMENT_3D ( 'NONE', #21764, #67632, #66526 ) ;
#49496 = EDGE_CURVE ( 'NONE', #18859, #50834, #61643, .T. ) ;
#49497 = DIRECTION ( 'NONE',  ( 1.000000000000000000, 0.000000000000000000, 0.000000000000000000 ) ) ;
#49498 = CARTESIAN_POINT ( 'NONE',  ( 7.468086116107294004, -12.33868914344945189, 0.000000000000000000 ) ) ;
#49499 = AXIS2_PLACEMENT_3D ( 'NONE', #7046, #25080, #8540 ) ;
#49500 = CARTESIAN_POINT ( 'NONE',  ( -97.30629616937497417, -208.6684592857803011, 85.93864583420048575 ) ) ;
#49501 = ORIENTED_EDGE ( 'NONE', *, *, #67635, .T. ) ;
#49502 = CARTESIAN_POINT ( 'NONE',  ( 0.000000000000000000, 68.27212725128275395, -31.46837873495001503 ) ) ;
#49503 = ORIENTED_EDGE ( 'NONE', *, *, #44994, .T. ) ;
#49504 = CARTESIAN_POINT ( 'NONE',  ( -97.64999999999996305, -209.9999999999999716, 90.00000000000000000 ) ) ;
#49505 = EDGE_CURVE ( 'NONE', #57738, #2902, #3036, .T. ) ;
#49507 = ADVANCED_FACE ( 'NONE', ( #61264 ), #2675, .T. ) ;
#49506 = CIRCLE ( 'NONE', #1579, 77.49899999999999523 ) ;
#49508 = FACE_BOUND ( 'NONE', #57986, .T. ) ;
#49509 = PLANE ( 'NONE',  #11699 ) ;
#49510 = CARTESIAN_POINT ( 'NONE',  ( 94.99999999999998579, 87.33691857156068750, 79.00656250086714749 ) ) ;
#49511 = CARTESIAN_POINT ( 'NONE',  ( 10.00000000000000000, -31.46837873495025306, 68.27212725128265447 ) ) ;
#49512 = DIRECTION ( 'NONE',  ( -0.000000000000000000, -0.000000000000000000, -1.000000000000000000 ) ) ;
#49513 = DIRECTION ( 'NONE',  ( -1.000000000000000000, 0.000000000000000000, -0.000000000000000000 ) ) ;
#49514 = DIRECTION ( 'NONE',  ( -0.000000000000000000, -0.000000000000000000, 1.000000000000000000 ) ) ;
#49515 = FACE_OUTER_BOUND ( 'NONE', #9153, .T. ) ;
#49516 = CARTESIAN_POINT ( 'NONE',  ( -92.34999999999996589, -211.5299782133523934, 87.08958333333333712 ) ) ;
#49517 = CARTESIAN_POINT ( 'NONE',  ( 10.00000000000000000, 68.26794271651262136, 31.47745569255165066 ) ) ;
#49518 = DIRECTION ( 'NONE',  ( -1.000000000000000000, 0.000000000000000000, -0.000000000000000000 ) ) ;
#49519 = ORIENTED_EDGE ( 'NONE', *, *, #51254, .F. ) ;
#49520 = CARTESIAN_POINT ( 'NONE',  ( -97.30629616937501680, 88.66845928578038638, 83.98072916753380923 ) ) ;
#49521 = PLANE ( 'NONE',  #58783 ) ;
#49522 = CARTESIAN_POINT ( 'NONE',  ( 10.00000000000000000, 0.000000000000000000, 0.000000000000000000 ) ) ;
#49523 = ORIENTED_EDGE ( 'NONE', *, *, #71691, .F. ) ;
#49524 = DIRECTION ( 'NONE',  ( 0.000000000000000000, 0.000000000000000000, -1.000000000000000000 ) ) ;
#49525 = DIRECTION ( 'NONE',  ( 0.000000000000000000, 0.000000000000000000, 1.000000000000000000 ) ) ;
#49526 = CARTESIAN_POINT ( 'NONE',  ( -2.459674775249762302, -3.512261536895417911E-15, -1.958521724548552858E-15 ) ) ;
#49527 = EDGE_CURVE ( 'NONE', #10067, #62877, #23223, .T. ) ;
#49528 = COLOUR_RGB ( '', 0.31764706, 0.68627451, 0.89019608) ;
#49529 = DIRECTION ( 'NONE',  ( 0.000000000000000000, -0.07845909572785224328, 0.9969173337331274087 ) ) ;
#49530 = CARTESIAN_POINT ( 'NONE',  ( 97.30629616937498838, -209.9999999999999716, 77.41906250086715602 ) ) ;
#49531 = TOROIDAL_SURFACE ( 'NONE', #23165, 2.699999999999999734, 0.2000000000000000111 ) ;
#49532 = VERTEX_POINT ( 'NONE', #60529 ) ;
#49533 = EDGE_CURVE ( 'NONE', #34583, #8597, #19905, .T. ) ;
#49534 = VERTEX_POINT ( 'NONE', #66171 ) ;
#49535 = EDGE_CURVE ( 'NONE', #1681, #11576, #48425, .T. ) ;
#49536 = AXIS2_PLACEMENT_3D ( 'NONE', #72974, #21480, #38791 ) ;
#49537 = CARTESIAN_POINT ( 'NONE',  ( 22.94323693612312809, -114.6983135802921083, 2.500000000000000000 ) ) ;
#49538 = LINE ( 'NONE', #32613, #37778 ) ;
#49539 = AXIS2_PLACEMENT_3D ( 'NONE', #23944, #46882, #46141 ) ;
#49540 = DIRECTION ( 'NONE',  ( -1.000000000000000000, 0.000000000000000000, 0.000000000000000000 ) ) ;
#49541 = DIRECTION ( 'NONE',  ( 0.000000000000000000, -0.3090169943749349057, -0.9510565162951576390 ) ) ;
#49542 = FACE_OUTER_BOUND ( 'NONE', #53003, .T. ) ;
#49543 = CARTESIAN_POINT ( 'NONE',  ( 92.69370383062501162, -209.9999999999999716, 76.46656250086715545 ) ) ;
#49544 = EDGE_CURVE ( 'NONE', #45145, #3846, #64008, .T. ) ;
#49545 = ORIENTED_EDGE ( 'NONE', *, *, #42010, .T. ) ;
#49546 = DIRECTION ( 'NONE',  ( 0.000000000000000000, 0.000000000000000000, -1.000000000000000000 ) ) ;
#49547 = ORIENTED_EDGE ( 'NONE', *, *, #31759, .F. ) ;
#49548 = VECTOR ( 'NONE', #38881, 1000.000000000000000 ) ;
#49549 = ORIENTED_EDGE ( 'NONE', *, *, #44734, .F. ) ;
#49550 = CARTESIAN_POINT ( 'NONE',  ( -97.64999999960633659, -209.9999706968024782, 82.45844277047601167 ) ) ;
#49551 = VECTOR ( 'NONE', #826, 1000.000000000000000 ) ;
#49552 = CARTESIAN_POINT ( 'NONE',  ( -92.35000000000003695, 90.00000000000004263, 89.12687500173430521 ) ) ;
#49553 = ORIENTED_EDGE ( 'NONE', *, *, #19333, .T. ) ;
#49554 = CARTESIAN_POINT ( 'NONE',  ( 0.000000000000000000, -74.65491531819111515, -8.830959090343204920 ) ) ;
#49555 = CARTESIAN_POINT ( 'NONE',  ( 96.32499999999998863, -212.2949673200287179, 81.40104166840096411 ) ) ;
#49556 = CARTESIAN_POINT ( 'NONE',  ( 93.67499999999998295, 92.29496732002878900, 86.71916666666666629 ) ) ;
#49557 = ORIENTED_EDGE ( 'NONE', *, *, #2361, .F. ) ;
#49558 = DIRECTION ( 'NONE',  ( 1.000000000000000000, -0.000000000000000000, -0.000000000000000000 ) ) ;
#49559 = CARTESIAN_POINT ( 'NONE',  ( -92.75110981005065014, -210.5903413996856273, 74.79348190356849102 ) ) ;
#49560 = VERTEX_POINT ( 'NONE', #14272 ) ;
#49561 = DIRECTION ( 'NONE',  ( -1.000000000000000000, -0.000000000000000000, 0.000000000000000000 ) ) ;
#49562 = CARTESIAN_POINT ( 'NONE',  ( -96.15314808468752972, 91.99731107132950569, 83.98072916753382344 ) ) ;
#49563 = EDGE_CURVE ( 'NONE', #53104, #64725, #58670, .T. ) ;
#49564 = CARTESIAN_POINT ( 'NONE',  ( 97.30629616937498838, 88.66845928578037217, 81.01739583420048518 ) ) ;
#49565 = EDGE_LOOP ( 'NONE', ( #17465, #68627, #60187, #10190 ) ) ;
#49566 = LINE ( 'NONE', #72494, #38443 ) ;
#49567 = ORIENTED_EDGE ( 'NONE', *, *, #22227, .F. ) ;
#49568 = DIRECTION ( 'NONE',  ( -1.000000000000000000, 0.000000000000000000, 0.000000000000000000 ) ) ;
#49569 = VERTEX_POINT ( 'NONE', #36834 ) ;
#49570 = VERTEX_POINT ( 'NONE', #37592 ) ;
#49571 = ADVANCED_FACE ( 'NONE', ( #59782 ), #14644, .F. ) ;
#49572 = VERTEX_POINT ( 'NONE', #26290 ) ;
#49573 = ADVANCED_FACE ( 'NONE', ( #49225 ), #72153, .F. ) ;
#49574 = CARTESIAN_POINT ( 'NONE',  ( -93.67499999999998295, -207.7050326799711968, 80.97770833506763211 ) ) ;
#49575 = CARTESIAN_POINT ( 'NONE',  ( 97.64999999999997726, 88.47002178664753558, 89.07395833506762983 ) ) ;
#49576 = EDGE_LOOP ( 'NONE', ( #11268, #58, #17693, #59023 ) ) ;
#49577 = CARTESIAN_POINT ( 'NONE',  ( 95.00000000000000000, -209.9999999999999716, 90.00000000000000000 ) ) ;
#49578 = CARTESIAN_POINT ( 'NONE',  ( -96.15314808468747287, -208.0026889286704943, 78.10697916753380809 ) ) ;
#49579 = ORIENTED_EDGE ( 'NONE', *, *, #54807, .F. ) ;
#49580 = EDGE_CURVE ( 'NONE', #38969, #69628, #40447, .T. ) ;
#49581 = DIRECTION ( 'NONE',  ( -1.000000000000000000, -0.000000000000000000, 0.000000000000000000 ) ) ;
#49582 = CYLINDRICAL_SURFACE ( 'NONE', #46444, 26.50000000000000355 ) ;
#49583 = CARTESIAN_POINT ( 'NONE',  ( -10.00000000000000000, 0.000000000000000000, 0.000000000000000000 ) ) ;
#49584 = CYLINDRICAL_SURFACE ( 'NONE', #49495, 31.99999999999998579 ) ;
#49585 =( GEOMETRIC_REPRESENTATION_CONTEXT ( 3 ) GLOBAL_UNCERTAINTY_ASSIGNED_CONTEXT ( ( #19734 ) ) GLOBAL_UNIT_ASSIGNED_CONTEXT ( ( #49739, #9535, #11017 ) ) REPRESENTATION_CONTEXT ( 'NONE', 'WORKASPACE' ) );
#49586 = DIRECTION ( 'NONE',  ( -1.000000000000000000, -0.000000000000000000, -0.000000000000000000 ) ) ;
#49587 = AXIS2_PLACEMENT_3D ( 'NONE', #3343, #31505, #53706 ) ;
#49588 = CARTESIAN_POINT ( 'NONE',  ( 15.00000000000000000, 23.49999999999999645, -1.500000000000003997 ) ) ;
#49589 = CARTESIAN_POINT ( 'NONE',  ( 94.99999999999998579, 87.33691857156068750, 89.16656250086712987 ) ) ;
#49590 = CARTESIAN_POINT ( 'NONE',  ( -2.500000000000015543, -73.00000000000001421, -258.2999999999999545 ) ) ;
#49591 = DIRECTION ( 'NONE',  ( 1.000000000000000000, -3.061616997868382648E-16, -0.000000000000000000 ) ) ;
#49592 = CARTESIAN_POINT ( 'NONE',  ( -92.35000000000003695, 90.00000000000004263, 87.14249999999999829 ) ) ;
#49593 = DIRECTION ( 'NONE',  ( -1.000000000000000000, 0.000000000000000000, 0.000000000000000000 ) ) ;
#49594 = CARTESIAN_POINT ( 'NONE',  ( 0.000000000000000000, 0.000000000000000000, 0.000000000000000000 ) ) ;
#49595 = CARTESIAN_POINT ( 'NONE',  ( -10.00000000000000000, 0.000000000000000000, 0.000000000000000000 ) ) ;
#49596 = AXIS2_PLACEMENT_3D ( 'NONE', #37457, #20880, #26145 ) ;
#49597 = DIRECTION ( 'NONE',  ( -1.000000000000000000, -0.000000000000000000, -0.000000000000000000 ) ) ;
#49598 = DIRECTION ( 'NONE',  ( -0.000000000000000000, -0.000000000000000000, 1.000000000000000000 ) ) ;
#49599 = AXIS2_PLACEMENT_3D ( 'NONE', #55241, #38324, #9751 ) ;
#49600 = CARTESIAN_POINT ( 'NONE',  ( 10.00000000000000000, -37.22597642581153821, -5.202137450156795850 ) ) ;
#49601 = AXIS2_PLACEMENT_3D ( 'NONE', #45186, #68107, #106 ) ;
#49602 = AXIS2_PLACEMENT_3D ( 'NONE', #6710, #36013, #59321 ) ;
#49603 = DIRECTION ( 'NONE',  ( -1.000000000000000000, 0.000000000000000000, 0.000000000000000000 ) ) ;
#49604 = CARTESIAN_POINT ( 'NONE',  ( -94.99999999999997158, -213.0599564267049857, 83.17374999999999829 ) ) ;
#49605 = ADVANCED_FACE ( 'NONE', ( #33796 ), #11, .T. ) ;
#49606 = DIRECTION ( 'NONE',  ( 0.000000000000000000, 0.8090169943749445647, 0.5877852522924770229 ) ) ;
#49607 = CARTESIAN_POINT ( 'NONE',  ( 50.00005079999999680, 0.000000000000000000, 12.50000000000000000 ) ) ;
#49608 = DIRECTION ( 'NONE',  ( 1.000000000000000000, -0.000000000000000000, 0.000000000000000000 ) ) ;
#49609 = CARTESIAN_POINT ( 'NONE',  ( 10.00000000000000000, -21.32104025579091910, -30.84782396557241313 ) ) ;
#49610 = ORIENTED_EDGE ( 'NONE', *, *, #39404, .T. ) ;
#49611 = EDGE_CURVE ( 'NONE', #36383, #30790, #16886, .T. ) ;
#49612 = ORIENTED_EDGE ( 'NONE', *, *, #39381, .F. ) ;
#49614 = ADVANCED_FACE ( 'NONE', ( #51829 ), #55981, .T. ) ;
#49613 = DIRECTION ( 'NONE',  ( -1.000000000000000000, -0.000000000000000000, -0.000000000000000000 ) ) ;
#49615 = CARTESIAN_POINT ( 'NONE',  ( 10.00000000000000000, 0.000000000000000000, 0.000000000000000000 ) ) ;
#49616 = ORIENTED_EDGE ( 'NONE', *, *, #59501, .F. ) ;
#49617 = AXIS2_PLACEMENT_3D ( 'NONE', #21683, #9667, #32588 ) ;
#49618 = CARTESIAN_POINT ( 'NONE',  ( 92.69370383062501162, -208.6684592857803295, 80.69989583420046131 ) ) ;
#49619 = CARTESIAN_POINT ( 'NONE',  ( 97.30629616937498838, -208.6684592857803295, 84.45697916753383083 ) ) ;
#49620 = VERTEX_POINT ( 'NONE', #22525 ) ;
#49621 = CARTESIAN_POINT ( 'NONE',  ( 96.15314808468750130, -211.9973110713294489, 84.93322916753382401 ) ) ;
#49622 = ADVANCED_FACE ( 'NONE', ( #67271 ), #68011, .T. ) ;
#49623 = VERTEX_POINT ( 'NONE', #43809 ) ;
#49624 = EDGE_CURVE ( 'NONE', #58686, #60033, #73633, .T. ) ;
#49625 = ORIENTED_EDGE ( 'NONE', *, *, #34310, .F. ) ;
#49626 = DIRECTION ( 'NONE',  ( -1.000000000000000000, 0.000000000000000000, 0.000000000000000000 ) ) ;
#49627 = ORIENTED_EDGE ( 'NONE', *, *, #63676, .T. ) ;
#49628 = CARTESIAN_POINT ( 'NONE',  ( -95.00000000000002842, 92.66308142843932671, 78.21281250086717307 ) ) ;
#49629 = EDGE_LOOP ( 'NONE', ( #13790, #15083, #69616, #72853 ) ) ;
#49630 = VERTEX_POINT ( 'NONE', #62389 ) ;
#49631 = CARTESIAN_POINT ( 'NONE',  ( 16.84844760790522855, -103.5491698323862124, 5.500000000000000000 ) ) ;
#49632 = ORIENTED_EDGE ( 'NONE', *, *, #31831, .T. ) ;
#49633 = CARTESIAN_POINT ( 'NONE',  ( 10.00000000000000000, 39.78640506895700213, -66.50666863321957578 ) ) ;
#49634 = CARTESIAN_POINT ( 'NONE',  ( 97.64999999999997726, -208.4700217866474645, 89.17979166840096639 ) ) ;
#49635 = ORIENTED_EDGE ( 'NONE', *, *, #5700, .T. ) ;
#49636 = CARTESIAN_POINT ( 'NONE',  ( 94.99999999999998579, 90.00000000000002842, 90.00000000000000000 ) ) ;
#49637 = CIRCLE ( 'NONE', #40062, 16.00000000000000355 ) ;
#49638 = EDGE_LOOP ( 'NONE', ( #5924, #27746, #57800, #27630 ) ) ;
#49639 =( BOUNDED_CURVE ( )  B_SPLINE_CURVE ( 2, ( #15654, #32921, #21653, #68274, #16390, #67523, #44608, #61894, #62267 ),
 .UNSPECIFIED., .F., .F. ) 
 B_SPLINE_CURVE_WITH_KNOTS ( ( 3, 2, 2, 2, 3 ),
 ( 0.4445132602993024373, 0.4515689946186892123, 0.4586247601596063483, 0.4656805257005234844, 0.4656806970079900854 ),
 .UNSPECIFIED. ) 
 CURVE ( )  GEOMETRIC_REPRESENTATION_ITEM ( )  RATIONAL_B_SPLINE_CURVE ( ( 0.9999988143388863771, 0.8660259966176188096, 1.000000000000000000, 0.8660254037844387076, 1.000000000000000000, 0.8660254037844387076, 1.000000000000000000, 0.9999967472206192642, 0.9999934945991874047 ) ) 
 REPRESENTATION_ITEM ( '' )  );
#49640 = DIRECTION ( 'NONE',  ( 0.000000000000000000, 0.000000000000000000, 1.000000000000000000 ) ) ;
#49641 = CIRCLE ( 'NONE', #47248, 16.00000000000000000 ) ;
#49642 = EDGE_CURVE ( 'NONE', #3543, #24664, #1626, .T. ) ;
#49643 = ORIENTED_EDGE ( 'NONE', *, *, #13291, .F. ) ;
#49644 = ORIENTED_EDGE ( 'NONE', *, *, #2417, .T. ) ;
#49645 = CIRCLE ( 'NONE', #44845, 82.00000000000000000 ) ;
#49646 = ORIENTED_EDGE ( 'NONE', *, *, #9693, .F. ) ;
#49647 = CARTESIAN_POINT ( 'NONE',  ( 95.00000000000000000, -207.3369185715606307, 76.14906250086716000 ) ) ;
#49648 = AXIS2_PLACEMENT_3D ( 'NONE', #68678, #73182, #45381 ) ;
#49649 = CARTESIAN_POINT ( 'NONE',  ( -2.499999999999965361, 90.00000000000000000, -310.0000000000000000 ) ) ;
#49650 = ORIENTED_EDGE ( 'NONE', *, *, #45722, .T. ) ;
#49651 = ORIENTED_EDGE ( 'NONE', *, *, #54481, .T. ) ;
#49652 = ORIENTED_EDGE ( 'NONE', *, *, #55174, .T. ) ;
#49653 = CARTESIAN_POINT ( 'NONE',  ( 0.000000000000000000, 77.32052557432849937, -5.256550761632002633 ) ) ;
#49654 = LINE ( 'NONE', #9074, #68330 ) ;
#49655 = CARTESIAN_POINT ( 'NONE',  ( -94.53673242685063371, 87.15692181550789996, 74.72378867588408013 ) ) ;
#49656 = ADVANCED_FACE ( 'NONE', ( #21770 ), #4027, .T. ) ;
#49657 = ADVANCED_FACE ( 'NONE', ( #56369 ), #11234, .F. ) ;
#49658 = VERTEX_POINT ( 'NONE', #16135 ) ;
#49659 = EDGE_CURVE ( 'NONE', #11006, #55103, #45091, .T. ) ;
#49660 = CARTESIAN_POINT ( 'NONE',  ( 94.99999999999998579, 87.33691857156068750, 79.00656250086713328 ) ) ;
#49661 = ORIENTED_EDGE ( 'NONE', *, *, #57531, .T. ) ;
#49662 = DIRECTION ( 'NONE',  ( 0.000000000000000000, -0.5877852522924625900, -0.8090169943749551118 ) ) ;
#49663 = DIRECTION ( 'NONE',  ( 0.000000000000000000, 0.000000000000000000, 1.000000000000000000 ) ) ;
#49664 = DIRECTION ( 'NONE',  ( -0.9580045777625452175, -0.2867529058022035837, 0.000000000000000000 ) ) ;
#49665 = DIRECTION ( 'NONE',  ( -1.000000000000000000, 0.000000000000000000, 0.000000000000000000 ) ) ;
#49666 = CARTESIAN_POINT ( 'NONE',  ( 0.000000000000000000, -40.68715046381921496, -10.41901085202121280 ) ) ;
#49667 = CARTESIAN_POINT ( 'NONE',  ( -96.15314808468745866, -211.9973110713294489, 78.95364583420047211 ) ) ;
#49668 = AXIS2_PLACEMENT_3D ( 'NONE', #39968, #40328, #40706 ) ;
#49669 = DIRECTION ( 'NONE',  ( -1.000000000000000000, 0.000000000000000000, -0.000000000000000000 ) ) ;
#49670 = CARTESIAN_POINT ( 'NONE',  ( 2.500000000000015987, -65.00000000000000000, -90.00000000000000000 ) ) ;
#49671 = DIRECTION ( 'NONE',  ( -0.000000000000000000, -0.000000000000000000, -1.000000000000000000 ) ) ;
#49672 = ORIENTED_EDGE ( 'NONE', *, *, #62121, .F. ) ;
#49673 = ORIENTED_EDGE ( 'NONE', *, *, #19113, .T. ) ;
#49674 = DIRECTION ( 'NONE',  ( -1.000000000000000000, 0.000000000000000000, 0.000000000000000000 ) ) ;
#49675 = CARTESIAN_POINT ( 'NONE',  ( -93.67499999999998295, -212.2949673200287179, 88.94166666666666288 ) ) ;
#49676 = DIRECTION ( 'NONE',  ( -1.000000000000000000, 0.000000000000000000, 0.000000000000000000 ) ) ;
#49677 = CARTESIAN_POINT ( 'NONE',  ( -97.30629616937501680, 88.66845928578038638, 81.44072916753381719 ) ) ;
#49678 = CARTESIAN_POINT ( 'NONE',  ( 11.99999999999999822, -81.34940948281344220, 10.30890764327355491 ) ) ;
#49679 = DIRECTION ( 'NONE',  ( -0.000000000000000000, 0.000000000000000000, 1.000000000000000000 ) ) ;
#49680 = AXIS2_PLACEMENT_3D ( 'NONE', #9943, #20854, #66726 ) ;
#49681 = ORIENTED_EDGE ( 'NONE', *, *, #36001, .F. ) ;
#49682 = DIRECTION ( 'NONE',  ( 1.000000000000000000, 0.000000000000000000, 0.000000000000000000 ) ) ;
#49683 = DIRECTION ( 'NONE',  ( 1.000000000000000000, -0.000000000000000000, -0.000000000000000000 ) ) ;
#49684 = CARTESIAN_POINT ( 'NONE',  ( -7.500000000000015987, -76.30000000000001137, -204.9999999999999716 ) ) ;
#49685 = AXIS2_PLACEMENT_3D ( 'NONE', #18847, #24867, #53807 ) ;
#49686 = DIRECTION ( 'NONE',  ( -1.000000000000000000, -0.000000000000000000, -0.000000000000000000 ) ) ;
#49687 = CARTESIAN_POINT ( 'NONE',  ( 97.64999999999999147, -209.9999999999999716, 88.49187500173430010 ) ) ;
#49688 = CARTESIAN_POINT ( 'NONE',  ( -92.69370383062498320, -209.9999999999999716, 84.40406250086715545 ) ) ;
#49689 = CARTESIAN_POINT ( 'NONE',  ( 11.99999999999999822, 14.66109333815564852, -73.73191006444555740 ) ) ;
#49690 = EDGE_CURVE ( 'NONE', #53859, #64729, #10872, .T. ) ;
#49691 = AXIS2_PLACEMENT_3D ( 'NONE', #63094, #33750, #63450 ) ;
#49692 = EDGE_LOOP ( 'NONE', ( #38540, #63256, #14619, #53802 ) ) ;
#49693 = AXIS2_PLACEMENT_3D ( 'NONE', #20768, #31309, #49341 ) ;
#49694 = CYLINDRICAL_SURFACE ( 'NONE', #27449, 31.99999999999998579 ) ;
#49695 = EDGE_CURVE ( 'NONE', #15962, #57613, #11589, .T. ) ;
#49696 = DIRECTION ( 'NONE',  ( -1.000000000000000000, 0.000000000000000000, -0.000000000000000000 ) ) ;
#49697 = LINE ( 'NONE', #60278, #68214 ) ;
#49698 = VERTEX_POINT ( 'NONE', #39072 ) ;
#49699 = LINE ( 'NONE', #26770, #61743 ) ;
#49700 = LINE ( 'NONE', #31310, #2330 ) ;
#49701 = FACE_OUTER_BOUND ( 'NONE', #19592, .T. ) ;
#49702 = CIRCLE ( 'NONE', #48490, 16.00000000000000355 ) ;
#49703 = EDGE_CURVE ( 'NONE', #19511, #45782, #45841, .T. ) ;
#49704 = EDGE_CURVE ( 'NONE', #11557, #15750, #53217, .T. ) ;
#49705 = FACE_OUTER_BOUND ( 'NONE', #6998, .T. ) ;
#49706 = EDGE_LOOP ( 'NONE', ( #18217, #42155, #63920, #21916 ) ) ;
#49707 = DIRECTION ( 'NONE',  ( 1.000000000000000000, -0.000000000000000000, 0.000000000000000000 ) ) ;
#49708 = PRESENTATION_STYLE_ASSIGNMENT (( #3152 ) ) ;
#49709 = ORIENTED_EDGE ( 'NONE', *, *, #7381, .T. ) ;
#49710 = B_SPLINE_CURVE_WITH_KNOTS ( 'NONE', 3,
 ( #67183, #55534, #42773, #65706, #55902, #14186, #60443, #37139, #60083, #21296, #66813, #20194, #66090, #9288, #9666, #8561, #49146, #2950, #10031, #25841, #72071, #15682, #38616, #44254 ),
 .UNSPECIFIED., .F., .F.,
 ( 4, 2, 2, 2, 2, 2, 2, 2, 2, 2, 2, 4 ),
 ( -0.009991285186810239943, -0.009254074022779373160, -0.008516862858748506376, -0.007779651694717638725, -0.007411046112702206201, -0.007042440530686772809, -0.006673834948671339418, -0.006305229366655907761, -0.005568018202625041845, -0.004830807038594175928, -0.004462201456578743404, -0.004093595874563310012 ),
 .UNSPECIFIED. ) ;
#49711 = CYLINDRICAL_SURFACE ( 'NONE', #64054, 31.99999999999999289 ) ;
#49712 = DIRECTION ( 'NONE',  ( -1.000000000000000000, -0.000000000000000000, 0.000000000000000000 ) ) ;
#49713 = ORIENTED_EDGE ( 'NONE', *, *, #67200, .T. ) ;
#49714 = CIRCLE ( 'NONE', #67720, 31.99999999999998579 ) ;
#49715 = FACE_OUTER_BOUND ( 'NONE', #68991, .T. ) ;
#49716 = EDGE_CURVE ( 'NONE', #71746, #48302, #65925, .T. ) ;
#49717 = ORIENTED_EDGE ( 'NONE', *, *, #27544, .F. ) ;
#49718 = DIRECTION ( 'NONE',  ( -1.000000000000000000, -0.000000000000000000, -0.000000000000000000 ) ) ;
#49719 = ORIENTED_EDGE ( 'NONE', *, *, #54555, .T. ) ;
#49720 = ORIENTED_EDGE ( 'NONE', *, *, #25857, .F. ) ;
#49721 = ORIENTED_EDGE ( 'NONE', *, *, #21023, .T. ) ;
#49722 = DIRECTION ( 'NONE',  ( -0.000000000000000000, -0.000000000000000000, -1.000000000000000000 ) ) ;
#49723 = ORIENTED_EDGE ( 'NONE', *, *, #30784, .F. ) ;
#49724 = CIRCLE ( 'NONE', #34129, 42.00000000000000000 ) ;
#49725 = EDGE_CURVE ( 'NONE', #29672, #59759, #1113, .T. ) ;
#49726 = ORIENTED_EDGE ( 'NONE', *, *, #9534, .F. ) ;
#49727 = CARTESIAN_POINT ( 'NONE',  ( 93.84685191531248449, 88.00268892867053694, 75.30239583420048177 ) ) ;
#49728 = DIRECTION ( 'NONE',  ( 1.427937372958396981E-15, -1.000000000000000000, 1.065814103640131031E-14 ) ) ;
#49729 = EDGE_CURVE ( 'NONE', #33851, #18122, #68846, .T. ) ;
#49730 = CARTESIAN_POINT ( 'NONE',  ( -12.00000000000000000, 17.30399999999999849, 0.000000000000000000 ) ) ;
#49731 = ORIENTED_EDGE ( 'NONE', *, *, #74116, .T. ) ;
#49732 = ORIENTED_EDGE ( 'NONE', *, *, #30687, .T. ) ;
#49733 = ORIENTED_EDGE ( 'NONE', *, *, #35168, .T. ) ;
#49734 = CARTESIAN_POINT ( 'NONE',  ( 96.15314808468748708, 88.00268892867053694, 88.58447916753381435 ) ) ;
#49736 = EDGE_LOOP ( 'NONE', ( #26475, #37292, #36784, #40698 ) ) ;
#49735 = ADVANCED_FACE ( 'NONE', ( #47661 ), #6707, .T. ) ;
#49737 = CARTESIAN_POINT ( 'NONE',  ( 95.00000000000000000, -207.3369185715606307, 86.94406250086714749 ) ) ;
#49738 = VECTOR ( 'NONE', #18669, 1000.000000000000000 ) ;
#49739 =( LENGTH_UNIT ( ) NAMED_UNIT ( * ) SI_UNIT ( .MILLI., .METRE. ) );
#49740 = LINE ( 'NONE', #15915, #52336 ) ;
#49741 = CARTESIAN_POINT ( 'NONE',  ( 95.00000000002597744, 90.00000000000007105, -65.00000000000000000 ) ) ;
#49742 = CYLINDRICAL_SURFACE ( 'NONE', #8896, 31.99999999999999289 ) ;
#49743 = CARTESIAN_POINT ( 'NONE',  ( 97.64999999989933599, 90.00002309722570715, 83.41187580057898288 ) ) ;
#49744 = DIRECTION ( 'NONE',  ( -0.000000000000000000, 1.000000000000000000, 1.224646799147353207E-16 ) ) ;
#49745 = DIRECTION ( 'NONE',  ( -2.628368902995164490E-16, -1.000000000000000000, 0.000000000000000000 ) ) ;
#49746 = CARTESIAN_POINT ( 'NONE',  ( -97.64999999999994884, -211.5299782133524502, 77.43229166840096411 ) ) ;
#49747 = CARTESIAN_POINT ( 'NONE',  ( -97.30629616937501680, 88.66845928578038638, 89.21947916753381946 ) ) ;
#49748 = EDGE_CURVE ( 'NONE', #68450, #60009, #40022, .T. ) ;
#49749 = ORIENTED_EDGE ( 'NONE', *, *, #22081, .T. ) ;
#49751 = CARTESIAN_POINT ( 'NONE',  ( -95.00000000000002842, 92.66308142843932671, 89.48406250086713953 ) ) ;
#49750 = CARTESIAN_POINT ( 'NONE',  ( 97.30629616937498838, 90.00000000000002842, 88.69031250086715090 ) ) ;
#49752 = AXIS2_PLACEMENT_3D ( 'NONE', #36706, #7408, #70166 ) ;
#49753 = ORIENTED_EDGE ( 'NONE', *, *, #55605, .F. ) ;
#49754 = CARTESIAN_POINT ( 'NONE',  ( 0.000000000000000000, 0.000000000000000000, 0.000000000000000000 ) ) ;
#49755 = AXIS2_PLACEMENT_3D ( 'NONE', #41399, #40665, #7191 ) ;
#49756 = DIRECTION ( 'NONE',  ( 0.000000000000000000, 0.000000000000000000, 1.000000000000000000 ) ) ;
#49757 = LINE ( 'NONE', #55785, #70346 ) ;
#49758 = CARTESIAN_POINT ( 'NONE',  ( 10.00000000000000000, 10.30890764327502573, -81.34940948281324324 ) ) ;
#49759 = CARTESIAN_POINT ( 'NONE',  ( -96.15314808468747287, -208.0026889286704943, 89.53697916753381492 ) ) ;
#49760 = ADVANCED_FACE ( 'NONE', ( #58958 ), #59317, .T. ) ;
#49761 = CARTESIAN_POINT ( 'NONE',  ( 10.00000000000000000, 33.79645857604513992, 16.45098606841138178 ) ) ;
#49763 = CARTESIAN_POINT ( 'NONE',  ( -1.084202172485504434E-14, -5.773502691896260863, -2.080000000000000071 ) ) ;
#49762 = CIRCLE ( 'NONE', #14771, 77.49900000000000944 ) ;
#49764 = AXIS2_PLACEMENT_3D ( 'NONE', #37054, #49065, #19746 ) ;
#49765 = DIRECTION ( 'NONE',  ( -1.000000000000000000, -0.000000000000000000, -0.000000000000000000 ) ) ;
#49766 = ORIENTED_EDGE ( 'NONE', *, *, #24140, .F. ) ;
#49767 = ORIENTED_EDGE ( 'NONE', *, *, #34115, .F. ) ;
#49768 = VECTOR ( 'NONE', #47755, 1000.000000000000000 ) ;
#49769 = CARTESIAN_POINT ( 'NONE',  ( -96.32500000000001705, 92.29496732002878900, 82.27416666666665890 ) ) ;
#49770 = DIRECTION ( 'NONE',  ( -1.000000000000000000, -0.000000000000000000, -0.000000000000000000 ) ) ;
#49771 = DIRECTION ( 'NONE',  ( 0.000000000000000000, 0.07845909572783797692, 0.9969173337331285190 ) ) ;
#49772 = DIRECTION ( 'NONE',  ( -0.7273375899149802093, 0.6862798483830544471, 0.000000000000000000 ) ) ;
#49773 = AXIS2_PLACEMENT_3D ( 'NONE', #28545, #12006, #45877 ) ;
#49774 = CARTESIAN_POINT ( 'NONE',  ( 0.000000000000000000, 0.000000000000000000, -6.000000000000000000 ) ) ;
#49775 = DIRECTION ( 'NONE',  ( 0.000000000000000000, 0.000000000000000000, 1.000000000000000000 ) ) ;
#49776 = DIRECTION ( 'NONE',  ( 0.000000000000000000, 0.000000000000000000, 1.000000000000000000 ) ) ;
#49777 = ORIENTED_EDGE ( 'NONE', *, *, #28912, .T. ) ;
#49778 = CARTESIAN_POINT ( 'NONE',  ( -92.69370383062502583, 91.33154071421968467, 81.75822916753381264 ) ) ;
#49779 = AXIS2_PLACEMENT_3D ( 'NONE', #31625, #50306, #13602 ) ;
#49780 = CYLINDRICAL_SURFACE ( 'NONE', #61964, 37.49900000000000233 ) ;
#49781 = DIRECTION ( 'NONE',  ( -1.000000000000000000, 0.000000000000000000, -0.000000000000000000 ) ) ;
#49782 =( NAMED_UNIT ( * ) SI_UNIT ( $, .STERADIAN. ) SOLID_ANGLE_UNIT ( ) );
#49783 = PLANE ( 'NONE',  #70510 ) ;
#49784 = CARTESIAN_POINT ( 'NONE',  ( -2.499999999999973355, 65.00000000000000000, -290.0000000000000568 ) ) ;
#49785 = CARTESIAN_POINT ( 'NONE',  ( 93.67500000000001137, -207.7050326799711968, 80.44854166840097776 ) ) ;
#49786 = DIRECTION ( 'NONE',  ( -0.000000000000000000, -0.000000000000000000, 1.000000000000000000 ) ) ;
#49787 = SHAPE_REPRESENTATION ( 'big gear_ISO - Spur gear 2M 80T 20PA 10FW ---S80A75H50L20.0N', ( #43395 ), #56652 ) ;
#49788 = CARTESIAN_POINT ( 'NONE',  ( -3.000000000000000000, -14.54903810567645195, -22.19967320028775504 ) ) ;
#49789 = CARTESIAN_POINT ( 'NONE',  ( 93.84685191531248449, 91.99731107132950569, 82.07572916753382231 ) ) ;
#49790 = CARTESIAN_POINT ( 'NONE',  ( -92.69370383062498320, -209.9999999999999716, 81.86406250086714920 ) ) ;
#49791 = DIRECTION ( 'NONE',  ( 1.000000000000000000, 0.000000000000000000, 0.000000000000000000 ) ) ;
#49792 = VERTEX_POINT ( 'NONE', #1844 ) ;
#49793 = FACE_OUTER_BOUND ( 'NONE', #14624, .T. ) ;
#49794 = CARTESIAN_POINT ( 'NONE',  ( -96.32499999999996021, -207.7050326799711968, 77.82916666666665151 ) ) ;
#49795 = ADVANCED_FACE ( 'NONE', ( #13072 ), #374, .T. ) ;
#49796 = DIRECTION ( 'NONE',  ( -1.000000000000000000, -0.000000000000000000, 0.000000000000000000 ) ) ;
#49797 = AXIS2_PLACEMENT_3D ( 'NONE', #38573, #55488, #27268 ) ;
#49798 = EDGE_CURVE ( 'NONE', #51811, #8967, #50789, .T. ) ;
#49799 = ADVANCED_FACE ( 'NONE', ( #7447 ), #69134, .T. ) ;
#49800 = CARTESIAN_POINT ( 'NONE',  ( -93.84685191531252713, 88.00268892867056536, 76.67822916753381435 ) ) ;
#49801 = CARTESIAN_POINT ( 'NONE',  ( 97.30629616937498838, -211.3315407142195852, 85.46239583420047836 ) ) ;
#49802 = EDGE_LOOP ( 'NONE', ( #69337, #9072 ) ) ;
#49803 = CARTESIAN_POINT ( 'NONE',  ( 97.01450244679210755, 88.86758821614978388, 74.79348190356853365 ) ) ;
#49804 = VERTEX_POINT ( 'NONE', #40547 ) ;
#49805 = CIRCLE ( 'NONE', #20992, 32.00000000000000000 ) ;
#49806 = DIRECTION ( 'NONE',  ( 0.000000000000000000, 0.5877852522924741363, -0.8090169943749465631 ) ) ;
#49807 = VECTOR ( 'NONE', #50769, 1000.000000000000000 ) ;
#49808 = ORIENTED_EDGE ( 'NONE', *, *, #24948, .F. ) ;
#49809 = CARTESIAN_POINT ( 'NONE',  ( 100.0010000000000190, -115.9999999999999716, -40.00000000000002132 ) ) ;
#49810 = AXIS2_PLACEMENT_3D ( 'NONE', #48966, #30934, #38440 ) ;
#49811 = ORIENTED_EDGE ( 'NONE', *, *, #8000, .T. ) ;
#49812 = ORIENTED_EDGE ( 'NONE', *, *, #29283, .F. ) ;
#49813 = AXIS2_PLACEMENT_3D ( 'NONE', #42395, #60800, #30723 ) ;
#49814 = EDGE_CURVE ( 'NONE', #72105, #10184, #26788, .T. ) ;
#49815 = CARTESIAN_POINT ( 'NONE',  ( 97.30629616937498838, -209.9999999999999716, 75.51406250086715488 ) ) ;
#49816 = CARTESIAN_POINT ( 'NONE',  ( 3.000000000000000000, 2.935248768560057897, -3.252606517456513302E-15 ) ) ;
#49817 = CARTESIAN_POINT ( 'NONE',  ( 0.000000000000000000, 68.67312586194995561, 35.91791733033500122 ) ) ;
#49818 = CYLINDRICAL_SURFACE ( 'NONE', #61673, 2.649999999999985700 ) ;
#49819 = CARTESIAN_POINT ( 'NONE',  ( 97.30629616937498838, 91.33154071421968467, 88.26697916753381890 ) ) ;
#49820 = DIRECTION ( 'NONE',  ( 0.000000000000000000, -0.8660254037844432595, -0.4999999999999920064 ) ) ;
#49821 = CARTESIAN_POINT ( 'NONE',  ( 93.67500000000001137, -212.2949673200287179, 80.58083333333331666 ) ) ;
#49822 = VECTOR ( 'NONE', #66060, 1000.000000000000000 ) ;
#49823 = ORIENTED_EDGE ( 'NONE', *, *, #64451, .F. ) ;
#49824 = ORIENTED_EDGE ( 'NONE', *, *, #39298, .F. ) ;
#49825 = ORIENTED_EDGE ( 'NONE', *, *, #11795, .F. ) ;
#49826 = VERTEX_POINT ( 'NONE', #58205 ) ;
#49827 = DIRECTION ( 'NONE',  ( 0.6064928550163524168, 0.7950889364178788110, 0.000000000000000000 ) ) ;
#49828 = EDGE_CURVE ( 'NONE', #18411, #16727, #10009, .T. ) ;
#49829 = EDGE_CURVE ( 'NONE', #25328, #35339, #71224, .T. ) ;
#49830 =( LENGTH_UNIT ( ) NAMED_UNIT ( * ) SI_UNIT ( .MILLI., .METRE. ) );
#49831 = FACE_OUTER_BOUND ( 'NONE', #60864, .T. ) ;
#49832 = AXIS2_PLACEMENT_3D ( 'NONE', #14469, #19729, #2858 ) ;
#49833 = CARTESIAN_POINT ( 'NONE',  ( -94.99999999999997158, -206.9400435732949575, 77.14124999999999943 ) ) ;
#49834 = FACE_OUTER_BOUND ( 'NONE', #37828, .T. ) ;
#49835 = FACE_OUTER_BOUND ( 'NONE', #24244, .T. ) ;
#49836 = DIRECTION ( 'NONE',  ( 0.000000000000000000, -0.2079116908177532363, -0.9781476007338069101 ) ) ;
#49837 = ORIENTED_EDGE ( 'NONE', *, *, #54427, .T. ) ;
#49838 = CARTESIAN_POINT ( 'NONE',  ( -94.99999999999997158, -206.9400435732949575, 85.47562500173431488 ) ) ;
#49839 = VERTEX_POINT ( 'NONE', #58572 ) ;
#49840 = CARTESIAN_POINT ( 'NONE',  ( -26.53422223201112828, -120.6595836127786043, 5.500000000000000000 ) ) ;
#49841 = EDGE_CURVE ( 'NONE', #48661, #63983, #29613, .T. ) ;
#49842 = EDGE_LOOP ( 'NONE', ( #12102, #26271, #2477, #48560 ) ) ;
#49843 = AXIS2_PLACEMENT_3D ( 'NONE', #43907, #37521, #31490 ) ;
#49844 = CARTESIAN_POINT ( 'NONE',  ( -95.00000000000002842, 86.94004357329504273, 81.34812500173430294 ) ) ;
#49845 = ORIENTED_EDGE ( 'NONE', *, *, #34814, .F. ) ;
#49846 = CARTESIAN_POINT ( 'NONE',  ( 92.69370383062498320, 91.33154071421968467, 82.12864583420048348 ) ) ;
#49847 = DIRECTION ( 'NONE',  ( -0.000000000000000000, -0.000000000000000000, 1.000000000000000000 ) ) ;
#49848 = CARTESIAN_POINT ( 'NONE',  ( 10.00000000000000000, 0.000000000000000000, 0.000000000000000000 ) ) ;
#49849 = CARTESIAN_POINT ( 'NONE',  ( 0.000000000000000000, 0.000000000000000000, 0.000000000000000000 ) ) ;
#49850 = CARTESIAN_POINT ( 'NONE',  ( 6.377742925735834234, -145.7647898336708181, 5.500000000000000000 ) ) ;
#49851 = CARTESIAN_POINT ( 'NONE',  ( 10.00000000000000000, 0.000000000000000000, 0.000000000000000000 ) ) ;
#49852 = ORIENTED_EDGE ( 'NONE', *, *, #72816, .T. ) ;
#49853 = DIRECTION ( 'NONE',  ( -1.000000000000000000, -0.000000000000000000, -0.000000000000000000 ) ) ;
#49854 = DIRECTION ( 'NONE',  ( -1.000000000000000000, 0.000000000000000000, -0.000000000000000000 ) ) ;
#49855 = VERTEX_POINT ( 'NONE', #12338 ) ;
#49856 = VERTEX_POINT ( 'NONE', #64230 ) ;
#49857 = CYLINDRICAL_SURFACE ( 'NONE', #61213, 31.99999999999998579 ) ;
#49858 = DIRECTION ( 'NONE',  ( 0.000000000000000000, 0.5877852522924708056, -0.8090169943749491166 ) ) ;
#49859 = CARTESIAN_POINT ( 'NONE',  ( 11.99999999999999822, 0.000000000000000000, 0.000000000000000000 ) ) ;
#49860 = CARTESIAN_POINT ( 'NONE',  ( -93.84685191531248449, -208.0026889286704943, 83.87489583420048689 ) ) ;
#49861 = ORIENTED_EDGE ( 'NONE', *, *, #39213, .F. ) ;
#49862 = TOROIDAL_SURFACE ( 'NONE', #61910, 2.699999999999999734, 0.2000000000000000111 ) ;
#49863 = DIRECTION ( 'NONE',  ( -1.000000000000000000, 0.000000000000000000, -0.000000000000000000 ) ) ;
#49864 = ORIENTED_EDGE ( 'NONE', *, *, #35476, .T. ) ;
#49865 = CARTESIAN_POINT ( 'NONE',  ( 0.000000000000000000, -120.0000000000000000, 2.500000000000000000 ) ) ;
#49866 = VECTOR ( 'NONE', #2967, 999.9999999999998863 ) ;
#49867 = CARTESIAN_POINT ( 'NONE',  ( 92.34999999999998010, 90.00001272874952463, 81.82437456149077093 ) ) ;
#49868 = CARTESIAN_POINT ( 'NONE',  ( 97.64999999997404245, -210.0000117261773198, 82.77687459617033028 ) ) ;
#49869 = CARTESIAN_POINT ( 'NONE',  ( 93.84685191531248449, 88.00268892867053694, 78.95364583420047211 ) ) ;
#49870 = FACE_OUTER_BOUND ( 'NONE', #47233, .T. ) ;
#49871 = CARTESIAN_POINT ( 'NONE',  ( 97.64999999999999147, 89.99999997928482287, 80.87187500099604165 ) ) ;
#49872 = CIRCLE ( 'NONE', #43891, 15.99999999999999822 ) ;
#49873 = FACE_OUTER_BOUND ( 'NONE', #54464, .T. ) ;
#49874 = CARTESIAN_POINT ( 'NONE',  ( 10.00000000000000000, 73.73191006444551476, 14.66109333815590254 ) ) ;
#49875 = DIRECTION ( 'NONE',  ( 3.035766082959412415E-16, 1.000000000000000000, 0.000000000000000000 ) ) ;
#49876 = LINE ( 'NONE', #40462, #39417 ) ;
#49877 =( BOUNDED_CURVE ( )  B_SPLINE_CURVE ( 2, ( #69104, #61983, #351, #710, #51426, #57821, #28872 ),
 .UNSPECIFIED., .F., .F. ) 
 B_SPLINE_CURVE_WITH_KNOTS ( ( 3, 2, 2, 3 ),
 ( 0.2708333333333337034, 0.2777777777777781232, 0.2847222222222224874, 0.2916666666666669072 ),
 .UNSPECIFIED. ) 
 CURVE ( )  GEOMETRIC_REPRESENTATION_ITEM ( )  RATIONAL_B_SPLINE_CURVE ( ( 0.9999999999999924505, 0.8660254037844462571, 1.000000000000000000, 0.8660254037844387076, 1.000000000000000000, 0.8660254037844343777, 1.000000000000004219 ) ) 
 REPRESENTATION_ITEM ( '' )  );
#49878 = CARTESIAN_POINT ( 'NONE',  ( 0.000000000000000000, 12.26510123303308752, -35.53030884539072787 ) ) ;
#49879 = VECTOR ( 'NONE', #5783, 1000.000000000000000 ) ;
#49880 = CARTESIAN_POINT ( 'NONE',  ( 93.67500000000001137, -212.2949673200287179, 78.67583333333332973 ) ) ;
#49881 = CARTESIAN_POINT ( 'NONE',  ( -92.35000000000177067, -209.9999969335172807, 75.79187510780353421 ) ) ;
#49882 = ORIENTED_EDGE ( 'NONE', *, *, #61306, .F. ) ;
#49883 = ADVANCED_FACE ( 'NONE', ( #29993 ), #41647, .T. ) ;
#49884 = CARTESIAN_POINT ( 'NONE',  ( -93.84685191531254134, 91.99731107132950569, 84.35114583420048007 ) ) ;
#49885 = FACE_OUTER_BOUND ( 'NONE', #72730, .T. ) ;
#49886 = ADVANCED_FACE ( 'NONE', ( #69848 ), #35278, .T. ) ;
#49887 = CIRCLE ( 'NONE', #55912, 13.71319123027096865 ) ;
#49888 = ADVANCED_FACE ( 'NONE', ( #1479 ), #64588, .T. ) ;
#49889 = DIRECTION ( 'NONE',  ( -0.6516173805718079581, 0.7585478161175706058, 0.000000000000000000 ) ) ;
#49890 = ORIENTED_EDGE ( 'NONE', *, *, #6862, .T. ) ;
#49891 = EDGE_CURVE ( 'NONE', #70907, #55045, #35182, .T. ) ;
#49892 = DIRECTION ( 'NONE',  ( -0.000000000000000000, -0.000000000000000000, 1.000000000000000000 ) ) ;
#49893 = CYLINDRICAL_SURFACE ( 'NONE', #20383, 32.00000000000000000 ) ;
#49894 = CYLINDRICAL_SURFACE ( 'NONE', #50400, 37.49900000000000233 ) ;
#49895 = EDGE_CURVE ( 'NONE', #8127, #44775, #58104, .T. ) ;
#49896 = CARTESIAN_POINT ( 'NONE',  ( -7.572224309238338336, -145.4393675041377492, -5.500000000000000000 ) ) ;
#49897 = CARTESIAN_POINT ( 'NONE',  ( 93.84685191531249870, -208.0026889286704943, 79.53572916753381605 ) ) ;
#49898 = ORIENTED_EDGE ( 'NONE', *, *, #15424, .T. ) ;
#49899 = ORIENTED_EDGE ( 'NONE', *, *, #19913, .F. ) ;
#49900 = EDGE_CURVE ( 'NONE', #33622, #49572, #66087, .T. ) ;
#49901 = EDGE_CURVE ( 'NONE', #66429, #34383, #52085, .T. ) ;
#49902 = CARTESIAN_POINT ( 'NONE',  ( -96.32499999999996021, -207.7050326799711968, 81.71854166840095957 ) ) ;
#49903 = CARTESIAN_POINT ( 'NONE',  ( 10.00000000000000000, -37.01155633439053361, -6.555932627142825986 ) ) ;
#49904 = DIRECTION ( 'NONE',  ( -1.000000000000000000, -0.000000000000000000, 0.000000000000000000 ) ) ;
#49905 = DIRECTION ( 'NONE',  ( 1.000000000000000000, -7.571537405616606460E-15, -2.598394312951952234E-14 ) ) ;
#49906 = AXIS2_PLACEMENT_3D ( 'NONE', #53476, #71487, #26373 ) ;
#49907 = CARTESIAN_POINT ( 'NONE',  ( 5.000000000000000000, 38.55633173627010279, 16.65560815589424593 ) ) ;
#49908 = CARTESIAN_POINT ( 'NONE',  ( 92.69370383062501162, -208.6684592857803011, 75.14364583420049826 ) ) ;
#49909 = ORIENTED_EDGE ( 'NONE', *, *, #13580, .F. ) ;
#49910 = CARTESIAN_POINT ( 'NONE',  ( 0.000000000000000000, -14.66109333815410487, -73.73191006444587003 ) ) ;
#49911 = VERTEX_POINT ( 'NONE', #61177 ) ;
#49912 = VECTOR ( 'NONE', #44589, 1000.000000000000000 ) ;
#49913 = ORIENTED_EDGE ( 'NONE', *, *, #54257, .T. ) ;
#49914 = DIRECTION ( 'NONE',  ( 1.000000000000000000, 0.000000000000000000, 0.000000000000000000 ) ) ;
#49915 = EDGE_CURVE ( 'NONE', #23048, #36276, #3309, .T. ) ;
#49916 = EDGE_CURVE ( 'NONE', #25977, #30113, #19658, .T. ) ;
#49917 = SURFACE_STYLE_USAGE ( .BOTH. , #4089 ) ;
#49918 = CIRCLE ( 'NONE', #29452, 31.99999999999998579 ) ;
#49919 = CARTESIAN_POINT ( 'NONE',  ( -97.65000000000001990, 90.00000000000004263, 89.44437500173430067 ) ) ;
#49920 = ORIENTED_EDGE ( 'NONE', *, *, #35132, .F. ) ;
#49921 = DIRECTION ( 'NONE',  ( 0.7533909544171996098, 0.6575728627325955200, -7.625282249115660656E-32 ) ) ;
#49922 = CARTESIAN_POINT ( 'NONE',  ( 92.35000000000002274, -211.5299782133524502, 78.70229166840096013 ) ) ;
#49923 = CARTESIAN_POINT ( 'NONE',  ( 96.32499999999997442, 92.29496732002878900, 80.26333333333332121 ) ) ;
#49924 = ORIENTED_EDGE ( 'NONE', *, *, #62327, .F. ) ;
#49925 = CYLINDRICAL_SURFACE ( 'NONE', #37064, 77.49899999999999523 ) ;
#49926 = ORIENTED_EDGE ( 'NONE', *, *, #21617, .T. ) ;
#49927 = CARTESIAN_POINT ( 'NONE',  ( -93.23660927304928236, -211.4937631030103944, 74.79348190356849102 ) ) ;
#49928 = AXIS2_PLACEMENT_3D ( 'NONE', #26479, #49412, #53953 ) ;
#49929 = ORIENTED_EDGE ( 'NONE', *, *, #65007, .F. ) ;
#49930 = VECTOR ( 'NONE', #36923, 1000.000000000000227 ) ;
#49931 = LINE ( 'NONE', #10839, #51194 ) ;
#49932 = CARTESIAN_POINT ( 'NONE',  ( -96.15314808468752972, 91.99731107132950569, 85.88572916753381037 ) ) ;
#49933 = CARTESIAN_POINT ( 'NONE',  ( 92.69370383062498320, 90.00000000000002842, 78.84781250086714977 ) ) ;
#49934 = VERTEX_POINT ( 'NONE', #72068 ) ;
#49935 = DIRECTION ( 'NONE',  ( 0.000000000000000000, 0.7431448254773862505, 0.6691306063588671194 ) ) ;
#49936 = LINE ( 'NONE', #71377, #18054 ) ;
#49937 = ORIENTED_EDGE ( 'NONE', *, *, #35499, .T. ) ;
#49938 = CARTESIAN_POINT ( 'NONE',  ( -7.500000000000015987, -76.29999999999999716, -255.0000000000000000 ) ) ;
#49939 = CARTESIAN_POINT ( 'NONE',  ( -96.15314808468747287, -208.0026889286704943, 81.91697916753381037 ) ) ;
#49940 = ORIENTED_EDGE ( 'NONE', *, *, #8574, .T. ) ;
#49941 = AXIS2_PLACEMENT_3D ( 'NONE', #60913, #2705, #9404 ) ;
#49942 = ORIENTED_EDGE ( 'NONE', *, *, #67240, .T. ) ;
#49943 = CARTESIAN_POINT ( 'NONE',  ( 0.000000000000000000, 0.000000000000000000, 0.000000000000000000 ) ) ;
#49944 = ORIENTED_EDGE ( 'NONE', *, *, #33634, .T. ) ;
#49945 = CARTESIAN_POINT ( 'NONE',  ( 11.99999999999999822, 58.39081064771751528, 50.95692526931350841 ) ) ;
#49946 = FACE_OUTER_BOUND ( 'NONE', #12696, .T. ) ;
#49947 = ORIENTED_EDGE ( 'NONE', *, *, #1563, .F. ) ;
#49948 = CARTESIAN_POINT ( 'NONE',  ( -96.15314808468745866, -211.9973110713294489, 78.31864583420048120 ) ) ;
#49949 = VERTEX_POINT ( 'NONE', #9662 ) ;
#49950 = DIRECTION ( 'NONE',  ( -1.000000000000000000, 0.000000000000000000, -0.000000000000000000 ) ) ;
#49951 = CYLINDRICAL_SURFACE ( 'NONE', #38058, 16.00000000000000000 ) ;
#49952 = CARTESIAN_POINT ( 'NONE',  ( 97.64999999964362587, 89.99995654222556141, 89.12687334326064104 ) ) ;
#49953 = CARTESIAN_POINT ( 'NONE',  ( 11.99999999999999822, 50.23322058963442061, -64.81221759200288091 ) ) ;
#49954 = DIRECTION ( 'NONE',  ( -0.000000000000000000, -0.000000000000000000, -1.000000000000000000 ) ) ;
#49955 = CARTESIAN_POINT ( 'NONE',  ( -92.35000000000003695, 90.00000000000004263, 89.68250000000000455 ) ) ;
#49956 = CARTESIAN_POINT ( 'NONE',  ( -62.50000000000000000, 0.000000000000000000, -184.9999999999999432 ) ) ;
#49957 = EDGE_CURVE ( 'NONE', #38652, #50748, #49645, .T. ) ;
#49958 = CARTESIAN_POINT ( 'NONE',  ( -94.99999999999997158, -213.0599564267049857, 85.71374999999999034 ) ) ;
#49959 = FACE_OUTER_BOUND ( 'NONE', #34962, .T. ) ;
#49960 = EDGE_CURVE ( 'NONE', #28934, #72658, #2947, .T. ) ;
#49961 = DIRECTION ( 'NONE',  ( 0.000000000000000000, 0.6691306063588563502, 0.7431448254773960205 ) ) ;
#49962 = CYLINDRICAL_SURFACE ( 'NONE', #40705, 31.99999999999998579 ) ;
#49963 = CARTESIAN_POINT ( 'NONE',  ( 0.000000000000000000, 3.061616997868382648E-16, -2.499999999999999556 ) ) ;
#49964 = EDGE_CURVE ( 'NONE', #21818, #49000, #61689, .T. ) ;
#49965 = CARTESIAN_POINT ( 'NONE',  ( -97.65000000000001990, 90.00000000000004263, 76.03000000000000114 ) ) ;
#49966 = AXIS2_PLACEMENT_3D ( 'NONE', #37309, #36177, #65507 ) ;
#49967 = CARTESIAN_POINT ( 'NONE',  ( 5.000000000000002665, -2.886751345948134873, -5.553418012614792509 ) ) ;
#49968 = EDGE_CURVE ( 'NONE', #37734, #68371, #54439, .T. ) ;
#49969 = DIRECTION ( 'NONE',  ( -0.000000000000000000, 0.8660254037844432595, 0.4999999999999921729 ) ) ;
#49970 = CARTESIAN_POINT ( 'NONE',  ( 97.64999999999999147, 90.00000000000002842, 75.00000000000000000 ) ) ;
#49971 = AXIS2_PLACEMENT_3D ( 'NONE', #9539, #3919, #61422 ) ;
#49972 = ADVANCED_FACE ( 'NONE', ( #20191 ), #43889, .F. ) ;
#49973 = CARTESIAN_POINT ( 'NONE',  ( -94.99999999999997158, -213.0599564267049857, 86.34874999999999545 ) ) ;
#49974 = AXIS2_PLACEMENT_3D ( 'NONE', #27270, #60042, #14894 ) ;
#49975 = CARTESIAN_POINT ( 'NONE',  ( -94.99999999999997158, -209.9999999999999716, 90.00000000000000000 ) ) ;
#49976 = PRODUCT ( 'electric motor unit', 'electric motor unit', '', ( #17395 ) ) ;
#49977 = VECTOR ( 'NONE', #32021, 1000.000000000000000 ) ;
#49978 = EDGE_CURVE ( 'NONE', #66920, #62456, #68886, .T. ) ;
#49979 = DIRECTION ( 'NONE',  ( -1.000000000000000000, -0.000000000000000000, -0.000000000000000000 ) ) ;
#49980 = CARTESIAN_POINT ( 'NONE',  ( 10.00000000000000000, 0.000000000000000000, 0.000000000000000000 ) ) ;
#49981 = DIRECTION ( 'NONE',  ( 0.000000000000000000, 0.000000000000000000, 1.000000000000000000 ) ) ;
#49982 = CARTESIAN_POINT ( 'NONE',  ( 13.83832728059186046, -142.6495187161941089, 2.500000000000000000 ) ) ;
#49983 = CARTESIAN_POINT ( 'NONE',  ( 92.69370383062501162, -211.3315407142195852, 75.09072916753382287 ) ) ;
#49984 = VECTOR ( 'NONE', #34560, 1000.000000000000000 ) ;
#49985 = ORIENTED_EDGE ( 'NONE', *, *, #12557, .F. ) ;
#49986 = VERTEX_POINT ( 'NONE', #25102 ) ;
#49987 = EDGE_CURVE ( 'NONE', #18460, #70614, #43155, .T. ) ;
#49988 = CARTESIAN_POINT ( 'NONE',  ( 0.000000000000000000, -44.99326035066101781, 68.55367621811126355 ) ) ;
#49989 = EDGE_CURVE ( 'NONE', #28223, #23361, #8923, .T. ) ;
#49990 = CARTESIAN_POINT ( 'NONE',  ( 0.000000000000000000, 14.60985201121729737, -18.46759930825688301 ) ) ;
#49991 = ORIENTED_EDGE ( 'NONE', *, *, #35385, .F. ) ;
#49992 = CARTESIAN_POINT ( 'NONE',  ( 95.00000000000000000, -212.6630814284392557, 77.10156250086711793 ) ) ;
#49993 = CARTESIAN_POINT ( 'NONE',  ( 92.69370383062501162, -211.3315407142195852, 85.40947916753381719 ) ) ;
#49994 = EDGE_LOOP ( 'NONE', ( #659, #59719, #22278, #9995, #47428 ) ) ;
#49995 = CARTESIAN_POINT ( 'NONE',  ( 97.30629616937498838, -208.6684592857803011, 85.09197916753380753 ) ) ;
#49996 = ORIENTED_EDGE ( 'NONE', *, *, #26207, .F. ) ;
#49997 = LINE ( 'NONE', #16170, #3497 ) ;
#49998 = ORIENTED_EDGE ( 'NONE', *, *, #1333, .F. ) ;
#49999 = DIRECTION ( 'NONE',  ( 0.000000000000000000, 0.000000000000000000, 1.000000000000000000 ) ) ;
#50000 = ORIENTED_EDGE ( 'NONE', *, *, #43666, .F. ) ;
#50001 = DIRECTION ( 'NONE',  ( 0.000000000000000000, 0.9723699203976773342, -0.2334453638559024213 ) ) ;
#50002 = ORIENTED_EDGE ( 'NONE', *, *, #838, .F. ) ;
#50003 = LINE ( 'NONE', #54550, #23310 ) ;
#50004 = CARTESIAN_POINT ( 'NONE',  ( 97.64999999999999147, -209.9999999999999716, 89.12687500173430521 ) ) ;
#50005 = EDGE_LOOP ( 'NONE', ( #66662, #11015, #2609, #11461 ) ) ;
#50006 = DIRECTION ( 'NONE',  ( -3.035766082959412415E-16, -1.000000000000000000, -0.000000000000000000 ) ) ;
#50007 = ORIENTED_EDGE ( 'NONE', *, *, #60274, .T. ) ;
#50008 = DIRECTION ( 'NONE',  ( -1.000000000000000000, 0.000000000000000000, -0.000000000000000000 ) ) ;
#50009 = AXIS2_PLACEMENT_3D ( 'NONE', #12419, #5691, #52273 ) ;
#50010 = ORIENTED_EDGE ( 'NONE', *, *, #41524, .T. ) ;
#50011 = VERTEX_POINT ( 'NONE', #70951 ) ;
#50012 = ORIENTED_EDGE ( 'NONE', *, *, #42374, .T. ) ;
#50013 = CARTESIAN_POINT ( 'NONE',  ( 96.15314808468748708, -208.0026889286704943, 74.82614583420047438 ) ) ;
#50014 = DIRECTION ( 'NONE',  ( 0.000000000000000000, 0.000000000000000000, 1.000000000000000000 ) ) ;
#50015 = ORIENTED_EDGE ( 'NONE', *, *, #44433, .F. ) ;
#50016 = ORIENTED_EDGE ( 'NONE', *, *, #14693, .F. ) ;
#50017 = AXIS2_PLACEMENT_3D ( 'NONE', #64397, #14360, #2756 ) ;
#50018 = ORIENTED_EDGE ( 'NONE', *, *, #67758, .T. ) ;
#50019 = VECTOR ( 'NONE', #1756, 1000.000000000000000 ) ;
#50020 = DIRECTION ( 'NONE',  ( -1.000000000000000000, 3.061616997868382648E-16, 0.000000000000000000 ) ) ;
#50021 = DIRECTION ( 'NONE',  ( -1.000000000000000000, 0.000000000000000000, 0.000000000000000000 ) ) ;
#50022 = CARTESIAN_POINT ( 'NONE',  ( -97.30629616937501680, 88.66845928578038638, 75.24947916753383481 ) ) ;
#50023 = EDGE_CURVE ( 'NONE', #48167, #26154, #19456, .T. ) ;
#50024 = ORIENTED_EDGE ( 'NONE', *, *, #1433, .T. ) ;
#50025 = AXIS2_PLACEMENT_3D ( 'NONE', #57855, #51091, #29618 ) ;
#50026 = CARTESIAN_POINT ( 'NONE',  ( 97.30629616937498838, 88.66845928578037217, 76.57239583420046358 ) ) ;
#50027 = ORIENTED_EDGE ( 'NONE', *, *, #32153, .F. ) ;
#50028 =( NAMED_UNIT ( * ) PLANE_ANGLE_UNIT ( ) SI_UNIT ( $, .RADIAN. ) );
#50029 = CARTESIAN_POINT ( 'NONE',  ( -94.99999999999997158, -207.3369185715606307, 88.21406250086714351 ) ) ;
#50030 = ORIENTED_EDGE ( 'NONE', *, *, #37215, .F. ) ;
#50031 = CARTESIAN_POINT ( 'NONE',  ( 0.1714266706912579152, -5.674529457426388923, -1.878862934774795823 ) ) ;
#50032 = CARTESIAN_POINT ( 'NONE',  ( 10.00000000000000178, 0.000000000000000000, 0.000000000000000000 ) ) ;
#50033 = FACE_OUTER_BOUND ( 'NONE', #20720, .T. ) ;
#50034 = CARTESIAN_POINT ( 'NONE',  ( -97.30629616937495996, -209.9999999999999716, 80.11781250086713158 ) ) ;
#50035 = DIRECTION ( 'NONE',  ( -1.000000000000000000, 0.000000000000000000, -0.000000000000000000 ) ) ;
#50036 = CARTESIAN_POINT ( 'NONE',  ( 14.53333333333331545, 0.000000000000000000, -1.466666666666671670 ) ) ;
#50037 = DIRECTION ( 'NONE',  ( 1.000000000000000000, 0.000000000000000000, 0.000000000000000000 ) ) ;
#50038 = ORIENTED_EDGE ( 'NONE', *, *, #30135, .T. ) ;
#50039 = AXIS2_PLACEMENT_3D ( 'NONE', #20879, #13755, #59634 ) ;
#50040 = ORIENTED_EDGE ( 'NONE', *, *, #60185, .T. ) ;
#50041 = CARTESIAN_POINT ( 'NONE',  ( -12.50000000000000000, -107.5000000000000000, 40.00000000000000000 ) ) ;
#50042 = EDGE_CURVE ( 'NONE', #8336, #24236, #60080, .T. ) ;
#50043 = CARTESIAN_POINT ( 'NONE',  ( 0.000000000000000000, 0.000000000000000000, 0.000000000000000000 ) ) ;
#50045 = EDGE_CURVE ( 'NONE', #61428, #11862, #8558, .T. ) ;
#50044 = CIRCLE ( 'NONE', #71677, 77.49899999999999523 ) ;
#50046 = CARTESIAN_POINT ( 'NONE',  ( 93.55421244156880789, -208.0396902886532757, 74.86947676125079454 ) ) ;
#50047 = CARTESIAN_POINT ( 'NONE',  ( -95.00000000000002842, 87.33691857156074434, 82.18156250086714465 ) ) ;
#50048 = CARTESIAN_POINT ( 'NONE',  ( 0.000000000000000000, 0.000000000000000000, -6.000000000000000000 ) ) ;
#50049 = CARTESIAN_POINT ( 'NONE',  ( 0.000000000000000000, 20.85821328998741109, 10.92862929874522315 ) ) ;
#50050 = EDGE_LOOP ( 'NONE', ( #30789, #47532, #74045, #20718 ) ) ;
#50051 = DIRECTION ( 'NONE',  ( 0.9827303690289279636, 0.1850432970638682395, -0.000000000000000000 ) ) ;
#50052 = EDGE_CURVE ( 'NONE', #64186, #47715, #2856, .T. ) ;
#50053 = EDGE_CURVE ( 'NONE', #26486, #69892, #33314, .T. ) ;
#50054 = CARTESIAN_POINT ( 'NONE',  ( -97.64999999999996305, -209.9999999999999716, 89.44437500173430067 ) ) ;
#50055 = CARTESIAN_POINT ( 'NONE',  ( 10.00000000000000000, -44.88180994100329713, -63.18004540533077318 ) ) ;
#50056 = CYLINDRICAL_SURFACE ( 'NONE', #69356, 37.49900000000000233 ) ;
#50057 = CARTESIAN_POINT ( 'NONE',  ( -97.65000000000003411, 91.52997821335256390, 87.40708333333333258 ) ) ;
#50058 = CARTESIAN_POINT ( 'NONE',  ( -94.99999999999997158, -212.6630814284392557, 79.16531250086715943 ) ) ;
#50059 = CARTESIAN_POINT ( 'NONE',  ( -94.99999999999997158, -213.0599564267049857, 87.06312500173429214 ) ) ;
#50060 = ORIENTED_EDGE ( 'NONE', *, *, #36829, .T. ) ;
#50061 = EDGE_CURVE ( 'NONE', #48148, #12834, #67551, .T. ) ;
#50062 = VECTOR ( 'NONE', #48484, 1000.000000000000000 ) ;
#50063 = CARTESIAN_POINT ( 'NONE',  ( 5.000000000000000000, -46.11716303203136391, -67.80270845531939017 ) ) ;
#50064 = CARTESIAN_POINT ( 'NONE',  ( -95.00000000000002842, 86.94004357329504273, 80.71312500173429783 ) ) ;
#50065 = CARTESIAN_POINT ( 'NONE',  ( -100.0000000000260059, -214.9999999999999716, 75.00000000001300293 ) ) ;
#50066 = VECTOR ( 'NONE', #12764, 1000.000000000000000 ) ;
#50067 = ORIENTED_EDGE ( 'NONE', *, *, #47679, .T. ) ;
#50068 = FACE_OUTER_BOUND ( 'NONE', #65656, .T. ) ;
#50069 = DIRECTION ( 'NONE',  ( -1.000000000000000000, 0.000000000000000000, -0.000000000000000000 ) ) ;
#50070 = AXIS2_PLACEMENT_3D ( 'NONE', #18428, #30439, #58658 ) ;
#50071 = VECTOR ( 'NONE', #52381, 1000.000000000000000 ) ;
#50072 = DIRECTION ( 'NONE',  ( -0.000000000000000000, -0.000000000000000000, 1.000000000000000000 ) ) ;
#50073 = ORIENTED_EDGE ( 'NONE', *, *, #1398, .T. ) ;
#50074 = EDGE_CURVE ( 'NONE', #13831, #25323, #11248, .T. ) ;
#50075 = CARTESIAN_POINT ( 'NONE',  ( 21.85433023846371370, -135.0628101570779620, -2.500000000000000444 ) ) ;
#50076 = DIRECTION ( 'NONE',  ( -1.000000000000000000, 0.000000000000000000, -0.000000000000000000 ) ) ;
#50077 = VERTEX_POINT ( 'NONE', #15679 ) ;
#50078 =( BOUNDED_CURVE ( )  B_SPLINE_CURVE ( 2, ( #66764, #15256, #46063, #12580, #17484, #23868, #603 ),
 .UNSPECIFIED., .F., .F. ) 
 B_SPLINE_CURVE_WITH_KNOTS ( ( 3, 2, 2, 3 ),
 ( 0.2916666666666669072, 0.2986111111111113270, 0.3055555555555557468, 0.3125000000000001665 ),
 .UNSPECIFIED. ) 
 CURVE ( )  GEOMETRIC_REPRESENTATION_ITEM ( )  RATIONAL_B_SPLINE_CURVE ( ( 0.9999999999999956701, 0.8660254037844430375, 1.000000000000000000, 0.8660254037844387076, 1.000000000000000000, 0.8660254037844354880, 1.000000000000003109 ) ) 
 REPRESENTATION_ITEM ( '' )  );
#50079 = CARTESIAN_POINT ( 'NONE',  ( 11.99999999999999822, 0.000000000000000000, 0.000000000000000000 ) ) ;
#50080 = CARTESIAN_POINT ( 'NONE',  ( -93.67499999999998295, -207.7050326799711968, 87.32770833506762642 ) ) ;
#50081 = EDGE_CURVE ( 'NONE', #48516, #65637, #20847, .T. ) ;
#50082 = ORIENTED_EDGE ( 'NONE', *, *, #39464, .T. ) ;
#50083 = DIRECTION ( 'NONE',  ( 0.000000000000000000, 0.000000000000000000, -1.000000000000000000 ) ) ;
#50084 = ORIENTED_EDGE ( 'NONE', *, *, #36224, .T. ) ;
#50085 = CARTESIAN_POINT ( 'NONE',  ( 12.49999999999999645, 1.530808498934191127E-15, -44.99999999999998579 ) ) ;
#50086 = LINE ( 'NONE', #13390, #64798 ) ;
#50087 = EDGE_LOOP ( 'NONE', ( #22462, #35449, #62337, #59038 ) ) ;
#50088 = VERTEX_POINT ( 'NONE', #67926 ) ;
#50089 = EDGE_LOOP ( 'NONE', ( #64287, #10637, #58040, #41150 ) ) ;
#50090 = LINE ( 'NONE', #4641, #59984 ) ;
#50091 = AXIS2_PLACEMENT_3D ( 'NONE', #49730, #50096, #46986 ) ;
#50092 = ORIENTED_EDGE ( 'NONE', *, *, #44414, .T. ) ;
#50093 = VERTEX_POINT ( 'NONE', #55898 ) ;
#50094 = CARTESIAN_POINT ( 'NONE',  ( 94.99999999999998579, 92.66308142843935514, 76.30781250086715772 ) ) ;
#50095 = CARTESIAN_POINT ( 'NONE',  ( 10.00000000000000000, 0.000000000000000000, 0.000000000000000000 ) ) ;
#50096 = DIRECTION ( 'NONE',  ( -1.000000000000000000, 0.000000000000000000, -0.000000000000000000 ) ) ;
#50097 = ORIENTED_EDGE ( 'NONE', *, *, #25748, .T. ) ;
#50098 = EDGE_LOOP ( 'NONE', ( #40027, #51577, #62462, #34601 ) ) ;
#50099 = ORIENTED_EDGE ( 'NONE', *, *, #66656, .T. ) ;
#50100 = CARTESIAN_POINT ( 'NONE',  ( 92.69370383062498320, 88.66845928578037217, 89.06072916753379332 ) ) ;
#50101 = EDGE_LOOP ( 'NONE', ( #34237, #31526, #61157, #74227 ) ) ;
#50102 = CARTESIAN_POINT ( 'NONE',  ( 97.30629616937498838, -208.6684592857803011, 86.20322916753382003 ) ) ;
#50103 = CARTESIAN_POINT ( 'NONE',  ( 94.99999999999998579, 90.00000000000002842, 90.00000000000000000 ) ) ;
#50104 = LINE ( 'NONE', #61038, #12590 ) ;
#50105 = DIRECTION ( 'NONE',  ( -1.000000000000000000, -0.000000000000000000, -0.000000000000000000 ) ) ;
#50106 = PLANE ( 'NONE',  #36771 ) ;
#50107 = CARTESIAN_POINT ( 'NONE',  ( -93.67499999999998295, -207.7050326799711968, 82.80333333333332746 ) ) ;
#50108 = CARTESIAN_POINT ( 'NONE',  ( 0.000000000000000000, 5.835314593368477354, 22.81335362449854642 ) ) ;
#50109 = CARTESIAN_POINT ( 'NONE',  ( -97.30629616937497417, -211.3315407142195852, 88.42572916753380241 ) ) ;
#50110 = CARTESIAN_POINT ( 'NONE',  ( -95.00000000000002842, 87.33691857156074434, 84.24531250086715772 ) ) ;
#50111 = EDGE_LOOP ( 'NONE', ( #71011, #9515, #28077, #15862 ) ) ;
#50113 = CARTESIAN_POINT ( 'NONE',  ( -96.15314808468752972, 91.99731107132950569, 88.26697916753380468 ) ) ;
#50112 = CARTESIAN_POINT ( 'NONE',  ( 97.30629616937498838, 88.66845928578037217, 86.73239583420047438 ) ) ;
#50114 = ORIENTED_EDGE ( 'NONE', *, *, #25227, .F. ) ;
#50115 = DIRECTION ( 'NONE',  ( -1.000000000000000000, -0.000000000000000000, 0.000000000000000000 ) ) ;
#50116 = AXIS2_PLACEMENT_3D ( 'NONE', #15673, #38603, #61540 ) ;
#50117 = CARTESIAN_POINT ( 'NONE',  ( 0.000000000000000000, 37.48860685352291000, -0.8828120875901940279 ) ) ;
#50118 = DIRECTION ( 'NONE',  ( -1.000000000000000000, 0.000000000000000000, 0.000000000000000000 ) ) ;
#50119 = DIRECTION ( 'NONE',  ( -1.000000000000000000, -0.000000000000000000, -0.000000000000000000 ) ) ;
#50120 = CARTESIAN_POINT ( 'NONE',  ( -92.69370383062498320, -208.6684592857803295, 89.37822916753378877 ) ) ;
#50121 = STYLED_ITEM ( 'NONE', ( #1111 ), #12168 ) ;
#50122 = DIRECTION ( 'NONE',  ( -1.000000000000000000, 0.000000000000000000, -0.000000000000000000 ) ) ;
#50123 = EDGE_CURVE ( 'NONE', #4061, #53067, #16419, .T. ) ;
#50124 = DIRECTION ( 'NONE',  ( -1.000000000000000000, -0.000000000000000000, -0.000000000000000000 ) ) ;
#50125 = LINE ( 'NONE', #45647, #64704 ) ;
#50126 = ORIENTED_EDGE ( 'NONE', *, *, #41680, .T. ) ;
#50127 = CIRCLE ( 'NONE', #32146, 4.750000000000000000 ) ;
#50128 = ORIENTED_EDGE ( 'NONE', *, *, #56665, .T. ) ;
#50129 = AXIS2_PLACEMENT_3D ( 'NONE', #53044, #18809, #41750 ) ;
#50130 = ADVANCED_FACE ( 'NONE', ( #62293 ), #17161, .T. ) ;
#50131 = CARTESIAN_POINT ( 'NONE',  ( -97.65000000000001990, 90.00000000000004263, 81.10999999999999943 ) ) ;
#50132 = EDGE_CURVE ( 'NONE', #36714, #428, #50998, .T. ) ;
#50133 = DIRECTION ( 'NONE',  ( -1.000000000000000000, 0.000000000000000000, 0.000000000000000000 ) ) ;
#50134 = CARTESIAN_POINT ( 'NONE',  ( 97.65000000000000568, -211.5299782133524218, 75.73895833506765030 ) ) ;
#50135 = DIRECTION ( 'NONE',  ( -1.000000000000000000, 0.000000000000000000, 0.000000000000000000 ) ) ;
#50136 = DIRECTION ( 'NONE',  ( -1.000000000000000000, 7.571543891232750625E-15, 2.563413034563919882E-14 ) ) ;
#50137 = LINE ( 'NONE', #38133, #17157 ) ;
#50138 = CARTESIAN_POINT ( 'NONE',  ( -94.99999999999997158, -209.9999999999999716, 90.00000000000000000 ) ) ;
#50139 = LINE ( 'NONE', #33978, #14395 ) ;
#50140 = ORIENTED_EDGE ( 'NONE', *, *, #57784, .T. ) ;
#50141 = CARTESIAN_POINT ( 'NONE',  ( -95.00000000000002842, 87.33691857156074434, 82.81656250086713555 ) ) ;
#50142 = ADVANCED_FACE ( 'NONE', ( #56276 ), #44633, .T. ) ;
#50143 = CARTESIAN_POINT ( 'NONE',  ( -8.826826895187510402, -94.96827758698185562, 2.500000000000000000 ) ) ;
#50144 = PLANE ( 'NONE',  #17441 ) ;
#50145 = VECTOR ( 'NONE', #19033, 1000.000000000000000 ) ;
#50146 = DIRECTION ( 'NONE',  ( -1.000000000000000000, -0.000000000000000000, 0.000000000000000000 ) ) ;
#50147 = CARTESIAN_POINT ( 'NONE',  ( 0.000000000000000000, 75.11725578898472122, -2.956366410619845730 ) ) ;
#50148 = AXIS2_PLACEMENT_3D ( 'NONE', #68318, #16811, #5547 ) ;
#50149 = CARTESIAN_POINT ( 'NONE',  ( 11.99999999999999822, 31.47745569255140552, 68.26794271651274926 ) ) ;
#50150 = CARTESIAN_POINT ( 'NONE',  ( -94.99999999999997158, -207.3369185715606307, 88.37281250086715545 ) ) ;
#50151 = AXIS2_PLACEMENT_3D ( 'NONE', #50556, #44567, #27242 ) ;
#50152 = CARTESIAN_POINT ( 'NONE',  ( 0.000000000000000000, -6.555932627142676772, 37.01155633439056203 ) ) ;
#50153 = VECTOR ( 'NONE', #18538, 1000.000000000000000 ) ;
#50154 = EDGE_CURVE ( 'NONE', #13883, #11059, #7650, .T. ) ;
#50155 = AXIS2_PLACEMENT_3D ( 'NONE', #39180, #62113, #29725 ) ;
#50156 = ADVANCED_FACE ( 'NONE', ( #68301 ), #55531, .T. ) ;
#50157 = CARTESIAN_POINT ( 'NONE',  ( 94.99999999999998579, 92.66308142843932671, 78.84781250086714977 ) ) ;
#50158 = CARTESIAN_POINT ( 'NONE',  ( -94.99999999999997158, -212.6630814284392557, 82.97531250086714749 ) ) ;
#50159 = CYLINDRICAL_SURFACE ( 'NONE', #53058, 31.99999999999998579 ) ;
#50160 = ORIENTED_EDGE ( 'NONE', *, *, #32514, .T. ) ;
#50161 = CARTESIAN_POINT ( 'NONE',  ( 92.35000000052950497, -209.9999663481461027, 81.18829462297289012 ) ) ;
#50162 = CARTESIAN_POINT ( 'NONE',  ( -97.64999999999994884, -208.4700217866474645, 76.61208333333333087 ) ) ;
#50163 = DIRECTION ( 'NONE',  ( 0.000000000000000000, 0.7071067811865487940, -0.7071067811865462405 ) ) ;
#50164 = CARTESIAN_POINT ( 'NONE',  ( -92.69370383062505425, 88.66845928578038638, 79.90614583420048689 ) ) ;
#50165 = CARTESIAN_POINT ( 'NONE',  ( 96.15314808468748708, -208.0026889286704943, 81.81114583420047381 ) ) ;
#50166 = EDGE_LOOP ( 'NONE', ( #7129, #1608, #26251, #49277 ) ) ;
#50167 = EDGE_CURVE ( 'NONE', #19199, #7429, #61920, .T. ) ;
#50168 = CARTESIAN_POINT ( 'NONE',  ( 0.000000000000000000, 0.000000000000000000, -54.99999999999998579 ) ) ;
#50169 = VERTEX_POINT ( 'NONE', #57020 ) ;
#50170 = AXIS2_PLACEMENT_3D ( 'NONE', #66124, #65381, #48442 ) ;
#50171 = CARTESIAN_POINT ( 'NONE',  ( 10.00000000000000000, 39.04073710021366139, -15.48615015657542848 ) ) ;
#50172 = EDGE_LOOP ( 'NONE', ( #15270, #56730, #32804, #56834 ) ) ;
#50173 = CIRCLE ( 'NONE', #71798, 37.49900000000001654 ) ;
#50174 = AXIS2_PLACEMENT_3D ( 'NONE', #73552, #22439, #57025 ) ;
#50175 = DIRECTION ( 'NONE',  ( 0.000000000000000000, 0.1564344650402312020, -0.9876883405951376593 ) ) ;
#50176 = VECTOR ( 'NONE', #49413, 1000.000000000000000 ) ;
#50177 = ORIENTED_EDGE ( 'NONE', *, *, #30107, .F. ) ;
#50178 = VERTEX_POINT ( 'NONE', #10028 ) ;
#50179 = AXIS2_PLACEMENT_3D ( 'NONE', #11882, #52114, #657 ) ;
#50180 = ORIENTED_EDGE ( 'NONE', *, *, #14757, .T. ) ;
#50181 = CARTESIAN_POINT ( 'NONE',  ( 96.15314808468750130, -211.9973110713294489, 76.67822916753381435 ) ) ;
#50182 = ORIENTED_EDGE ( 'NONE', *, *, #29208, .T. ) ;
#50183 = FACE_OUTER_BOUND ( 'NONE', #32476, .T. ) ;
#50184 = CARTESIAN_POINT ( 'NONE',  ( 15.00000000000000000, 23.59884966291538078, 12.14883922797231008 ) ) ;
#50185 = CARTESIAN_POINT ( 'NONE',  ( 94.99999999999998579, 87.33691857156068750, 86.78531250086716398 ) ) ;
#50186 = LINE ( 'NONE', #23764, #39380 ) ;
#50187 = CARTESIAN_POINT ( 'NONE',  ( 92.35000000000002274, -211.5299782133524502, 76.71791666666666742 ) ) ;
#50188 = ORIENTED_EDGE ( 'NONE', *, *, #9071, .T. ) ;
#50189 = ORIENTED_EDGE ( 'NONE', *, *, #37534, .F. ) ;
#50190 = ORIENTED_EDGE ( 'NONE', *, *, #19284, .F. ) ;
#50191 = ORIENTED_EDGE ( 'NONE', *, *, #38783, .F. ) ;
#50192 = CIRCLE ( 'NONE', #67064, 31.99999999999998579 ) ;
#50193 = SURFACE_STYLE_USAGE ( .BOTH. , #39313 ) ;
#50194 = CARTESIAN_POINT ( 'NONE',  ( 10.00000000000000000, -51.02545421589285723, -55.20638768913812555 ) ) ;
#50195 = CARTESIAN_POINT ( 'NONE',  ( -2.499999999999970690, 73.00000000000001421, -255.0000000000000000 ) ) ;
#50196 = VECTOR ( 'NONE', #32920, 1000.000000000000000 ) ;
#50197 = CARTESIAN_POINT ( 'NONE',  ( 10.00000000000000000, -65.59268652807237743, 36.72794159290217664 ) ) ;
#50198 = CARTESIAN_POINT ( 'NONE',  ( 2.500000000000015987, 65.00000000000000000, -290.0000000000000568 ) ) ;
#50199 = VECTOR ( 'NONE', #48625, 1000.000000000000000 ) ;
#50200 = FACE_OUTER_BOUND ( 'NONE', #70234, .T. ) ;
#50201 = VECTOR ( 'NONE', #69946, 1000.000000000000000 ) ;
#50202 = EDGE_LOOP ( 'NONE', ( #60253, #18850, #42415, #48825 ) ) ;
#50203 = CARTESIAN_POINT ( 'NONE',  ( -96.32499999999996021, -212.2949673200287179, 83.20020833506764291 ) ) ;
#50204 = ORIENTED_EDGE ( 'NONE', *, *, #8419, .T. ) ;
#50205 = CARTESIAN_POINT ( 'NONE',  ( -97.30629616937501680, 90.00000000000004263, 89.64281250086713726 ) ) ;
#50206 = VERTEX_POINT ( 'NONE', #16796 ) ;
#50208 = CARTESIAN_POINT ( 'NONE',  ( -92.35000000000005116, 91.52997821335253548, 81.55979166840097605 ) ) ;
#50207 = CARTESIAN_POINT ( 'NONE',  ( 96.32499999999998863, 87.70503267997126784, 81.40104166840096411 ) ) ;
#50209 = AXIS2_PLACEMENT_3D ( 'NONE', #62795, #21402, #5642 ) ;
#50210 = ORIENTED_EDGE ( 'NONE', *, *, #43581, .F. ) ;
#50211 = CARTESIAN_POINT ( 'NONE',  ( 92.69370383062498320, 90.00000000000002842, 84.08656250086716000 ) ) ;
#50212 = DIRECTION ( 'NONE',  ( -1.000000000000000000, 0.000000000000000000, 0.000000000000000000 ) ) ;
#50213 = CARTESIAN_POINT ( 'NONE',  ( -97.64995850909681963, 88.46999783186339528, 85.68729332542761767 ) ) ;
#50214 = EDGE_CURVE ( 'NONE', #22824, #24493, #45753, .T. ) ;
#50215 = DIRECTION ( 'NONE',  ( -1.000000000000000000, 0.000000000000000000, -0.000000000000000000 ) ) ;
#50216 = CARTESIAN_POINT ( 'NONE',  ( -22.67106064244953245, -113.6342314410295842, 5.500000000000000000 ) ) ;
#50217 = CARTESIAN_POINT ( 'NONE',  ( 0.000000000000000000, -1.732050807568877859, -1.752539433813135784E-17 ) ) ;
#50218 = ORIENTED_EDGE ( 'NONE', *, *, #54519, .F. ) ;
#50219 = CARTESIAN_POINT ( 'NONE',  ( 10.00000000000000000, 0.000000000000000000, 0.000000000000000000 ) ) ;
#50220 = LINE ( 'NONE', #3014, #46947 ) ;
#50221 = DIRECTION ( 'NONE',  ( -1.000000000000000000, 0.000000000000000000, 0.000000000000000000 ) ) ;
#50222 = EDGE_LOOP ( 'NONE', ( #28328, #4473, #32065, #63524 ) ) ;
#50223 = ADVANCED_FACE ( 'NONE', ( #56659 ), #5160, .T. ) ;
#50224 = VERTEX_POINT ( 'NONE', #10403 ) ;
#50225 = EDGE_CURVE ( 'NONE', #24060, #73031, #68675, .T. ) ;
#50226 = EDGE_CURVE ( 'NONE', #62552, #17492, #4047, .T. ) ;
#50227 = DIRECTION ( 'NONE',  ( -1.000000000000000000, 0.000000000000000000, 0.000000000000000000 ) ) ;
#50228 = CARTESIAN_POINT ( 'NONE',  ( -97.64999999978466860, 90.00002100773832581, 79.91868729552945183 ) ) ;
#50229 = FACE_OUTER_BOUND ( 'NONE', #51965, .T. ) ;
#50230 = ADVANCED_FACE ( 'NONE', ( #49870 ), #50243, .T. ) ;
#50231 = CARTESIAN_POINT ( 'NONE',  ( -96.15314808468747287, -208.0026889286704943, 79.53572916753381605 ) ) ;
#50232 = VERTEX_POINT ( 'NONE', #18262 ) ;
#50233 = MECHANICAL_DESIGN_GEOMETRIC_PRESENTATION_REPRESENTATION (  '', ( #68227 ), #56202 ) ;
#50234 = CARTESIAN_POINT ( 'NONE',  ( 96.32499999999998863, -212.2949673200287179, 81.32166666666667254 ) ) ;
#50235 = VERTEX_POINT ( 'NONE', #64141 ) ;
#50236 = AXIS2_PLACEMENT_3D ( 'NONE', #29374, #52316, #39940 ) ;
#50237 = VECTOR ( 'NONE', #23366, 1000.000000000000000 ) ;
#50238 = EDGE_CURVE ( 'NONE', #46961, #51872, #28038, .T. ) ;
#50239 = CARTESIAN_POINT ( 'NONE',  ( -92.34999999999999432, -211.5299782133524218, 77.64395833506762301 ) ) ;
#50240 = AXIS2_PLACEMENT_3D ( 'NONE', #56832, #5337, #35002 ) ;
#50241 = CARTESIAN_POINT ( 'NONE',  ( 93.84685191531248449, 91.99731107132950569, 77.47197916753380298 ) ) ;
#50242 = VECTOR ( 'NONE', #15876, 1000.000000000000000 ) ;
#50243 = CYLINDRICAL_SURFACE ( 'NONE', #64069, 31.99999999999999289 ) ;
#50244 = CARTESIAN_POINT ( 'NONE',  ( 11.99999999999999822, 0.000000000000000000, 0.000000000000000000 ) ) ;
#50245 = CARTESIAN_POINT ( 'NONE',  ( 10.00000000000000000, -4.992566952384716927, -37.16516213103282951 ) ) ;
#50246 = CYLINDRICAL_SURFACE ( 'NONE', #11250, 31.99999999999998579 ) ;
#50247 = DIRECTION ( 'NONE',  ( 0.000000000000000000, 0.000000000000000000, 1.000000000000000000 ) ) ;
#50248 = CARTESIAN_POINT ( 'NONE',  ( 97.64999999999999147, -209.9999999999999716, 84.60249999999999204 ) ) ;
#50249 = CARTESIAN_POINT ( 'NONE',  ( 96.32499999999998863, -212.2949673200287179, 83.22666666666665947 ) ) ;
#50250 = ADVANCED_FACE ( 'NONE', ( #285 ), #6977, .T. ) ;
#50251 = CARTESIAN_POINT ( 'NONE',  ( 0.000000000000000000, 64.81221759200417409, -50.23322058963276504 ) ) ;
#50252 = CARTESIAN_POINT ( 'NONE',  ( -97.64999999960633659, -209.9999706968024782, 82.45844277047601167 ) ) ;
#50253 = VECTOR ( 'NONE', #45666, 1000.000000000000000 ) ;
#50254 = VERTEX_POINT ( 'NONE', #52854 ) ;
#50255 = CARTESIAN_POINT ( 'NONE',  ( -96.15314808468752972, 91.99731107132950569, 82.55197916753380127 ) ) ;
#50256 = ADVANCED_FACE ( 'NONE', ( #11873 ), #6264, .T. ) ;
#50257 = EDGE_CURVE ( 'NONE', #11086, #20441, #41562, .T. ) ;
#50258 = DIRECTION ( 'NONE',  ( -1.000000000000000000, -0.000000000000000000, 0.000000000000000000 ) ) ;
#50259 = CIRCLE ( 'NONE', #7068, 31.99999999999998579 ) ;
#50260 = CIRCLE ( 'NONE', #10666, 77.49900000000002365 ) ;
#50261 = CIRCLE ( 'NONE', #37068, 32.00000000000000000 ) ;
#50262 = CARTESIAN_POINT ( 'NONE',  ( -10.21100092698785033, -95.54625877152835756, -2.500000000000000000 ) ) ;
#50263 = EDGE_CURVE ( 'NONE', #54483, #29284, #32858, .T. ) ;
#50264 = ORIENTED_EDGE ( 'NONE', *, *, #12889, .F. ) ;
#50265 = VECTOR ( 'NONE', #43824, 1000.000000000000227 ) ;
#50266 = DIRECTION ( 'NONE',  ( 0.000000000000000000, 0.000000000000000000, 1.000000000000000000 ) ) ;
#50267 = DIRECTION ( 'NONE',  ( 0.000000000000000000, 0.9945218953682742891, -0.1045284632676436315 ) ) ;
#50268 = CARTESIAN_POINT ( 'NONE',  ( 10.00000000000000000, -0.8261519478425671803, -77.49459641780887864 ) ) ;
#50269 = DIRECTION ( 'NONE',  ( 0.000000000000000000, 0.000000000000000000, -1.000000000000000000 ) ) ;
#50270 = CARTESIAN_POINT ( 'NONE',  ( 92.69370383062501162, -209.9999999999999716, 77.10156250086714635 ) ) ;
#50271 = ORIENTED_EDGE ( 'NONE', *, *, #25725, .F. ) ;
#50272 = ORIENTED_EDGE ( 'NONE', *, *, #12235, .T. ) ;
#50273 = CIRCLE ( 'NONE', #70716, 31.99999999999999645 ) ;
#50274 = CARTESIAN_POINT ( 'NONE',  ( 96.92110976540175216, -208.6943671794273030, 74.79348190356853365 ) ) ;
#50275 = CARTESIAN_POINT ( 'NONE',  ( 11.99999999999999822, 0.000000000000000000, 0.000000000000000000 ) ) ;
#50276 = CARTESIAN_POINT ( 'NONE',  ( -97.64999999947052345, 90.00003365185393989, 81.18829462297244959 ) ) ;
#50277 = DIRECTION ( 'NONE',  ( 0.000000000000000000, -0.6494480483301739993, -0.7604059656000391465 ) ) ;
#50278 = VECTOR ( 'NONE', #26071, 1000.000000000000000 ) ;
#50279 = DIRECTION ( 'NONE',  ( 1.000000000000000000, -0.000000000000000000, -0.000000000000000000 ) ) ;
#50280 = CARTESIAN_POINT ( 'NONE',  ( 97.64999999999997726, -208.4700217866474645, 89.73541666666666572 ) ) ;
#50281 = VECTOR ( 'NONE', #3168, 1000.000000000000000 ) ;
#50282 = AXIS2_PLACEMENT_3D ( 'NONE', #62406, #27038, #31942 ) ;
#50283 = ORIENTED_EDGE ( 'NONE', *, *, #13815, .F. ) ;
#50284 = CARTESIAN_POINT ( 'NONE',  ( 10.00000000000000000, -23.16143007188481207, 73.95703589263968070 ) ) ;
#50285 = ORIENTED_EDGE ( 'NONE', *, *, #38260, .F. ) ;
#50286 = EDGE_LOOP ( 'NONE', ( #63371, #6997, #45048, #43314 ) ) ;
#50287 = DIRECTION ( 'NONE',  ( 0.000000000000000000, 0.000000000000000000, -1.000000000000000000 ) ) ;
#50288 = AXIS2_PLACEMENT_3D ( 'NONE', #26666, #33045, #72884 ) ;
#50289 = LINE ( 'NONE', #34121, #10103 ) ;
#50290 = CIRCLE ( 'NONE', #44357, 31.99999999999998579 ) ;
#50291 = ORIENTED_EDGE ( 'NONE', *, *, #38950, .T. ) ;
#50292 = DIRECTION ( 'NONE',  ( 0.000000000000000000, -0.7071067811865535679, 0.7071067811865414665 ) ) ;
#50293 = CARTESIAN_POINT ( 'NONE',  ( 93.67500000000001137, -207.7050326799711968, 78.54354166840096241 ) ) ;
#50294 = CARTESIAN_POINT ( 'NONE',  ( 97.64999999999997726, 91.52997821335252127, 82.75041666666665208 ) ) ;
#50295 = EDGE_LOOP ( 'NONE', ( #25033, #25518, #54082, #37721 ) ) ;
#50296 = CYLINDRICAL_SURFACE ( 'NONE', #39543, 16.00000000000000000 ) ;
#50297 = ORIENTED_EDGE ( 'NONE', *, *, #48237, .T. ) ;
#50298 = ORIENTED_EDGE ( 'NONE', *, *, #40511, .T. ) ;
#50299 = FACE_OUTER_BOUND ( 'NONE', #30030, .T. ) ;
#50300 = CARTESIAN_POINT ( 'NONE',  ( -93.84685191531252713, 88.00268892867056536, 85.56822916753381492 ) ) ;
#50301 = CARTESIAN_POINT ( 'NONE',  ( 93.84685191531248449, 91.99731107132950569, 79.37697916753380412 ) ) ;
#50302 = ORIENTED_EDGE ( 'NONE', *, *, #11687, .T. ) ;
#50303 = DIRECTION ( 'NONE',  ( 2.628368902995175337E-16, 1.000000000000000000, 0.000000000000000000 ) ) ;
#50304 = LINE ( 'NONE', #33013, #4082 ) ;
#50305 = CIRCLE ( 'NONE', #5909, 31.99999999999998579 ) ;
#50306 = DIRECTION ( 'NONE',  ( 1.000000000000000000, 0.000000000000000000, 0.000000000000000000 ) ) ;
#50307 = EDGE_CURVE ( 'NONE', #25402, #17509, #31617, .T. ) ;
#50308 = DIRECTION ( 'NONE',  ( -1.000000000000000000, -0.000000000000000000, -0.000000000000000000 ) ) ;
#50309 = VERTEX_POINT ( 'NONE', #58119 ) ;
#50310 = DIRECTION ( 'NONE',  ( 0.000000000000000000, -0.8660254037844421493, -0.4999999999999939493 ) ) ;
#50311 = CIRCLE ( 'NONE', #70689, 31.99999999999998579 ) ;
#50313 = CARTESIAN_POINT ( 'NONE',  ( -94.99999999999997158, -212.6630814284392557, 80.91156250086714863 ) ) ;
#50312 = AXIS2_PLACEMENT_3D ( 'NONE', #61526, #54764, #20170 ) ;
#50314 = ORIENTED_EDGE ( 'NONE', *, *, #47800, .F. ) ;
#50315 = EDGE_CURVE ( 'NONE', #3906, #2716, #56867, .T. ) ;
#50316 = ORIENTED_EDGE ( 'NONE', *, *, #3578, .T. ) ;
#50317 = DIRECTION ( 'NONE',  ( -1.000000000000000000, 0.000000000000000000, 0.000000000000000000 ) ) ;
#50318 = VECTOR ( 'NONE', #52232, 1000.000000000000000 ) ;
#50319 = EDGE_CURVE ( 'NONE', #33300, #42737, #23537, .T. ) ;
#50320 = ADVANCED_FACE ( 'NONE', ( #41945 ), #70481, .F. ) ;
#50321 = ORIENTED_EDGE ( 'NONE', *, *, #10518, .T. ) ;
#50322 = CARTESIAN_POINT ( 'NONE',  ( 11.99999999999999822, -20.41045688087772092, -72.35160999960838524 ) ) ;
#50323 = VECTOR ( 'NONE', #16071, 999.9999999999998863 ) ;
#50324 = CARTESIAN_POINT ( 'NONE',  ( 92.34999999999999432, 90.00000000000002842, 88.17437500173430465 ) ) ;
#50325 = VERTEX_POINT ( 'NONE', #35918 ) ;
#50326 =( BOUNDED_CURVE ( )  B_SPLINE_CURVE ( 2, ( #2542, #55097, #59636, #14121, #24677, #70900, #25426 ),
 .UNSPECIFIED., .F., .F. ) 
 B_SPLINE_CURVE_WITH_KNOTS ( ( 3, 2, 2, 3 ),
 ( 0.6041666666666670737, 0.6111111111111116045, 0.6180555555555559133, 0.6250000000000003331 ),
 .UNSPECIFIED. ) 
 CURVE ( )  GEOMETRIC_REPRESENTATION_ITEM ( )  RATIONAL_B_SPLINE_CURVE ( ( 0.9999999999999914513, 0.8660254037844472563, 1.000000000000000000, 0.8660254037844387076, 1.000000000000000000, 0.8660254037844322683, 1.000000000000006439 ) ) 
 REPRESENTATION_ITEM ( '' )  );
#50327 = CARTESIAN_POINT ( 'NONE',  ( -97.30629616937497417, -211.3315407142195852, 75.09072916753382287 ) ) ;
#50328 = ORIENTED_EDGE ( 'NONE', *, *, #55997, .T. ) ;
#50329 = DIRECTION ( 'NONE',  ( 0.000000000000000000, 0.4067366430757887730, -0.9135454576426059736 ) ) ;
#50330 = DIRECTION ( 'NONE',  ( 0.000000000000000000, 0.3090169943749411785, 0.9510565162951556406 ) ) ;
#50331 = DIRECTION ( 'NONE',  ( 1.000000000000000000, 0.000000000000000000, 0.000000000000000000 ) ) ;
#50332 = FACE_OUTER_BOUND ( 'NONE', #61048, .T. ) ;
#50333 = FACE_OUTER_BOUND ( 'NONE', #63034, .T. ) ;
#50334 = DIRECTION ( 'NONE',  ( -0.000000000000000000, -0.000000000000000000, -1.000000000000000000 ) ) ;
#50335 = LINE ( 'NONE', #49956, #18845 ) ;
#50336 = CARTESIAN_POINT ( 'NONE',  ( 10.05638427806949586, -98.76043467366159234, -2.500000000000000000 ) ) ;
#50337 = CARTESIAN_POINT ( 'NONE',  ( 94.99999999999998579, 86.94004357329502852, 81.34812500173430294 ) ) ;
#50338 = CARTESIAN_POINT ( 'NONE',  ( 4.999999999999999112, -16.65560815589383381, -38.55633173627028754 ) ) ;
#50339 = EDGE_CURVE ( 'NONE', #688, #40404, #43670, .T. ) ;
#50340 = CYLINDRICAL_SURFACE ( 'NONE', #39274, 37.49900000000000233 ) ;
#50341 = CARTESIAN_POINT ( 'NONE',  ( 10.00000000000000000, -75.54627589209931671, -17.28742895386164591 ) ) ;
#50342 = CARTESIAN_POINT ( 'NONE',  ( 93.67499999999999716, 87.70503267997126784, 77.40583333333331950 ) ) ;
#50343 = CARTESIAN_POINT ( 'NONE',  ( 15.00000000000000000, -4.261787119645322974, -26.19803753235774835 ) ) ;
#50344 = AXIS2_PLACEMENT_3D ( 'NONE', #7609, #13971, #65138 ) ;
#50345 = CARTESIAN_POINT ( 'NONE',  ( 11.59999999999999964, -0.8299999999999999600, -1.199999999999999956 ) ) ;
#50346 = AXIS2_PLACEMENT_3D ( 'NONE', #15898, #16638, #56509 ) ;
#50347 = AXIS2_PLACEMENT_3D ( 'NONE', #70968, #71704, #59336 ) ;
#50348 = CARTESIAN_POINT ( 'NONE',  ( 22.08297821871651578, -111.8242998470044540, -2.500000000000000000 ) ) ;
#50349 = VECTOR ( 'NONE', #30893, 1000.000000000000000 ) ;
#50350 = DIRECTION ( 'NONE',  ( -1.000000000000000000, 0.000000000000000000, 0.000000000000000000 ) ) ;
#50351 = EDGE_CURVE ( 'NONE', #28874, #70060, #71325, .T. ) ;
#50352 = ADVANCED_FACE ( 'NONE', ( #23911 ), #69764, .T. ) ;
#50353 = CARTESIAN_POINT ( 'NONE',  ( 10.00000000000000000, 0.000000000000000000, 0.000000000000000000 ) ) ;
#50354 = CARTESIAN_POINT ( 'NONE',  ( -92.34999999999999432, -209.9999999999999716, 84.60249999999999204 ) ) ;
#50355 = AXIS2_PLACEMENT_3D ( 'NONE', #54438, #26598, #65726 ) ;
#50356 = CARTESIAN_POINT ( 'NONE',  ( -6.880223345695647197, -142.5202692415819854, 5.500000000000000000 ) ) ;
#50357 = CARTESIAN_POINT ( 'NONE',  ( 0.000000000000000000, 12.24744871391588852, 2.500000000000003553 ) ) ;
#50358 = CARTESIAN_POINT ( 'NONE',  ( 10.00000000000000000, -25.88420570971419821, 27.13269053701087330 ) ) ;
#50359 = CARTESIAN_POINT ( 'NONE',  ( -23.97194136764370498, -131.3950000906648938, 5.500000000000000000 ) ) ;
#50360 = CARTESIAN_POINT ( 'NONE',  ( 0.000000000000000000, -79.10210256391353312, -21.60688246758668640 ) ) ;
#50361 = AXIS2_PLACEMENT_3D ( 'NONE', #33391, #4870, #22131 ) ;
#50362 = AXIS2_PLACEMENT_3D ( 'NONE', #52816, #51321, #74255 ) ;
#50363 = VECTOR ( 'NONE', #11851, 1000.000000000000000 ) ;
#50364 = CARTESIAN_POINT ( 'NONE',  ( 93.84685191531251292, -211.9973110713294489, 88.63739583420048973 ) ) ;
#50365 = ORIENTED_EDGE ( 'NONE', *, *, #23544, .T. ) ;
#50366 = CIRCLE ( 'NONE', #38352, 77.49899999999998101 ) ;
#50367 = ORIENTED_EDGE ( 'NONE', *, *, #35146, .T. ) ;
#50368 = VECTOR ( 'NONE', #42420, 1000.000000000000000 ) ;
#50369 = DIRECTION ( 'NONE',  ( -0.000000000000000000, -0.000000000000000000, -1.000000000000000000 ) ) ;
#50370 = ORIENTED_EDGE ( 'NONE', *, *, #37379, .T. ) ;
#50371 = CARTESIAN_POINT ( 'NONE',  ( 0.000000000000000000, -22.64427369931148348, -30.00120703465229965 ) ) ;
#50372 = CARTESIAN_POINT ( 'NONE',  ( 96.15314808468748708, -208.0026889286704943, 77.36614583420046642 ) ) ;
#50373 = ORIENTED_EDGE ( 'NONE', *, *, #47963, .F. ) ;
#50374 = CARTESIAN_POINT ( 'NONE',  ( 95.00000000000000000, -212.6630814284392557, 83.61031250086716682 ) ) ;
#50375 = ORIENTED_EDGE ( 'NONE', *, *, #1804, .T. ) ;
#50376 = ORIENTED_EDGE ( 'NONE', *, *, #28912, .F. ) ;
#50377 = CARTESIAN_POINT ( 'NONE',  ( 2.500000000000034639, 90.00000000000000000, -90.00000000000000000 ) ) ;
#50378 = VERTEX_POINT ( 'NONE', #58483 ) ;
#50379 = DIRECTION ( 'NONE',  ( 0.2306669878475637314, 0.9730327541852493711, 0.000000000000000000 ) ) ;
#50380 = EDGE_LOOP ( 'NONE', ( #39607, #52434, #56771, #46356 ) ) ;
#50381 = DIRECTION ( 'NONE',  ( 1.000000000000000000, 0.000000000000000000, 0.000000000000000000 ) ) ;
#50382 = CARTESIAN_POINT ( 'NONE',  ( 95.00000000000000000, -206.9400435732949575, 88.65062500173431204 ) ) ;
#50383 = ORIENTED_EDGE ( 'NONE', *, *, #49960, .T. ) ;
#50384 = CARTESIAN_POINT ( 'NONE',  ( 10.00000000000000000, 0.000000000000000000, 0.000000000000000000 ) ) ;
#50385 = ORIENTED_EDGE ( 'NONE', *, *, #2441, .T. ) ;
#50386 = CYLINDRICAL_SURFACE ( 'NONE', #34826, 77.49899999999999523 ) ;
#50387 = CONICAL_SURFACE ( 'NONE', #26352, 2.649999999999999467, 1.029744258676654312 ) ;
#50388 = PRODUCT_RELATED_PRODUCT_CATEGORY ( 'part', '', ( #27159 ) ) ;
#50389 = VERTEX_POINT ( 'NONE', #30277 ) ;
#50390 = CIRCLE ( 'NONE', #27601, 31.99999999999999289 ) ;
#50391 = EDGE_CURVE ( 'NONE', #21912, #58096, #64503, .T. ) ;
#50392 = AXIS2_PLACEMENT_3D ( 'NONE', #36558, #3128, #2406 ) ;
#50393 = ORIENTED_EDGE ( 'NONE', *, *, #60274, .F. ) ;
#50394 = ORIENTED_EDGE ( 'NONE', *, *, #43127, .F. ) ;
#50395 = CARTESIAN_POINT ( 'NONE',  ( 92.69370383062501162, -211.3315407142195852, 76.36072916753381890 ) ) ;
#50396 = DIRECTION ( 'NONE',  ( -1.000000000000000000, -0.000000000000000000, -0.000000000000000000 ) ) ;
#50397 = VERTEX_POINT ( 'NONE', #24645 ) ;
#50398 = ORIENTED_EDGE ( 'NONE', *, *, #61567, .F. ) ;
#50399 = ADVANCED_FACE ( 'NONE', ( #17524 ), #47576, .T. ) ;
#50400 = AXIS2_PLACEMENT_3D ( 'NONE', #73566, #10419, #61569 ) ;
#50401 = ORIENTED_EDGE ( 'NONE', *, *, #47599, .T. ) ;
#50402 = CARTESIAN_POINT ( 'NONE',  ( 10.00000000000000000, 32.34446384429971744, 26.79245525562727082 ) ) ;
#50403 = DIRECTION ( 'NONE',  ( 0.000000000000000000, 0.000000000000000000, 1.000000000000000000 ) ) ;
#50404 = ADVANCED_FACE ( 'NONE', ( #51740 ), #40456, .F. ) ;
#50405 = CARTESIAN_POINT ( 'NONE',  ( -92.35000000000005116, 88.47002178664754979, 89.62958333333332916 ) ) ;
#50406 = ORIENTED_EDGE ( 'NONE', *, *, #70682, .F. ) ;
#50407 = CARTESIAN_POINT ( 'NONE',  ( 92.69370383062498320, 91.33154071421968467, 78.15989583420048348 ) ) ;
#50408 = VERTEX_POINT ( 'NONE', #3225 ) ;
#50409 = DIRECTION ( 'NONE',  ( -1.000000000000000000, -0.000000000000000000, -0.000000000000000000 ) ) ;
#50410 = CARTESIAN_POINT ( 'NONE',  ( -94.99999999999997158, -207.3369185715606307, 88.84906250086713442 ) ) ;
#50412 = VERTEX_POINT ( 'NONE', #8472 ) ;
#50411 = ADVANCED_FACE ( 'NONE', ( #20851 ), #60355, .F. ) ;
#50413 = DIRECTION ( 'NONE',  ( 0.2867529058022035837, -0.9580045777625452175, 0.000000000000000000 ) ) ;
#50414 = FACE_OUTER_BOUND ( 'NONE', #22101, .T. ) ;
#50415 = FACE_OUTER_BOUND ( 'NONE', #67776, .T. ) ;
#50416 = CARTESIAN_POINT ( 'NONE',  ( -92.69370383062498320, -208.6684592857803295, 78.58322916753381548 ) ) ;
#50417 = AXIS2_PLACEMENT_3D ( 'NONE', #37861, #61164, #15283 ) ;
#50418 = CARTESIAN_POINT ( 'NONE',  ( 10.00000000000000000, 0.000000000000000000, 0.000000000000000000 ) ) ;
#50419 = LINE ( 'NONE', #44799, #4346 ) ;
#50420 = AXIS2_PLACEMENT_3D ( 'NONE', #39084, #16894, #34538 ) ;
#50421 = DIRECTION ( 'NONE',  ( -1.000000000000000000, 0.000000000000000000, 0.000000000000000000 ) ) ;
#50422 = ORIENTED_EDGE ( 'NONE', *, *, #13414, .F. ) ;
#50423 = CIRCLE ( 'NONE', #70807, 12.49999999999999645 ) ;
#50424 = CIRCLE ( 'NONE', #56457, 16.00000000000000355 ) ;
#50425 = ORIENTED_EDGE ( 'NONE', *, *, #71604, .F. ) ;
#50426 = DIRECTION ( 'NONE',  ( -1.000000000000000000, -0.000000000000000000, -0.000000000000000000 ) ) ;
#50427 = CIRCLE ( 'NONE', #28811, 31.99999999999998579 ) ;
#50428 = VECTOR ( 'NONE', #3882, 1000.000000000000000 ) ;
#50429 = DIRECTION ( 'NONE',  ( 0.000000000000000000, 0.000000000000000000, 1.000000000000000000 ) ) ;
#50430 = EDGE_CURVE ( 'NONE', #70995, #19678, #38935, .T. ) ;
#50431 = PLANE ( 'NONE',  #16346 ) ;
#50432 = EDGE_CURVE ( 'NONE', #69505, #73572, #43445, .T. ) ;
#50433 = CARTESIAN_POINT ( 'NONE',  ( -95.00000000000002842, 87.33691857156074434, 80.27656250086714351 ) ) ;
#50434 = DIRECTION ( 'NONE',  ( -1.000000000000000000, 0.000000000000000000, 0.000000000000000000 ) ) ;
#50435 = DIRECTION ( 'NONE',  ( -1.000000000000000000, 0.000000000000000000, 0.000000000000000000 ) ) ;
#50436 = EDGE_LOOP ( 'NONE', ( #4643, #55497, #54669, #51226 ) ) ;
#50437 = DIRECTION ( 'NONE',  ( -1.000000000000000000, -0.000000000000000000, -0.000000000000000000 ) ) ;
#50438 = LINE ( 'NONE', #67362, #8835 ) ;
#50439 = PLANE ( 'NONE',  #52633 ) ;
#50440 = ADVANCED_FACE ( 'NONE', ( #48685 ), #2506, .T. ) ;
#50441 = LINE ( 'NONE', #66003, #34628 ) ;
#50442 = CARTESIAN_POINT ( 'NONE',  ( 6.938893903907228378E-15, 0.000000000000000000, -15.77977592589476608 ) ) ;
#50443 = CARTESIAN_POINT ( 'NONE',  ( 97.65000000000000568, -208.4700217866474645, 88.54479166840097548 ) ) ;
#50444 = CARTESIAN_POINT ( 'NONE',  ( -93.84685191531247028, -211.9973110713294489, 77.94822916753382458 ) ) ;
#50445 = CARTESIAN_POINT ( 'NONE',  ( 0.000000000000000000, -26.01480285779785362, -70.53064760720343429 ) ) ;
#50446 = EDGE_LOOP ( 'NONE', ( #38503, #3584, #65737, #155 ) ) ;
#50447 = LINE ( 'NONE', #66279, #19090 ) ;
#50448 = DIRECTION ( 'NONE',  ( 1.000000000000000000, 0.000000000000000000, -0.000000000000000000 ) ) ;
#50449 = DIRECTION ( 'NONE',  ( -1.000000000000000000, -0.000000000000000000, -0.000000000000000000 ) ) ;
#50450 = VERTEX_POINT ( 'NONE', #2861 ) ;
#50451 = CARTESIAN_POINT ( 'NONE',  ( 10.00000000000000000, 77.19088730480534366, -6.903761155836915187 ) ) ;
#50452 = AXIS2_PLACEMENT_3D ( 'NONE', #8178, #52941, #31104 ) ;
#50453 = DIRECTION ( 'NONE',  ( 0.000000000000000000, 0.6494480483301793283, 0.7604059656000345946 ) ) ;
#50454 = CIRCLE ( 'NONE', #18050, 82.00000000000000000 ) ;
#50455 = UNCERTAINTY_MEASURE_WITH_UNIT (LENGTH_MEASURE( 1.000000000000000082E-05 ), #48956, 'distance_accuracy_value', 'NONE');
#50456 = AXIS2_PLACEMENT_3D ( 'NONE', #7895, #24452, #65428 ) ;
#50457 = CARTESIAN_POINT ( 'NONE',  ( 11.99999999999999822, 0.000000000000000000, 0.000000000000000000 ) ) ;
#50458 = EDGE_LOOP ( 'NONE', ( #9881, #5759, #12103, #63716 ) ) ;
#50459 = CARTESIAN_POINT ( 'NONE',  ( 11.99999999999999822, 0.8261519478441983200, -77.49459641780885022 ) ) ;
#50460 = DIRECTION ( 'NONE',  ( 0.000000000000000000, 0.8090169943749487835, -0.5877852522924713607 ) ) ;
#50461 = VERTEX_POINT ( 'NONE', #36661 ) ;
#50462 = CARTESIAN_POINT ( 'NONE',  ( 95.00000000000000000, -207.3369185715606307, 87.57906250086713840 ) ) ;
#50463 = CARTESIAN_POINT ( 'NONE',  ( 92.34999999999992326, -208.4700217866474929, 86.13708333333332234 ) ) ;
#50464 = VERTEX_POINT ( 'NONE', #25393 ) ;
#50465 = EDGE_CURVE ( 'NONE', #34383, #64804, #25755, .T. ) ;
#50466 = DIRECTION ( 'NONE',  ( 1.000000000000000000, 0.000000000000000000, 0.000000000000000000 ) ) ;
#50467 = VECTOR ( 'NONE', #52091, 1000.000000000000000 ) ;
#50468 = ORIENTED_EDGE ( 'NONE', *, *, #63771, .F. ) ;
#50469 = DIRECTION ( 'NONE',  ( -0.7071067811865479058, 0.000000000000000000, 0.7071067811865472397 ) ) ;
#50470 = VERTEX_POINT ( 'NONE', #49426 ) ;
#50471 = CIRCLE ( 'NONE', #26490, 77.49899999999999523 ) ;
#50472 = FACE_OUTER_BOUND ( 'NONE', #73873, .T. ) ;
#50473 = ORIENTED_EDGE ( 'NONE', *, *, #31999, .F. ) ;
#50474 = ORIENTED_EDGE ( 'NONE', *, *, #44597, .F. ) ;
#50475 = EDGE_CURVE ( 'NONE', #31594, #1097, #20104, .T. ) ;
#50476 = CIRCLE ( 'NONE', #37297, 31.99999999999999289 ) ;
#50477 = ORIENTED_EDGE ( 'NONE', *, *, #32771, .F. ) ;
#50478 = LINE ( 'NONE', #67021, #14332 ) ;
#50479 = EDGE_CURVE ( 'NONE', #5506, #58503, #65999, .T. ) ;
#50480 = ORIENTED_EDGE ( 'NONE', *, *, #9020, .T. ) ;
#50481 = VERTEX_POINT ( 'NONE', #64881 ) ;
#50482 = CARTESIAN_POINT ( 'NONE',  ( 97.30629616937498838, 88.66845928578037217, 77.36614583420048064 ) ) ;
#50483 = DIRECTION ( 'NONE',  ( -1.000000000000000000, -0.000000000000000000, -0.000000000000000000 ) ) ;
#50484 = CARTESIAN_POINT ( 'NONE',  ( 14.59956846177685996, -138.4757300459248484, 5.500000000000000000 ) ) ;
#50485 = ORIENTED_EDGE ( 'NONE', *, *, #58819, .F. ) ;
#50486 = ADVANCED_FACE ( 'NONE', ( #13359 ), #60721, .F. ) ;
#50487 = ORIENTED_EDGE ( 'NONE', *, *, #68202, .F. ) ;
#50488 = VERTEX_POINT ( 'NONE', #66363 ) ;
#50489 = CARTESIAN_POINT ( 'NONE',  ( 93.84685191531248449, 88.00268892867053694, 87.84364583420047268 ) ) ;
#50490 = ORIENTED_EDGE ( 'NONE', *, *, #49987, .T. ) ;
#50491 = CARTESIAN_POINT ( 'NONE',  ( 97.30629616937498838, -209.9999999999999716, 84.88031250086713442 ) ) ;
#50492 = DIRECTION ( 'NONE',  ( -1.000000000000000000, -0.000000000000000000, -0.000000000000000000 ) ) ;
#50493 = DIRECTION ( 'NONE',  ( -1.000000000000000000, -0.000000000000000000, 0.000000000000000000 ) ) ;
#50494 = LINE ( 'NONE', #39228, #7719 ) ;
#50495 = DIRECTION ( 'NONE',  ( 0.000000000000000000, 0.3826834323650841752, 0.9238795325112891810 ) ) ;
#50496 = DIRECTION ( 'NONE',  ( -1.000000000000000000, -0.000000000000000000, 0.000000000000000000 ) ) ;
#50497 = LINE ( 'NONE', #62160, #36018 ) ;
#50498 = CARTESIAN_POINT ( 'NONE',  ( -92.69370383062498320, -208.6684592857803011, 87.47322916753381605 ) ) ;
#50499 = CARTESIAN_POINT ( 'NONE',  ( -95.00000000000002842, 92.66308142843932671, 85.83281250086714920 ) ) ;
#50500 = ORIENTED_EDGE ( 'NONE', *, *, #17080, .F. ) ;
#50502 = CARTESIAN_POINT ( 'NONE',  ( -93.84685191531252713, 88.00268892867056536, 85.40947916753380298 ) ) ;
#50501 = CARTESIAN_POINT ( 'NONE',  ( 92.69370383062498320, 88.66845928578037217, 86.52072916753381548 ) ) ;
#50503 = ORIENTED_EDGE ( 'NONE', *, *, #3448, .T. ) ;
#50504 = CARTESIAN_POINT ( 'NONE',  ( 0.000000000000000000, -10.41901085202050581, -40.68715046381939970 ) ) ;
#50505 = EDGE_CURVE ( 'NONE', #14126, #52133, #7703, .T. ) ;
#50506 = CARTESIAN_POINT ( 'NONE',  ( -97.64999999999996305, -211.5299782133524218, 80.60729166840097548 ) ) ;
#50507 = DIRECTION ( 'NONE',  ( -1.000000000000000000, 0.000000000000000000, -0.000000000000000000 ) ) ;
#50508 = DIRECTION ( 'NONE',  ( -1.000000000000000000, -0.000000000000000000, -0.000000000000000000 ) ) ;
#50509 = LINE ( 'NONE', #67058, #17039 ) ;
#50510 = CARTESIAN_POINT ( 'NONE',  ( 92.35000000000000853, -208.4700217866474645, 82.32708333333334849 ) ) ;
#50511 = DIRECTION ( 'NONE',  ( 0.000000000000000000, 0.6494480483301793283, 0.7604059656000345946 ) ) ;
#50512 = DIRECTION ( 'NONE',  ( -1.000000000000000000, -0.000000000000000000, 0.000000000000000000 ) ) ;
#50513 = CIRCLE ( 'NONE', #49324, 2.649999999999985700 ) ;
#50514 = EDGE_LOOP ( 'NONE', ( #9808, #62305 ) ) ;
#50515 = ORIENTED_EDGE ( 'NONE', *, *, #41669, .F. ) ;
#50516 = CARTESIAN_POINT ( 'NONE',  ( -92.35000000000005116, 88.47002178664754979, 80.73958333333332860 ) ) ;
#50517 = EDGE_CURVE ( 'NONE', #48877, #34480, #42679, .T. ) ;
#50518 = DIRECTION ( 'NONE',  ( 0.000000000000000000, 0.000000000000000000, -1.000000000000000000 ) ) ;
#50519 = ADVANCED_FACE ( 'NONE', ( #9201, #32120 ), #55062, .T. ) ;
#50520 = CARTESIAN_POINT ( 'NONE',  ( -93.67500000000003979, 87.70503267997129626, 78.78166666666666629 ) ) ;
#50521 = CARTESIAN_POINT ( 'NONE',  ( 10.00000000000000000, 30.00120703465236716, -22.64427369931138756 ) ) ;
#50522 = FACE_OUTER_BOUND ( 'NONE', #21084, .T. ) ;
#50523 = DIRECTION ( 'NONE',  ( 0.000000000000000000, 0.000000000000000000, -1.000000000000000000 ) ) ;
#50524 = LINE ( 'NONE', #27961, #8497 ) ;
#50525 = DIRECTION ( 'NONE',  ( -1.000000000000000000, 0.000000000000000000, 0.000000000000000000 ) ) ;
#50526 = B_SPLINE_CURVE_WITH_KNOTS ( 'NONE', 3,
 ( #69945, #22620, #29712, #62489 ),
 .UNSPECIFIED., .F., .F.,
 ( 4, 4 ),
 ( 2.380735200870747991E-07, 0.002921158011986710323 ),
 .UNSPECIFIED. ) ;
#50527 = EDGE_CURVE ( 'NONE', #65293, #28744, #61751, .T. ) ;
#50528 = ORIENTED_EDGE ( 'NONE', *, *, #21034, .F. ) ;
#50529 = CARTESIAN_POINT ( 'NONE',  ( -97.30629616937501680, 88.66845928578038638, 83.34572916753380412 ) ) ;
#50530 = AXIS2_PLACEMENT_3D ( 'NONE', #58661, #1202, #1930 ) ;
#50531 = LINE ( 'NONE', #20846, #39158 ) ;
#50532 = CARTESIAN_POINT ( 'NONE',  ( 95.00000000000000000, -209.9999999999999716, 90.00000000000000000 ) ) ;
#50533 = AXIS2_PLACEMENT_3D ( 'NONE', #6057, #6770, #11657 ) ;
#50534 = LINE ( 'NONE', #11063, #41820 ) ;
#50535 = DIRECTION ( 'NONE',  ( -1.000000000000000000, 0.000000000000000000, 0.000000000000000000 ) ) ;
#50536 = CARTESIAN_POINT ( 'NONE',  ( 92.35000000000000853, -209.9999999999999716, 90.00000000000000000 ) ) ;
#50537 = CARTESIAN_POINT ( 'NONE',  ( 92.35000000002544596, 90.00000000000008527, -74.99999999999992895 ) ) ;
#50538 = VECTOR ( 'NONE', #28906, 1000.000000000000000 ) ;
#50539 =( BOUNDED_CURVE ( )  B_SPLINE_CURVE ( 2, ( #46260, #41717, #24430, #7876, #37202, #42471, #25535 ),
 .UNSPECIFIED., .F., .F. ) 
 B_SPLINE_CURVE_WITH_KNOTS ( ( 3, 2, 2, 3 ),
 ( 0.2499999999999995837, 0.2569444444444442532, 0.2638888888888890061, 0.2708333333333337034 ),
 .UNSPECIFIED. ) 
 CURVE ( )  GEOMETRIC_REPRESENTATION_ITEM ( )  RATIONAL_B_SPLINE_CURVE ( ( 1.000000000000007994, 0.8660254037844307140, 1.000000000000000000, 0.8660254037844387076, 1.000000000000000000, 0.8660254037844311581, 1.000000000000007550 ) ) 
 REPRESENTATION_ITEM ( '' )  );
#50540 = CARTESIAN_POINT ( 'NONE',  ( 92.69370383062498320, 90.00000000000002842, 81.54656250086715374 ) ) ;
#50541 = CARTESIAN_POINT ( 'NONE',  ( -92.69370383062498320, -209.9999999999999716, 81.22906250086715829 ) ) ;
#50542 = CARTESIAN_POINT ( 'NONE',  ( -92.35000000000005116, 91.52997821335253548, 84.73479166840094479 ) ) ;
#50543 = ORIENTED_EDGE ( 'NONE', *, *, #53137, .T. ) ;
#50544 = DIRECTION ( 'NONE',  ( 0.000000000000000000, 0.000000000000000000, 1.000000000000000000 ) ) ;
#50545 = CARTESIAN_POINT ( 'NONE',  ( -89.17737905728745318, -39.70432723693717492, 5.500000000000000000 ) ) ;
#50546 = CARTESIAN_POINT ( 'NONE',  ( 92.34999999999999432, 90.00000000000002842, 85.63437500173431260 ) ) ;
#50547 = CARTESIAN_POINT ( 'NONE',  ( -95.00000000000002842, 87.33691857156074434, 79.16531250086715943 ) ) ;
#50548 = CARTESIAN_POINT ( 'NONE',  ( 95.00000000000000000, -207.3369185715606307, 80.59406250086715318 ) ) ;
#50549 = ORIENTED_EDGE ( 'NONE', *, *, #30732, .F. ) ;
#50550 = LINE ( 'NONE', #66385, #11840 ) ;
#50551 = ORIENTED_EDGE ( 'NONE', *, *, #33273, .F. ) ;
#50552 = CARTESIAN_POINT ( 'NONE',  ( 11.99999999999999822, -64.81221759200380461, 50.23322058963326242 ) ) ;
#50553 = VERTEX_POINT ( 'NONE', #59990 ) ;
#50554 = EDGE_CURVE ( 'NONE', #74050, #47235, #40117, .T. ) ;
#50555 = AXIS2_PLACEMENT_3D ( 'NONE', #3200, #65972, #37398 ) ;
#50557 = AXIS2_PLACEMENT_3D ( 'NONE', #18714, #64589, #41292 ) ;
#50556 = CARTESIAN_POINT ( 'NONE',  ( 0.000000000000000000, -33.79645857604501913, -16.45098606841161626 ) ) ;
#50558 = ORIENTED_EDGE ( 'NONE', *, *, #65354, .F. ) ;
#50559 = EDGE_LOOP ( 'NONE', ( #27902, #29310, #73853, #33267 ) ) ;
#50560 = EDGE_CURVE ( 'NONE', #12079, #1966, #42319, .T. ) ;
#50561 = VERTEX_POINT ( 'NONE', #8093 ) ;
#50562 = CARTESIAN_POINT ( 'NONE',  ( 4.999999999999999112, 9.188173127307294408, 40.98264845739752360 ) ) ;
#50563 = ADVANCED_FACE ( 'NONE', ( #31012 ), #10685, .F. ) ;
#50564 = ORIENTED_EDGE ( 'NONE', *, *, #73040, .T. ) ;
#50565 = DIRECTION ( 'NONE',  ( 0.000000000000000000, 0.9238795325112851842, 0.3826834323650938341 ) ) ;
#50566 = CARTESIAN_POINT ( 'NONE',  ( 94.99999999999998579, 87.33691857156068750, 85.51531250086713953 ) ) ;
#50567 = LINE ( 'NONE', #46702, #35758 ) ;
#50568 = CARTESIAN_POINT ( 'NONE',  ( 92.35000000000000853, -209.9999999999999716, 77.93499999999998806 ) ) ;
#50569 = EDGE_LOOP ( 'NONE', ( #11918, #16548, #40822, #23953 ) ) ;
#50570 = EDGE_CURVE ( 'NONE', #29646, #36497, #31681, .T. ) ;
#50571 = ORIENTED_EDGE ( 'NONE', *, *, #70274, .F. ) ;
#50572 = ORIENTED_EDGE ( 'NONE', *, *, #51999, .F. ) ;
#50573 = VERTEX_POINT ( 'NONE', #27217 ) ;
#50574 = DIRECTION ( 'NONE',  ( 1.000000000000000000, 0.000000000000000000, 0.000000000000000000 ) ) ;
#50575 = VECTOR ( 'NONE', #20374, 1000.000000000000114 ) ;
#50576 = CIRCLE ( 'NONE', #198, 15.99999999999999467 ) ;
#50577 = CARTESIAN_POINT ( 'NONE',  ( 0.000000000000000000, 0.000000000000000000, 0.000000000000000000 ) ) ;
#50578 = CYLINDRICAL_SURFACE ( 'NONE', #55625, 2.649999999999985700 ) ;
#50579 = AXIS2_PLACEMENT_3D ( 'NONE', #9948, #38532, #61468 ) ;
#50580 = CARTESIAN_POINT ( 'NONE',  ( 95.00000000000000000, -209.9999999999999716, 90.00000000000000000 ) ) ;
#50581 = CARTESIAN_POINT ( 'NONE',  ( 94.99999999999998579, 90.00000000000002842, 90.00000000000000000 ) ) ;
#50582 = CARTESIAN_POINT ( 'NONE',  ( -96.32499999999996021, -212.2949673200287179, 83.83520833506763381 ) ) ;
#50583 = ORIENTED_EDGE ( 'NONE', *, *, #47218, .F. ) ;
#50584 = CARTESIAN_POINT ( 'NONE',  ( -94.99999999999997158, -206.9400435732949575, 83.57062500173429953 ) ) ;
#50585 = EDGE_LOOP ( 'NONE', ( #49861, #47126, #41641, #32612 ) ) ;
#50586 = DIRECTION ( 'NONE',  ( -1.000000000000000000, 0.000000000000000000, -0.000000000000000000 ) ) ;
#50587 = EDGE_LOOP ( 'NONE', ( #63743, #38161, #2349, #8494 ) ) ;
#50589 = CARTESIAN_POINT ( 'NONE',  ( -97.65000000000001990, 91.52997821335253548, 83.67645833506762187 ) ) ;
#50588 = CARTESIAN_POINT ( 'NONE',  ( 97.64999999999999147, 90.00000000000002842, 83.41187500173430180 ) ) ;
#50590 = VECTOR ( 'NONE', #9024, 1000.000000000000000 ) ;
#50591 = ORIENTED_EDGE ( 'NONE', *, *, #63390, .F. ) ;
#50592 = CARTESIAN_POINT ( 'NONE',  ( 97.30629616937498838, 88.66845928578037217, 82.44614583420049314 ) ) ;
#50593 = EDGE_CURVE ( 'NONE', #9802, #14986, #40013, .T. ) ;
#50594 = LINE ( 'NONE', #73148, #25870 ) ;
#50595 = DIRECTION ( 'NONE',  ( 0.000000000000000000, 0.000000000000000000, 1.000000000000000000 ) ) ;
#50596 = DIRECTION ( 'NONE',  ( -1.000000000000000000, 0.000000000000000000, 0.000000000000000000 ) ) ;
#50597 = CARTESIAN_POINT ( 'NONE',  ( 92.34999999999999432, 90.00000000000002842, 88.09499999999999886 ) ) ;
#50598 = ORIENTED_EDGE ( 'NONE', *, *, #6117, .T. ) ;
#50599 = DIRECTION ( 'NONE',  ( 0.000000000000000000, 0.000000000000000000, 1.000000000000000000 ) ) ;
#50600 = CARTESIAN_POINT ( 'NONE',  ( -93.67500000000003979, 87.70503267997129626, 82.67104166840096013 ) ) ;
#50601 = LINE ( 'NONE', #34804, #43200 ) ;
#50602 = VERTEX_POINT ( 'NONE', #39269 ) ;
#50603 = ORIENTED_EDGE ( 'NONE', *, *, #235, .T. ) ;
#50604 = ADVANCED_FACE ( 'NONE', ( #56937 ), #67459, .T. ) ;
#50605 = PRODUCT ( 'coupling', 'coupling', '', ( #67417 ) ) ;
#50606 = CARTESIAN_POINT ( 'NONE',  ( 0.000000000000000000, -33.17418723428294669, -17.67226234102862747 ) ) ;
#50607 = EDGE_CURVE ( 'NONE', #10745, #9630, #67755, .T. ) ;
#50608 = CARTESIAN_POINT ( 'NONE',  ( -92.35000000000003695, 89.99999990163421160, 80.23687499810812085 ) ) ;
#50609 = CARTESIAN_POINT ( 'NONE',  ( -93.84685191531247028, -211.9973110713294489, 81.12322916753382174 ) ) ;
#50610 = EDGE_LOOP ( 'NONE', ( #29011, #73010 ) ) ;
#50611 = CARTESIAN_POINT ( 'NONE',  ( -95.00000000000002842, 87.33691857156074434, 88.53156250086713897 ) ) ;
#50612 = VERTEX_POINT ( 'NONE', #56571 ) ;
#50613 = CIRCLE ( 'NONE', #66250, 77.49900000000000944 ) ;
#50614 = DIRECTION ( 'NONE',  ( 0.000000000000000000, -1.776356839400250465E-15, -1.000000000000000000 ) ) ;
#50615 = VECTOR ( 'NONE', #14184, 1000.000000000000000 ) ;
#50616 = PLANE ( 'NONE',  #57515 ) ;
#50617 = VECTOR ( 'NONE', #25203, 1000.000000000000114 ) ;
#50618 = DIRECTION ( 'NONE',  ( 0.000000000000000000, 0.000000000000000000, -1.000000000000000000 ) ) ;
#50619 = CARTESIAN_POINT ( 'NONE',  ( 9.984461079971730157, -95.40710393340120277, 5.500000000000000000 ) ) ;
#50620 = DIRECTION ( 'NONE',  ( 0.000000000000000000, 0.000000000000000000, 1.000000000000000000 ) ) ;
#50621 = CARTESIAN_POINT ( 'NONE',  ( 10.00000000000000000, 50.95692526931414790, -58.39081064771693974 ) ) ;
#50622 = CARTESIAN_POINT ( 'NONE',  ( 11.99999999999999822, 59.46389618801966037, 49.70050353004911159 ) ) ;
#50623 = DIRECTION ( 'NONE',  ( -1.000000000000000000, -0.000000000000000000, -0.000000000000000000 ) ) ;
#50624 = CARTESIAN_POINT ( 'NONE',  ( 14.59956846177685996, -138.4757300459248484, 2.500000000000000000 ) ) ;
#50625 = FACE_OUTER_BOUND ( 'NONE', #28956, .T. ) ;
#50626 = CARTESIAN_POINT ( 'NONE',  ( 92.35001655588493463, -208.4700122281028598, 79.23145767387347860 ) ) ;
#50627 = DIRECTION ( 'NONE',  ( 0.000000000000000000, 0.000000000000000000, -1.000000000000000000 ) ) ;
#50628 = DIRECTION ( 'NONE',  ( -1.000000000000000000, 0.000000000000000000, -0.000000000000000000 ) ) ;
#50629 = DIRECTION ( 'NONE',  ( -1.000000000000000000, -0.000000000000000000, -0.000000000000000000 ) ) ;
#50630 = ORIENTED_EDGE ( 'NONE', *, *, #26377, .F. ) ;
#50631 = CARTESIAN_POINT ( 'NONE',  ( 10.00000000000000000, -37.22597642581153821, 10.79786254984320415 ) ) ;
#50632 = CARTESIAN_POINT ( 'NONE',  ( -96.15314808468752972, 91.99731107132950569, 79.37697916753380412 ) ) ;
#50633 = CIRCLE ( 'NONE', #47051, 23.50000000000489919 ) ;
#50634 = AXIS2_PLACEMENT_3D ( 'NONE', #35242, #58173, #6671 ) ;
#50635 = VECTOR ( 'NONE', #42241, 999.9999999999998863 ) ;
#50636 = DIRECTION ( 'NONE',  ( -1.000000000000000000, 0.000000000000000000, 0.000000000000000000 ) ) ;
#50637 = EDGE_CURVE ( 'NONE', #39991, #35258, #62198, .T. ) ;
#50638 = ORIENTED_EDGE ( 'NONE', *, *, #43480, .F. ) ;
#50639 = CARTESIAN_POINT ( 'NONE',  ( 10.00000000000000000, -54.21277698773636899, -55.38113227695839669 ) ) ;
#50640 = CARTESIAN_POINT ( 'NONE',  ( 15.00000000000000000, 14.60985201121703980, -18.46759930825707841 ) ) ;
#50641 = CARTESIAN_POINT ( 'NONE',  ( 6.000000000000000000, 29.01471420065563933, 76.69515212746026123 ) ) ;
#50642 = ADVANCED_FACE ( 'NONE', ( #66723 ), #38145, .T. ) ;
#50643 = CARTESIAN_POINT ( 'NONE',  ( -96.32499999999996021, -207.7050326799711968, 84.81416666666666515 ) ) ;
#50644 = CARTESIAN_POINT ( 'NONE',  ( 95.00000000000000000, -212.6630814284392557, 75.99031250086716227 ) ) ;
#50645 = ADVANCED_FACE ( 'NONE', ( #27606 ), #4700, .T. ) ;
#50646 = ORIENTED_EDGE ( 'NONE', *, *, #3327, .F. ) ;
#50647 = EDGE_CURVE ( 'NONE', #769, #56779, #61833, .T. ) ;
#50648 = VERTEX_POINT ( 'NONE', #61080 ) ;
#50649 = CARTESIAN_POINT ( 'NONE',  ( -0.0004442498512760095037, 0.001194404164628348752, -49.00000000000000000 ) ) ;
#50650 = DIRECTION ( 'NONE',  ( -1.000000000000000000, -0.000000000000000000, -0.000000000000000000 ) ) ;
#50651 = CIRCLE ( 'NONE', #33618, 31.99999999999997868 ) ;
#50652 = CARTESIAN_POINT ( 'NONE',  ( -93.67499999999998295, -207.7050326799711968, 85.42270833506762528 ) ) ;
#50653 = CARTESIAN_POINT ( 'NONE',  ( 11.99999999999999822, -59.46389618801999433, 49.70050353004867816 ) ) ;
#50654 = CARTESIAN_POINT ( 'NONE',  ( -10.00000000000000000, 0.000000000000000000, 0.000000000000000000 ) ) ;
#50655 = CARTESIAN_POINT ( 'NONE',  ( 96.32499999999998863, -212.2949673200287179, 87.03666666666666174 ) ) ;
#50656 = EDGE_CURVE ( 'NONE', #32383, #64543, #21965, .T. ) ;
#50657 = VECTOR ( 'NONE', #38691, 1000.000000000000000 ) ;
#50658 = EDGE_LOOP ( 'NONE', ( #22925, #9079, #31956, #30519 ) ) ;
#50659 = CARTESIAN_POINT ( 'NONE',  ( 0.000000000000000000, -41.76106447765533147, 62.50884508063410294 ) ) ;
#50660 = ORIENTED_EDGE ( 'NONE', *, *, #25289, .F. ) ;
#50661 = ORIENTED_EDGE ( 'NONE', *, *, #39986, .F. ) ;
#50662 = CARTESIAN_POINT ( 'NONE',  ( 26.00000000000000355, 0.000000000000000000, 2.445500000000000007 ) ) ;
#50663 = VECTOR ( 'NONE', #7323, 1000.000000000000000 ) ;
#50664 = CARTESIAN_POINT ( 'NONE',  ( 2.500000000000005773, 4.330127018922191873, -6.000000000000000000 ) ) ;
#50665 = VERTEX_POINT ( 'NONE', #44915 ) ;
#50666 = CARTESIAN_POINT ( 'NONE',  ( 92.34999999999999432, 88.47002178664753558, 87.51291666666666913 ) ) ;
#50667 = CARTESIAN_POINT ( 'NONE',  ( 96.32499999999998863, -207.7050326799711968, 80.97770833506763211 ) ) ;
#50668 = CARTESIAN_POINT ( 'NONE',  ( 97.64999999999999147, 90.00000000000002842, 81.42749999999999488 ) ) ;
#50669 = ORIENTED_EDGE ( 'NONE', *, *, #29840, .F. ) ;
#50670 = DIRECTION ( 'NONE',  ( -0.000000000000000000, -0.000000000000000000, -1.000000000000000000 ) ) ;
#50671 = AXIS2_PLACEMENT_3D ( 'NONE', #7891, #31186, #60159 ) ;
#50672 = VERTEX_POINT ( 'NONE', #73459 ) ;
#50673 = CARTESIAN_POINT ( 'NONE',  ( 10.00000000000000000, 0.000000000000000000, 0.000000000000000000 ) ) ;
#50674 = EDGE_CURVE ( 'NONE', #31053, #3025, #64122, .T. ) ;
#50675 = VERTEX_POINT ( 'NONE', #39643 ) ;
#50676 = CARTESIAN_POINT ( 'NONE',  ( 92.34999999999999432, 89.99997747860817299, 84.36437578067153709 ) ) ;
#50677 = CIRCLE ( 'NONE', #45878, 15.99999999999999822 ) ;
#50678 = CARTESIAN_POINT ( 'NONE',  ( -93.84685191531252713, 88.00268892867056536, 83.66322916753382799 ) ) ;
#50679 = CARTESIAN_POINT ( 'NONE',  ( 92.69370383062498320, 88.66845928578037217, 78.26572916753380582 ) ) ;
#50680 = ADVANCED_FACE ( 'NONE', ( #62586 ), #55439, .T. ) ;
#50681 = ORIENTED_EDGE ( 'NONE', *, *, #43832, .T. ) ;
#50682 = DIRECTION ( 'NONE',  ( -1.000000000000000000, 0.000000000000000000, 0.000000000000000000 ) ) ;
#50683 = CARTESIAN_POINT ( 'NONE',  ( -94.99999999999997158, -209.9999999999999716, 90.00000000000000000 ) ) ;
#50684 = CARTESIAN_POINT ( 'NONE',  ( 93.67499999999999716, 87.70503267997126784, 88.91520833506763211 ) ) ;
#50685 = FACE_OUTER_BOUND ( 'NONE', #31429, .T. ) ;
#50686 = ORIENTED_EDGE ( 'NONE', *, *, #70177, .F. ) ;
#50687 = DIRECTION ( 'NONE',  ( -1.000000000000000000, 0.000000000000000000, 0.000000000000000000 ) ) ;
#50688 = VECTOR ( 'NONE', #35952, 1000.000000000000000 ) ;
#50689 = EDGE_CURVE ( 'NONE', #45726, #49118, #26858, .T. ) ;
#50690 = VECTOR ( 'NONE', #64848, 1000.000000000000000 ) ;
#50691 = CARTESIAN_POINT ( 'NONE',  ( -92.69370383062498320, -208.6684592857803011, 76.67822916753378593 ) ) ;
#50692 = ORIENTED_EDGE ( 'NONE', *, *, #13888, .T. ) ;
#50693 = EDGE_LOOP ( 'NONE', ( #42181, #27707, #48057, #4554 ) ) ;
#50694 = PLANE ( 'NONE',  #67329 ) ;
#50695 = ORIENTED_EDGE ( 'NONE', *, *, #39539, .T. ) ;
#50696 = ADVANCED_FACE ( 'NONE', ( #21207 ), #44159, .F. ) ;
#50697 = DIRECTION ( 'NONE',  ( 0.000000000000000000, -1.065814103640136079E-14, -1.000000000000000000 ) ) ;
#50698 = CARTESIAN_POINT ( 'NONE',  ( -97.65000000000003411, -211.5299782133524502, 77.98791666666667766 ) ) ;
#50699 = VERTEX_POINT ( 'NONE', #57677 ) ;
#50700 = CARTESIAN_POINT ( 'NONE',  ( -93.33922900947476364, -211.6002630214759961, 74.64190534806809296 ) ) ;
#50701 = ORIENTED_EDGE ( 'NONE', *, *, #27780, .F. ) ;
#50702 = CARTESIAN_POINT ( 'NONE',  ( 96.32499999999997442, 92.29496732002878900, 88.59770833506763665 ) ) ;
#50703 = PLANE ( 'NONE',  #56038 ) ;
#50704 = LINE ( 'NONE', #5241, #44141 ) ;
#50705 = DIRECTION ( 'NONE',  ( -1.000000000000000000, 0.000000000000000000, 0.000000000000000000 ) ) ;
#50706 = EDGE_CURVE ( 'NONE', #68597, #47328, #37714, .T. ) ;
#50707 = FACE_OUTER_BOUND ( 'NONE', #31907, .T. ) ;
#50708 = CARTESIAN_POINT ( 'NONE',  ( 93.67500000000001137, -207.7050326799711968, 86.16354166840096696 ) ) ;
#50709 = CARTESIAN_POINT ( 'NONE',  ( 97.30629616937498838, 88.66845928578035796, 83.55739583420047722 ) ) ;
#50710 = DIRECTION ( 'NONE',  ( -1.000000000000000000, -0.000000000000000000, -0.000000000000000000 ) ) ;
#50711 = DIRECTION ( 'NONE',  ( -1.000000000000000000, 0.000000000000000000, 0.000000000000000000 ) ) ;
#50712 = CARTESIAN_POINT ( 'NONE',  ( 92.34999999999998010, -208.4700217866475498, 86.77208333333334167 ) ) ;
#50713 = PLANE ( 'NONE',  #20789 ) ;
#50714 = DIRECTION ( 'NONE',  ( -1.000000000000000000, -0.000000000000000000, -0.000000000000000000 ) ) ;
#50715 = CARTESIAN_POINT ( 'NONE',  ( -97.65000000000001990, 90.00000000000004263, 84.36437500173430237 ) ) ;
#50716 = DIRECTION ( 'NONE',  ( -1.000000000000000000, -0.000000000000000000, -0.000000000000000000 ) ) ;
#50717 = DIRECTION ( 'NONE',  ( 0.000000000000000000, 0.000000000000000000, -1.000000000000000000 ) ) ;
#50718 = LINE ( 'NONE', #39832, #33626 ) ;
#50719 = PLANE ( 'NONE',  #40945 ) ;
#50720 = CARTESIAN_POINT ( 'NONE',  ( -92.69370383062505425, 91.33154071421968467, 88.74322916753382628 ) ) ;
#50721 = DIRECTION ( 'NONE',  ( -0.2306669878475648139, -0.9730327541852491491, 0.000000000000000000 ) ) ;
#50722 = AXIS2_PLACEMENT_3D ( 'NONE', #30946, #47877, #23842 ) ;
#50723 = CARTESIAN_POINT ( 'NONE',  ( -92.34999999999999432, -208.4700217866474645, 85.92541666666664923 ) ) ;
#50724 = CIRCLE ( 'NONE', #14714, 77.49899999999999523 ) ;
#50725 = DIRECTION ( 'NONE',  ( -1.000000000000000000, 0.000000000000000000, 0.000000000000000000 ) ) ;
#50726 = CIRCLE ( 'NONE', #1514, 82.00000000000000000 ) ;
#50727 = CARTESIAN_POINT ( 'NONE',  ( 2.459674775249774736, 1.719108899120423124E-13, 15.80000000000028670 ) ) ;
#50728 = DIRECTION ( 'NONE',  ( -1.000000000000000000, 0.000000000000000000, 0.000000000000000000 ) ) ;
#50729 = DIRECTION ( 'NONE',  ( 1.000000000000000000, 1.427937372958405461E-15, 7.962523111839130290E-16 ) ) ;
#50730 = CYLINDRICAL_SURFACE ( 'NONE', #13796, 82.00000000000000000 ) ;
#50731 = EDGE_CURVE ( 'NONE', #17476, #28753, #53133, .T. ) ;
#50732 = AXIS2_PLACEMENT_3D ( 'NONE', #3579, #32484, #50523 ) ;
#50733 = AXIS2_PLACEMENT_3D ( 'NONE', #42861, #41738, #42129 ) ;
#50734 = CARTESIAN_POINT ( 'NONE',  ( 96.15314808468748708, -208.0026889286704943, 85.77989583420048803 ) ) ;
#50735 = EDGE_CURVE ( 'NONE', #41314, #36799, #68783, .T. ) ;
#50736 = EDGE_LOOP ( 'NONE', ( #25371, #25874 ) ) ;
#50737 = EDGE_CURVE ( 'NONE', #11359, #24241, #5308, .T. ) ;
#50738 = ORIENTED_EDGE ( 'NONE', *, *, #13521, .F. ) ;
#50739 = EDGE_CURVE ( 'NONE', #5518, #33832, #22725, .T. ) ;
#50740 = DIRECTION ( 'NONE',  ( -0.1850432970638667129, 0.9827303690289281857, 0.000000000000000000 ) ) ;
#50741 = ORIENTED_EDGE ( 'NONE', *, *, #52375, .F. ) ;
#50742 = DIRECTION ( 'NONE',  ( -1.000000000000000000, -0.000000000000000000, -0.000000000000000000 ) ) ;
#50743 = CARTESIAN_POINT ( 'NONE',  ( 96.15314808468750130, -211.9973110713294489, 77.15447916753380753 ) ) ;
#50744 = VERTEX_POINT ( 'NONE', #35104 ) ;
#50745 = CARTESIAN_POINT ( 'NONE',  ( 92.69370383062501162, -208.6684592857803011, 83.39864583420050792 ) ) ;
#50746 = VERTEX_POINT ( 'NONE', #30190 ) ;
#50747 = FACE_BOUND ( 'NONE', #58147, .T. ) ;
#50748 = VERTEX_POINT ( 'NONE', #1309 ) ;
#50749 = ORIENTED_EDGE ( 'NONE', *, *, #14277, .T. ) ;
#50750 = CARTESIAN_POINT ( 'NONE',  ( -95.00000000000002842, 92.66308142843932671, 75.03781250086714749 ) ) ;
#50751 = EDGE_CURVE ( 'NONE', #67112, #22210, #56932, .T. ) ;
#50752 = LINE ( 'NONE', #16931, #11242 ) ;
#50753 = EDGE_LOOP ( 'NONE', ( #55966, #48519 ) ) ;
#50754 = CARTESIAN_POINT ( 'NONE',  ( 0.000000000000000000, 0.000000000000000000, -56.19999999999998863 ) ) ;
#50755 = DIRECTION ( 'NONE',  ( -1.000000000000000000, -0.000000000000000000, -0.000000000000000000 ) ) ;
#50756 = EDGE_CURVE ( 'NONE', #61868, #49297, #64057, .T. ) ;
#50757 = VERTEX_POINT ( 'NONE', #46385 ) ;
#50758 = DIRECTION ( 'NONE',  ( -1.000000000000000000, 7.571541139944063212E-15, 2.603472992745718826E-14 ) ) ;
#50759 = ORIENTED_EDGE ( 'NONE', *, *, #56807, .T. ) ;
#50760 =( BOUNDED_CURVE ( )  B_SPLINE_CURVE ( 2, ( #66076, #31462, #14545, #66797, #72056, #2576, #20177 ),
 .UNSPECIFIED., .F., .F. ) 
 B_SPLINE_CURVE_WITH_KNOTS ( ( 3, 2, 2, 3 ),
 ( 0.4374999999999994449, 0.4444444444444441422, 0.4513888888888888951, 0.4583333333333335924 ),
 .UNSPECIFIED. ) 
 CURVE ( )  GEOMETRIC_REPRESENTATION_ITEM ( )  RATIONAL_B_SPLINE_CURVE ( ( 1.000000000000010658, 0.8660254037844280495, 1.000000000000000000, 0.8660254037844387076, 1.000000000000000000, 0.8660254037844333785, 1.000000000000005329 ) ) 
 REPRESENTATION_ITEM ( '' )  );
#50761 = CARTESIAN_POINT ( 'NONE',  ( 10.00000000000000000, 0.000000000000000000, 0.000000000000000000 ) ) ;
#50762 = ORIENTED_EDGE ( 'NONE', *, *, #17334, .F. ) ;
#50763 = MECHANICAL_DESIGN_GEOMETRIC_PRESENTATION_REPRESENTATION (  '', ( #44774 ), #8699 ) ;
#50764 = ORIENTED_EDGE ( 'NONE', *, *, #44469, .T. ) ;
#50765 = ORIENTED_EDGE ( 'NONE', *, *, #46028, .F. ) ;
#50766 = CARTESIAN_POINT ( 'NONE',  ( 92.69370383062501162, -209.9999999999999716, 76.30781250086714351 ) ) ;
#50767 = ADVANCED_FACE ( 'NONE', ( #18541 ), #46024, .F. ) ;
#50768 = ADVANCED_FACE ( 'NONE', ( #6181 ), #45665, .T. ) ;
#50769 = DIRECTION ( 'NONE',  ( -0.000000000000000000, -0.000000000000000000, 1.000000000000000000 ) ) ;
#50770 = ORIENTED_EDGE ( 'NONE', *, *, #49206, .F. ) ;
#50771 = ORIENTED_EDGE ( 'NONE', *, *, #44815, .F. ) ;
#50772 = EDGE_LOOP ( 'NONE', ( #69799, #30071, #70929, #10907 ) ) ;
#50773 = CARTESIAN_POINT ( 'NONE',  ( 11.99999999999999822, 0.000000000000000000, 0.000000000000000000 ) ) ;
#50774 = CARTESIAN_POINT ( 'NONE',  ( 10.00000000000000000, 37.58145647212453611, 0.6853352020791767529 ) ) ;
#50775 = CARTESIAN_POINT ( 'NONE',  ( -95.00000000000002842, 92.66308142843932671, 76.94281250086714863 ) ) ;
#50776 = VERTEX_POINT ( 'NONE', #17798 ) ;
#50777 = DIRECTION ( 'NONE',  ( 0.000000000000000000, -0.9510565162951503115, 0.3090169943749573878 ) ) ;
#50778 = CIRCLE ( 'NONE', #61577, 82.00000000000000000 ) ;
#50779 = ORIENTED_EDGE ( 'NONE', *, *, #53622, .F. ) ;
#50780 = CARTESIAN_POINT ( 'NONE',  ( 15.69955575014928328, 0.001194404164567414856, -70.59999999999959641 ) ) ;
#50781 = CARTESIAN_POINT ( 'NONE',  ( -97.30629616937495996, -209.9999999999999716, 87.73781250086713612 ) ) ;
#50782 = ORIENTED_EDGE ( 'NONE', *, *, #40000, .F. ) ;
#50783 = CARTESIAN_POINT ( 'NONE',  ( -92.34999999999999432, -209.9999999999999716, 75.71250000000000568 ) ) ;
#50784 = DIRECTION ( 'NONE',  ( 0.000000000000000000, 0.000000000000000000, 1.000000000000000000 ) ) ;
#50785 = LINE ( 'NONE', #18067, #72874 ) ;
#50786 = CARTESIAN_POINT ( 'NONE',  ( -94.99999999999997158, -207.3369185715606307, 78.05406250086714692 ) ) ;
#50787 = CARTESIAN_POINT ( 'NONE',  ( 97.64999999999690772, -210.0000040461968638, 77.06187486178042434 ) ) ;
#50788 = LINE ( 'NONE', #39151, #64390 ) ;
#50789 = CIRCLE ( 'NONE', #18368, 42.00000000000000000 ) ;
#50790 = DIRECTION ( 'NONE',  ( -1.000000000000000000, 0.000000000000000000, -0.000000000000000000 ) ) ;
#50791 = AXIS2_PLACEMENT_3D ( 'NONE', #10875, #34172, #57115 ) ;
#50792 = ORIENTED_EDGE ( 'NONE', *, *, #52417, .F. ) ;
#50793 = CARTESIAN_POINT ( 'NONE',  ( 15.00000000000000000, 18.84667830672579569, -18.68964196561269375 ) ) ;
#50794 = CARTESIAN_POINT ( 'NONE',  ( -95.00000000000002842, 93.05995642670504253, 76.50624999999999432 ) ) ;
#50795 = CARTESIAN_POINT ( 'NONE',  ( 92.80789733908686401, -208.8322938842642031, 74.89296886168679634 ) ) ;
#50796 = CARTESIAN_POINT ( 'NONE',  ( -93.84685191531252713, 88.00268892867056536, 82.23447916753380582 ) ) ;
#50797 = LINE ( 'NONE', #73723, #44248 ) ;
#50798 = CARTESIAN_POINT ( 'NONE',  ( 0.000000000000000000, -74.65374052328644439, -8.840884882375878107 ) ) ;
#50799 = ORIENTED_EDGE ( 'NONE', *, *, #10589, .F. ) ;
#50800 = CARTESIAN_POINT ( 'NONE',  ( 16.84844760790522855, -103.5491698323862124, 5.500000000000000000 ) ) ;
#50801 = DIRECTION ( 'NONE',  ( -1.000000000000000000, 0.000000000000000000, 0.000000000000000000 ) ) ;
#50802 = DIRECTION ( 'NONE',  ( -1.000000000000000000, 0.000000000000000000, 0.000000000000000000 ) ) ;
#50803 = DIRECTION ( 'NONE',  ( -1.000000000000000000, 0.000000000000000000, 0.000000000000000000 ) ) ;
#50804 = FACE_OUTER_BOUND ( 'NONE', #34114, .T. ) ;
#50805 = DIRECTION ( 'NONE',  ( 0.000000000000000000, 0.000000000000000000, 1.000000000000000000 ) ) ;
#50806 = CARTESIAN_POINT ( 'NONE',  ( -94.99999999999997158, -212.6630814284392557, 77.89531250086714920 ) ) ;
#50807 = CARTESIAN_POINT ( 'NONE',  ( -92.35000000000003695, 90.00000000000004263, 81.42749999999999488 ) ) ;
#50808 = APPLICATION_CONTEXT ( 'automotive_design' ) ;
#50809 = AXIS2_PLACEMENT_3D ( 'NONE', #24737, #41651, #42402 ) ;
#50810 = VERTEX_POINT ( 'NONE', #57297 ) ;
#50811 = DIRECTION ( 'NONE',  ( -0.000000000000000000, -0.000000000000000000, 1.000000000000000000 ) ) ;
#50812 = CARTESIAN_POINT ( 'NONE',  ( -97.65000000000001990, 88.47002178664754979, 80.60729166840097548 ) ) ;
#50813 = CARTESIAN_POINT ( 'NONE',  ( 0.000000000000000000, -64.81221759200306565, -50.23322058963418613 ) ) ;
#50814 = ORIENTED_EDGE ( 'NONE', *, *, #72549, .T. ) ;
#50815 = AXIS2_PLACEMENT_3D ( 'NONE', #36618, #64838, #8433 ) ;
#50816 = CARTESIAN_POINT ( 'NONE',  ( 97.65000000000000568, 91.52997821335252127, 77.11479166840095445 ) ) ;
#50818 = EDGE_CURVE ( 'NONE', #70509, #7952, #46131, .T. ) ;
#50817 = CYLINDRICAL_SURFACE ( 'NONE', #40276, 2.649999999999999467 ) ;
#50819 = CIRCLE ( 'NONE', #19581, 31.99999999999998579 ) ;
#50820 = EDGE_CURVE ( 'NONE', #59815, #71840, #72407, .T. ) ;
#50821 = DIRECTION ( 'NONE',  ( 0.000000000000000000, -0.3826834323650969427, 0.9238795325112837409 ) ) ;
#50822 = EDGE_LOOP ( 'NONE', ( #48548, #3362, #49418, #66256 ) ) ;
#50823 = EDGE_CURVE ( 'NONE', #44712, #41422, #23095, .T. ) ;
#50824 = DIRECTION ( 'NONE',  ( 0.000000000000000000, 0.5877852522924685852, 0.8090169943749507819 ) ) ;
#50825 = DIRECTION ( 'NONE',  ( -0.000000000000000000, -0.000000000000000000, 1.000000000000000000 ) ) ;
#50826 = ORIENTED_EDGE ( 'NONE', *, *, #12207, .T. ) ;
#50827 = VECTOR ( 'NONE', #43097, 1000.000000000000000 ) ;
#50828 = EDGE_CURVE ( 'NONE', #64812, #8792, #17358, .T. ) ;
#50829 = CARTESIAN_POINT ( 'NONE',  ( 0.000000000000000000, -33.00180498840060039, 17.80606268964528027 ) ) ;
#50830 = CARTESIAN_POINT ( 'NONE',  ( 0.000000000000000000, -49.70050353004932475, 59.46389618801944721 ) ) ;
#50831 = VECTOR ( 'NONE', #22446, 1000.000000000000000 ) ;
#50832 = VERTEX_POINT ( 'NONE', #11780 ) ;
#50833 = CARTESIAN_POINT ( 'NONE',  ( 15.00000000000000000, 0.000000000000000000, 0.000000000000000000 ) ) ;
#50834 = VERTEX_POINT ( 'NONE', #562 ) ;
#50835 = VECTOR ( 'NONE', #18624, 1000.000000000000114 ) ;
#50836 = LINE ( 'NONE', #44095, #60998 ) ;
#50837 = ORIENTED_EDGE ( 'NONE', *, *, #40264, .T. ) ;
#50838 = AXIS2_PLACEMENT_3D ( 'NONE', #54878, #48862, #66900 ) ;
#50839 = AXIS2_PLACEMENT_3D ( 'NONE', #18265, #24648, #64144 ) ;
#50840 = LINE ( 'NONE', #57614, #70836 ) ;
#50841 = VERTEX_POINT ( 'NONE', #6896 ) ;
#50842 = ORIENTED_EDGE ( 'NONE', *, *, #51256, .F. ) ;
#50843 = ORIENTED_EDGE ( 'NONE', *, *, #57536, .F. ) ;
#50844 = CYLINDRICAL_SURFACE ( 'NONE', #4763, 31.99999999999998579 ) ;
#50845 = EDGE_CURVE ( 'NONE', #70056, #66947, #34729, .T. ) ;
#50846 = EDGE_CURVE ( 'NONE', #24130, #8991, #29440, .T. ) ;
#50847 = ORIENTED_EDGE ( 'NONE', *, *, #69750, .F. ) ;
#50848 = ORIENTED_EDGE ( 'NONE', *, *, #72333, .F. ) ;
#50849 = CARTESIAN_POINT ( 'NONE',  ( 96.32499999999997442, 92.29496732002878900, 87.24833333333333485 ) ) ;
#50850 = DIRECTION ( 'NONE',  ( 0.000000000000000000, 0.000000000000000000, 1.000000000000000000 ) ) ;
#50851 = DIRECTION ( 'NONE',  ( 0.6575728627325955200, -0.7533909544171996098, -1.230411769795008318E-16 ) ) ;
#50852 = EDGE_LOOP ( 'NONE', ( #28024, #17686, #29673, #62751 ) ) ;
#50853 = CIRCLE ( 'NONE', #71290, 31.99999999999998224 ) ;
#50854 = ORIENTED_EDGE ( 'NONE', *, *, #32044, .F. ) ;
#50855 = ORIENTED_EDGE ( 'NONE', *, *, #17836, .T. ) ;
#50856 = CARTESIAN_POINT ( 'NONE',  ( 96.15314808468748708, 91.99731107132950569, 89.43114583420047836 ) ) ;
#50857 = ORIENTED_EDGE ( 'NONE', *, *, #59736, .T. ) ;
#50858 = CARTESIAN_POINT ( 'NONE',  ( 97.30629616937498838, -209.9999999999999716, 86.78531250086714977 ) ) ;
#50859 = EDGE_CURVE ( 'NONE', #20743, #73822, #7636, .T. ) ;
#50860 = EDGE_CURVE ( 'NONE', #62434, #68980, #43620, .T. ) ;
#50861 = DIRECTION ( 'NONE',  ( 0.000000000000000000, 0.000000000000000000, -1.000000000000000000 ) ) ;
#50862 = DIRECTION ( 'NONE',  ( -0.000000000000000000, -0.000000000000000000, 1.000000000000000000 ) ) ;
#50863 = CARTESIAN_POINT ( 'NONE',  ( 11.99999999999999822, -36.73666225445845157, -65.58780272294114866 ) ) ;
#50864 = CARTESIAN_POINT ( 'NONE',  ( 10.00000000000000000, 0.000000000000000000, 0.000000000000000000 ) ) ;
#50865 = CARTESIAN_POINT ( 'NONE',  ( 0.000000000000000000, 0.000000000000000000, 0.000000000000000000 ) ) ;
#50866 = CARTESIAN_POINT ( 'NONE',  ( -96.32499999999996021, -207.7050326799711968, 82.90916666666666401 ) ) ;
#50867 = CARTESIAN_POINT ( 'NONE',  ( 0.000000000000000000, 0.000000000000000000, 0.000000000000000000 ) ) ;
#50868 = CARTESIAN_POINT ( 'NONE',  ( -97.30629616937495996, -209.9999999999999716, 86.46781250086714010 ) ) ;
#50869 = CARTESIAN_POINT ( 'NONE',  ( -95.00000000000002842, 87.33691857156074434, 86.15031250086714465 ) ) ;
#50870 = ORIENTED_EDGE ( 'NONE', *, *, #16049, .F. ) ;
#50871 = AXIS2_PLACEMENT_3D ( 'NONE', #44546, #66366, #37792 ) ;
#50873 = CARTESIAN_POINT ( 'NONE',  ( -96.15314808468751551, 88.00268892867056536, 85.93864583420048575 ) ) ;
#50872 = CARTESIAN_POINT ( 'NONE',  ( 97.30629616937498838, 91.33154071421968467, 84.29822916753380468 ) ) ;
#50874 = EDGE_LOOP ( 'NONE', ( #7314, #27368, #13036, #61598 ) ) ;
#50875 = DIRECTION ( 'NONE',  ( 0.000000000000000000, -0.9510565162951502005, -0.3090169943749581094 ) ) ;
#50876 = CYLINDRICAL_SURFACE ( 'NONE', #38547, 2.649999999999985700 ) ;
#50877 = CYLINDRICAL_SURFACE ( 'NONE', #5566, 2.649999999999985700 ) ;
#50878 = CARTESIAN_POINT ( 'NONE',  ( 10.00000000000000000, 46.11716303203284184, -67.80270845531838120 ) ) ;
#50879 = CARTESIAN_POINT ( 'NONE',  ( -97.30629616937497417, -208.6684592857803295, 89.58989583420047609 ) ) ;
#50880 = AXIS2_PLACEMENT_3D ( 'NONE', #25669, #71517, #53136 ) ;
#50881 = DIRECTION ( 'NONE',  ( -1.000000000000000000, -0.000000000000000000, 0.000000000000000000 ) ) ;
#50882 = DIRECTION ( 'NONE',  ( 1.000000000000000000, 0.000000000000000000, -0.000000000000000000 ) ) ;
#50883 = CARTESIAN_POINT ( 'NONE',  ( -97.65000000000001990, 90.00000000000004263, 90.00000000000000000 ) ) ;
#50884 = CARTESIAN_POINT ( 'NONE',  ( 8.000000000000007105, 1.142349898368116708E-14, 6.370018489481387452E-15 ) ) ;
#50885 = DIRECTION ( 'NONE',  ( 0.9730327541852497042, -0.2306669878475623159, 0.000000000000000000 ) ) ;
#50886 = VERTEX_POINT ( 'NONE', #2414 ) ;
#50887 = ORIENTED_EDGE ( 'NONE', *, *, #73483, .T. ) ;
#50888 = SHAPE_REPRESENTATION ( 'socket head cap screw_iso_ISO 4762 M6 x 20 - 20N', ( #43395 ), #13531 ) ;
#50889 = CARTESIAN_POINT ( 'NONE',  ( -92.35000000000003695, 90.00000000000004263, 80.15749999999999886 ) ) ;
#50890 = CARTESIAN_POINT ( 'NONE',  ( 21.07894319797337701, -103.8699611390234878, -5.500000000000000000 ) ) ;
#50891 = DIRECTION ( 'NONE',  ( 0.000000000000000000, -0.9876883405951359940, -0.1564344650402420545 ) ) ;
#50892 = CARTESIAN_POINT ( 'NONE',  ( -3.249999999999999556, -13.95926121303099343, -1.199999999999999956 ) ) ;
#50893 = DIRECTION ( 'NONE',  ( 1.000000000000000000, 0.000000000000000000, 0.000000000000000000 ) ) ;
#50894 = CYLINDRICAL_SURFACE ( 'NONE', #68790, 82.00000000000000000 ) ;
#50895 = DIRECTION ( 'NONE',  ( -0.9997280174009349762, 0.02332147558787671729, 0.000000000000000000 ) ) ;
#50896 = VECTOR ( 'NONE', #15426, 1000.000000000000000 ) ;
#50897 = FACE_OUTER_BOUND ( 'NONE', #16113, .T. ) ;
#50898 = ORIENTED_EDGE ( 'NONE', *, *, #5728, .F. ) ;
#50899 = CARTESIAN_POINT ( 'NONE',  ( -97.30629616937501680, 91.33154071421968467, 78.79489583420047438 ) ) ;
#50900 = CARTESIAN_POINT ( 'NONE',  ( 97.64999999999999147, 90.00000000000002842, 90.00000000000000000 ) ) ;
#50901 = AXIS2_PLACEMENT_3D ( 'NONE', #59232, #7726, #19368 ) ;
#50902 = CIRCLE ( 'NONE', #73696, 16.00000000000000000 ) ;
#50903 = LINE ( 'NONE', #11062, #59455 ) ;
#50904 = DIRECTION ( 'NONE',  ( -8.587739980083048116E-16, -1.065814103640131346E-14, -1.000000000000000000 ) ) ;
#50905 = DIRECTION ( 'NONE',  ( 0.000000000000000000, 0.9876883405951383255, -0.1564344650402276216 ) ) ;
#50906 = DIRECTION ( 'NONE',  ( 1.000000000000000000, 0.000000000000000000, 0.000000000000000000 ) ) ;
#50907 = CARTESIAN_POINT ( 'NONE',  ( -94.99999999999997158, -212.6630814284392557, 88.69031250086716511 ) ) ;
#50908 = EDGE_CURVE ( 'NONE', #41967, #10069, #11180, .T. ) ;
#50909 = EDGE_CURVE ( 'NONE', #53791, #27456, #53213, .T. ) ;
#50910 = EDGE_CURVE ( 'NONE', #51295, #45415, #32736, .T. ) ;
#50911 = CARTESIAN_POINT ( 'NONE',  ( 94.99999999999998579, 87.33691857156068750, 78.53031250086715431 ) ) ;
#50912 = AXIS2_PLACEMENT_3D ( 'NONE', #71937, #30973, #32455 ) ;
#50913 = ADVANCED_FACE ( 'NONE', ( #65906 ), #42970, .T. ) ;
#50914 = CARTESIAN_POINT ( 'NONE',  ( -93.84685191531248449, -208.0026889286704943, 81.33489583420049485 ) ) ;
#50915 = CYLINDRICAL_SURFACE ( 'NONE', #8629, 77.49899999999999523 ) ;
#50916 = ORIENTED_EDGE ( 'NONE', *, *, #45070, .F. ) ;
#50917 = CARTESIAN_POINT ( 'NONE',  ( 10.00000000000000000, 0.000000000000000000, 0.000000000000000000 ) ) ;
#50918 = DIRECTION ( 'NONE',  ( 0.6691306063588569053, 0.7431448254773954654, 0.000000000000000000 ) ) ;
#50919 = DIRECTION ( 'NONE',  ( 1.000000000000000000, 1.427937372958405461E-15, 7.962523111839130290E-16 ) ) ;
#50920 = EDGE_CURVE ( 'NONE', #53249, #42793, #55623, .T. ) ;
#50921 = CARTESIAN_POINT ( 'NONE',  ( -95.00000000000002842, 92.66308142843932671, 78.21281250086717307 ) ) ;
#50922 = CARTESIAN_POINT ( 'NONE',  ( 92.69370383062501162, -209.9999999999999716, 80.11781250086713158 ) ) ;
#50923 = ORIENTED_EDGE ( 'NONE', *, *, #48873, .T. ) ;
#50924 = CIRCLE ( 'NONE', #12499, 31.99999999999998934 ) ;
#50925 = CARTESIAN_POINT ( 'NONE',  ( 11.99999999999999822, -70.53064760720336324, 26.01480285779810231 ) ) ;
#50926 = ORIENTED_EDGE ( 'NONE', *, *, #29715, .F. ) ;
#50927 = ADVANCED_FACE ( 'NONE', ( #2778 ), #14002, .F. ) ;
#50928 = DIRECTION ( 'NONE',  ( 1.000000000000000000, -0.000000000000000000, 0.000000000000000000 ) ) ;
#50929 = ORIENTED_EDGE ( 'NONE', *, *, #72418, .T. ) ;
#50930 = VECTOR ( 'NONE', #2419, 1000.000000000000000 ) ;
#50931 = CARTESIAN_POINT ( 'NONE',  ( 11.99999999999999822, 0.000000000000000000, 0.000000000000000000 ) ) ;
#50932 = VECTOR ( 'NONE', #43296, 999.9999999999998863 ) ;
#50933 = ORIENTED_EDGE ( 'NONE', *, *, #70082, .T. ) ;
#50934 = ORIENTED_EDGE ( 'NONE', *, *, #71466, .T. ) ;
#50935 = ORIENTED_EDGE ( 'NONE', *, *, #69497, .F. ) ;
#50936 = CARTESIAN_POINT ( 'NONE',  ( -2.981742216678212820, 0.000000000000000000, 0.000000000000000000 ) ) ;
#50937 = EDGE_CURVE ( 'NONE', #22009, #17976, #19790, .T. ) ;
#50938 = EDGE_CURVE ( 'NONE', #68378, #72362, #53364, .T. ) ;
#50939 = ORIENTED_EDGE ( 'NONE', *, *, #10342, .F. ) ;
#50940 = DIRECTION ( 'NONE',  ( -1.000000000000000000, 0.000000000000000000, 0.000000000000000000 ) ) ;
#50941 = CIRCLE ( 'NONE', #19704, 31.99999999999999289 ) ;
#50942 = CARTESIAN_POINT ( 'NONE',  ( 92.35000000003290666, -209.9999916046337205, 84.99910573348564924 ) ) ;
#50943 = CARTESIAN_POINT ( 'NONE',  ( 94.99999999999998579, 92.66308142843935514, 85.19781250086714408 ) ) ;
#50944 = CIRCLE ( 'NONE', #52124, 0.5000000000000004441 ) ;
#50945 = DIRECTION ( 'NONE',  ( -0.02332147558787823691, -0.9997280174009349762, 0.000000000000000000 ) ) ;
#50946 = CARTESIAN_POINT ( 'NONE',  ( 97.64999999999997726, -208.4700217866474645, 78.30541666666668732 ) ) ;
#50947 = VERTEX_POINT ( 'NONE', #32031 ) ;
#50948 = VERTEX_POINT ( 'NONE', #36205 ) ;
#50949 = ORIENTED_EDGE ( 'NONE', *, *, #34143, .F. ) ;
#50950 = VECTOR ( 'NONE', #57210, 1000.000000000000000 ) ;
#50951 = ORIENTED_EDGE ( 'NONE', *, *, #43256, .T. ) ;
#50952 = LINE ( 'NONE', #16369, #10575 ) ;
#50953 = VECTOR ( 'NONE', #21978, 1000.000000000000000 ) ;
#50954 =( NAMED_UNIT ( * ) SI_UNIT ( $, .STERADIAN. ) SOLID_ANGLE_UNIT ( ) );
#50955 = CARTESIAN_POINT ( 'NONE',  ( -10.00000000000000000, 0.000000000000000000, 0.000000000000000000 ) ) ;
#50956 = CARTESIAN_POINT ( 'NONE',  ( 0.000000000000000000, 0.000000000000000000, 0.000000000000000000 ) ) ;
#50957 = DIRECTION ( 'NONE',  ( -1.000000000000000000, 0.000000000000000000, 0.000000000000000000 ) ) ;
#50958 = VECTOR ( 'NONE', #22244, 1000.000000000000000 ) ;
#50959 = LINE ( 'NONE', #22389, #71993 ) ;
#50960 = CYLINDRICAL_SURFACE ( 'NONE', #29570, 2.649999999999985700 ) ;
#50961 = EDGE_LOOP ( 'NONE', ( #67775, #8239, #24584, #18463 ) ) ;
#50962 = CARTESIAN_POINT ( 'NONE',  ( -97.64999999999994884, -211.5299782133524502, 82.51229166840094820 ) ) ;
#50963 = VERTEX_POINT ( 'NONE', #1671 ) ;
#50964 = DIRECTION ( 'NONE',  ( -1.000000000000000000, 0.000000000000000000, 0.000000000000000000 ) ) ;
#50965 = VECTOR ( 'NONE', #40213, 1000.000000000000000 ) ;
#50966 = VERTEX_POINT ( 'NONE', #8005 ) ;
#50968 = CARTESIAN_POINT ( 'NONE',  ( -97.65000000000001990, 90.00000000000004263, 78.01437500173430806 ) ) ;
#50967 = CARTESIAN_POINT ( 'NONE',  ( 92.34999999999999432, 90.00000000000002842, 81.82437500173429612 ) ) ;
#50969 = ORIENTED_EDGE ( 'NONE', *, *, #15809, .F. ) ;
#50970 = CARTESIAN_POINT ( 'NONE',  ( 92.69370383062498320, 88.66845928578037217, 84.13947916753383538 ) ) ;
#50971 = CARTESIAN_POINT ( 'NONE',  ( 92.34999999999999432, 90.00000000000002842, 83.65000000000000568 ) ) ;
#50972 = DIRECTION ( 'NONE',  ( -1.000000000000000000, 0.000000000000000000, -0.000000000000000000 ) ) ;
#50973 = VECTOR ( 'NONE', #28487, 1000.000000000000000 ) ;
#50974 = DIRECTION ( 'NONE',  ( -1.000000000000000000, -0.000000000000000000, -0.000000000000000000 ) ) ;
#50975 = DIRECTION ( 'NONE',  ( -0.000000000000000000, 0.000000000000000000, 1.000000000000000000 ) ) ;
#50976 = DIRECTION ( 'NONE',  ( 0.000000000000000000, -0.5877852522924689183, 0.8090169943749504489 ) ) ;
#50977 = ORIENTED_EDGE ( 'NONE', *, *, #57315, .F. ) ;
#50978 = CARTESIAN_POINT ( 'NONE',  ( 7.999999999999992895, 1.142349898368116708E-14, 6.370018489481387452E-15 ) ) ;
#50979 = CARTESIAN_POINT ( 'NONE',  ( -97.65000000000001990, 88.47002178664754979, 82.51229166840094820 ) ) ;
#50980 = CARTESIAN_POINT ( 'NONE',  ( 1.560000000000000053, 0.000000000000000000, 0.000000000000000000 ) ) ;
#50981 = ORIENTED_EDGE ( 'NONE', *, *, #65899, .F. ) ;
#50982 = ORIENTED_EDGE ( 'NONE', *, *, #62785, .F. ) ;
#50983 = DIRECTION ( 'NONE',  ( 1.000000000000000000, -3.061616997868383141E-16, 0.000000000000000000 ) ) ;
#50984 = EDGE_CURVE ( 'NONE', #28467, #56010, #18536, .T. ) ;
#50985 = LINE ( 'NONE', #57371, #40878 ) ;
#50986 = CARTESIAN_POINT ( 'NONE',  ( 12.00000000000000000, 16.83928648764945635, 16.46020748918027010 ) ) ;
#50987 = DIRECTION ( 'NONE',  ( 0.000000000000000000, 0.000000000000000000, 1.000000000000000000 ) ) ;
#50988 =( BOUNDED_CURVE ( )  B_SPLINE_CURVE ( 2, ( #52613, #1165, #41700, #41339, #12754, #35680, #58622 ),
 .UNSPECIFIED., .F., .F. ) 
 B_SPLINE_CURVE_WITH_KNOTS ( ( 3, 2, 2, 3 ),
 ( 0.2963422021981248489, 0.3033979182579413236, 0.3104536837988239872, 0.3175094496506953301 ),
 .UNSPECIFIED. ) 
 CURVE ( )  GEOMETRIC_REPRESENTATION_ITEM ( )  RATIONAL_B_SPLINE_CURVE ( ( 0.9999981209241337599, 0.8660263433289606683, 1.000000000000000000, 0.8660254037844387076, 1.000000000000000000, 0.8660254037844387076, 1.000000000000000000 ) ) 
 REPRESENTATION_ITEM ( '' )  );
#50989 = CARTESIAN_POINT ( 'NONE',  ( -97.30629616937495996, -209.9999999999999716, 80.27656250086714351 ) ) ;
#50990 = ORIENTED_EDGE ( 'NONE', *, *, #42788, .F. ) ;
#50991 = CARTESIAN_POINT ( 'NONE',  ( -92.69370383062502583, 88.66845928578038638, 88.63739583420047552 ) ) ;
#50992 = ORIENTED_EDGE ( 'NONE', *, *, #71563, .F. ) ;
#50993 = CARTESIAN_POINT ( 'NONE',  ( 10.00000000000000000, -25.88420570971381807, -27.13269053701123212 ) ) ;
#50994 = AXIS2_PLACEMENT_3D ( 'NONE', #27356, #34488, #28107 ) ;
#50995 = CARTESIAN_POINT ( 'NONE',  ( -97.28022634950859526, -211.1627451397946231, 74.94226573542150049 ) ) ;
#50996 = CARTESIAN_POINT ( 'NONE',  ( 10.00000000000000000, -30.00120703465189465, -22.64427369931201639 ) ) ;
#50997 = DIRECTION ( 'NONE',  ( 1.000000000000000000, 0.000000000000000000, 0.000000000000000000 ) ) ;
#50998 = LINE ( 'NONE', #4412, #48488 ) ;
#50999 = CARTESIAN_POINT ( 'NONE',  ( 0.000000000000000000, 71.91182617369230456, -28.89263327155667938 ) ) ;
#51000 = EDGE_CURVE ( 'NONE', #36560, #8213, #5193, .T. ) ;
#51001 = DIRECTION ( 'NONE',  ( -0.000000000000000000, -0.000000000000000000, 1.000000000000000000 ) ) ;
#51002 = LINE ( 'NONE', #73924, #23226 ) ;
#51003 = CARTESIAN_POINT ( 'NONE',  ( 97.64999999999999147, 90.00000000000002842, 90.00000000000000000 ) ) ;
#51004 = EDGE_CURVE ( 'NONE', #32855, #24127, #64164, .T. ) ;
#51005 = CARTESIAN_POINT ( 'NONE',  ( 0.000000000000000000, 0.000000000000000000, 0.000000000000000000 ) ) ;
#51006 = AXIS2_PLACEMENT_3D ( 'NONE', #35304, #46218, #69152 ) ;
#51007 = CARTESIAN_POINT ( 'NONE',  ( 0.000000000000000000, 12.24744871391589207, 2.500000000000000000 ) ) ;
#51008 = CARTESIAN_POINT ( 'NONE',  ( 92.69370383062498320, 91.33154071421968467, 89.74864583420048803 ) ) ;
#51009 = EDGE_CURVE ( 'NONE', #55876, #65477, #27472, .T. ) ;
#51010 = CARTESIAN_POINT ( 'NONE',  ( -97.30629616937495996, -209.9999999999999716, 89.16656250086715829 ) ) ;
#51011 = LINE ( 'NONE', #68686, #68637 ) ;
#51012 = ORIENTED_EDGE ( 'NONE', *, *, #64167, .T. ) ;
#51013 = EDGE_CURVE ( 'NONE', #48732, #46548, #26402, .T. ) ;
#51014 = LINE ( 'NONE', #73935, #50831 ) ;
#51015 = CARTESIAN_POINT ( 'NONE',  ( -95.00000000000002842, 87.33691857156074434, 78.37156250086714238 ) ) ;
#51016 = AXIS2_PLACEMENT_3D ( 'NONE', #38809, #32780, #10982 ) ;
#51017 = DIRECTION ( 'NONE',  ( -1.000000000000000000, 0.000000000000000000, 0.000000000000000000 ) ) ;
#51018 = ORIENTED_EDGE ( 'NONE', *, *, #15969, .T. ) ;
#51019 = CARTESIAN_POINT ( 'NONE',  ( -11.99999999999999645, 0.000000000000000000, -13.90444123027096879 ) ) ;
#51020 = CARTESIAN_POINT ( 'NONE',  ( 97.64999999999999147, 89.99999998014077107, 85.95187500101400246 ) ) ;
#51021 = EDGE_CURVE ( 'NONE', #6219, #1606, #14942, .T. ) ;
#51022 = DIRECTION ( 'NONE',  ( 0.000000000000000000, 0.1564344650402312020, -0.9876883405951376593 ) ) ;
#51023 = AXIS2_PLACEMENT_3D ( 'NONE', #52834, #69375, #997 ) ;
#51024 = CARTESIAN_POINT ( 'NONE',  ( 10.00000000000000000, 35.95386929396241271, 10.96151621346552751 ) ) ;
#51025 = CARTESIAN_POINT ( 'NONE',  ( 93.84685191531249870, -208.0026889286704943, 75.09072916753380866 ) ) ;
#51026 = ORIENTED_EDGE ( 'NONE', *, *, #37440, .T. ) ;
#51027 = ORIENTED_EDGE ( 'NONE', *, *, #47626, .F. ) ;
#51028 = ADVANCED_FACE ( 'NONE', ( #9477 ), #21874, .F. ) ;
#51029 = DIRECTION ( 'NONE',  ( -1.000000000000000000, 0.000000000000000000, -0.000000000000000000 ) ) ;
#51030 = DIRECTION ( 'NONE',  ( 0.000000000000000000, 0.000000000000000000, -1.000000000000000000 ) ) ;
#51031 = CARTESIAN_POINT ( 'NONE',  ( 10.00000000000000000, -33.00180498840035170, -17.80606268964575278 ) ) ;
#51032 = DIRECTION ( 'NONE',  ( -1.000000000000000000, -0.000000000000000000, -0.000000000000000000 ) ) ;
#51033 = ADVANCED_FACE ( 'NONE', ( #38798 ), #62493, .T. ) ;
#51034 = CARTESIAN_POINT ( 'NONE',  ( 2.500000000000031530, 80.00000000000000000, -310.0000000000000000 ) ) ;
#51035 = CARTESIAN_POINT ( 'NONE',  ( 92.35000000000000853, -209.9999999999999716, 86.82500000000000284 ) ) ;
#51036 = ORIENTED_EDGE ( 'NONE', *, *, #42890, .T. ) ;
#51037 = ORIENTED_EDGE ( 'NONE', *, *, #16640, .F. ) ;
#51038 = FACE_OUTER_BOUND ( 'NONE', #18233, .T. ) ;
#51039 = ORIENTED_EDGE ( 'NONE', *, *, #35123, .F. ) ;
#51040 = ORIENTED_EDGE ( 'NONE', *, *, #3860, .T. ) ;
#51041 = DIRECTION ( 'NONE',  ( -0.4796670183876317051, 0.8774505977381971134, 0.000000000000000000 ) ) ;
#51042 = CARTESIAN_POINT ( 'NONE',  ( 10.00000000000000000, 35.92658777277511462, 10.74501242461295014 ) ) ;
#51043 = ORIENTED_EDGE ( 'NONE', *, *, #50739, .F. ) ;
#51044 = CARTESIAN_POINT ( 'NONE',  ( 96.32499999999998863, 87.70503267997126784, 87.67166666666666686 ) ) ;
#51045 = CARTESIAN_POINT ( 'NONE',  ( 92.35000000000000853, -209.9999999999999716, 78.01437500173430806 ) ) ;
#51046 = CARTESIAN_POINT ( 'NONE',  ( 97.64999999999999147, 90.00000000000002842, 80.79249999999998977 ) ) ;
#51047 = EDGE_LOOP ( 'NONE', ( #65514, #71268, #53535, #4653 ) ) ;
#51048 = CARTESIAN_POINT ( 'NONE',  ( 97.64999999999999147, -209.9999999999999716, 90.00000000000000000 ) ) ;
#51049 = ORIENTED_EDGE ( 'NONE', *, *, #61687, .T. ) ;
#51050 = DIRECTION ( 'NONE',  ( 0.000000000000000000, -0.9238795325112906243, 0.3826834323650804559 ) ) ;
#51051 = ORIENTED_EDGE ( 'NONE', *, *, #14364, .T. ) ;
#51052 = CARTESIAN_POINT ( 'NONE',  ( -96.32500000000001705, 92.29496732002878900, 89.33854166840096411 ) ) ;
#51053 = CARTESIAN_POINT ( 'NONE',  ( -97.30629616937501680, 91.33154071421968467, 80.85864583420048746 ) ) ;
#51054 = CARTESIAN_POINT ( 'NONE',  ( 94.99999999999998579, 87.33691857156068750, 77.73656250086713726 ) ) ;
#51055 = CIRCLE ( 'NONE', #43880, 31.99999999999998579 ) ;
#51056 = ORIENTED_EDGE ( 'NONE', *, *, #27326, .T. ) ;
#51057 = CARTESIAN_POINT ( 'NONE',  ( -14.09999999999999964, 1.726751986797767995E-15, 0.000000000000000000 ) ) ;
#51058 = FACE_OUTER_BOUND ( 'NONE', #25495, .T. ) ;
#51059 = CYLINDRICAL_SURFACE ( 'NONE', #65425, 37.49900000000000233 ) ;
#51060 = DIRECTION ( 'NONE',  ( -0.000000000000000000, -0.000000000000000000, 1.000000000000000000 ) ) ;
#51061 = ORIENTED_EDGE ( 'NONE', *, *, #8716, .T. ) ;
#51062 = DIRECTION ( 'NONE',  ( -1.000000000000000000, -0.000000000000000000, 0.000000000000000000 ) ) ;
#51063 = VECTOR ( 'NONE', #70974, 1000.000000000000114 ) ;
#51064 = CARTESIAN_POINT ( 'NONE',  ( -97.30629616937495996, -209.9999999999999716, 78.21281250086714465 ) ) ;
#51065 = ORIENTED_EDGE ( 'NONE', *, *, #32057, .F. ) ;
#51066 = ORIENTED_EDGE ( 'NONE', *, *, #24554, .T. ) ;
#51068 = DIRECTION ( 'NONE',  ( 0.000000000000000000, 0.000000000000000000, 1.000000000000000000 ) ) ;
#51067 = AXIS2_PLACEMENT_3D ( 'NONE', #23262, #63861, #18342 ) ;
#51069 = ORIENTED_EDGE ( 'NONE', *, *, #20864, .T. ) ;
#51070 = FACE_OUTER_BOUND ( 'NONE', #47558, .T. ) ;
#51071 = EDGE_CURVE ( 'NONE', #44773, #3345, #47681, .T. ) ;
#51072 = DIRECTION ( 'NONE',  ( 0.000000000000000000, 0.000000000000000000, 1.000000000000000000 ) ) ;
#51073 = VERTEX_POINT ( 'NONE', #66635 ) ;
#51074 = CARTESIAN_POINT ( 'NONE',  ( -94.99999999999997158, -207.3369185715606307, 89.64281250086715147 ) ) ;
#51075 = VERTEX_POINT ( 'NONE', #44817 ) ;
#51076 = CARTESIAN_POINT ( 'NONE',  ( -97.64999999999997726, 88.47002178664750716, 76.71791666666666742 ) ) ;
#51077 = CARTESIAN_POINT ( 'NONE',  ( -11.63999999999999702, 1.552852141318844077E-15, -12.50000000000000000 ) ) ;
#51078 = DIRECTION ( 'NONE',  ( 0.000000000000000000, -0.1045284632676558301, -0.9945218953682731788 ) ) ;
#51079 = CYLINDRICAL_SURFACE ( 'NONE', #21908, 77.49899999999999523 ) ;
#51080 = AXIS2_PLACEMENT_3D ( 'NONE', #52361, #18881, #64766 ) ;
#51081 = DIRECTION ( 'NONE',  ( 1.000000000000000000, 0.000000000000000000, 0.000000000000000000 ) ) ;
#51082 = EDGE_CURVE ( 'NONE', #49949, #67626, #73748, .T. ) ;
#51083 = AXIS2_PLACEMENT_3D ( 'NONE', #60349, #54696, #49423 ) ;
#51084 = LINE ( 'NONE', #57474, #37340 ) ;
#51085 = CARTESIAN_POINT ( 'NONE',  ( 96.15314808468748708, 91.99731107132950569, 83.71614583420047495 ) ) ;
#51086 = DIRECTION ( 'NONE',  ( 0.000000000000000000, 0.000000000000000000, 1.000000000000000000 ) ) ;
#51087 = DIRECTION ( 'NONE',  ( -1.000000000000000000, -0.000000000000000000, 0.000000000000000000 ) ) ;
#51088 = EDGE_CURVE ( 'NONE', #67020, #46606, #37765, .T. ) ;
#51089 = DIRECTION ( 'NONE',  ( -1.000000000000000000, -0.000000000000000000, -0.000000000000000000 ) ) ;
#51090 = DIRECTION ( 'NONE',  ( -1.000000000000000000, -0.000000000000000000, -0.000000000000000000 ) ) ;
#51091 = DIRECTION ( 'NONE',  ( 1.000000000000000000, -3.035766082959412415E-16, 0.000000000000000000 ) ) ;
#51092 = CARTESIAN_POINT ( 'NONE',  ( -97.65000000000001990, 91.52997821335253548, 84.31145833506762699 ) ) ;
#51093 = CARTESIAN_POINT ( 'NONE',  ( 0.000000000000000000, 0.000000000000000000, -6.000000000000000000 ) ) ;
#51094 = CARTESIAN_POINT ( 'NONE',  ( 13.83832728059186046, -142.6495187161941089, 5.500000000000000000 ) ) ;
#51095 = DIRECTION ( 'NONE',  ( 0.000000000000000000, 0.000000000000000000, 1.000000000000000000 ) ) ;
#51096 = EDGE_CURVE ( 'NONE', #61856, #27431, #59222, .T. ) ;
#51097 = CARTESIAN_POINT ( 'NONE',  ( 92.35000000046409241, -210.0000309672231253, 77.38038495127494798 ) ) ;
#51098 = CYLINDRICAL_SURFACE ( 'NONE', #66574, 31.99999999999998579 ) ;
#51099 = CARTESIAN_POINT ( 'NONE',  ( 7.400000000000003908, 1.056673655987569448E-14, 5.892267102770835596E-15 ) ) ;
#51100 = CARTESIAN_POINT ( 'NONE',  ( -94.99999999999997158, -213.0599564267049857, 85.71374999999997613 ) ) ;
#51101 = CARTESIAN_POINT ( 'NONE',  ( -92.35000000000005116, 88.47002178664753558, 80.10458333333330927 ) ) ;
#51102 = EDGE_CURVE ( 'NONE', #29721, #68284, #16603, .T. ) ;
#51103 = CARTESIAN_POINT ( 'NONE',  ( -97.65000000000001990, 90.00000000000004263, 77.29999999999999716 ) ) ;
#51104 = EDGE_CURVE ( 'NONE', #66094, #46998, #35178, .T. ) ;
#51105 = VECTOR ( 'NONE', #28399, 1000.000000000000000 ) ;
#51106 = CARTESIAN_POINT ( 'NONE',  ( 3.000000000000000000, -1.467624384280027838, 2.542000000000001592 ) ) ;
#51107 = DIRECTION ( 'NONE',  ( 0.000000000000000000, 0.000000000000000000, 1.000000000000000000 ) ) ;
#51108 = CARTESIAN_POINT ( 'NONE',  ( 0.000000000000000000, 0.000000000000000000, -56.19999999999998863 ) ) ;
#51109 = EDGE_CURVE ( 'NONE', #12392, #65491, #24553, .T. ) ;
#51110 = CIRCLE ( 'NONE', #52292, 16.00000000000000000 ) ;
#51111 = CARTESIAN_POINT ( 'NONE',  ( 96.15314808468750130, -211.9973110713294489, 86.83822916753382515 ) ) ;
#51112 = AXIS2_PLACEMENT_3D ( 'NONE', #60825, #32228, #53423 ) ;
#51113 = VERTEX_POINT ( 'NONE', #43712 ) ;
#51114 = AXIS2_PLACEMENT_3D ( 'NONE', #28424, #1014, #64137 ) ;
#51115 = ORIENTED_EDGE ( 'NONE', *, *, #917, .F. ) ;
#51116 = ADVANCED_FACE ( 'NONE', ( #21489 ), #22250, .T. ) ;
#51117 = CARTESIAN_POINT ( 'NONE',  ( 11.99999999999999822, 0.000000000000000000, 0.000000000000000000 ) ) ;
#51118 = ORIENTED_EDGE ( 'NONE', *, *, #47143, .T. ) ;
#51119 = DIRECTION ( 'NONE',  ( 0.000000000000000000, 0.000000000000000000, 1.000000000000000000 ) ) ;
#51120 = CARTESIAN_POINT ( 'NONE',  ( 97.30629616937498838, -208.6684592857803295, 78.58322916753381548 ) ) ;
#51121 = ORIENTED_EDGE ( 'NONE', *, *, #20156, .F. ) ;
#51122 = CARTESIAN_POINT ( 'NONE',  ( 96.15314808468748708, -208.0026889286704943, 84.50989583420049200 ) ) ;
#51123 = ORIENTED_EDGE ( 'NONE', *, *, #67071, .F. ) ;
#51124 = DIRECTION ( 'NONE',  ( 0.000000000000000000, -0.9876883405951393247, 0.1564344650402205161 ) ) ;
#51125 = ORIENTED_EDGE ( 'NONE', *, *, #29005, .T. ) ;
#51126 = ORIENTED_EDGE ( 'NONE', *, *, #25637, .F. ) ;
#51127 = SURFACE_STYLE_FILL_AREA ( #11274 ) ;
#51128 =( GEOMETRIC_REPRESENTATION_CONTEXT ( 3 ) GLOBAL_UNCERTAINTY_ASSIGNED_CONTEXT ( ( #65436 ) ) GLOBAL_UNIT_ASSIGNED_CONTEXT ( ( #44088, #54627, #48975 ) ) REPRESENTATION_CONTEXT ( 'NONE', 'WORKASPACE' ) );
#51129 = CARTESIAN_POINT ( 'NONE',  ( 0.000000000000000000, 0.000000000000000000, 0.000000000000000000 ) ) ;
#51130 = EDGE_LOOP ( 'NONE', ( #22025, #8445, #66068, #27500 ) ) ;
#51131 = CARTESIAN_POINT ( 'NONE',  ( -11.99999999999999645, 0.000000000000000000, 0.000000000000000000 ) ) ;
#51132 = CARTESIAN_POINT ( 'NONE',  ( 96.32499999999998863, -212.2949673200287179, 86.48104166840096241 ) ) ;
#51133 = ORIENTED_EDGE ( 'NONE', *, *, #18386, .F. ) ;
#51134 = DIRECTION ( 'NONE',  ( 0.000000000000000000, 0.000000000000000000, 1.000000000000000000 ) ) ;
#51135 = VERTEX_POINT ( 'NONE', #67365 ) ;
#51136 = DIRECTION ( 'NONE',  ( -1.000000000000000000, 0.000000000000000000, -0.000000000000000000 ) ) ;
#51137 = EDGE_LOOP ( 'NONE', ( #43668, #21616 ) ) ;
#51138 = ORIENTED_EDGE ( 'NONE', *, *, #6450, .T. ) ;
#51139 = EDGE_LOOP ( 'NONE', ( #70632, #52700, #48633, #55820 ) ) ;
#51140 = CARTESIAN_POINT ( 'NONE',  ( 95.00000000000000000, -212.6630814284392557, 75.83156250086715033 ) ) ;
#51141 = CARTESIAN_POINT ( 'NONE',  ( 35.50000000000000711, -120.0000000000000000, -2.500000000000000000 ) ) ;
#51142 = ORIENTED_EDGE ( 'NONE', *, *, #25527, .T. ) ;
#51143 = ORIENTED_EDGE ( 'NONE', *, *, #29424, .T. ) ;
#51144 = VERTEX_POINT ( 'NONE', #15869 ) ;
#51145 = LINE ( 'NONE', #29318, #7288 ) ;
#51146 = CARTESIAN_POINT ( 'NONE',  ( 12.50000000000000000, -120.0000000000000000, -40.00000000000000711 ) ) ;
#51147 = CARTESIAN_POINT ( 'NONE',  ( -92.69370383062504004, 90.00000000000004263, 75.51406250086715488 ) ) ;
#51148 = ORIENTED_EDGE ( 'NONE', *, *, #52963, .F. ) ;
#51149 = CARTESIAN_POINT ( 'NONE',  ( 0.000000000000000000, -63.18004540533059554, 44.88180994100355292 ) ) ;
#51150 = ORIENTED_EDGE ( 'NONE', *, *, #61640, .T. ) ;
#51151 = CARTESIAN_POINT ( 'NONE',  ( 10.00000000000000000, 0.000000000000000000, 37.49900000000000233 ) ) ;
#51152 = CARTESIAN_POINT ( 'NONE',  ( -93.84685191531247028, -211.9973110713294489, 86.67947916753381321 ) ) ;
#51153 = VERTEX_POINT ( 'NONE', #12075 ) ;
#51154 = AXIS2_PLACEMENT_3D ( 'NONE', #56909, #50507, #22694 ) ;
#51155 = CARTESIAN_POINT ( 'NONE',  ( 92.48104893696870477, -210.1706338775360337, 74.92125785461004739 ) ) ;
#51156 = LINE ( 'NONE', #40259, #11653 ) ;
#51157 = CARTESIAN_POINT ( 'NONE',  ( -92.69370383062498320, -209.9999999999999716, 77.89531250086714920 ) ) ;
#51158 = EDGE_CURVE ( 'NONE', #72505, #36317, #47361, .T. ) ;
#51159 = EDGE_CURVE ( 'NONE', #2154, #31895, #6805, .T. ) ;
#51160 = DIRECTION ( 'NONE',  ( -1.000000000000000000, -0.000000000000000000, -0.000000000000000000 ) ) ;
#51161 = FACE_OUTER_BOUND ( 'NONE', #66913, .T. ) ;
#51162 = EDGE_CURVE ( 'NONE', #33442, #42798, #30550, .T. ) ;
#51163 = VECTOR ( 'NONE', #1503, 1000.000000000000000 ) ;
#51164 = DIRECTION ( 'NONE',  ( 0.000000000000000000, 0.000000000000000000, 1.000000000000000000 ) ) ;
#51165 = AXIS2_PLACEMENT_3D ( 'NONE', #66358, #53216, #1753 ) ;
#51166 = ADVANCED_FACE ( 'NONE', ( #52297 ), #29718, .T. ) ;
#51167 = CARTESIAN_POINT ( 'NONE',  ( -92.35000000000003695, 90.00000000000004263, 76.34749999999999659 ) ) ;
#51168 = CARTESIAN_POINT ( 'NONE',  ( -14.87942725330654348, -141.9795960975983178, 5.500000000000000000 ) ) ;
#51169 = CARTESIAN_POINT ( 'NONE',  ( -95.00000000000002842, 92.66308142843932671, 81.86406250086714920 ) ) ;
#51170 = PLANE ( 'NONE',  #13052 ) ;
#51171 = CARTESIAN_POINT ( 'NONE',  ( 11.99999999999999822, -75.11764819372145041, -2.946379043147127064 ) ) ;
#51172 = AXIS2_PLACEMENT_3D ( 'NONE', #6793, #51912, #18081 ) ;
#51173 = AXIS2_PLACEMENT_3D ( 'NONE', #63211, #22607, #33878 ) ;
#51174 = ADVANCED_FACE ( 'NONE', ( #34262 ), #23725, .F. ) ;
#51175 = ORIENTED_EDGE ( 'NONE', *, *, #35638, .T. ) ;
#51176 = CARTESIAN_POINT ( 'NONE',  ( 0.000000000000000000, 0.000000000000000000, -0.3501037691048548561 ) ) ;
#51177 = CARTESIAN_POINT ( 'NONE',  ( 97.64999999964365429, -210.0000434577794408, 89.12687334326047051 ) ) ;
#51178 = CARTESIAN_POINT ( 'NONE',  ( 10.00000000000000000, 0.6853352020790449695, 37.58145647212454321 ) ) ;
#51179 = CARTESIAN_POINT ( 'NONE',  ( 0.000000000000000000, -55.19960302592029677, -51.03279382321147750 ) ) ;
#51180 = CARTESIAN_POINT ( 'NONE',  ( 0.000000000000000000, -1.278221433540145613, -26.51162292216073979 ) ) ;
#51181 = AXIS2_PLACEMENT_3D ( 'NONE', #48884, #71807, #20319 ) ;
#51182 = CARTESIAN_POINT ( 'NONE',  ( -97.65000000000001990, 90.00000000000004263, 85.63437500173431260 ) ) ;
#51183 = CARTESIAN_POINT ( 'NONE',  ( -97.30629616937495996, -209.9999999999999716, 80.91156250086716284 ) ) ;
#51184 = CARTESIAN_POINT ( 'NONE',  ( -7.468086116107294004, -12.33868914344945189, -1.199999999999999956 ) ) ;
#51185 = VERTEX_POINT ( 'NONE', #28618 ) ;
#51186 = DIRECTION ( 'NONE',  ( 0.000000000000000000, -0.7071067811865536790, 0.7071067811865413555 ) ) ;
#51187 = EDGE_CURVE ( 'NONE', #370, #69518, #64329, .T. ) ;
#51188 = CARTESIAN_POINT ( 'NONE',  ( 94.99999999999998579, 93.05995642670504253, 76.58562500173430010 ) ) ;
#51189 = CYLINDRICAL_SURFACE ( 'NONE', #50155, 42.00000000000000000 ) ;
#51190 = DIRECTION ( 'NONE',  ( -1.000000000000000000, 0.000000000000000000, 0.000000000000000000 ) ) ;
#51191 = DIRECTION ( 'NONE',  ( -1.000000000000000000, -0.000000000000000000, -0.000000000000000000 ) ) ;
#51192 = EDGE_CURVE ( 'NONE', #52450, #48511, #45570, .T. ) ;
#51193 = EDGE_CURVE ( 'NONE', #40320, #64962, #41390, .T. ) ;
#51194 = VECTOR ( 'NONE', #56333, 1000.000000000000000 ) ;
#51195 = CARTESIAN_POINT ( 'NONE',  ( -18.24502636017239965, -100.7225776329765665, 2.500000000000000000 ) ) ;
#51196 = ORIENTED_EDGE ( 'NONE', *, *, #8576, .T. ) ;
#51197 = CARTESIAN_POINT ( 'NONE',  ( 10.00000000000000178, 0.000000000000000000, 0.000000000000000000 ) ) ;
#51198 = ADVANCED_FACE ( 'NONE', ( #68493 ), #35382, .F. ) ;
#51199 = DIRECTION ( 'NONE',  ( -0.000000000000000000, -0.000000000000000000, 1.000000000000000000 ) ) ;
#51200 = ORIENTED_EDGE ( 'NONE', *, *, #51638, .F. ) ;
#51201 =( BOUNDED_CURVE ( )  B_SPLINE_CURVE ( 2, ( #68820, #429, #69551, #35690, #58633, #23324, #5672 ),
 .UNSPECIFIED., .F., .F. ) 
 B_SPLINE_CURVE_WITH_KNOTS ( ( 3, 2, 2, 3 ),
 ( 0.7408554641904511184, 0.7479111473372028751, 0.7549669128781208993, 0.7620226289501886852 ),
 .UNSPECIFIED. ) 
 CURVE ( )  GEOMETRIC_REPRESENTATION_ITEM ( )  RATIONAL_B_SPLINE_CURVE ( ( 0.9999968710422149076, 0.8660269682816007508, 1.000000000000000000, 0.8660254037844387076, 1.000000000000000000, 0.8660263430970057685, 0.9999981213880371200 ) ) 
 REPRESENTATION_ITEM ( '' )  );
#51202 = CARTESIAN_POINT ( 'NONE',  ( 97.30629616937498838, -209.9999999999999716, 86.78531250086714977 ) ) ;
#51203 = DIRECTION ( 'NONE',  ( -1.000000000000000000, -0.000000000000000000, -0.000000000000000000 ) ) ;
#51204 = AXIS2_PLACEMENT_3D ( 'NONE', #38773, #68090, #33484 ) ;
#51205 = ORIENTED_EDGE ( 'NONE', *, *, #45355, .F. ) ;
#51206 = CARTESIAN_POINT ( 'NONE',  ( 97.64999999999999147, -209.9999999999999716, 89.68250000000000455 ) ) ;
#51207 = VERTEX_POINT ( 'NONE', #35015 ) ;
#51208 = CARTESIAN_POINT ( 'NONE',  ( -92.34999999999999432, -208.4700217866474645, 84.73479166840094479 ) ) ;
#51209 = ORIENTED_EDGE ( 'NONE', *, *, #19286, .T. ) ;
#51210 = CARTESIAN_POINT ( 'NONE',  ( -96.32499999999996021, -212.2949673200287179, 80.02520833506763154 ) ) ;
#51211 = ORIENTED_EDGE ( 'NONE', *, *, #31409, .T. ) ;
#51212 = VECTOR ( 'NONE', #15613, 1000.000000000000000 ) ;
#51213 = CARTESIAN_POINT ( 'NONE',  ( 10.00000000000000000, -62.20884554313985149, -46.21855187248698371 ) ) ;
#51214 = ORIENTED_EDGE ( 'NONE', *, *, #2824, .F. ) ;
#51215 = VECTOR ( 'NONE', #44727, 1000.000000000000000 ) ;
#51216 = ORIENTED_EDGE ( 'NONE', *, *, #49231, .T. ) ;
#51217 = CARTESIAN_POINT ( 'NONE',  ( 10.00000000000000000, -4.992566952385247170, 37.16516213103275845 ) ) ;
#51218 = EDGE_LOOP ( 'NONE', ( #66139, #32572, #47077, #26985 ) ) ;
#51219 = PRODUCT_DEFINITION_SHAPE ( 'NONE', 'NONE',  #74377 ) ;
#51220 = AXIS2_PLACEMENT_3D ( 'NONE', #17256, #5994, #64234 ) ;
#51221 = ORIENTED_EDGE ( 'NONE', *, *, #66544, .T. ) ;
#51222 = CARTESIAN_POINT ( 'NONE',  ( 95.46326757314949418, 87.15692181550788575, 74.72378867588406592 ) ) ;
#51223 = CARTESIAN_POINT ( 'NONE',  ( 10.00000000000000000, 9.188173127307297960, 40.98264845739753071 ) ) ;
#51224 = PLANE ( 'NONE',  #33302 ) ;
#51225 = ORIENTED_EDGE ( 'NONE', *, *, #2853, .F. ) ;
#51226 = ORIENTED_EDGE ( 'NONE', *, *, #63066, .T. ) ;
#51227 = ORIENTED_EDGE ( 'NONE', *, *, #73767, .F. ) ;
#51228 = CARTESIAN_POINT ( 'NONE',  ( 94.99999999999998579, 92.66308142843935514, 83.76906250086713612 ) ) ;
#51229 = VERTEX_POINT ( 'NONE', #40281 ) ;
#51230 = CARTESIAN_POINT ( 'NONE',  ( 95.00000000000000000, -212.6630814284392557, 84.72156250086713669 ) ) ;
#51231 = CARTESIAN_POINT ( 'NONE',  ( -97.64999999999996305, -209.9999999999999716, 81.18937500173430521 ) ) ;
#51232 = CIRCLE ( 'NONE', #29593, 82.00000000000000000 ) ;
#51233 = CARTESIAN_POINT ( 'NONE',  ( 0.000000000000000000, 54.21277698773675979, 55.38113227695801299 ) ) ;
#51234 = DIRECTION ( 'NONE',  ( 0.000000000000000000, -0.2079116908177533474, 0.9781476007338069101 ) ) ;
#51235 = DIRECTION ( 'NONE',  ( -0.000000000000000000, -0.000000000000000000, 1.000000000000000000 ) ) ;
#51236 = DIRECTION ( 'NONE',  ( -1.000000000000000000, -0.000000000000000000, 0.000000000000000000 ) ) ;
#51237 = CYLINDRICAL_SURFACE ( 'NONE', #17878, 37.49900000000000233 ) ;
#51238 = CARTESIAN_POINT ( 'NONE',  ( -92.69370383062498320, -211.3315407142195852, 86.73239583420047438 ) ) ;
#51239 = CARTESIAN_POINT ( 'NONE',  ( -96.15314808468751551, 88.00268892867056536, 85.46239583420047836 ) ) ;
#51240 = ORIENTED_EDGE ( 'NONE', *, *, #36083, .T. ) ;
#51242 = CARTESIAN_POINT ( 'NONE',  ( -92.69370383062502583, 91.33154071421968467, 84.29822916753380468 ) ) ;
#51241 = CARTESIAN_POINT ( 'NONE',  ( 93.84685191531248449, 88.00268892867053694, 82.76364583420047438 ) ) ;
#51243 = ORIENTED_EDGE ( 'NONE', *, *, #27863, .T. ) ;
#51244 = DIRECTION ( 'NONE',  ( 0.000000000000000000, 0.000000000000000000, 1.000000000000000000 ) ) ;
#51245 = CARTESIAN_POINT ( 'NONE',  ( 11.99999999999999822, -76.66974797899830207, -11.30684508768420571 ) ) ;
#51246 = DIRECTION ( 'NONE',  ( -1.000000000000000000, -0.000000000000000000, 0.000000000000000000 ) ) ;
#51247 = CARTESIAN_POINT ( 'NONE',  ( 0.000000000000000000, 0.000000000000000000, 0.000000000000000000 ) ) ;
#51248 = CARTESIAN_POINT ( 'NONE',  ( 3.000000000000000000, 4.131365146527187385E-15, 2.541999999999999371 ) ) ;
#51249 = DIRECTION ( 'NONE',  ( -1.000000000000000000, -0.000000000000000000, -0.000000000000000000 ) ) ;
#51250 = CARTESIAN_POINT ( 'NONE',  ( -10.00000000000000000, 0.000000000000000000, 0.000000000000000000 ) ) ;
#51251 = CARTESIAN_POINT ( 'NONE',  ( 0.000000000000000000, -73.44644590900043113, -24.73286445877782924 ) ) ;
#51252 = ORIENTED_EDGE ( 'NONE', *, *, #8909, .T. ) ;
#51253 = AXIS2_PLACEMENT_3D ( 'NONE', #56081, #20393, #54964 ) ;
#51254 = EDGE_CURVE ( 'NONE', #54092, #16556, #34164, .T. ) ;
#51255 = ORIENTED_EDGE ( 'NONE', *, *, #15867, .F. ) ;
#51256 = EDGE_CURVE ( 'NONE', #38048, #14970, #27919, .T. ) ;
#51257 = CARTESIAN_POINT ( 'NONE',  ( -93.67500000000003979, 87.70503267997129626, 79.41666666666665719 ) ) ;
#51258 = DIRECTION ( 'NONE',  ( 0.000000000000000000, -0.9969173337331271867, -0.07845909572785571273 ) ) ;
#51259 = DIRECTION ( 'NONE',  ( 0.000000000000000000, 0.000000000000000000, -1.000000000000000000 ) ) ;
#51260 = CARTESIAN_POINT ( 'NONE',  ( -97.64999999999994884, -209.9999678257240703, 76.74437388893710477 ) ) ;
#51261 = DIRECTION ( 'NONE',  ( 1.000000000000000000, 1.427937372958405461E-15, 7.962523111839130290E-16 ) ) ;
#51262 = CARTESIAN_POINT ( 'NONE',  ( -92.34999999999999432, -210.0000001167898631, 84.68187499741277691 ) ) ;
#51263 = DIRECTION ( 'NONE',  ( -0.000000000000000000, -0.000000000000000000, -1.000000000000000000 ) ) ;
#51264 = EDGE_CURVE ( 'NONE', #31708, #23659, #35606, .T. ) ;
#51265 = VECTOR ( 'NONE', #14266, 1000.000000000000000 ) ;
#51266 = EDGE_LOOP ( 'NONE', ( #61990, #15048, #47057, #23110 ) ) ;
#51267 = CARTESIAN_POINT ( 'NONE',  ( -92.69370383062502583, 88.66845928578038638, 77.84239583420045960 ) ) ;
#51268 = VECTOR ( 'NONE', #57243, 1000.000000000000000 ) ;
#51269 = CARTESIAN_POINT ( 'NONE',  ( 103.9230484541331947, -179.9999999999990337, 5.500000000000000000 ) ) ;
#51270 = DIRECTION ( 'NONE',  ( -1.000000000000000000, 0.000000000000000000, 0.000000000000000000 ) ) ;
#51271 = DIRECTION ( 'NONE',  ( 0.000000000000000000, 0.000000000000000000, 1.000000000000000000 ) ) ;
#51272 = CIRCLE ( 'NONE', #66887, 12.49999999999999645 ) ;
#51273 = CYLINDRICAL_SURFACE ( 'NONE', #28514, 16.00000000000000000 ) ;
#51274 = CARTESIAN_POINT ( 'NONE',  ( 11.99999999999999822, 0.000000000000000000, 0.000000000000000000 ) ) ;
#51275 = CARTESIAN_POINT ( 'NONE',  ( -93.84685191531248449, -208.0026889286704943, 88.31989583420048007 ) ) ;
#51276 = AXIS2_PLACEMENT_3D ( 'NONE', #4795, #45377, #61919 ) ;
#51277 = ADVANCED_FACE ( 'NONE', ( #471 ), #11330, .F. ) ;
#51278 = EDGE_CURVE ( 'NONE', #30710, #52760, #49762, .T. ) ;
#51279 = AXIS2_PLACEMENT_3D ( 'NONE', #57590, #28995, #68114 ) ;
#51280 = CARTESIAN_POINT ( 'NONE',  ( 97.30629616937498838, 88.66845928578035796, 77.36614583420048064 ) ) ;
#51281 = CARTESIAN_POINT ( 'NONE',  ( -92.69370383062498320, -208.6684592857803295, 80.64697916753382856 ) ) ;
#51282 = DIRECTION ( 'NONE',  ( -1.000000000000000000, 0.000000000000000000, 0.000000000000000000 ) ) ;
#51283 = ORIENTED_EDGE ( 'NONE', *, *, #61518, .F. ) ;
#51284 = DIRECTION ( 'NONE',  ( 1.000000000000000000, -7.571537405616606460E-15, -2.598394312951952234E-14 ) ) ;
#51285 = DIRECTION ( 'NONE',  ( -1.000000000000000000, 0.000000000000000000, 0.000000000000000000 ) ) ;
#51286 = LINE ( 'NONE', #27981, #19716 ) ;
#51287 = ADVANCED_FACE ( 'NONE', ( #8664 ), #43264, .T. ) ;
#51288 = EDGE_CURVE ( 'NONE', #43739, #27052, #13549, .T. ) ;
#51289 = CIRCLE ( 'NONE', #20043, 77.49899999999999523 ) ;
#51290 = CARTESIAN_POINT ( 'NONE',  ( -92.69370383062505425, 88.66845928578038638, 77.36614583420048064 ) ) ;
#51291 = CARTESIAN_POINT ( 'NONE',  ( 96.15314808468750130, -211.9973110713294489, 81.59947916753381492 ) ) ;
#51292 = VERTEX_POINT ( 'NONE', #65445 ) ;
#51293 = AXIS2_PLACEMENT_3D ( 'NONE', #42633, #14040, #61026 ) ;
#51294 = DIRECTION ( 'NONE',  ( 0.000000000000000000, 0.000000000000000000, -1.000000000000000000 ) ) ;
#51295 = VERTEX_POINT ( 'NONE', #25575 ) ;
#51296 = DIRECTION ( 'NONE',  ( 0.000000000000000000, -0.5000000000000039968, 0.8660254037844363761 ) ) ;
#51297 = ORIENTED_EDGE ( 'NONE', *, *, #51109, .T. ) ;
#51298 = CARTESIAN_POINT ( 'NONE',  ( 6.000000000000000000, 80.55351364060611274, -15.33399622253396899 ) ) ;
#51299 = ORIENTED_EDGE ( 'NONE', *, *, #46249, .F. ) ;
#51300 = ORIENTED_EDGE ( 'NONE', *, *, #31480, .T. ) ;
#51301 = EDGE_LOOP ( 'NONE', ( #53652, #62366, #46266, #52505 ) ) ;
#51302 = DIRECTION ( 'NONE',  ( -1.000000000000000000, 0.000000000000000000, 0.000000000000000000 ) ) ;
#51303 = VERTEX_POINT ( 'NONE', #71055 ) ;
#51304 = LINE ( 'NONE', #34017, #4013 ) ;
#51305 = CARTESIAN_POINT ( 'NONE',  ( 93.67500000000001137, -207.7050326799711968, 84.89354166840095672 ) ) ;
#51306 = CARTESIAN_POINT ( 'NONE',  ( 97.30629616937498838, 90.00000000000002842, 82.49906250086715431 ) ) ;
#51307 = STYLED_ITEM ( 'NONE', ( #42028 ), #61761 ) ;
#51308 = CARTESIAN_POINT ( 'NONE',  ( 97.64999999999997726, -208.4700217866474645, 77.67041666666665378 ) ) ;
#51309 = VECTOR ( 'NONE', #50310, 1000.000000000000000 ) ;
#51310 = VERTEX_POINT ( 'NONE', #19921 ) ;
#51311 = VERTEX_POINT ( 'NONE', #65806 ) ;
#51312 = ORIENTED_EDGE ( 'NONE', *, *, #23573, .F. ) ;
#51313 = VERTEX_POINT ( 'NONE', #19192 ) ;
#51314 = DIRECTION ( 'NONE',  ( 0.000000000000000000, 0.000000000000000000, 1.000000000000000000 ) ) ;
#51315 = LINE ( 'NONE', #61875, #59545 ) ;
#51316 = AXIS2_PLACEMENT_3D ( 'NONE', #63208, #34609, #23704 ) ;
#51317 = CARTESIAN_POINT ( 'NONE',  ( 10.00000000000000000, 22.64427369931169309, 30.00120703465213623 ) ) ;
#51318 = CARTESIAN_POINT ( 'NONE',  ( 10.00000000000000000, 0.6853352020795618893, -37.58145647212453611 ) ) ;
#51319 = CIRCLE ( 'NONE', #29681, 31.99999999999999289 ) ;
#51320 = DIRECTION ( 'NONE',  ( 0.000000000000000000, 0.000000000000000000, -1.000000000000000000 ) ) ;
#51321 = DIRECTION ( 'NONE',  ( -1.000000000000000000, -0.000000000000000000, 0.000000000000000000 ) ) ;
#51322 = CYLINDRICAL_SURFACE ( 'NONE', #8019, 77.49899999999999523 ) ;
#51323 = EDGE_LOOP ( 'NONE', ( #41156, #1302, #42085, #2937 ) ) ;
#51324 = CARTESIAN_POINT ( 'NONE',  ( -97.64999999999996305, -209.9999999999999716, 83.09437500173430635 ) ) ;
#51325 = ORIENTED_EDGE ( 'NONE', *, *, #33723, .F. ) ;
#51326 = DIRECTION ( 'NONE',  ( 0.000000000000000000, 0.000000000000000000, -1.000000000000000000 ) ) ;
#51328 = ORIENTED_EDGE ( 'NONE', *, *, #47689, .F. ) ;
#51327 = ADVANCED_FACE ( 'NONE', ( #24469 ), #13183, .T. ) ;
#51330 = CARTESIAN_POINT ( 'NONE',  ( -92.35000000000005116, 91.52997821335253548, 80.28979166840098003 ) ) ;
#51329 = CARTESIAN_POINT ( 'NONE',  ( 97.64999999999999147, 90.00000000000002842, 78.33187500173430351 ) ) ;
#51331 = ORIENTED_EDGE ( 'NONE', *, *, #32942, .F. ) ;
#51332 = CARTESIAN_POINT ( 'NONE',  ( 97.30629616937498838, 90.00000000000002842, 85.03906250086714635 ) ) ;
#51333 = CARTESIAN_POINT ( 'NONE',  ( 0.000000000000000000, -26.23277895567245821, -4.042438405570103477 ) ) ;
#51334 = LINE ( 'NONE', #57357, #34301 ) ;
#51335 = EDGE_CURVE ( 'NONE', #3018, #27662, #42419, .T. ) ;
#51336 = LINE ( 'NONE', #68275, #12191 ) ;
#51337 = DIRECTION ( 'NONE',  ( 1.000000000000000000, 0.000000000000000000, 0.000000000000000000 ) ) ;
#51338 = DIRECTION ( 'NONE',  ( -1.000000000000000000, -0.000000000000000000, 0.000000000000000000 ) ) ;
#51339 = EDGE_LOOP ( 'NONE', ( #69349, #7934, #32750, #48538 ) ) ;
#51340 = DIRECTION ( 'NONE',  ( -1.000000000000000000, -0.000000000000000000, -0.000000000000000000 ) ) ;
#51341 = LINE ( 'NONE', #74278, #28908 ) ;
#51342 = CARTESIAN_POINT ( 'NONE',  ( -23.30023580412278505, -123.4057321492263384, 5.500000000000000000 ) ) ;
#51343 = EDGE_LOOP ( 'NONE', ( #23219, #21341, #25343, #7357 ) ) ;
#51344 = ADVANCED_FACE ( 'NONE', ( #25216 ), #14291, .F. ) ;
#51345 = EDGE_LOOP ( 'NONE', ( #61565, #33921, #26620, #70639 ) ) ;
#51346 = CARTESIAN_POINT ( 'NONE',  ( -92.34999999999999432, -211.5299782133524218, 75.10395833506764518 ) ) ;
#51347 = VECTOR ( 'NONE', #26994, 1000.000000000000000 ) ;
#51348 = EDGE_CURVE ( 'NONE', #65222, #70426, #37241, .T. ) ;
#51349 = LINE ( 'NONE', #17148, #2500 ) ;
#51350 = CARTESIAN_POINT ( 'NONE',  ( 96.66135172262730180, -211.6008015735635865, 74.79754476654878204 ) ) ;
#51351 = DIRECTION ( 'NONE',  ( -1.000000000000000000, -0.000000000000000000, -0.000000000000000000 ) ) ;
#51352 = CARTESIAN_POINT ( 'NONE',  ( -96.15314808468745866, -211.9973110713294489, 81.01739583420049939 ) ) ;
#51353 = ORIENTED_EDGE ( 'NONE', *, *, #72032, .T. ) ;
#51354 = EDGE_CURVE ( 'NONE', #32448, #41826, #11245, .T. ) ;
#51355 = EDGE_LOOP ( 'NONE', ( #55328, #63258, #50000, #70221 ) ) ;
#51356 = CYLINDRICAL_SURFACE ( 'NONE', #33065, 31.99999999999998579 ) ;
#51357 = CARTESIAN_POINT ( 'NONE',  ( 7.103376864691351012E-17, -120.0000000000000000, -64.00000000000000000 ) ) ;
#51358 = CARTESIAN_POINT ( 'NONE',  ( 0.000000000000000000, -81.50828551894234408, 8.966570791700414489 ) ) ;
#51359 = DIRECTION ( 'NONE',  ( 0.000000000000000000, 0.000000000000000000, 1.000000000000000000 ) ) ;
#51360 = CARTESIAN_POINT ( 'NONE',  ( 11.99999999999999822, 76.41127070299273782, 12.93880638057342836 ) ) ;
#51361 = CARTESIAN_POINT ( 'NONE',  ( 96.32499999999998863, 87.70503267997126784, 78.22604166840096696 ) ) ;
#51362 = DIRECTION ( 'NONE',  ( -1.000000000000000000, 0.000000000000000000, -0.000000000000000000 ) ) ;
#51363 = CARTESIAN_POINT ( 'NONE',  ( 0.000000000000000000, -21.32104025579135964, 30.84782396557210760 ) ) ;
#51364 = CARTESIAN_POINT ( 'NONE',  ( 95.00000000002597744, 90.00000000000007105, -75.00000000000000000 ) ) ;
#51365 = EDGE_CURVE ( 'NONE', #51185, #44202, #7298, .T. ) ;
#51366 = DIRECTION ( 'NONE',  ( 0.000000000000000000, 0.9876883405951372152, 0.1564344650402346160 ) ) ;
#51367 = EDGE_CURVE ( 'NONE', #55201, #56506, #48871, .T. ) ;
#51368 = AXIS2_PLACEMENT_3D ( 'NONE', #67965, #67220, #39775 ) ;
#51369 = CARTESIAN_POINT ( 'NONE',  ( 94.99999999999998579, 92.66308142843932671, 86.46781250086714010 ) ) ;
#51370 = AXIS2_PLACEMENT_3D ( 'NONE', #63054, #52110, #45005 ) ;
#51371 = CARTESIAN_POINT ( 'NONE',  ( -92.69370383062498320, -211.3315407142195852, 88.79614583420048746 ) ) ;
#51372 = CARTESIAN_POINT ( 'NONE',  ( 97.64999999999999147, 90.00000000000002842, 82.69749999999999091 ) ) ;
#51373 = ORIENTED_EDGE ( 'NONE', *, *, #54571, .T. ) ;
#51374 = CARTESIAN_POINT ( 'NONE',  ( 11.99999999999999822, 59.03961581697399907, 46.53671651293969802 ) ) ;
#51375 = CARTESIAN_POINT ( 'NONE',  ( -96.15314808468751551, 88.00268892867056536, 80.85864583420047325 ) ) ;
#51376 = AXIS2_PLACEMENT_3D ( 'NONE', #71962, #55049, #2848 ) ;
#51377 = CIRCLE ( 'NONE', #56162, 37.49900000000000944 ) ;
#51378 = DIRECTION ( 'NONE',  ( -1.000000000000000000, -0.000000000000000000, -0.000000000000000000 ) ) ;
#51379 = ORIENTED_EDGE ( 'NONE', *, *, #38976, .T. ) ;
#51380 = CARTESIAN_POINT ( 'NONE',  ( 92.35000000021534561, -209.9999789922616458, 79.91868729553134187 ) ) ;
#51381 = FACE_OUTER_BOUND ( 'NONE', #15632, .T. ) ;
#51382 = FACE_OUTER_BOUND ( 'NONE', #23991, .T. ) ;
#51383 = CARTESIAN_POINT ( 'NONE',  ( -97.64999999999993463, -208.4700217866474361, 84.86708333333332632 ) ) ;
#51384 = CARTESIAN_POINT ( 'NONE',  ( 96.15314808468750130, -211.9973110713294489, 75.40822916753381833 ) ) ;
#51385 = AXIS2_PLACEMENT_3D ( 'NONE', #39043, #73238, #67610 ) ;
#51386 = ORIENTED_EDGE ( 'NONE', *, *, #9695, .F. ) ;
#51387 = VERTEX_POINT ( 'NONE', #71789 ) ;
#51388 = CIRCLE ( 'NONE', #63434, 15.99999999999999822 ) ;
#51389 = AXIS2_PLACEMENT_3D ( 'NONE', #2410, #47491, #42231 ) ;
#51390 = CARTESIAN_POINT ( 'NONE',  ( 95.00000000000000000, -207.3369185715606307, 85.83281250086717762 ) ) ;
#51391 = CARTESIAN_POINT ( 'NONE',  ( 11.99999999999999822, 0.000000000000000000, 77.49899999999999523 ) ) ;
#51392 = DIRECTION ( 'NONE',  ( 0.000000000000000000, 0.000000000000000000, 1.000000000000000000 ) ) ;
#51393 = CIRCLE ( 'NONE', #65797, 82.00000000000000000 ) ;
#51394 = DIRECTION ( 'NONE',  ( 0.000000000000000000, 0.000000000000000000, 1.000000000000000000 ) ) ;
#51395 = CARTESIAN_POINT ( 'NONE',  ( 93.67500000000001137, -212.2949673200287179, 76.77083333333332860 ) ) ;
#51396 = CYLINDRICAL_SURFACE ( 'NONE', #26112, 42.00000000000000000 ) ;
#51397 = CARTESIAN_POINT ( 'NONE',  ( 97.64999999999999147, -209.9999999999999716, 88.41249999999999432 ) ) ;
#51398 = EDGE_CURVE ( 'NONE', #26897, #33925, #53045, .T. ) ;
#51399 = ORIENTED_EDGE ( 'NONE', *, *, #29959, .T. ) ;
#51400 = EDGE_LOOP ( 'NONE', ( #5880, #11585, #2558, #27065 ) ) ;
#51401 = ORIENTED_EDGE ( 'NONE', *, *, #41853, .T. ) ;
#51402 = EDGE_LOOP ( 'NONE', ( #23034, #26279, #53276, #67413 ) ) ;
#51403 = CARTESIAN_POINT ( 'NONE',  ( 95.00000000000000000, -209.9999999999999716, 90.00000000000000000 ) ) ;
#51404 =( LENGTH_UNIT ( ) NAMED_UNIT ( * ) SI_UNIT ( .MILLI., .METRE. ) );
#51405 = CARTESIAN_POINT ( 'NONE',  ( 5.000000000000000000, 2.886751345948137981, -5.553418012614792509 ) ) ;
#51406 = ADVANCED_FACE ( 'NONE', ( #30097 ), #7913, .F. ) ;
#51407 = CARTESIAN_POINT ( 'NONE',  ( 97.64999999999999147, 90.00000000000002842, 87.77749999999998920 ) ) ;
#51408 = CARTESIAN_POINT ( 'NONE',  ( 96.32499999999998863, -207.7050326799711968, 78.43770833506764006 ) ) ;
#51409 = CARTESIAN_POINT ( 'NONE',  ( 97.64999999999997726, 91.52997821335252127, 82.11541666666666117 ) ) ;
#51410 = ADVANCED_FACE ( 'NONE', ( #18811 ), #41751, .T. ) ;
#51411 = ORIENTED_EDGE ( 'NONE', *, *, #53495, .F. ) ;
#51412 = DIRECTION ( 'NONE',  ( 0.000000000000000000, 0.000000000000000000, 1.000000000000000000 ) ) ;
#51413 = ORIENTED_EDGE ( 'NONE', *, *, #49659, .T. ) ;
#51414 = DIRECTION ( 'NONE',  ( -1.000000000000000000, 0.000000000000000000, 0.000000000000000000 ) ) ;
#51415 = EDGE_LOOP ( 'NONE', ( #33174, #40811, #23861, #46167 ) ) ;
#51416 = DIRECTION ( 'NONE',  ( 0.000000000000000000, -0.07845909572785220165, 0.9969173337331274087 ) ) ;
#51417 =( BOUNDED_CURVE ( )  B_SPLINE_CURVE ( 2, ( #43263, #25213, #7549, #59798, #24831, #30829, #2316 ),
 .UNSPECIFIED., .F., .F. ) 
 B_SPLINE_CURVE_WITH_KNOTS ( ( 3, 2, 2, 3 ),
 ( 0.8125000000000002220, 0.8194444444444446418, 0.8263888888888889506, 0.8333333333333334814 ),
 .UNSPECIFIED. ) 
 CURVE ( )  GEOMETRIC_REPRESENTATION_ITEM ( )  RATIONAL_B_SPLINE_CURVE ( ( 0.9999999999999956701, 0.8660254037844430375, 1.000000000000000000, 0.8660254037844387076, 1.000000000000000000, 0.8660254037844365982, 1.000000000000002220 ) ) 
 REPRESENTATION_ITEM ( '' )  );
#51418 = CARTESIAN_POINT ( 'NONE',  ( -93.84685191531252713, 88.00268892867056536, 82.39322916753381776 ) ) ;
#51419 = CARTESIAN_POINT ( 'NONE',  ( 94.99999999999998579, 87.33691857156068750, 77.10156250086711793 ) ) ;
#51420 = VERTEX_POINT ( 'NONE', #59423 ) ;
#51421 = CARTESIAN_POINT ( 'NONE',  ( 5.000000000000000000, 35.47612816024523852, 22.48208911017513145 ) ) ;
#51422 = VECTOR ( 'NONE', #30275, 1000.000000000000000 ) ;
#51423 = CIRCLE ( 'NONE', #31021, 77.49899999999999523 ) ;
#51424 = EDGE_CURVE ( 'NONE', #44177, #60576, #30831, .T. ) ;
#51425 = CARTESIAN_POINT ( 'NONE',  ( 10.00000000000000000, -40.68715046381937128, 10.41901085202062660 ) ) ;
#51426 = CARTESIAN_POINT ( 'NONE',  ( 93.67500000000001137, -212.2949673200287179, 85.66083333333332916 ) ) ;
#51427 = CARTESIAN_POINT ( 'NONE',  ( 5.000000000000002665, 78.73519480814955784, 22.90783923731657268 ) ) ;
#51428 = ORIENTED_EDGE ( 'NONE', *, *, #43732, .F. ) ;
#51429 = CARTESIAN_POINT ( 'NONE',  ( 10.00000000000000000, -62.50329211542465657, 41.76937507738766442 ) ) ;
#51430 = CARTESIAN_POINT ( 'NONE',  ( -97.30629616937495996, -209.9999999999999716, 77.57781250086713953 ) ) ;
#51431 = ORIENTED_EDGE ( 'NONE', *, *, #20955, .T. ) ;
#51432 = AXIS2_PLACEMENT_3D ( 'NONE', #19635, #31287, #42580 ) ;
#51433 = VERTEX_POINT ( 'NONE', #67941 ) ;
#51434 = FACE_BOUND ( 'NONE', #50585, .T. ) ;
#51435 = ORIENTED_EDGE ( 'NONE', *, *, #74205, .T. ) ;
#51436 = CARTESIAN_POINT ( 'NONE',  ( 0.000000000000000000, 0.000000000000000000, 0.000000000000000000 ) ) ;
#51437 = DIRECTION ( 'NONE',  ( 0.000000000000000000, 0.000000000000000000, -1.000000000000000000 ) ) ;
#51438 = ORIENTED_EDGE ( 'NONE', *, *, #2033, .T. ) ;
#51439 = CARTESIAN_POINT ( 'NONE',  ( -94.99999999999997158, -212.6630814284392557, 75.83156250086715033 ) ) ;
#51440 = ORIENTED_EDGE ( 'NONE', *, *, #66540, .F. ) ;
#51442 = EDGE_CURVE ( 'NONE', #44231, #48627, #49641, .T. ) ;
#51441 = CARTESIAN_POINT ( 'NONE',  ( 10.00000000000000000, 35.92658777277511462, 10.74501242461295014 ) ) ;
#51443 = DIRECTION ( 'NONE',  ( 0.000000000000000000, -0.9876883405951358830, -0.1564344650402421932 ) ) ;
#51444 = CARTESIAN_POINT ( 'NONE',  ( 12.00000000000000000, -3.948201729842355068, -23.21447184625292692 ) ) ;
#51445 = CARTESIAN_POINT ( 'NONE',  ( 0.000000000000000000, 0.000000000000000000, 0.000000000000000000 ) ) ;
#51446 = CIRCLE ( 'NONE', #1107, 12.74999999999999822 ) ;
#51447 = DIRECTION ( 'NONE',  ( 0.000000000000000000, -0.9510565162951544194, -0.3090169943749450643 ) ) ;
#51448 = AXIS2_PLACEMENT_3D ( 'NONE', #67500, #44949, #67871 ) ;
#51449 = CYLINDRICAL_SURFACE ( 'NONE', #44535, 42.00000000000000000 ) ;
#51450 = CARTESIAN_POINT ( 'NONE',  ( 92.69370383062498320, 88.66845928578035796, 83.98072916753380923 ) ) ;
#51451 = CARTESIAN_POINT ( 'NONE',  ( -10.90076147243505211, 0.000000000000000000, 0.000000000000000000 ) ) ;
#51452 = CARTESIAN_POINT ( 'NONE',  ( -7.499999999999968914, 79.99999999999998579, -269.9999999999999432 ) ) ;
#51453 = FACE_OUTER_BOUND ( 'NONE', #25416, .T. ) ;
#51454 = AXIS2_PLACEMENT_3D ( 'NONE', #43285, #7573, #37632 ) ;
#51455 = CARTESIAN_POINT ( 'NONE',  ( -5.000000000000000000, 1.101175676120956348, -0.7375066809288767233 ) ) ;
#51456 = VECTOR ( 'NONE', #50627, 1000.000000000000000 ) ;
#51457 = FACE_OUTER_BOUND ( 'NONE', #55542, .T. ) ;
#51458 = EDGE_CURVE ( 'NONE', #25082, #17154, #36454, .T. ) ;
#51459 = CARTESIAN_POINT ( 'NONE',  ( 2.008727693139922721, 4.613763217533267458, -0.5592653008974296514 ) ) ;
#51460 = DIRECTION ( 'NONE',  ( -1.000000000000000000, 0.000000000000000000, 0.000000000000000000 ) ) ;
#51461 = EDGE_CURVE ( 'NONE', #57911, #51433, #494, .T. ) ;
#51462 = AXIS2_PLACEMENT_3D ( 'NONE', #4151, #27047, #49981 ) ;
#51463 = DIRECTION ( 'NONE',  ( 0.000000000000000000, 0.6494480483301793283, 0.7604059656000345946 ) ) ;
#51464 = EDGE_CURVE ( 'NONE', #24628, #52585, #67649, .T. ) ;
#51465 = CARTESIAN_POINT ( 'NONE',  ( 0.000000000000000000, -12.93880638057369659, 76.41127070299266677 ) ) ;
#51466 = LINE ( 'NONE', #57859, #9752 ) ;
#51467 = CARTESIAN_POINT ( 'NONE',  ( -97.30629616937501680, 91.33154071421968467, 89.58989583420047609 ) ) ;
#51468 = DIRECTION ( 'NONE',  ( -8.119982227976398872E-16, -1.065814103640131188E-14, -1.000000000000000000 ) ) ;
#51469 = VECTOR ( 'NONE', #55400, 1000.000000000000000 ) ;
#51470 = CARTESIAN_POINT ( 'NONE',  ( -96.32500000000001705, 87.70503267997129626, 79.94583333333332575 ) ) ;
#51471 = ORIENTED_EDGE ( 'NONE', *, *, #6066, .T. ) ;
#51472 = AXIS2_PLACEMENT_3D ( 'NONE', #18947, #59189, #31707 ) ;
#51473 = DIRECTION ( 'NONE',  ( 1.000000000000000000, -0.000000000000000000, 0.000000000000000000 ) ) ;
#51474 = CARTESIAN_POINT ( 'NONE',  ( 0.000000000000000000, 24.81905959214261514, 9.408202855044827118 ) ) ;
#51475 = AXIS2_PLACEMENT_3D ( 'NONE', #60630, #19643, #36943 ) ;
#51476 = AXIS2_PLACEMENT_3D ( 'NONE', #39835, #52572, #28527 ) ;
#51477 = CARTESIAN_POINT ( 'NONE',  ( 0.000000000000000000, 8.688484142253939169, 21.88630264137371029 ) ) ;
#51478 = CARTESIAN_POINT ( 'NONE',  ( 96.15314808468748708, -208.0026889286704943, 85.14489583420048291 ) ) ;
#51479 = AXIS2_PLACEMENT_3D ( 'NONE', #33887, #57937, #69215 ) ;
#51480 = VECTOR ( 'NONE', #5641, 1000.000000000000114 ) ;
#51481 = VERTEX_POINT ( 'NONE', #74312 ) ;
#51482 = ORIENTED_EDGE ( 'NONE', *, *, #30855, .T. ) ;
#51483 = CARTESIAN_POINT ( 'NONE',  ( -97.64999999999996305, -209.9999999999999716, 87.45999999999999375 ) ) ;
#51484 = ORIENTED_EDGE ( 'NONE', *, *, #42193, .F. ) ;
#51485 = CARTESIAN_POINT ( 'NONE',  ( 11.99999999999999822, 18.89407956138362010, -75.16055320797013906 ) ) ;
#51486 = CARTESIAN_POINT ( 'NONE',  ( 97.30629616937498838, -208.6684592857803295, 77.94822916753381037 ) ) ;
#51487 = ORIENTED_EDGE ( 'NONE', *, *, #4273, .F. ) ;
#51488 = CARTESIAN_POINT ( 'NONE',  ( 93.84685191531249870, -208.0026889286704943, 81.44072916753381719 ) ) ;
#51489 = CIRCLE ( 'NONE', #32435, 15.99999999999999645 ) ;
#51490 = AXIS2_PLACEMENT_3D ( 'NONE', #71026, #7151, #1188 ) ;
#51491 = ADVANCED_FACE ( 'NONE', ( #62306 ), #32790, .T. ) ;
#51492 = ORIENTED_EDGE ( 'NONE', *, *, #74282, .F. ) ;
#51493 = DIRECTION ( 'NONE',  ( -0.000000000000000000, 0.5000000000000003331, -0.8660254037844384856 ) ) ;
#51494 = ORIENTED_EDGE ( 'NONE', *, *, #6731, .F. ) ;
#51495 = ORIENTED_EDGE ( 'NONE', *, *, #10504, .F. ) ;
#51496 = CARTESIAN_POINT ( 'NONE',  ( -93.84685191531252713, 88.00268892867056536, 75.40822916753381833 ) ) ;
#51497 = VECTOR ( 'NONE', #36490, 1000.000000000000000 ) ;
#51498 = CIRCLE ( 'NONE', #3491, 31.99999999999998579 ) ;
#51499 = CARTESIAN_POINT ( 'NONE',  ( -23.54415474984308787, -120.4156646670583086, -5.500000000000000000 ) ) ;
#51500 = ADVANCED_FACE ( 'NONE', ( #40107 ), #63061, .T. ) ;
#51501 = AXIS2_PLACEMENT_3D ( 'NONE', #50659, #67590, #37908 ) ;
#51502 = VERTEX_POINT ( 'NONE', #57395 ) ;
#51503 = CARTESIAN_POINT ( 'NONE',  ( -21.67772167707813935, -110.8034581014852762, 5.500000000000000000 ) ) ;
#51504 = CARTESIAN_POINT ( 'NONE',  ( 92.35000000000002274, -208.4700217866474645, 86.85145833506763324 ) ) ;
#51505 = CIRCLE ( 'NONE', #53871, 31.99999999999998934 ) ;
#51506 = ADVANCED_FACE ( 'NONE', ( #3408 ), #11164, .T. ) ;
#51507 = ORIENTED_EDGE ( 'NONE', *, *, #26233, .T. ) ;
#51508 = CARTESIAN_POINT ( 'NONE',  ( 10.00000000000000000, -55.19960302592029677, -51.03279382321147750 ) ) ;
#51509 = ORIENTED_EDGE ( 'NONE', *, *, #52108, .T. ) ;
#51510 = MECHANICAL_DESIGN_GEOMETRIC_PRESENTATION_REPRESENTATION (  '', ( #20266 ), #71890 ) ;
#51511 = CARTESIAN_POINT ( 'NONE',  ( 0.000000000000000000, 80.28980883073781172, -16.65972982744850128 ) ) ;
#51512 = VERTEX_POINT ( 'NONE', #23191 ) ;
#51513 = EDGE_CURVE ( 'NONE', #54682, #59396, #53256, .T. ) ;
#51514 = ORIENTED_EDGE ( 'NONE', *, *, #3779, .T. ) ;
#51515 = ORIENTED_EDGE ( 'NONE', *, *, #34472, .T. ) ;
#51516 = DIRECTION ( 'NONE',  ( -1.000000000000000000, 0.000000000000000000, -0.000000000000000000 ) ) ;
#51517 = CARTESIAN_POINT ( 'NONE',  ( 0.000000000000000000, 0.000000000000000000, -125.0000000000000000 ) ) ;
#51518 = ORIENTED_EDGE ( 'NONE', *, *, #19096, .T. ) ;
#51519 = ORIENTED_EDGE ( 'NONE', *, *, #22151, .F. ) ;
#51520 = VERTEX_POINT ( 'NONE', #50631 ) ;
#51521 = DIRECTION ( 'NONE',  ( 0.000000000000000000, 0.000000000000000000, -1.000000000000000000 ) ) ;
#51522 = CARTESIAN_POINT ( 'NONE',  ( -94.99999999999997158, -206.9400435732949575, 88.57124999999999204 ) ) ;
#51524 = CARTESIAN_POINT ( 'NONE',  ( -97.65000000000001990, 88.47002178664754979, 86.87791666666664980 ) ) ;
#51523 = VECTOR ( 'NONE', #37298, 1000.000000000000114 ) ;
#51525 = ORIENTED_EDGE ( 'NONE', *, *, #66821, .F. ) ;
#51526 = FACE_OUTER_BOUND ( 'NONE', #14486, .T. ) ;
#51527 = EDGE_LOOP ( 'NONE', ( #16956, #43290, #12315, #27748 ) ) ;
#51528 = DIRECTION ( 'NONE',  ( 0.000000000000000000, 0.000000000000000000, 1.000000000000000000 ) ) ;
#51529 = CARTESIAN_POINT ( 'NONE',  ( -97.30629616937497417, -211.3315407142195852, 85.88572916753382458 ) ) ;
#51530 = VERTEX_POINT ( 'NONE', #54884 ) ;
#51531 = CIRCLE ( 'NONE', #64737, 32.00000000000000000 ) ;
#51533 = EDGE_CURVE ( 'NONE', #14021, #58339, #49241, .T. ) ;
#51532 = CARTESIAN_POINT ( 'NONE',  ( 32.50000000000000000, -120.0000000000000000, 102.9091629284897493 ) ) ;
#51534 = DIRECTION ( 'NONE',  ( 0.000000000000000000, -0.7431448254773878048, 0.6691306063588654540 ) ) ;
#51535 = CARTESIAN_POINT ( 'NONE',  ( 10.00000000000000000, -37.22597642581153821, -5.202137450156795850 ) ) ;
#51536 = CARTESIAN_POINT ( 'NONE',  ( -92.69370383062498320, -211.3315407142195852, 75.30239583420048177 ) ) ;
#51537 = CIRCLE ( 'NONE', #8276, 16.00000000000000000 ) ;
#51538 = VECTOR ( 'NONE', #48665, 1000.000000000000000 ) ;
#51539 = VECTOR ( 'NONE', #3290, 1000.000000000000000 ) ;
#51540 = DIRECTION ( 'NONE',  ( -0.000000000000000000, -0.000000000000000000, 1.000000000000000000 ) ) ;
#51541 = PLANE ( 'NONE',  #29473 ) ;
#51542 = DIRECTION ( 'NONE',  ( -1.000000000000000000, -0.000000000000000000, -0.000000000000000000 ) ) ;
#51543 = AXIS2_PLACEMENT_3D ( 'NONE', #49980, #56391, #67663 ) ;
#51544 = LINE ( 'NONE', #99, #69947 ) ;
#51545 = CARTESIAN_POINT ( 'NONE',  ( 94.99999999999998579, 86.94004357329502852, 80.07812500173429271 ) ) ;
#51546 = EDGE_CURVE ( 'NONE', #28466, #54954, #68688, .T. ) ;
#51547 = CARTESIAN_POINT ( 'NONE',  ( -92.69370383062504004, 90.00000000000004263, 79.80031250086713612 ) ) ;
#51548 = CARTESIAN_POINT ( 'NONE',  ( 10.00000000000000000, 0.000000000000000000, 0.000000000000000000 ) ) ;
#51549 = CARTESIAN_POINT ( 'NONE',  ( 10.00000000000000000, 74.65491531819118620, 23.16904090965733332 ) ) ;
#51550 = EDGE_CURVE ( 'NONE', #31993, #25646, #5171, .T. ) ;
#51551 = ORIENTED_EDGE ( 'NONE', *, *, #72943, .F. ) ;
#51552 = FACE_BOUND ( 'NONE', #50514, .T. ) ;
#51553 = AXIS2_PLACEMENT_3D ( 'NONE', #51436, #11577, #39803 ) ;
#51554 = DIRECTION ( 'NONE',  ( 0.000000000000000000, -0.1564344650402170189, -0.9876883405951399908 ) ) ;
#51556 = CARTESIAN_POINT ( 'NONE',  ( 92.35000000019411459, -210.0000198427945861, 86.27002759516706476 ) ) ;
#51555 = VECTOR ( 'NONE', #32544, 1000.000000000000000 ) ;
#51557 = CIRCLE ( 'NONE', #35936, 31.99999999999998934 ) ;
#51558 = CARTESIAN_POINT ( 'NONE',  ( 10.00000000000000000, 46.53671651294032330, -59.03961581697353012 ) ) ;
#51559 = CARTESIAN_POINT ( 'NONE',  ( -3.000000000000000000, 6.762365576493643893, -25.66652317338391853 ) ) ;
#51560 = CARTESIAN_POINT ( 'NONE',  ( 3.000000000000000000, -2.935248768560059673, 2.602085213965210642E-15 ) ) ;
#51561 = CARTESIAN_POINT ( 'NONE',  ( -96.15314808468747287, -208.0026889286704943, 80.80572916753382628 ) ) ;
#51562 = AXIS2_PLACEMENT_3D ( 'NONE', #68343, #964, #30230 ) ;
#51563 = AXIS2_PLACEMENT_3D ( 'NONE', #13189, #12810, #53053 ) ;
#51564 = CARTESIAN_POINT ( 'NONE',  ( 0.000000000000000000, -34.44570377933549565, -69.42325613327476219 ) ) ;
#51565 = ORIENTED_EDGE ( 'NONE', *, *, #56006, .F. ) ;
#51566 = CARTESIAN_POINT ( 'NONE',  ( 10.00000000000000000, 0.000000000000000000, 0.000000000000000000 ) ) ;
#51567 = CARTESIAN_POINT ( 'NONE',  ( -92.35000000000003695, 90.00000000000004263, 90.00000000000000000 ) ) ;
#51568 = CARTESIAN_POINT ( 'NONE',  ( 97.64999999999999147, -209.9999999999999716, 81.42749999999999488 ) ) ;
#51569 = FACE_OUTER_BOUND ( 'NONE', #5736, .T. ) ;
#51570 = DIRECTION ( 'NONE',  ( 1.000000000000000000, 0.000000000000000000, 0.000000000000000000 ) ) ;
#51571 = VERTEX_POINT ( 'NONE', #73558 ) ;
#51572 = DIRECTION ( 'NONE',  ( 1.000000000000000000, -0.000000000000000000, -0.000000000000000000 ) ) ;
#51573 = DIRECTION ( 'NONE',  ( 0.000000000000000000, 0.000000000000000000, -1.000000000000000000 ) ) ;
#51574 = ORIENTED_EDGE ( 'NONE', *, *, #31396, .F. ) ;
#51575 = CARTESIAN_POINT ( 'NONE',  ( 93.84685191531251292, -211.9973110713294489, 89.11364583420048291 ) ) ;
#51576 = DIRECTION ( 'NONE',  ( -8.326672684688524170E-16, -1.065814103640131188E-14, -1.000000000000000000 ) ) ;
#51577 = ORIENTED_EDGE ( 'NONE', *, *, #65900, .F. ) ;
#51578 = VECTOR ( 'NONE', #49401, 1000.000000000000227 ) ;
#51579 = EDGE_CURVE ( 'NONE', #18566, #63634, #66182, .T. ) ;
#51580 = CYLINDRICAL_SURFACE ( 'NONE', #47650, 31.99999999999998579 ) ;
#51581 = AXIS2_PLACEMENT_3D ( 'NONE', #8351, #71114, #71484 ) ;
#51582 = ORIENTED_EDGE ( 'NONE', *, *, #20360, .F. ) ;
#51583 = EDGE_LOOP ( 'NONE', ( #6164, #12845, #15068, #36151 ) ) ;
#51584 = CARTESIAN_POINT ( 'NONE',  ( -97.64999999999996305, -211.5299782133524218, 79.97229166840095615 ) ) ;
#51585 = ADVANCED_FACE ( 'NONE', ( #20673 ), #43626, .F. ) ;
#51586 = ORIENTED_EDGE ( 'NONE', *, *, #9424, .T. ) ;
#51587 = CARTESIAN_POINT ( 'NONE',  ( 0.000000000000000000, -16.23288003029473359, -33.80338159004301701 ) ) ;
#51588 = VERTEX_POINT ( 'NONE', #45014 ) ;
#51589 = CIRCLE ( 'NONE', #59989, 16.00000000000000000 ) ;
#51590 = EDGE_CURVE ( 'NONE', #70614, #34322, #16011, .T. ) ;
#51591 = ORIENTED_EDGE ( 'NONE', *, *, #66295, .T. ) ;
#51592 = CARTESIAN_POINT ( 'NONE',  ( -94.99999999999997158, -209.9999999999999716, 90.00000000000000000 ) ) ;
#51593 = ORIENTED_EDGE ( 'NONE', *, *, #17168, .F. ) ;
#51594 = ORIENTED_EDGE ( 'NONE', *, *, #38720, .F. ) ;
#51595 = CARTESIAN_POINT ( 'NONE',  ( 94.87443773336545405, 87.35320520944273426, 74.99648857272264024 ) ) ;
#51596 = DIRECTION ( 'NONE',  ( 0.000000000000000000, 0.000000000000000000, -1.000000000000000000 ) ) ;
#51597 = ORIENTED_EDGE ( 'NONE', *, *, #19947, .F. ) ;
#51598 = CIRCLE ( 'NONE', #73211, 12.49999999999999645 ) ;
#51599 = EDGE_CURVE ( 'NONE', #4312, #24083, #51014, .T. ) ;
#51600 = ORIENTED_EDGE ( 'NONE', *, *, #35635, .F. ) ;
#51601 = CARTESIAN_POINT ( 'NONE',  ( 94.99999999999998579, 87.33691857156068750, 86.62656250086715204 ) ) ;
#51602 = ORIENTED_EDGE ( 'NONE', *, *, #56784, .T. ) ;
#51603 = AXIS2_PLACEMENT_3D ( 'NONE', #52768, #63695, #55906 ) ;
#51604 = CARTESIAN_POINT ( 'NONE',  ( 96.15314808468750130, -211.9973110713294489, 80.32947916753380468 ) ) ;
#51605 = VECTOR ( 'NONE', #51612, 1000.000000000000000 ) ;
#51606 = AXIS2_PLACEMENT_3D ( 'NONE', #50980, #70847, #8072 ) ;
#51607 = APPLICATION_PROTOCOL_DEFINITION ( 'draft international standard', 'automotive_design', 1998, #36427 ) ;
#51608 = CARTESIAN_POINT ( 'NONE',  ( -93.67499999999998295, -212.2949673200287179, 81.40104166840096411 ) ) ;
#51609 = FACE_OUTER_BOUND ( 'NONE', #16215, .T. ) ;
#51610 = FACE_OUTER_BOUND ( 'NONE', #69954, .T. ) ;
#51611 = CARTESIAN_POINT ( 'NONE',  ( 15.00000000000000000, 16.83928648764922542, -16.46020748918050458 ) ) ;
#51612 = DIRECTION ( 'NONE',  ( 1.000000000000000000, -0.000000000000000000, 0.000000000000000000 ) ) ;
#51613 = CARTESIAN_POINT ( 'NONE',  ( 96.32499999999998863, 87.70503267997126784, 85.21104166840096639 ) ) ;
#51614 = CIRCLE ( 'NONE', #40785, 31.99999999999998579 ) ;
#51615 = CARTESIAN_POINT ( 'NONE',  ( -97.30629616937497417, -208.6684592857803011, 85.14489583420048291 ) ) ;
#51616 = CARTESIAN_POINT ( 'NONE',  ( -96.15314808468752972, 91.99731107132950569, 84.61572916753381435 ) ) ;
#51617 = VERTEX_POINT ( 'NONE', #68314 ) ;
#51618 = EDGE_CURVE ( 'NONE', #50744, #18038, #46079, .T. ) ;
#51620 = CARTESIAN_POINT ( 'NONE',  ( -92.69370383062502583, 91.33154071421968467, 86.20322916753382003 ) ) ;
#51619 = CARTESIAN_POINT ( 'NONE',  ( 96.15314808468748708, 91.99731107132950569, 83.71614583420047495 ) ) ;
#51621 = VERTEX_POINT ( 'NONE', #29915 ) ;
#51622 = LINE ( 'NONE', #47102, #37152 ) ;
#51624 = EDGE_CURVE ( 'NONE', #61202, #31529, #29542, .T. ) ;
#51623 = DIRECTION ( 'NONE',  ( -1.000000000000000000, -0.000000000000000000, -0.000000000000000000 ) ) ;
#51625 = CARTESIAN_POINT ( 'NONE',  ( 0.000000000000000000, -2.946379043145784582, -75.11764819372150725 ) ) ;
#51626 = CARTESIAN_POINT ( 'NONE',  ( -6.509281303079589520, -14.89695620656361008, -1.199999999999999956 ) ) ;
#51627 = CARTESIAN_POINT ( 'NONE',  ( -94.99999999999997158, -212.6630814284392557, 87.26156250086714294 ) ) ;
#51628 = CARTESIAN_POINT ( 'NONE',  ( 11.99999999999999822, -35.91791733033525702, 68.67312586194982771 ) ) ;
#51629 = FACE_OUTER_BOUND ( 'NONE', #27766, .T. ) ;
#51630 = DIRECTION ( 'NONE',  ( 0.000000000000000000, 1.000000000000000000, 3.491481338843133355E-15 ) ) ;
#51631 = EDGE_CURVE ( 'NONE', #71207, #52228, #13641, .T. ) ;
#51632 = EDGE_CURVE ( 'NONE', #10248, #52892, #58130, .T. ) ;
#51633 = CARTESIAN_POINT ( 'NONE',  ( 0.000000000000000000, -0.8660254037844384856, -1.500000000000000000 ) ) ;
#51634 = ORIENTED_EDGE ( 'NONE', *, *, #41177, .F. ) ;
#51635 = ORIENTED_EDGE ( 'NONE', *, *, #22615, .F. ) ;
#51636 = CARTESIAN_POINT ( 'NONE',  ( -95.00000000000002842, 93.05995642670501411, 77.77624999999999034 ) ) ;
#51637 = DIRECTION ( 'NONE',  ( -1.000000000000000000, 0.000000000000000000, 0.000000000000000000 ) ) ;
#51638 = EDGE_CURVE ( 'NONE', #16639, #986, #44841, .T. ) ;
#51639 = CARTESIAN_POINT ( 'NONE',  ( 95.00000000000000000, -209.9999999999999716, 90.00000000000000000 ) ) ;
#51640 = CARTESIAN_POINT ( 'NONE',  ( -92.35000000000003695, 90.00000015433754186, 79.60187500750917877 ) ) ;
#51641 = DIRECTION ( 'NONE',  ( 7.959965316982041921E-16, 1.065814103640131188E-14, 1.000000000000000000 ) ) ;
#51642 = LINE ( 'NONE', #10307, #63729 ) ;
#51643 =( BOUNDED_CURVE ( )  B_SPLINE_CURVE ( 2, ( #41293, #35280, #53675, #47663, #7073, #13074, #70209 ),
 .UNSPECIFIED., .F., .F. ) 
 B_SPLINE_CURVE_WITH_KNOTS ( ( 3, 2, 2, 3 ),
 ( 0.5833333333333329263, 0.5902777777777776791, 0.5972222222222223209, 0.6041666666666670737 ),
 .UNSPECIFIED. ) 
 CURVE ( )  GEOMETRIC_REPRESENTATION_ITEM ( )  RATIONAL_B_SPLINE_CURVE ( ( 1.000000000000008660, 0.8660254037844301589, 1.000000000000000000, 0.8660254037844387076, 1.000000000000000000, 0.8660254037844301589, 1.000000000000008660 ) ) 
 REPRESENTATION_ITEM ( '' )  );
#51644 = DIRECTION ( 'NONE',  ( 1.000000000000000000, 0.000000000000000000, 0.000000000000000000 ) ) ;
#51645 = AXIS2_PLACEMENT_3D ( 'NONE', #21519, #67393, #38830 ) ;
#51646 = ORIENTED_EDGE ( 'NONE', *, *, #61563, .T. ) ;
#51647 = CARTESIAN_POINT ( 'NONE',  ( -96.15314808468751551, 88.00268892867056536, 78.31864583420048120 ) ) ;
#51648 = EDGE_CURVE ( 'NONE', #40343, #32004, #23277, .T. ) ;
#51650 = DIRECTION ( 'NONE',  ( -1.000000000000000000, -0.000000000000000000, 0.000000000000000000 ) ) ;
#51649 = VECTOR ( 'NONE', #29430, 1000.000000000000000 ) ;
#51651 = ADVANCED_BREP_SHAPE_REPRESENTATION ( '', ( #61761, #43395 ), #59156 ) ;
#51652 = CARTESIAN_POINT ( 'NONE',  ( -8.826826895187510402, -94.96827758698185562, 5.500000000000000000 ) ) ;
#51653 = DIRECTION ( 'NONE',  ( -1.000000000000000000, 0.000000000000000000, -0.000000000000000000 ) ) ;
#51654 = DIRECTION ( 'NONE',  ( 0.000000000000000000, 0.1564344650402312020, -0.9876883405951376593 ) ) ;
#51655 = AXIS2_PLACEMENT_3D ( 'NONE', #60139, #62745, #39047 ) ;
#51656 = DIRECTION ( 'NONE',  ( -1.000000000000000000, 0.000000000000000000, 0.000000000000000000 ) ) ;
#51657 = CARTESIAN_POINT ( 'NONE',  ( -92.69370383062498320, -209.9999999999999716, 88.84906250086716284 ) ) ;
#51658 = CARTESIAN_POINT ( 'NONE',  ( 97.30629616937498838, 91.33154071421968467, 78.74197916753381321 ) ) ;
#51659 = CARTESIAN_POINT ( 'NONE',  ( -97.30629616937495996, -209.9999999999999716, 80.91156250086716284 ) ) ;
#51660 = CARTESIAN_POINT ( 'NONE',  ( 5.822613034544236399, -142.8165987265839760, 5.500000000000000000 ) ) ;
#51661 = CIRCLE ( 'NONE', #13224, 37.49900000000001654 ) ;
#51662 = ORIENTED_EDGE ( 'NONE', *, *, #59268, .F. ) ;
#51663 = CARTESIAN_POINT ( 'NONE',  ( 12.49999999999999645, 1.530808498934191127E-15, 125.0000000000000000 ) ) ;
#51664 = CARTESIAN_POINT ( 'NONE',  ( -92.34999999999999432, -211.5299782133524502, 75.65958333333333030 ) ) ;
#51665 = CARTESIAN_POINT ( 'NONE',  ( 0.000000000000000000, -15.33399622253423722, -80.55351364060604169 ) ) ;
#51666 = CIRCLE ( 'NONE', #58914, 82.00000000000000000 ) ;
#51667 = AXIS2_PLACEMENT_3D ( 'NONE', #28653, #63266, #70344 ) ;
#51668 = AXIS2_PLACEMENT_3D ( 'NONE', #33529, #55733, #9868 ) ;
#51669 = CARTESIAN_POINT ( 'NONE',  ( -97.30629616937501680, 91.33154071421968467, 76.41364583420049428 ) ) ;
#51670 = CARTESIAN_POINT ( 'NONE',  ( 95.00000000000000000, -212.6630814284392557, 80.27656250086714351 ) ) ;
#51671 = ORIENTED_EDGE ( 'NONE', *, *, #20547, .F. ) ;
#51672 = CARTESIAN_POINT ( 'NONE',  ( 10.00000000000000000, 0.000000000000000000, 0.000000000000000000 ) ) ;
#51673 = VERTEX_POINT ( 'NONE', #35197 ) ;
#51674 = FACE_OUTER_BOUND ( 'NONE', #3074, .T. ) ;
#51675 = EDGE_LOOP ( 'NONE', ( #30947, #15609, #73335, #54546 ) ) ;
#51676 = EDGE_CURVE ( 'NONE', #9142, #45831, #12264, .T. ) ;
#51677 = CIRCLE ( 'NONE', #61289, 16.00000000000000000 ) ;
#51678 = CARTESIAN_POINT ( 'NONE',  ( 10.00000000000000000, -2.946379043146863719, 75.11764819372146462 ) ) ;
#51679 = EDGE_CURVE ( 'NONE', #6029, #1787, #14964, .T. ) ;
#51680 = ORIENTED_EDGE ( 'NONE', *, *, #73675, .T. ) ;
#51681 = EDGE_LOOP ( 'NONE', ( #43871, #16999, #28, #17967 ) ) ;
#51683 = EDGE_CURVE ( 'NONE', #24878, #71079, #22661, .T. ) ;
#51682 = EDGE_LOOP ( 'NONE', ( #13510, #63720, #2439, #12012, #11084, #32440 ) ) ;
#51684 = EDGE_CURVE ( 'NONE', #20558, #60145, #25610, .T. ) ;
#51685 = CARTESIAN_POINT ( 'NONE',  ( -17.50000000000000355, 0.000000000000000000, -20.00000000000000000 ) ) ;
#51686 = ORIENTED_EDGE ( 'NONE', *, *, #15375, .F. ) ;
#51687 = VERTEX_POINT ( 'NONE', #41575 ) ;
#51688 = CARTESIAN_POINT ( 'NONE',  ( 93.84685191531248449, 91.99731107132950569, 83.98072916753382344 ) ) ;
#51689 = DIRECTION ( 'NONE',  ( 1.000000000000000000, 0.000000000000000000, 0.000000000000000000 ) ) ;
#51690 = VERTEX_POINT ( 'NONE', #64152 ) ;
#51691 = ORIENTED_EDGE ( 'NONE', *, *, #10435, .T. ) ;
#51692 = AXIS2_PLACEMENT_3D ( 'NONE', #54055, #19087, #58207 ) ;
#51693 = ORIENTED_EDGE ( 'NONE', *, *, #31196, .F. ) ;
#51694 = ORIENTED_EDGE ( 'NONE', *, *, #43037, .T. ) ;
#51695 = FACE_OUTER_BOUND ( 'NONE', #34481, .T. ) ;
#51696 = VECTOR ( 'NONE', #286, 1000.000000000000000 ) ;
#51697 = DIRECTION ( 'NONE',  ( -2.991080821941227764E-16, -1.441094914046774813E-15, 0.9999999999999998890 ) ) ;
#51698 = CARTESIAN_POINT ( 'NONE',  ( 92.34999999999999432, 90.00000000000002842, 84.28499999999999659 ) ) ;
#51699 = DIRECTION ( 'NONE',  ( -1.000000000000000000, 3.061616997868382648E-16, 0.000000000000000000 ) ) ;
#51700 = EDGE_CURVE ( 'NONE', #58103, #50011, #12627, .T. ) ;
#51701 = CARTESIAN_POINT ( 'NONE',  ( 10.00000000000000000, -59.75363087400112505, 56.15606465354937882 ) ) ;
#51702 = CIRCLE ( 'NONE', #19280, 15.70000000000327312 ) ;
#51703 = CARTESIAN_POINT ( 'NONE',  ( 2.117611129180199558, -93.54218975225703048, -5.500000000000000000 ) ) ;
#51704 = LINE ( 'NONE', #252, #32323 ) ;
#51705 = EDGE_CURVE ( 'NONE', #47354, #44992, #52017, .T. ) ;
#51706 = DIRECTION ( 'NONE',  ( 1.427937372958396981E-15, -1.000000000000000000, 1.065814103640131031E-14 ) ) ;
#51707 = VERTEX_POINT ( 'NONE', #58880 ) ;
#51708 = CARTESIAN_POINT ( 'NONE',  ( -96.32499999999996021, -207.7050326799711968, 82.98854166840096980 ) ) ;
#51709 = VERTEX_POINT ( 'NONE', #70492 ) ;
#51710 = CARTESIAN_POINT ( 'NONE',  ( 0.000000000000000000, 0.000000000000000000, -1.199999999999999956 ) ) ;
#51711 = ORIENTED_EDGE ( 'NONE', *, *, #3493, .F. ) ;
#51713 = CARTESIAN_POINT ( 'NONE',  ( -96.32500000000001705, 92.29496732002878900, 77.90854166840097150 ) ) ;
#51712 = CARTESIAN_POINT ( 'NONE',  ( 97.64999999999999147, 90.00000000000002842, 77.69687500173431260 ) ) ;
#51714 = ORIENTED_EDGE ( 'NONE', *, *, #7025, .T. ) ;
#51715 = CARTESIAN_POINT ( 'NONE',  ( 97.30629616937498838, 88.66845928578037217, 78.63614583420049087 ) ) ;
#51716 = DIRECTION ( 'NONE',  ( 4.476705744456278560E-17, -1.000000000000000000, 8.723836835350694626E-17 ) ) ;
#51717 = DIRECTION ( 'NONE',  ( 1.000000000000000000, 0.000000000000000000, 0.000000000000000000 ) ) ;
#51718 = VECTOR ( 'NONE', #73263, 1000.000000000000000 ) ;
#51719 = LINE ( 'NONE', #57737, #25846 ) ;
#51720 = VERTEX_POINT ( 'NONE', #53598 ) ;
#51721 = DIRECTION ( 'NONE',  ( 1.000000000000000000, -0.000000000000000000, -0.000000000000000000 ) ) ;
#51722 = CARTESIAN_POINT ( 'NONE',  ( -3.000000000000000000, 23.50000000000000000, -1.500000000000001332 ) ) ;
#51723 = B_SPLINE_CURVE_WITH_KNOTS ( 'NONE', 3,
 ( #11398, #23069, #68925, #52736, #1286, #25640 ),
 .UNSPECIFIED., .F., .F.,
 ( 4, 2, 4 ),
 ( 0.008070708573309213693, 0.009531758523483287518, 0.01099280847365736134 ),
 .UNSPECIFIED. ) ;
#51724 = VECTOR ( 'NONE', #71104, 1000.000000000000000 ) ;
#51725 = EDGE_CURVE ( 'NONE', #29601, #46060, #29196, .T. ) ;
#51726 = EDGE_CURVE ( 'NONE', #61246, #56682, #19006, .T. ) ;
#51727 = CARTESIAN_POINT ( 'NONE',  ( 11.99999999999999822, 12.93880638057426502, -76.41127070299258150 ) ) ;
#51728 = EDGE_LOOP ( 'NONE', ( #42467, #7946, #7490, #13330 ) ) ;
#51729 = AXIS2_PLACEMENT_3D ( 'NONE', #57547, #12039, #18057 ) ;
#51730 = ORIENTED_EDGE ( 'NONE', *, *, #743, .T. ) ;
#51731 = DIRECTION ( 'NONE',  ( -1.000000000000000000, 0.000000000000000000, 0.000000000000000000 ) ) ;
#51732 = CARTESIAN_POINT ( 'NONE',  ( 0.000000000000000000, 31.52238457039599595, 27.75498641678753842 ) ) ;
#51733 = DIRECTION ( 'NONE',  ( -0.000000000000000000, -0.000000000000000000, 1.000000000000000000 ) ) ;
#51734 = CARTESIAN_POINT ( 'NONE',  ( -94.99999999999997158, -212.6630814284392557, 82.34031250086714238 ) ) ;
#51735 = ORIENTED_EDGE ( 'NONE', *, *, #6649, .T. ) ;
#51736 = CARTESIAN_POINT ( 'NONE',  ( -12.00000000000000000, 2.123263276254396040E-15, 17.30399999999999849 ) ) ;
#51737 = DIRECTION ( 'NONE',  ( 1.000000000000000000, 0.000000000000000000, -0.000000000000000000 ) ) ;
#51738 = DIRECTION ( 'NONE',  ( 1.000000000000000000, 0.000000000000000000, -0.000000000000000000 ) ) ;
#51739 = CARTESIAN_POINT ( 'NONE',  ( 92.69370383062498320, 90.00000000000002842, 76.30781250086714351 ) ) ;
#51740 = FACE_OUTER_BOUND ( 'NONE', #22049, .T. ) ;
#51741 = CARTESIAN_POINT ( 'NONE',  ( 0.000000000000000000, 0.000000000000000000, 0.000000000000000000 ) ) ;
#51742 = DIRECTION ( 'NONE',  ( 0.000000000000000000, 0.9723699203976773342, -0.2334453638559023381 ) ) ;
#51743 = FACE_OUTER_BOUND ( 'NONE', #17518, .T. ) ;
#51744 = CARTESIAN_POINT ( 'NONE',  ( 0.000000000000000000, 0.000000000000000000, 0.000000000000000000 ) ) ;
#51745 = DIRECTION ( 'NONE',  ( -1.000000000000000000, -0.000000000000000000, -0.000000000000000000 ) ) ;
#51746 = CARTESIAN_POINT ( 'NONE',  ( 97.30629616937498838, 88.66845928578035796, 87.52614583420049144 ) ) ;
#51747 = CARTESIAN_POINT ( 'NONE',  ( 0.000000000000000000, -75.16055320797043748, 18.89407956138229494 ) ) ;
#51748 = CARTESIAN_POINT ( 'NONE',  ( 97.64999999999994884, 88.47002178664752137, 82.64458333333332973 ) ) ;
#51749 = VERTEX_POINT ( 'NONE', #64895 ) ;
#51750 = CIRCLE ( 'NONE', #40925, 31.99999999999998579 ) ;
#51751 = CARTESIAN_POINT ( 'NONE',  ( 15.00000000000000000, -13.04903810567675393, -19.60159698893424718 ) ) ;
#51752 = CIRCLE ( 'NONE', #1406, 16.00000000000000000 ) ;
#51753 = CARTESIAN_POINT ( 'NONE',  ( -93.84685191531254134, 91.99731107132950569, 78.00114583420048575 ) ) ;
#51754 = AXIS2_PLACEMENT_3D ( 'NONE', #32485, #43437, #21196 ) ;
#51755 = DIRECTION ( 'NONE',  ( 0.000000000000000000, 1.000000000000000000, 3.491481338843133355E-15 ) ) ;
#51756 = EDGE_LOOP ( 'NONE', ( #28421, #17374, #47000, #22894 ) ) ;
#51757 = CARTESIAN_POINT ( 'NONE',  ( 0.000000000000000000, 70.53064760720316428, -26.01480285779861035 ) ) ;
#51758 = DIRECTION ( 'NONE',  ( -0.000000000000000000, -0.000000000000000000, 1.000000000000000000 ) ) ;
#51759 = LINE ( 'NONE', #309, #4779 ) ;
#51760 = EDGE_CURVE ( 'NONE', #35341, #47641, #13370, .T. ) ;
#51761 = CIRCLE ( 'NONE', #36135, 42.00000000000000000 ) ;
#51762 = ADVANCED_FACE ( 'NONE', ( #11886 ), #15223, .T. ) ;
#51763 = CARTESIAN_POINT ( 'NONE',  ( 10.00000000000000000, 20.40083707022882820, 72.35432306680490910 ) ) ;
#51765 = CARTESIAN_POINT ( 'NONE',  ( -7.500000000000016875, -80.00000000000001421, -269.9999999999999432 ) ) ;
#51764 = CIRCLE ( 'NONE', #19351, 82.00000000000000000 ) ;
#51766 = EDGE_CURVE ( 'NONE', #39841, #10200, #3237, .T. ) ;
#51767 = VERTEX_POINT ( 'NONE', #43817 ) ;
#51768 = AXIS2_PLACEMENT_3D ( 'NONE', #25481, #70579, #2958 ) ;
#51770 = ORIENTED_EDGE ( 'NONE', *, *, #4006, .T. ) ;
#51769 = SHAPE_REPRESENTATION ( 'ISO 5597-32-4-5_GB_SEALS_TYPE1 32X4X5 L1', ( #43395 ), #72282 ) ;
#51771 = EDGE_CURVE ( 'NONE', #70837, #11203, #66734, .T. ) ;
#51772 = CARTESIAN_POINT ( 'NONE',  ( 93.84685191531251292, -211.9973110713294489, 82.92239583420048632 ) ) ;
#51773 = CARTESIAN_POINT ( 'NONE',  ( -96.32499999999996021, -207.7050326799711968, 81.00416666666666288 ) ) ;
#51774 = CARTESIAN_POINT ( 'NONE',  ( 16.30584220631899228, -140.9432449716519784, -5.500000000000000000 ) ) ;
#51775 = VECTOR ( 'NONE', #21036, 1000.000000000000000 ) ;
#51776 = CARTESIAN_POINT ( 'NONE',  ( 5.000000000000000000, 2.059541880722000506, -1.329159518034687126 ) ) ;
#51777 = EDGE_CURVE ( 'NONE', #38565, #4451, #32509, .T. ) ;
#51778 = LINE ( 'NONE', #62333, #53697 ) ;
#51779 = CARTESIAN_POINT ( 'NONE',  ( 95.00000000000000000, -206.9400435732949575, 89.84125000000000227 ) ) ;
#51780 = EDGE_LOOP ( 'NONE', ( #27067, #16635, #44877, #62064 ) ) ;
#51781 = VERTEX_POINT ( 'NONE', #20860 ) ;
#51782 = EDGE_LOOP ( 'NONE', ( #12923, #29420, #28099, #15435 ) ) ;
#51783 = ORIENTED_EDGE ( 'NONE', *, *, #42775, .T. ) ;
#51784 = CARTESIAN_POINT ( 'NONE',  ( -93.84685191531252713, 88.00268892867056536, 86.83822916753382515 ) ) ;
#51785 = DIRECTION ( 'NONE',  ( 0.000000000000000000, 0.000000000000000000, 1.000000000000000000 ) ) ;
#51786 = CARTESIAN_POINT ( 'NONE',  ( -97.65000000000001990, 90.00000000000004263, 83.65000000000000568 ) ) ;
#51787 = CARTESIAN_POINT ( 'NONE',  ( 97.64999999999997726, -211.5299782133524502, 75.73895833506765030 ) ) ;
#51788 = CARTESIAN_POINT ( 'NONE',  ( 97.64999999999997726, 88.47002178664753558, 80.10458333333332348 ) ) ;
#51789 = EDGE_CURVE ( 'NONE', #24685, #67688, #37801, .T. ) ;
#51790 = EDGE_LOOP ( 'NONE', ( #16409, #29657, #12560, #10856 ) ) ;
#51791 = CARTESIAN_POINT ( 'NONE',  ( 0.000000000000000000, 15.33399622253601713, -80.55351364060572905 ) ) ;
#51792 = ORIENTED_EDGE ( 'NONE', *, *, #68582, .T. ) ;
#51793 = EDGE_CURVE ( 'NONE', #31332, #68814, #59328, .T. ) ;
#51794 = CARTESIAN_POINT ( 'NONE',  ( -93.67499999999998295, -207.7050326799711968, 82.88270833506763324 ) ) ;
#51795 = ORIENTED_EDGE ( 'NONE', *, *, #71382, .T. ) ;
#51796 = CARTESIAN_POINT ( 'NONE',  ( 10.00000000000000000, -70.53064760720336324, 26.01480285779810231 ) ) ;
#51797 = CARTESIAN_POINT ( 'NONE',  ( -93.84685191531254134, 91.99731107132950569, 81.96989583420048575 ) ) ;
#51798 = CARTESIAN_POINT ( 'NONE',  ( 94.99999999999998579, 92.66308142843935514, 75.51406250086714067 ) ) ;
#51799 = EDGE_LOOP ( 'NONE', ( #23956, #13846, #19037, #31737 ) ) ;
#51800 = DIRECTION ( 'NONE',  ( 0.000000000000000000, 0.8910065241883691201, -0.4539904997395446951 ) ) ;
#51801 = DIRECTION ( 'NONE',  ( -0.6064928550163511956, -0.7950889364178798102, 0.000000000000000000 ) ) ;
#51802 = LINE ( 'NONE', #67987, #50973 ) ;
#51803 = VECTOR ( 'NONE', #2386, 1000.000000000000000 ) ;
#51804 = DIRECTION ( 'NONE',  ( 1.000000000000000000, 0.000000000000000000, 0.000000000000000000 ) ) ;
#51805 = VERTEX_POINT ( 'NONE', #42693 ) ;
#51806 = FACE_OUTER_BOUND ( 'NONE', #38551, .T. ) ;
#51807 = CIRCLE ( 'NONE', #46975, 31.99999999999999289 ) ;
#51808 = EDGE_CURVE ( 'NONE', #55194, #66496, #52078, .T. ) ;
#51809 = EDGE_CURVE ( 'NONE', #70414, #2397, #31673, .T. ) ;
#51810 = CARTESIAN_POINT ( 'NONE',  ( -92.69370383062498320, -208.6684592857803011, 79.21822916753380639 ) ) ;
#51811 = VERTEX_POINT ( 'NONE', #42330 ) ;
#51812 = VERTEX_POINT ( 'NONE', #25403 ) ;
#51813 = FACE_BOUND ( 'NONE', #65197, .T. ) ;
#51814 = CIRCLE ( 'NONE', #39801, 77.49899999999999523 ) ;
#51815 = ORIENTED_EDGE ( 'NONE', *, *, #16892, .T. ) ;
#51816 = FACE_OUTER_BOUND ( 'NONE', #7938, .T. ) ;
#51817 = DIRECTION ( 'NONE',  ( 1.000000000000000000, 0.000000000000000000, 0.000000000000000000 ) ) ;
#51818 = ORIENTED_EDGE ( 'NONE', *, *, #7778, .F. ) ;
#51819 = CARTESIAN_POINT ( 'NONE',  ( -93.84685191531248449, -208.0026889286704943, 75.46114583420047950 ) ) ;
#51820 = ORIENTED_EDGE ( 'NONE', *, *, #59353, .F. ) ;
#51821 = DIRECTION ( 'NONE',  ( 0.000000000000000000, 0.000000000000000000, 1.000000000000000000 ) ) ;
#51822 = CARTESIAN_POINT ( 'NONE',  ( -100.0000000000260485, 95.00000000000001421, -75.00000000000000000 ) ) ;
#51823 = LINE ( 'NONE', #68392, #26676 ) ;
#51824 = ORIENTED_EDGE ( 'NONE', *, *, #68495, .F. ) ;
#51825 = DIRECTION ( 'NONE',  ( -1.000000000000000000, -0.000000000000000000, -0.000000000000000000 ) ) ;
#51826 = CIRCLE ( 'NONE', #72192, 16.00000000000000355 ) ;
#51827 = AXIS2_PLACEMENT_3D ( 'NONE', #73973, #39035, #34879 ) ;
#51828 = CARTESIAN_POINT ( 'NONE',  ( 96.15314808468748708, 88.00268892867053694, 83.50447916753381605 ) ) ;
#51829 = FACE_OUTER_BOUND ( 'NONE', #8979, .T. ) ;
#51830 = VECTOR ( 'NONE', #59617, 1000.000000000000000 ) ;
#51831 = FACE_OUTER_BOUND ( 'NONE', #72508, .T. ) ;
#51832 = FACE_OUTER_BOUND ( 'NONE', #48620, .T. ) ;
#51833 = DIRECTION ( 'NONE',  ( 0.000000000000000000, 0.3090169943749411230, 0.9510565162951555296 ) ) ;
#51834 = CARTESIAN_POINT ( 'NONE',  ( 10.00000000000000000, -74.65491531819124305, 8.830959090342128448 ) ) ;
#51835 = CARTESIAN_POINT ( 'NONE',  ( 10.00000000000000000, -22.74946021919153694, 29.81001611431000597 ) ) ;
#51836 = DIRECTION ( 'NONE',  ( -1.000000000000000000, -0.000000000000000000, -0.000000000000000000 ) ) ;
#51837 = CARTESIAN_POINT ( 'NONE',  ( 97.65000000000000568, 88.47002178664753558, 78.83458333333334167 ) ) ;
#51838 = EDGE_CURVE ( 'NONE', #19675, #56878, #38024, .T. ) ;
#51839 = DIRECTION ( 'NONE',  ( 0.000000000000000000, 0.000000000000000000, 1.000000000000000000 ) ) ;
#51840 = CARTESIAN_POINT ( 'NONE',  ( -95.00000000000002842, 92.66308142843932671, 88.21406250086712930 ) ) ;
#51841 = CARTESIAN_POINT ( 'NONE',  ( 0.000000000000000000, 51.29473840253223926, 63.97538442413444670 ) ) ;
#51842 = ADVANCED_FACE ( 'NONE', ( #59619 ), #31025, .T. ) ;
#51843 = ADVANCED_FACE ( 'NONE', ( #8483, #71989 ), #71618, .T. ) ;
#51844 = CARTESIAN_POINT ( 'NONE',  ( 0.000000000000000000, -22.74946021919153694, 29.81001611431000597 ) ) ;
#51845 = PRODUCT_DEFINITION_SHAPE ( 'NONE', 'NONE',  #74353 ) ;
#51846 = ADVANCED_FACE ( 'NONE', ( #65631 ), #3607, .T. ) ;
#51847 = FACE_OUTER_BOUND ( 'NONE', #28281, .T. ) ;
#51848 = DIRECTION ( 'NONE',  ( 0.000000000000000000, 0.000000000000000000, -1.000000000000000000 ) ) ;
#51849 = CARTESIAN_POINT ( 'NONE',  ( 10.00000000000000000, 0.000000000000000000, 0.000000000000000000 ) ) ;
#51850 = EDGE_CURVE ( 'NONE', #67382, #16471, #53978, .T. ) ;
#51851 = CARTESIAN_POINT ( 'NONE',  ( 0.000000000000000000, 0.000000000000000000, -4.400000000000001243 ) ) ;
#51852 = AXIS2_PLACEMENT_3D ( 'NONE', #45912, #6779, #40257 ) ;
#51853 = CARTESIAN_POINT ( 'NONE',  ( 2.500000000000034639, 89.99999999999998579, -279.9999999999999432 ) ) ;
#51854 = CARTESIAN_POINT ( 'NONE',  ( 92.69370383062501162, -209.9999999999999716, 85.99156250086716113 ) ) ;
#51855 = VECTOR ( 'NONE', #23718, 1000.000000000000114 ) ;
#51856 = ORIENTED_EDGE ( 'NONE', *, *, #10623, .T. ) ;
#51857 = ORIENTED_EDGE ( 'NONE', *, *, #72795, .F. ) ;
#51858 = CARTESIAN_POINT ( 'NONE',  ( 10.00000000000000000, 0.000000000000000000, 0.000000000000000000 ) ) ;
#51859 = EDGE_LOOP ( 'NONE', ( #25704, #30668, #59803, #26276 ) ) ;
#51860 = DIRECTION ( 'NONE',  ( -1.000000000000000000, -0.000000000000000000, 0.000000000000000000 ) ) ;
#51861 = VECTOR ( 'NONE', #41165, 1000.000000000000000 ) ;
#51862 =( BOUNDED_CURVE ( )  B_SPLINE_CURVE ( 2, ( #1272, #893, #35782, #164, #23055, #6499, #28297 ),
 .UNSPECIFIED., .F., .F. ) 
 B_SPLINE_CURVE_WITH_KNOTS ( ( 3, 2, 2, 3 ),
 ( 0.04166666666666644231, 0.04861111111111085514, 0.05555555555555525410, 0.06249999999999966693 ),
 .UNSPECIFIED. ) 
 CURVE ( )  GEOMETRIC_REPRESENTATION_ITEM ( )  RATIONAL_B_SPLINE_CURVE ( ( 1.000000000000004219, 0.8660254037844343777, 1.000000000000000000, 0.8660254037844387076, 1.000000000000000000, 0.8660254037844451469, 0.9999999999999935607 ) ) 
 REPRESENTATION_ITEM ( '' )  );
#51863 = B_SPLINE_CURVE_WITH_KNOTS ( 'NONE', 3,
 ( #64572, #46544, #1829, #48025, #13059, #35619 ),
 .UNSPECIFIED., .F., .F.,
 ( 4, 2, 4 ),
 ( 0.008070708573309213693, 0.009531758523483289253, 0.01099280847365736308 ),
 .UNSPECIFIED. ) ;
#51864 = LINE ( 'NONE', #69163, #9982 ) ;
#51865 = EDGE_CURVE ( 'NONE', #46312, #73310, #60517, .T. ) ;
#51866 = ORIENTED_EDGE ( 'NONE', *, *, #25697, .T. ) ;
#51867 = CARTESIAN_POINT ( 'NONE',  ( 97.30629616937498838, -208.6684592857803011, 84.45697916753383083 ) ) ;
#51868 = ORIENTED_EDGE ( 'NONE', *, *, #25058, .F. ) ;
#51869 = DIRECTION ( 'NONE',  ( 0.000000000000000000, -0.4539904997395351471, -0.8910065241883737830 ) ) ;
#51870 = ORIENTED_EDGE ( 'NONE', *, *, #31783, .F. ) ;
#51871 = AXIS2_PLACEMENT_3D ( 'NONE', #63946, #52277, #34994 ) ;
#51872 = VERTEX_POINT ( 'NONE', #2872 ) ;
#51873 = DIRECTION ( 'NONE',  ( 0.000000000000000000, 0.000000000000000000, 1.000000000000000000 ) ) ;
#51874 = UNCERTAINTY_MEASURE_WITH_UNIT (LENGTH_MEASURE( 1.000000000000000082E-05 ), #64731, 'distance_accuracy_value', 'NONE');
#51875 = AXIS2_PLACEMENT_3D ( 'NONE', #24978, #19334, #47914 ) ;
#51876 = DIRECTION ( 'NONE',  ( -0.000000000000000000, -0.000000000000000000, 1.000000000000000000 ) ) ;
#51877 = ORIENTED_EDGE ( 'NONE', *, *, #31831, .F. ) ;
#51878 = CARTESIAN_POINT ( 'NONE',  ( 95.00000000000000000, -209.9999999999999716, 90.00000000000000000 ) ) ;
#51879 = CARTESIAN_POINT ( 'NONE',  ( 96.32499999999998863, -207.7050326799711968, 88.59770833506763665 ) ) ;
#51880 = ADVANCED_FACE ( 'NONE', ( #37434 ), #60367, .T. ) ;
#51881 = ORIENTED_EDGE ( 'NONE', *, *, #58678, .F. ) ;
#51882 = CARTESIAN_POINT ( 'NONE',  ( 5.000000000000000000, 2.886751345948134428, -2.080000000000000071 ) ) ;
#51883 = EDGE_CURVE ( 'NONE', #23196, #28466, #67845, .T. ) ;
#51884 = ORIENTED_EDGE ( 'NONE', *, *, #57459, .F. ) ;
#51885 = DIRECTION ( 'NONE',  ( -1.000000000000000000, -0.000000000000000000, -0.000000000000000000 ) ) ;
#51886 = EDGE_CURVE ( 'NONE', #29642, #51953, #53403, .T. ) ;
#51887 = ORIENTED_EDGE ( 'NONE', *, *, #16210, .F. ) ;
#51888 = ORIENTED_EDGE ( 'NONE', *, *, #14767, .F. ) ;
#51889 = ORIENTED_EDGE ( 'NONE', *, *, #63915, .T. ) ;
#51890 = DIRECTION ( 'NONE',  ( 0.000000000000000000, -0.5877852522924803536, 0.8090169943749422332 ) ) ;
#51891 = CARTESIAN_POINT ( 'NONE',  ( -5.000000000000000000, -4.846777557549235459E-18, -0.5080592402122449114 ) ) ;
#51892 = ORIENTED_EDGE ( 'NONE', *, *, #26329, .T. ) ;
#51893 = ORIENTED_EDGE ( 'NONE', *, *, #68155, .T. ) ;
#51894 = ORIENTED_EDGE ( 'NONE', *, *, #70852, .T. ) ;
#51895 = DIRECTION ( 'NONE',  ( 0.000000000000000000, 0.9510565162951544194, -0.3090169943749446757 ) ) ;
#51896 = DIRECTION ( 'NONE',  ( 0.000000000000000000, -0.9723699203976741146, -0.2334453638559160493 ) ) ;
#51897 = CARTESIAN_POINT ( 'NONE',  ( -95.00000000000002842, 93.05995642670501411, 86.03125000000000000 ) ) ;
#51898 = ORIENTED_EDGE ( 'NONE', *, *, #27313, .F. ) ;
#51899 = DIRECTION ( 'NONE',  ( -1.000000000000000000, -0.000000000000000000, -0.000000000000000000 ) ) ;
#51900 = ORIENTED_EDGE ( 'NONE', *, *, #737, .T. ) ;
#51901 = CYLINDRICAL_SURFACE ( 'NONE', #37214, 77.49899999999999523 ) ;
#51902 = CARTESIAN_POINT ( 'NONE',  ( -96.15314808468745866, -211.9973110713294489, 87.84364583420047268 ) ) ;
#51903 = VERTEX_POINT ( 'NONE', #39279 ) ;
#51904 = CARTESIAN_POINT ( 'NONE',  ( -92.34999999999999432, -211.5299782133524218, 79.54895833506762415 ) ) ;
#51905 = DIRECTION ( 'NONE',  ( 0.000000000000000000, 0.000000000000000000, 1.000000000000000000 ) ) ;
#51906 = CARTESIAN_POINT ( 'NONE',  ( 93.67499999999999716, 87.70503267997126784, 81.21583333333333599 ) ) ;
#51907 = CARTESIAN_POINT ( 'NONE',  ( -96.15314808468745866, -211.9973110713294489, 76.41364583420048007 ) ) ;
#51908 = DIRECTION ( 'NONE',  ( 0.000000000000000000, -0.7071067811865535679, 0.7071067811865414665 ) ) ;
#51909 = CARTESIAN_POINT ( 'NONE',  ( 0.000000000000000000, -33.00180498840035170, -17.80606268964575278 ) ) ;
#51910 = DIRECTION ( 'NONE',  ( 0.000000000000000000, 0.000000000000000000, 1.000000000000000000 ) ) ;
#51911 = CARTESIAN_POINT ( 'NONE',  ( 1.192633404626820770, -120.9097392825245407, 2.500000000000000000 ) ) ;
#51912 = DIRECTION ( 'NONE',  ( -1.000000000000000000, -0.000000000000000000, -0.000000000000000000 ) ) ;
#51914 = EDGE_CURVE ( 'NONE', #19251, #35508, #19650, .T. ) ;
#51913 = CONICAL_SURFACE ( 'NONE', #33930, 5.000000000000000888, 1.047197551196596299 ) ;
#51915 = CARTESIAN_POINT ( 'NONE',  ( -97.30629616937501680, 88.66845928578038638, 76.99572916753380980 ) ) ;
#51916 = DIRECTION ( 'NONE',  ( -1.000000000000000000, 0.000000000000000000, 0.000000000000000000 ) ) ;
#51917 = DIRECTION ( 'NONE',  ( 0.000000000000000000, 0.000000000000000000, 1.000000000000000000 ) ) ;
#51918 = AXIS2_PLACEMENT_3D ( 'NONE', #58937, #35986, #54395 ) ;
#51919 = ORIENTED_EDGE ( 'NONE', *, *, #51809, .T. ) ;
#51920 = DIRECTION ( 'NONE',  ( -0.000000000000000000, -0.000000000000000000, -1.000000000000000000 ) ) ;
#51921 = FACE_OUTER_BOUND ( 'NONE', #16937, .T. ) ;
#51922 = FACE_OUTER_BOUND ( 'NONE', #10284, .T. ) ;
#51923 = CIRCLE ( 'NONE', #21924, 31.99999999999999289 ) ;
#51924 = CARTESIAN_POINT ( 'NONE',  ( 0.000000000000000000, 75.16055320797030959, 18.89407956138283851 ) ) ;
#51925 = DIRECTION ( 'NONE',  ( 0.3311129884571280546, 0.9435911131814402886, 0.000000000000000000 ) ) ;
#51926 = CARTESIAN_POINT ( 'NONE',  ( -92.35000000000012221, 90.00000071509187194, 85.31687502647973531 ) ) ;
#51927 = CARTESIAN_POINT ( 'NONE',  ( -96.15314808468747287, -208.0026889286704943, 75.09072916753380866 ) ) ;
#51928 = EDGE_CURVE ( 'NONE', #46606, #45876, #38885, .T. ) ;
#51929 = EDGE_CURVE ( 'NONE', #1611, #19251, #18469, .T. ) ;
#51930 = CARTESIAN_POINT ( 'NONE',  ( -97.64999999999996305, -209.9999999999999716, 79.83999999999998920 ) ) ;
#51931 = ORIENTED_EDGE ( 'NONE', *, *, #57044, .T. ) ;
#51932 = CARTESIAN_POINT ( 'NONE',  ( 13.83832728059186046, -142.6495187161941089, 5.500000000000000000 ) ) ;
#51933 = DIRECTION ( 'NONE',  ( 1.000000000000000000, 1.427937372958405461E-15, 7.962523111839130290E-16 ) ) ;
#51934 = PRESENTATION_STYLE_ASSIGNMENT (( #13191 ) ) ;
#51935 = EDGE_CURVE ( 'NONE', #53076, #48097, #73689, .T. ) ;
#51936 = FACE_OUTER_BOUND ( 'NONE', #27469, .T. ) ;
#51937 = EDGE_CURVE ( 'NONE', #37162, #5395, #25671, .T. ) ;
#51938 = CARTESIAN_POINT ( 'NONE',  ( 0.000000000000000000, -27.05870788708250885, 26.08949754953014022 ) ) ;
#51939 = EDGE_LOOP ( 'NONE', ( #69326, #17581, #68897, #47981 ) ) ;
#51940 = CYLINDRICAL_SURFACE ( 'NONE', #52859, 31.99999999999999289 ) ;
#51941 = CARTESIAN_POINT ( 'NONE',  ( -97.64999999996642543, 89.99999234487438571, 78.01464417100932280 ) ) ;
#51942 = ORIENTED_EDGE ( 'NONE', *, *, #37337, .T. ) ;
#51943 = CARTESIAN_POINT ( 'NONE',  ( 92.69370383062501162, -211.3315407142195852, 87.79072916753379729 ) ) ;
#51944 = LINE ( 'NONE', #69241, #46706 ) ;
#51945 = EDGE_CURVE ( 'NONE', #39761, #59464, #21976, .T. ) ;
#51946 = EDGE_LOOP ( 'NONE', ( #58223, #51919, #27155, #71702 ) ) ;
#51947 = CARTESIAN_POINT ( 'NONE',  ( 0.000000000000000000, -14.67089635893658794, -73.72996012237454977 ) ) ;
#51948 = ORIENTED_EDGE ( 'NONE', *, *, #29262, .F. ) ;
#51949 = FACE_OUTER_BOUND ( 'NONE', #16090, .T. ) ;
#51950 = EDGE_LOOP ( 'NONE', ( #51594, #24235, #17784, #67961 ) ) ;
#51951 = CARTESIAN_POINT ( 'NONE',  ( -96.15314808468752972, 91.99731107132950569, 82.07572916753382231 ) ) ;
#51952 = VECTOR ( 'NONE', #18560, 1000.000000000000000 ) ;
#51953 = VERTEX_POINT ( 'NONE', #3968 ) ;
#51954 = CARTESIAN_POINT ( 'NONE',  ( 10.00000000000000000, -66.50666863321973210, -39.78640506895676765 ) ) ;
#51955 = ORIENTED_EDGE ( 'NONE', *, *, #19758, .F. ) ;
#51956 = ORIENTED_EDGE ( 'NONE', *, *, #15038, .F. ) ;
#51957 = DIRECTION ( 'NONE',  ( -1.000000000000000000, 0.000000000000000000, 0.000000000000000000 ) ) ;
#51958 = ADVANCED_FACE ( 'NONE', ( #49793 ), #45674, .T. ) ;
#51959 = EDGE_CURVE ( 'NONE', #14970, #52132, #52075, .T. ) ;
#51960 = ORIENTED_EDGE ( 'NONE', *, *, #39318, .T. ) ;
#51961 = AXIS2_PLACEMENT_3D ( 'NONE', #45408, #56308, #63080 ) ;
#51962 = ORIENTED_EDGE ( 'NONE', *, *, #30558, .T. ) ;
#51963 = CARTESIAN_POINT ( 'NONE',  ( 10.00000000000000000, -32.34446384429989507, 26.79245525562703278 ) ) ;
#51964 = ADVANCED_FACE ( 'NONE', ( #21219 ), #61471, .T. ) ;
#51965 = EDGE_LOOP ( 'NONE', ( #69877, #63170, #3010, #26806 ) ) ;
#51966 = ORIENTED_EDGE ( 'NONE', *, *, #45678, .F. ) ;
#51967 = CARTESIAN_POINT ( 'NONE',  ( 97.30629616937498838, 91.33154071421968467, 84.29822916753380468 ) ) ;
#51968 = AXIS2_PLACEMENT_3D ( 'NONE', #60342, #25384, #8825 ) ;
#51969 = ORIENTED_EDGE ( 'NONE', *, *, #71868, .F. ) ;
#51970 = CARTESIAN_POINT ( 'NONE',  ( 93.84685191531251292, -211.9973110713294489, 80.22364583420046813 ) ) ;
#51971 = AXIS2_PLACEMENT_3D ( 'NONE', #57854, #39075, #52195 ) ;
#51972 = PRODUCT_CONTEXT ( 'NONE', #33027, 'mechanical' ) ;
#51973 = CARTESIAN_POINT ( 'NONE',  ( -92.34999999999999432, -209.9999999999999716, 76.34749999999999659 ) ) ;
#51974 = DIRECTION ( 'NONE',  ( -1.000000000000000000, -0.000000000000000000, 0.000000000000000000 ) ) ;
#51975 = CYLINDRICAL_SURFACE ( 'NONE', #6543, 31.99999999999998579 ) ;
#51976 = CARTESIAN_POINT ( 'NONE',  ( 10.00000000000000000, -40.98264845739743834, -9.188173127307738497 ) ) ;
#51977 = CARTESIAN_POINT ( 'NONE',  ( -7.499999999999969802, 73.00000000000001421, -255.0000000000000000 ) ) ;
#51978 = CARTESIAN_POINT ( 'NONE',  ( 0.000000000000000000, 26.02418014898310261, 70.52718814184268581 ) ) ;
#51979 = CARTESIAN_POINT ( 'NONE',  ( -94.99999999999997158, -212.6630814284392557, 84.08656250086713158 ) ) ;
#51980 = CARTESIAN_POINT ( 'NONE',  ( -96.15314808468752972, 91.99731107132950569, 82.71072916753381321 ) ) ;
#51981 = VERTEX_POINT ( 'NONE', #33997 ) ;
#51982 = CARTESIAN_POINT ( 'NONE',  ( 92.69370383062498320, 90.00000000000002842, 84.56281250086713897 ) ) ;
#51983 = ORIENTED_EDGE ( 'NONE', *, *, #29505, .F. ) ;
#51984 = DIRECTION ( 'NONE',  ( 0.000000000000000000, 0.000000000000000000, -1.000000000000000000 ) ) ;
#51985 = CARTESIAN_POINT ( 'NONE',  ( 97.64999999999999147, 89.99999988321010846, 84.68187499741277691 ) ) ;
#51986 = DIRECTION ( 'NONE',  ( 1.000000000000000000, -0.000000000000000000, 0.000000000000000000 ) ) ;
#51987 = CARTESIAN_POINT ( 'NONE',  ( -94.99999999999997158, -207.3369185715606307, 86.94406250086714749 ) ) ;
#51988 = CARTESIAN_POINT ( 'NONE',  ( 10.00000000000000000, 41.19522573413826194, -65.64334221924865176 ) ) ;
#51989 = LINE ( 'NONE', #41101, #66211 ) ;
#51990 = DIRECTION ( 'NONE',  ( -1.000000000000000000, 0.000000000000000000, 0.000000000000000000 ) ) ;
#51991 = DIRECTION ( 'NONE',  ( -0.000000000000000000, -0.000000000000000000, 1.000000000000000000 ) ) ;
#51992 = ORIENTED_EDGE ( 'NONE', *, *, #67721, .F. ) ;
#51993 = ORIENTED_EDGE ( 'NONE', *, *, #40511, .F. ) ;
#51994 = CARTESIAN_POINT ( 'NONE',  ( -92.35000000000005116, 91.52997821335253548, 76.40041666666667197 ) ) ;
#51995 = DIRECTION ( 'NONE',  ( 0.000000000000000000, 0.000000000000000000, -1.000000000000000000 ) ) ;
#51996 = CARTESIAN_POINT ( 'NONE',  ( -94.94576887096259554, -207.6112450486804164, 74.83591575723764322 ) ) ;
#51997 = CARTESIAN_POINT ( 'NONE',  ( -10.43921258969510824, -98.89258801967538659, 5.500000000000000000 ) ) ;
#51998 = VECTOR ( 'NONE', #57387, 1000.000000000000000 ) ;
#51999 = EDGE_CURVE ( 'NONE', #64000, #40627, #6470, .T. ) ;
#52000 = CARTESIAN_POINT ( 'NONE',  ( 50.00005079999999680, 12.24744871391589207, 2.500000000000000000 ) ) ;
#52001 = CARTESIAN_POINT ( 'NONE',  ( -97.65000000000003411, -208.4700217866474929, 78.51708333333334622 ) ) ;
#52002 = ORIENTED_EDGE ( 'NONE', *, *, #14084, .F. ) ;
#52003 = CARTESIAN_POINT ( 'NONE',  ( -96.15314808468752972, 91.99731107132950569, 78.74197916753381321 ) ) ;
#52004 = EDGE_CURVE ( 'NONE', #10456, #67765, #49208, .T. ) ;
#52005 = AXIS2_PLACEMENT_3D ( 'NONE', #54296, #60677, #49002 ) ;
#52006 = CARTESIAN_POINT ( 'NONE',  ( 11.99999999999999822, -71.87247863392384772, -39.47590169984923136 ) ) ;
#52007 = DIRECTION ( 'NONE',  ( -1.000000000000000000, 0.000000000000000000, 0.000000000000000000 ) ) ;
#52008 = EDGE_CURVE ( 'NONE', #8374, #48253, #12905, .T. ) ;
#52009 = AXIS2_PLACEMENT_3D ( 'NONE', #7842, #3713, #36407 ) ;
#52010 = DIRECTION ( 'NONE',  ( 1.000000000000000000, 1.427937372958405461E-15, 7.962523111839130290E-16 ) ) ;
#52011 = LINE ( 'NONE', #47493, #47728 ) ;
#52012 = CARTESIAN_POINT ( 'NONE',  ( -96.32500000000001705, 87.70503267997129626, 75.58020833506763836 ) ) ;
#52013 = CARTESIAN_POINT ( 'NONE',  ( -92.69370383062498320, -209.9999999999999716, 85.03906250086714635 ) ) ;
#52014 = SURFACE_SIDE_STYLE ('',( #1673 ) ) ;
#52015 = EDGE_CURVE ( 'NONE', #53859, #47697, #52777, .T. ) ;
#52016 = VECTOR ( 'NONE', #48345, 1000.000000000000000 ) ;
#52017 = CIRCLE ( 'NONE', #40065, 77.49899999999999523 ) ;
#52018 = CARTESIAN_POINT ( 'NONE',  ( 93.84685191531248449, 91.99731107132950569, 75.72572916753382799 ) ) ;
#52019 = CARTESIAN_POINT ( 'NONE',  ( -97.30629616937497417, -208.6684592857803295, 78.95364583420045790 ) ) ;
#52020 = CARTESIAN_POINT ( 'NONE',  ( 10.00000000000000000, -70.53064760720297954, -26.01480285779911839 ) ) ;
#52021 = EDGE_LOOP ( 'NONE', ( #7590, #18662, #49913, #14853 ) ) ;
#52022 = EDGE_CURVE ( 'NONE', #68267, #26992, #71263, .T. ) ;
#52023 = FACE_OUTER_BOUND ( 'NONE', #7260, .T. ) ;
#52024 = DIRECTION ( 'NONE',  ( -1.000000000000000000, 0.000000000000000000, 0.000000000000000000 ) ) ;
#52025 = CARTESIAN_POINT ( 'NONE',  ( 12.50000000000000000, 0.000000000000000000, 0.000000000000000000 ) ) ;
#52026 = AXIS2_PLACEMENT_3D ( 'NONE', #29251, #46933, #13449 ) ;
#52027 = CIRCLE ( 'NONE', #15661, 0.5000000000000004441 ) ;
#52028 = CIRCLE ( 'NONE', #37655, 4.750000000000000000 ) ;
#52029 = CARTESIAN_POINT ( 'NONE',  ( -10.00000000000000000, 0.000000000000000000, 0.000000000000000000 ) ) ;
#52030 = CARTESIAN_POINT ( 'NONE',  ( 93.84685191531251292, -211.9973110713294489, 76.41364583420048007 ) ) ;
#52031 = ORIENTED_EDGE ( 'NONE', *, *, #69019, .T. ) ;
#52032 = DIRECTION ( 'NONE',  ( -1.000000000000000000, -0.000000000000000000, -0.000000000000000000 ) ) ;
#52033 = ADVANCED_FACE ( 'NONE', ( #52023 ), #63700, .T. ) ;
#52034 = ORIENTED_EDGE ( 'NONE', *, *, #58819, .T. ) ;
#52035 = DIRECTION ( 'NONE',  ( -0.000000000000000000, -0.000000000000000000, -1.000000000000000000 ) ) ;
#52036 = EDGE_CURVE ( 'NONE', #70028, #32694, #64066, .T. ) ;
#52037 = ORIENTED_EDGE ( 'NONE', *, *, #22848, .F. ) ;
#52038 = DIRECTION ( 'NONE',  ( 2.603472992746261562E-14, 2.546204323184492723E-14, -1.000000000000000000 ) ) ;
#52039 = ADVANCED_FACE ( 'NONE', ( #571 ), #18914, .T. ) ;
#52040 = ORIENTED_EDGE ( 'NONE', *, *, #70440, .F. ) ;
#52041 = ORIENTED_EDGE ( 'NONE', *, *, #40778, .F. ) ;
#52042 = EDGE_LOOP ( 'NONE', ( #58077, #58075, #68539, #63486 ) ) ;
#52043 = CARTESIAN_POINT ( 'NONE',  ( 0.000000000000000000, -37.22597642581153821, -5.202137450156795850 ) ) ;
#52044 = EDGE_CURVE ( 'NONE', #19421, #2104, #23464, .T. ) ;
#52045 = ORIENTED_EDGE ( 'NONE', *, *, #40182, .F. ) ;
#52046 = CIRCLE ( 'NONE', #18452, 31.99999999999998579 ) ;
#52047 = ORIENTED_EDGE ( 'NONE', *, *, #66822, .T. ) ;
#52048 = CARTESIAN_POINT ( 'NONE',  ( 92.69370383062498320, 88.66845928578037217, 83.50447916753383026 ) ) ;
#52049 = EDGE_CURVE ( 'NONE', #68067, #53386, #14879, .T. ) ;
#52050 = DIRECTION ( 'NONE',  ( -0.9580045777625456616, -0.2867529058022021404, 0.000000000000000000 ) ) ;
#52051 = ORIENTED_EDGE ( 'NONE', *, *, #13235, .T. ) ;
#52052 = VECTOR ( 'NONE', #58780, 1000.000000000000000 ) ;
#52053 = EDGE_CURVE ( 'NONE', #27169, #20441, #28724, .T. ) ;
#52054 = ORIENTED_EDGE ( 'NONE', *, *, #60751, .F. ) ;
#52055 = ORIENTED_EDGE ( 'NONE', *, *, #4186, .F. ) ;
#52056 = VERTEX_POINT ( 'NONE', #53143 ) ;
#52057 = ORIENTED_EDGE ( 'NONE', *, *, #8159, .F. ) ;
#52058 = FACE_BOUND ( 'NONE', #48087, .T. ) ;
#52059 = AXIS2_PLACEMENT_3D ( 'NONE', #19031, #14877, #47607 ) ;
#52060 = DIRECTION ( 'NONE',  ( 1.224646799147353207E-16, 1.000000000000000000, 0.000000000000000000 ) ) ;
#52061 = CARTESIAN_POINT ( 'NONE',  ( 10.00000000000000000, 35.38097989696528600, -12.42422080174602605 ) ) ;
#52062 = DIRECTION ( 'NONE',  ( -1.000000000000000000, -0.000000000000000000, 0.000000000000000000 ) ) ;
#52063 = CARTESIAN_POINT ( 'NONE',  ( 10.00000000000000000, -69.42325613327415113, -34.44570377933673910 ) ) ;
#52064 = CARTESIAN_POINT ( 'NONE',  ( 1.560000000000000053, -1.732050807568877859, -1.752539433813135784E-17 ) ) ;
#52065 = LINE ( 'NONE', #608, #43199 ) ;
#52066 = CARTESIAN_POINT ( 'NONE',  ( 10.00000000000000000, 0.000000000000000000, 0.000000000000000000 ) ) ;
#52067 = VERTEX_POINT ( 'NONE', #18552 ) ;
#52068 = CARTESIAN_POINT ( 'NONE',  ( -96.32499999999996021, -207.7050326799711968, 80.44854166840097776 ) ) ;
#52069 = ORIENTED_EDGE ( 'NONE', *, *, #46257, .F. ) ;
#52070 = DIRECTION ( 'NONE',  ( 0.000000000000000000, 0.8090169943749486725, -0.5877852522924713607 ) ) ;
#52071 = ORIENTED_EDGE ( 'NONE', *, *, #4889, .F. ) ;
#52073 = CARTESIAN_POINT ( 'NONE',  ( -97.65000000000001990, 90.00000000000004263, 79.28437500173430408 ) ) ;
#52072 = CARTESIAN_POINT ( 'NONE',  ( 97.64999999999999147, 90.00000000000002842, 79.60187500173429953 ) ) ;
#52074 = CIRCLE ( 'NONE', #35285, 82.00000000000000000 ) ;
#52075 =( BOUNDED_CURVE ( )  B_SPLINE_CURVE ( 2, ( #21598, #16714, #39652, #26867, #38903, #10697, #33623, #56580, #5080, #72714, #28348 ),
 .UNSPECIFIED., .F., .F. ) 
 B_SPLINE_CURVE_WITH_KNOTS ( ( 3, 2, 2, 2, 2, 3 ),
 ( 0.1481709449575320525, 0.1481710763585296908, 0.1552268418994117993, 0.1622826074402939078, 0.1693383729811760163, 0.1693384224419976214 ),
 .UNSPECIFIED. ) 
 CURVE ( )  GEOMETRIC_REPRESENTATION_ITEM ( )  RATIONAL_B_SPLINE_CURVE ( ( 0.9999950100190690971, 0.9999975049630689394, 1.000000000000000000, 0.8660254037844387076, 1.000000000000000000, 0.8660254037844387076, 1.000000000000000000, 0.8660254037844387076, 1.000000000000000000, 0.9999990608398812153, 0.9999981216929294536 ) ) 
 REPRESENTATION_ITEM ( '' )  );
#52076 = ORIENTED_EDGE ( 'NONE', *, *, #32239, .T. ) ;
#52077 = CARTESIAN_POINT ( 'NONE',  ( 97.30629616937498838, 90.00000000000002842, 79.95906250086714806 ) ) ;
#52078 = CIRCLE ( 'NONE', #553, 82.00000000000000000 ) ;
#52079 = LINE ( 'NONE', #5868, #10965 ) ;
#52080 = CARTESIAN_POINT ( 'NONE',  ( 11.99999999999999822, 41.76106447765580043, -62.50884508063379741 ) ) ;
#52081 = LINE ( 'NONE', #69374, #57834 ) ;
#52082 = CARTESIAN_POINT ( 'NONE',  ( 5.999999999999999112, 50.23322058963442771, -64.81221759200288091 ) ) ;
#52083 = ORIENTED_EDGE ( 'NONE', *, *, #69605, .T. ) ;
#52084 = DIRECTION ( 'NONE',  ( 0.000000000000000000, -0.7071067811865389130, -0.7071067811865563435 ) ) ;
#52086 = LINE ( 'NONE', #11850, #70910 ) ;
#52085 = CIRCLE ( 'NONE', #10053, 31.99999999999999289 ) ;
#52087 = VECTOR ( 'NONE', #4144, 1000.000000000000000 ) ;
#52088 = LINE ( 'NONE', #51727, #50363 ) ;
#52089 = ORIENTED_EDGE ( 'NONE', *, *, #22345, .T. ) ;
#52090 = ORIENTED_EDGE ( 'NONE', *, *, #36952, .F. ) ;
#52091 = DIRECTION ( 'NONE',  ( -0.6575728627325955200, 0.7533909544171997208, 0.000000000000000000 ) ) ;
#52092 = CARTESIAN_POINT ( 'NONE',  ( -2.618768541235303005, -4.261555969668739507, -0.5078976954042990766 ) ) ;
#52093 = DIRECTION ( 'NONE',  ( 1.000000000000000000, 0.000000000000000000, -0.000000000000000000 ) ) ;
#52094 = CARTESIAN_POINT ( 'NONE',  ( -92.69370383062498320, -209.9999999999999716, 77.41906250086715602 ) ) ;
#52095 =( BOUNDED_CURVE ( )  B_SPLINE_CURVE ( 2, ( #73553, #50626, #29442, #67936, #17804, #16425, #935 ),
 .UNSPECIFIED., .F., .F. ) 
 B_SPLINE_CURVE_WITH_KNOTS ( ( 3, 2, 2, 3 ),
 ( 0.6773535682752289677, 0.6844092574655884498, 0.6914650230064715020, 0.6985206468843491168 ),
 .UNSPECIFIED. ) 
 CURVE ( )  GEOMETRIC_REPRESENTATION_ITEM ( )  RATIONAL_B_SPLINE_CURVE ( ( 0.9999971005499468379, 0.8660268535251529620, 1.000000000000000000, 0.8660254037844387076, 1.000000000000000000, 0.8660280936759657822, 0.9999946203249591159 ) ) 
 REPRESENTATION_ITEM ( '' )  );
#52096 = ORIENTED_EDGE ( 'NONE', *, *, #30537, .T. ) ;
#52097 = AXIS2_PLACEMENT_3D ( 'NONE', #39418, #51801, #67611 ) ;
#52098 = ADVANCED_FACE ( 'NONE', ( #70404 ), #6548, .T. ) ;
#52099 = CARTESIAN_POINT ( 'NONE',  ( 0.000000000000000000, 0.000000000000000000, 0.000000000000000000 ) ) ;
#52100 = CARTESIAN_POINT ( 'NONE',  ( 23.11608002360578240, -124.4885236261218182, 2.500000000000000000 ) ) ;
#52101 = EDGE_CURVE ( 'NONE', #57864, #61855, #11790, .T. ) ;
#52102 = CYLINDRICAL_SURFACE ( 'NONE', #18942, 16.00000000000000000 ) ;
#52103 = CARTESIAN_POINT ( 'NONE',  ( 96.15314808468748708, 88.00268892867053694, 75.24947916753380639 ) ) ;
#52104 = DIRECTION ( 'NONE',  ( -1.000000000000000000, 0.000000000000000000, 0.000000000000000000 ) ) ;
#52105 = LINE ( 'NONE', #10780, #43287 ) ;
#52106 = FACE_OUTER_BOUND ( 'NONE', #59450, .T. ) ;
#52107 = DIRECTION ( 'NONE',  ( 1.000000000000000000, 0.000000000000000000, 0.000000000000000000 ) ) ;
#52108 = EDGE_CURVE ( 'NONE', #65473, #72308, #72509, .T. ) ;
#52109 = CARTESIAN_POINT ( 'NONE',  ( 15.00000000000000000, 24.81905959214260804, -9.408202855044828894 ) ) ;
#52110 = DIRECTION ( 'NONE',  ( -1.000000000000000000, 0.000000000000000000, 0.000000000000000000 ) ) ;
#52111 = VECTOR ( 'NONE', #62666, 1000.000000000000000 ) ;
#52112 = EDGE_CURVE ( 'NONE', #4678, #23323, #35477, .T. ) ;
#52113 = CARTESIAN_POINT ( 'NONE',  ( 96.15314808468748708, 91.99731107132950569, 88.95489583420049939 ) ) ;
#52114 = DIRECTION ( 'NONE',  ( -1.000000000000000000, 0.000000000000000000, -0.000000000000000000 ) ) ;
#52115 = DIRECTION ( 'NONE',  ( 0.000000000000000000, 0.000000000000000000, -1.000000000000000000 ) ) ;
#52116 = ORIENTED_EDGE ( 'NONE', *, *, #17007, .T. ) ;
#52117 = DIRECTION ( 'NONE',  ( -1.000000000000000000, -0.000000000000000000, -0.000000000000000000 ) ) ;
#52118 = CARTESIAN_POINT ( 'NONE',  ( -93.84685191531252713, 88.00268892867056536, 79.69447916753379957 ) ) ;
#52119 = AXIS2_PLACEMENT_3D ( 'NONE', #33087, #57526, #39495 ) ;
#52120 = CARTESIAN_POINT ( 'NONE',  ( 93.84685191531249870, -208.0026889286704943, 86.99697916753380866 ) ) ;
#52121 = VERTEX_POINT ( 'NONE', #1321 ) ;
#52122 = CIRCLE ( 'NONE', #34152, 37.49900000000000233 ) ;
#52123 = CARTESIAN_POINT ( 'NONE',  ( -97.65000000000001990, 90.00000000000004263, 90.00000000000000000 ) ) ;
#52125 = CARTESIAN_POINT ( 'NONE',  ( -10.00000000000000000, 0.000000000000000000, 0.000000000000000000 ) ) ;
#52124 = AXIS2_PLACEMENT_3D ( 'NONE', #56101, #4617, #51190 ) ;
#52126 = EDGE_LOOP ( 'NONE', ( #21079, #40716, #58547, #50024 ) ) ;
#52127 = DIRECTION ( 'NONE',  ( -1.000000000000000000, -0.000000000000000000, 0.000000000000000000 ) ) ;
#52128 = EDGE_CURVE ( 'NONE', #74057, #15980, #23741, .T. ) ;
#52130 = ADVANCED_FACE ( 'NONE', ( #13648 ), #36957, .F. ) ;
#52129 = VECTOR ( 'NONE', #5454, 1000.000000000000000 ) ;
#52131 = CARTESIAN_POINT ( 'NONE',  ( 10.00000000000000000, 0.000000000000000000, 0.000000000000000000 ) ) ;
#52132 = VERTEX_POINT ( 'NONE', #8391 ) ;
#52133 = VERTEX_POINT ( 'NONE', #54979 ) ;
#52134 = CARTESIAN_POINT ( 'NONE',  ( 92.69370383062501162, -211.3315407142195852, 82.23447916753383424 ) ) ;
#52135 = DIRECTION ( 'NONE',  ( -1.000000000000000000, 0.000000000000000000, 0.000000000000000000 ) ) ;
#52136 = EDGE_CURVE ( 'NONE', #66421, #59589, #43362, .T. ) ;
#52137 = CARTESIAN_POINT ( 'NONE',  ( -8.000000000000019540, 1.628656900575238863E-13, 15.79999999999999183 ) ) ;
#52138 = DIRECTION ( 'NONE',  ( -1.000000000000000000, 0.000000000000000000, 0.000000000000000000 ) ) ;
#52139 = DIRECTION ( 'NONE',  ( -1.000000000000000000, -0.000000000000000000, -0.000000000000000000 ) ) ;
#52140 = CARTESIAN_POINT ( 'NONE',  ( 10.00000000000000000, 0.000000000000000000, 0.000000000000000000 ) ) ;
#52141 = CARTESIAN_POINT ( 'NONE',  ( 93.67500000000001137, -207.7050326799711968, 84.17916666666666003 ) ) ;
#52142 = ORIENTED_EDGE ( 'NONE', *, *, #36078, .T. ) ;
#52143 = VERTEX_POINT ( 'NONE', #66284 ) ;
#52144 = VERTEX_POINT ( 'NONE', #42243 ) ;
#52145 = EDGE_LOOP ( 'NONE', ( #29018, #778, #34131, #47194 ) ) ;
#52146 = DIRECTION ( 'NONE',  ( 0.000000000000000000, -0.5224985647159380298, -0.8526401643540988395 ) ) ;
#52147 = FILL_AREA_STYLE ('',( #17942 ) ) ;
#52148 = CARTESIAN_POINT ( 'NONE',  ( -95.00000000000002842, 92.66308142843932671, 86.46781250086716852 ) ) ;
#52149 = CARTESIAN_POINT ( 'NONE',  ( 11.99999999999999822, -22.90783923731685334, 78.73519480814947258 ) ) ;
#52150 = CARTESIAN_POINT ( 'NONE',  ( 0.000000000000000000, -71.91182617369166508, -28.89263327155821770 ) ) ;
#52151 = CARTESIAN_POINT ( 'NONE',  ( 93.67500000000001137, -207.7050326799711968, 75.36854166840096525 ) ) ;
#52152 = CARTESIAN_POINT ( 'NONE',  ( 94.99999999999998579, 86.94004357329500010, 78.72875000000001933 ) ) ;
#52153 = ORIENTED_EDGE ( 'NONE', *, *, #30644, .T. ) ;
#52154 = CARTESIAN_POINT ( 'NONE',  ( -94.99999999999997158, -206.9400435732949575, 89.28562500173430294 ) ) ;
#52155 = ORIENTED_EDGE ( 'NONE', *, *, #58930, .T. ) ;
#52156 = CARTESIAN_POINT ( 'NONE',  ( -97.64999999953492704, -210.0000309987302956, 83.09538598079114990 ) ) ;
#52157 = CIRCLE ( 'NONE', #45767, 16.00000000000000000 ) ;
#52158 = VERTEX_POINT ( 'NONE', #8760 ) ;
#52159 = CARTESIAN_POINT ( 'NONE',  ( 96.32499999999998863, 87.70503267997126784, 84.57604166840096127 ) ) ;
#52160 = CARTESIAN_POINT ( 'NONE',  ( -95.00000000000002842, 92.66308142843932671, 81.38781250086715602 ) ) ;
#52161 = CARTESIAN_POINT ( 'NONE',  ( 93.84685191531248449, 88.00268892867053694, 75.14364583420046984 ) ) ;
#52162 = VERTEX_POINT ( 'NONE', #71895 ) ;
#52163 = LINE ( 'NONE', #34885, #9372 ) ;
#52164 = DIRECTION ( 'NONE',  ( -1.000000000000000000, 0.000000000000000000, 0.000000000000000000 ) ) ;
#52165 = FACE_OUTER_BOUND ( 'NONE', #51415, .T. ) ;
#52166 = LINE ( 'NONE', #53283, #62505 ) ;
#52167 = ORIENTED_EDGE ( 'NONE', *, *, #17071, .F. ) ;
#52168 = CARTESIAN_POINT ( 'NONE',  ( 4.999999999999999112, -40.68715046381937128, 10.41901085202062660 ) ) ;
#52169 = CARTESIAN_POINT ( 'NONE',  ( -96.15314808468745866, -211.9973110713294489, 77.04864583420047097 ) ) ;
#52170 = AXIS2_PLACEMENT_3D ( 'NONE', #49554, #20235, #19499 ) ;
#52171 = ORIENTED_EDGE ( 'NONE', *, *, #72449, .T. ) ;
#52172 = ORIENTED_EDGE ( 'NONE', *, *, #21475, .F. ) ;
#52173 = DIRECTION ( 'NONE',  ( 0.000000000000000000, 0.000000000000000000, 1.000000000000000000 ) ) ;
#52174 = ORIENTED_EDGE ( 'NONE', *, *, #72872, .T. ) ;
#52175 = CARTESIAN_POINT ( 'NONE',  ( 10.00000000000000000, 30.80686688397010542, 21.53537804866092387 ) ) ;
#52176 = DIRECTION ( 'NONE',  ( -1.000000000000000000, 0.000000000000000000, 0.000000000000000000 ) ) ;
#52177 = EDGE_LOOP ( 'NONE', ( #22371, #34774, #37827, #70201 ) ) ;
#52178 = CARTESIAN_POINT ( 'NONE',  ( -97.30629616937495996, -209.9999999999999716, 89.16656250086715829 ) ) ;
#52179 = ORIENTED_EDGE ( 'NONE', *, *, #63996, .T. ) ;
#52180 = CIRCLE ( 'NONE', #67748, 31.99999999999998934 ) ;
#52181 = CARTESIAN_POINT ( 'NONE',  ( 10.00000000000000000, -41.76937507738831812, 62.50329211542423025 ) ) ;
#52182 = CARTESIAN_POINT ( 'NONE',  ( -3.000000000000000000, -22.32062822937469804, -14.36278369418829826 ) ) ;
#52183 = VECTOR ( 'NONE', #36161, 1000.000000000000000 ) ;
#52184 = VERTEX_POINT ( 'NONE', #7647 ) ;
#52185 = ORIENTED_EDGE ( 'NONE', *, *, #27911, .F. ) ;
#52186 = EDGE_CURVE ( 'NONE', #20082, #48441, #7695, .T. ) ;
#52187 = CARTESIAN_POINT ( 'NONE',  ( -97.65000000000001990, 89.99996406046686559, 83.72937624475873974 ) ) ;
#52188 = VECTOR ( 'NONE', #33152, 1000.000000000000000 ) ;
#52189 = ADVANCED_FACE ( 'NONE', ( #53880 ), #70788, .T. ) ;
#52190 =( LENGTH_UNIT ( ) NAMED_UNIT ( * ) SI_UNIT ( .MILLI., .METRE. ) );
#52191 = CARTESIAN_POINT ( 'NONE',  ( 92.69370383062498320, 90.00000000000002842, 85.83281250086714920 ) ) ;
#52192 = DIRECTION ( 'NONE',  ( -1.000000000000000000, -0.000000000000000000, 0.000000000000000000 ) ) ;
#52193 = CARTESIAN_POINT ( 'NONE',  ( 0.000000000000000000, 77.16300072079700101, -27.74655509720590985 ) ) ;
#52194 = CARTESIAN_POINT ( 'NONE',  ( 95.00000000000000000, -206.9400435732949575, 86.66624999999999091 ) ) ;
#52195 = DIRECTION ( 'NONE',  ( 0.000000000000000000, 0.000000000000000000, 1.000000000000000000 ) ) ;
#52197 = EDGE_CURVE ( 'NONE', #33517, #49560, #65345, .T. ) ;
#52196 = FACE_OUTER_BOUND ( 'NONE', #21098, .T. ) ;
#52198 = CARTESIAN_POINT ( 'NONE',  ( 97.64999999999999147, -210.0000000334413244, 87.85687500050293863 ) ) ;
#52199 = DIRECTION ( 'NONE',  ( -1.000000000000000000, 0.000000000000000000, -0.000000000000000000 ) ) ;
#52200 = AXIS2_PLACEMENT_3D ( 'NONE', #15916, #38848, #33194 ) ;
#52201 = EDGE_CURVE ( 'NONE', #21432, #26057, #52180, .T. ) ;
#52202 = DIRECTION ( 'NONE',  ( -1.000000000000000000, 0.000000000000000000, -0.000000000000000000 ) ) ;
#52203 = CIRCLE ( 'NONE', #56999, 31.99999999999998934 ) ;
#52204 = CARTESIAN_POINT ( 'NONE',  ( 10.00000000000000000, 0.000000000000000000, 0.000000000000000000 ) ) ;
#52205 = ADVANCED_FACE ( 'NONE', ( #25315 ), #47866, .F. ) ;
#52206 = PLANE ( 'NONE',  #8937 ) ;
#52207 = CYLINDRICAL_SURFACE ( 'NONE', #53962, 12.49999999999999645 ) ;
#52208 = ADVANCED_FACE ( 'NONE', ( #20024 ), #3507, .F. ) ;
#52209 = DIRECTION ( 'NONE',  ( -0.000000000000000000, -0.000000000000000000, -1.000000000000000000 ) ) ;
#52210 = EDGE_CURVE ( 'NONE', #38305, #26020, #3144, .T. ) ;
#52211 = ORIENTED_EDGE ( 'NONE', *, *, #59179, .F. ) ;
#52212 = CARTESIAN_POINT ( 'NONE',  ( -3.000000000000000000, 26.50000000000000000, -1.500000000000001332 ) ) ;
#52213 = DIRECTION ( 'NONE',  ( 0.000000000000000000, 0.000000000000000000, 1.000000000000000000 ) ) ;
#52214 = DIRECTION ( 'NONE',  ( 0.000000000000000000, 0.000000000000000000, 1.000000000000000000 ) ) ;
#52215 = CYLINDRICAL_SURFACE ( 'NONE', #60622, 12.50000000000000000 ) ;
#52216 = CARTESIAN_POINT ( 'NONE',  ( -92.35000000000003695, 90.00000000000004263, 90.00000000000000000 ) ) ;
#52217 = EDGE_CURVE ( 'NONE', #44776, #24481, #65047, .T. ) ;
#52218 = ADVANCED_FACE ( 'NONE', ( #65174 ), #14012, .F. ) ;
#52219 = AXIS2_PLACEMENT_3D ( 'NONE', #50197, #62251, #56981 ) ;
#52220 = CARTESIAN_POINT ( 'NONE',  ( 92.69370383062501162, -208.6684592857803011, 84.03364583420049883 ) ) ;
#52221 = EDGE_LOOP ( 'NONE', ( #55217, #8228, #70382, #52544 ) ) ;
#52222 = EDGE_LOOP ( 'NONE', ( #4744, #64257, #30679, #5000 ) ) ;
#52223 = CARTESIAN_POINT ( 'NONE',  ( 10.00000000000000000, 76.41127070299292257, -12.93880638057232346 ) ) ;
#52224 = ORIENTED_EDGE ( 'NONE', *, *, #72615, .F. ) ;
#52225 = DIRECTION ( 'NONE',  ( -1.000000000000000000, 0.000000000000000000, -0.000000000000000000 ) ) ;
#52226 = CARTESIAN_POINT ( 'NONE',  ( 97.30629616937498838, -209.9999999999999716, 75.99031250086714806 ) ) ;
#52227 = VECTOR ( 'NONE', #14670, 1000.000000000000114 ) ;
#52228 = VERTEX_POINT ( 'NONE', #25676 ) ;
#52229 = VECTOR ( 'NONE', #27841, 1000.000000000000000 ) ;
#52230 = CARTESIAN_POINT ( 'NONE',  ( 97.30629616937498838, -208.6684592857803011, 79.37697916753381833 ) ) ;
#52231 = ORIENTED_EDGE ( 'NONE', *, *, #60444, .F. ) ;
#52232 = DIRECTION ( 'NONE',  ( -1.000000000000000000, 0.000000000000000000, 0.000000000000000000 ) ) ;
#52233 = ORIENTED_EDGE ( 'NONE', *, *, #43294, .T. ) ;
#52234 = AXIS2_PLACEMENT_3D ( 'NONE', #61566, #44272, #50266 ) ;
#52235 = ORIENTED_EDGE ( 'NONE', *, *, #7951, .F. ) ;
#52236 = CARTESIAN_POINT ( 'NONE',  ( 0.000000000000000000, -76.41127070299280888, 12.93880638057289012 ) ) ;
#52237 =( NAMED_UNIT ( * ) SI_UNIT ( $, .STERADIAN. ) SOLID_ANGLE_UNIT ( ) );
#52238 = CARTESIAN_POINT ( 'NONE',  ( 0.000000000000000000, 73.44644590900094272, -24.73286445877628026 ) ) ;
#52239 = VECTOR ( 'NONE', #2585, 1000.000000000000000 ) ;
#52240 = EDGE_LOOP ( 'NONE', ( #35273, #47162, #15345, #25709 ) ) ;
#52241 = CARTESIAN_POINT ( 'NONE',  ( 0.000000000000000000, 31.47745569255237896, -68.26794271651228030 ) ) ;
#52242 = CARTESIAN_POINT ( 'NONE',  ( 93.67500000000001137, -212.2949673200287179, 87.01020833506763097 ) ) ;
#52243 = ORIENTED_EDGE ( 'NONE', *, *, #48959, .F. ) ;
#52244 = DIRECTION ( 'NONE',  ( -1.000000000000000000, 0.000000000000000000, 0.000000000000000000 ) ) ;
#52245 = APPLICATION_CONTEXT ( 'automotive_design' ) ;
#52246 = VERTEX_POINT ( 'NONE', #8016 ) ;
#52247 = CARTESIAN_POINT ( 'NONE',  ( 10.00000000000000000, -51.03279382321048985, -55.19960302592120627 ) ) ;
#52248 = ORIENTED_EDGE ( 'NONE', *, *, #47344, .T. ) ;
#52249 = CONICAL_SURFACE ( 'NONE', #36635, 2.541999999999999815, 1.047197551196591858 ) ;
#52250 = CARTESIAN_POINT ( 'NONE',  ( 92.34999999999999432, 88.47002178664753558, 85.68729166840097378 ) ) ;
#52251 = ORIENTED_EDGE ( 'NONE', *, *, #23845, .F. ) ;
#52252 =( LENGTH_UNIT ( ) NAMED_UNIT ( * ) SI_UNIT ( .MILLI., .METRE. ) );
#52253 = ORIENTED_EDGE ( 'NONE', *, *, #40385, .F. ) ;
#52254 = CARTESIAN_POINT ( 'NONE',  ( 11.99999999999999822, 73.95703589263975175, 23.16143007188452785 ) ) ;
#52255 = CARTESIAN_POINT ( 'NONE',  ( 10.00000000000000000, 0.000000000000000000, 0.000000000000000000 ) ) ;
#52256 = ORIENTED_EDGE ( 'NONE', *, *, #65548, .F. ) ;
#52257 = VERTEX_POINT ( 'NONE', #2788 ) ;
#52258 = AXIS2_PLACEMENT_3D ( 'NONE', #26111, #49781, #66720 ) ;
#52259 = ORIENTED_EDGE ( 'NONE', *, *, #14935, .F. ) ;
#52260 = DIRECTION ( 'NONE',  ( 1.000000000000000000, 0.000000000000000000, 0.000000000000000000 ) ) ;
#52261 = CYLINDRICAL_SURFACE ( 'NONE', #32494, 31.99999999999998579 ) ;
#52262 = EDGE_CURVE ( 'NONE', #56011, #1858, #42979, .T. ) ;
#52263 = CARTESIAN_POINT ( 'NONE',  ( -93.67500000000003979, 87.70503267997129626, 87.03666666666666174 ) ) ;
#52264 = VERTEX_POINT ( 'NONE', #22260 ) ;
#52265 = DIRECTION ( 'NONE',  ( -0.02332147558787930897, -0.9997280174009348652, 0.000000000000000000 ) ) ;
#52266 = EDGE_CURVE ( 'NONE', #48891, #10101, #33523, .T. ) ;
#52267 = VECTOR ( 'NONE', #71329, 999.9999999999998863 ) ;
#52268 = VERTEX_POINT ( 'NONE', #73374 ) ;
#52269 = CYLINDRICAL_SURFACE ( 'NONE', #11911, 12.74999999999999822 ) ;
#52270 = CARTESIAN_POINT ( 'NONE',  ( -93.84685191531247028, -211.9973110713294489, 85.40947916753380298 ) ) ;
#52271 = ORIENTED_EDGE ( 'NONE', *, *, #33362, .F. ) ;
#52272 = CARTESIAN_POINT ( 'NONE',  ( -97.64999999999997726, -209.9999856621396930, 79.28437450583719226 ) ) ;
#52273 = DIRECTION ( 'NONE',  ( 0.000000000000000000, 0.4067366430758009854, 0.9135454576426004225 ) ) ;
#52274 = DIRECTION ( 'NONE',  ( 0.000000000000000000, 0.000000000000000000, 1.000000000000000000 ) ) ;
#52275 = CARTESIAN_POINT ( 'NONE',  ( -96.15314808468745866, -211.9973110713294489, 77.68364583420047609 ) ) ;
#52276 = ADVANCED_FACE ( 'NONE', ( #50068 ), #22632, .F. ) ;
#52277 = DIRECTION ( 'NONE',  ( -1.000000000000000000, -0.000000000000000000, -0.000000000000000000 ) ) ;
#52278 = CARTESIAN_POINT ( 'NONE',  ( 10.00000000000000000, 0.000000000000000000, 0.000000000000000000 ) ) ;
#52279 = CIRCLE ( 'NONE', #43870, 37.49900000000000233 ) ;
#52280 = EDGE_CURVE ( 'NONE', #7707, #34514, #21882, .T. ) ;
#52281 = DIRECTION ( 'NONE',  ( 0.000000000000000000, 0.8090169943749486725, -0.5877852522924713607 ) ) ;
#52282 = CARTESIAN_POINT ( 'NONE',  ( -1.250000000000000000, -12.36245420541525597, -1.199999999999999956 ) ) ;
#52283 = CARTESIAN_POINT ( 'NONE',  ( 12.00000000000000000, -20.55727247249748757, -16.78983467731284662 ) ) ;
#52284 = LINE ( 'NONE', #70294, #9144 ) ;
#52285 = CARTESIAN_POINT ( 'NONE',  ( -95.00000000000002842, 92.66308142843932671, 79.32406250086714294 ) ) ;
#52286 = CARTESIAN_POINT ( 'NONE',  ( -12.49999999999999645, 1.530808498934191127E-15, -125.0000000000000000 ) ) ;
#52287 = CARTESIAN_POINT ( 'NONE',  ( -0.1915406271734583221, -121.4877204670710427, 2.500000000000000000 ) ) ;
#52288 = EDGE_CURVE ( 'NONE', #13480, #779, #26949, .T. ) ;
#52289 = ORIENTED_EDGE ( 'NONE', *, *, #9082, .F. ) ;
#52290 = VECTOR ( 'NONE', #53561, 1000.000000000000000 ) ;
#52291 = DIRECTION ( 'NONE',  ( 0.000000000000000000, 0.000000000000000000, 1.000000000000000000 ) ) ;
#52293 = CARTESIAN_POINT ( 'NONE',  ( 0.000000000000000000, 67.80270845531887858, 46.11716303203210288 ) ) ;
#52292 = AXIS2_PLACEMENT_3D ( 'NONE', #23495, #18585, #64099 ) ;
#52294 = FACE_OUTER_BOUND ( 'NONE', #44771, .T. ) ;
#52295 = DIRECTION ( 'NONE',  ( 0.000000000000000000, 0.000000000000000000, -1.000000000000000000 ) ) ;
#52296 = CARTESIAN_POINT ( 'NONE',  ( 0.000000000000000000, 76.41127070299273782, 12.93880638057342836 ) ) ;
#52297 = FACE_OUTER_BOUND ( 'NONE', #72420, .T. ) ;
#52298 = CARTESIAN_POINT ( 'NONE',  ( -93.84685191531247028, -211.9973110713294489, 76.67822916753381435 ) ) ;
#52299 = ADVANCED_FACE ( 'NONE', ( #15500, #60992 ), #10981, .F. ) ;
#52300 = DIRECTION ( 'NONE',  ( -1.000000000000000000, 0.000000000000000000, -0.000000000000000000 ) ) ;
#52301 = EDGE_CURVE ( 'NONE', #40680, #69529, #73741, .T. ) ;
#52302 = VECTOR ( 'NONE', #38409, 1000.000000000000000 ) ;
#52303 =( BOUNDED_CURVE ( )  B_SPLINE_CURVE ( 2, ( #54299, #48650, #70827, #13685, #38104, #3553, #32083, #14800, #8436 ),
 .UNSPECIFIED., .F., .F. ) 
 B_SPLINE_CURVE_WITH_KNOTS ( ( 3, 2, 2, 2, 3 ),
 ( 0.7620226289464456793, 0.7620226784152968058, 0.7690784439561787478, 0.7761342094970608008, 0.7831899741065913023 ),
 .UNSPECIFIED. ) 
 CURVE ( )  GEOMETRIC_REPRESENTATION_ITEM ( )  RATIONAL_B_SPLINE_CURVE ( ( 0.9999981213880071440, 0.9999990606874179511, 1.000000000000000000, 0.8660254037844387076, 1.000000000000000000, 0.8660254037844387076, 1.000000000000000000, 0.8660254037844387076, 1.000000000000000000 ) ) 
 REPRESENTATION_ITEM ( '' )  );
#52304 = ORIENTED_EDGE ( 'NONE', *, *, #53986, .T. ) ;
#52305 = DIRECTION ( 'NONE',  ( 0.000000000000000000, -0.9723699203976789995, 0.2334453638558956767 ) ) ;
#52306 = VECTOR ( 'NONE', #2483, 1000.000000000000114 ) ;
#52307 = DIRECTION ( 'NONE',  ( 0.000000000000000000, 0.000000000000000000, 1.000000000000000000 ) ) ;
#52308 = DIRECTION ( 'NONE',  ( 0.000000000000000000, 0.000000000000000000, -1.000000000000000000 ) ) ;
#52309 = DIRECTION ( 'NONE',  ( 0.000000000000000000, 0.000000000000000000, 1.000000000000000000 ) ) ;
#52310 = CARTESIAN_POINT ( 'NONE',  ( 3.000000000000000000, -2.935248768560059673, 2.602085213965210642E-15 ) ) ;
#52311 = EDGE_LOOP ( 'NONE', ( #15752, #18133, #327, #6565 ) ) ;
#52312 = FACE_OUTER_BOUND ( 'NONE', #4189, .T. ) ;
#52313 = DIRECTION ( 'NONE',  ( -1.000000000000000000, 0.000000000000000000, 0.000000000000000000 ) ) ;
#52314 = VERTEX_POINT ( 'NONE', #9489 ) ;
#52315 = CARTESIAN_POINT ( 'NONE',  ( 96.15314808468750130, -211.9973110713294489, 84.13947916753380696 ) ) ;
#52316 = DIRECTION ( 'NONE',  ( -1.000000000000000000, 0.000000000000000000, 0.000000000000000000 ) ) ;
#52317 = ORIENTED_EDGE ( 'NONE', *, *, #28168, .T. ) ;
#52318 = CARTESIAN_POINT ( 'NONE',  ( -11.59517495878806947, -96.12423995607481686, 5.500000000000000000 ) ) ;
#52319 = ORIENTED_EDGE ( 'NONE', *, *, #69679, .F. ) ;
#52320 = DIRECTION ( 'NONE',  ( 1.000000000000000000, 1.427937372958405461E-15, 7.962523111839130290E-16 ) ) ;
#52321 = EDGE_LOOP ( 'NONE', ( #69883, #39217, #53233, #72428 ) ) ;
#52322 = CARTESIAN_POINT ( 'NONE',  ( -96.15314808468751551, 88.00268892867056536, 82.28739583420048120 ) ) ;
#52323 = ORIENTED_EDGE ( 'NONE', *, *, #45687, .F. ) ;
#52324 = ORIENTED_EDGE ( 'NONE', *, *, #34734, .F. ) ;
#52325 = ORIENTED_EDGE ( 'NONE', *, *, #15118, .F. ) ;
#52326 = FACE_OUTER_BOUND ( 'NONE', #72859, .T. ) ;
#52327 = EDGE_CURVE ( 'NONE', #68050, #34509, #26146, .T. ) ;
#52328 = ORIENTED_EDGE ( 'NONE', *, *, #51335, .F. ) ;
#52329 = CARTESIAN_POINT ( 'NONE',  ( -12.49999999999999645, 0.000000000000000000, -44.99999999999998579 ) ) ;
#52330 = EDGE_LOOP ( 'NONE', ( #51893, #72250, #59838, #18034 ) ) ;
#52331 = DIRECTION ( 'NONE',  ( 0.000000000000000000, -0.000000000000000000, 1.000000000000000000 ) ) ;
#52332 = AXIS2_PLACEMENT_3D ( 'NONE', #20369, #32008, #54948 ) ;
#52333 = VERTEX_POINT ( 'NONE', #67753 ) ;
#52334 = ORIENTED_EDGE ( 'NONE', *, *, #30363, .F. ) ;
#52335 = ORIENTED_EDGE ( 'NONE', *, *, #49150, .T. ) ;
#52336 = VECTOR ( 'NONE', #21927, 1000.000000000000000 ) ;
#52337 = CARTESIAN_POINT ( 'NONE',  ( 92.69370383062501162, -211.3315407142195852, 82.71072916753379900 ) ) ;
#52338 = SHAPE_DEFINITION_REPRESENTATION ( #54771, #51769 ) ;
#52339 = DIRECTION ( 'NONE',  ( -1.000000000000000000, 0.000000000000000000, 0.000000000000000000 ) ) ;
#52340 = CARTESIAN_POINT ( 'NONE',  ( 0.000000000000000000, -2.543863470247813119, -81.96053171279903893 ) ) ;
#52341 = AXIS2_PLACEMENT_3D ( 'NONE', #9307, #36125, #41765 ) ;
#52342 = DIRECTION ( 'NONE',  ( 0.000000000000000000, 0.3826834323650905589, -0.9238795325112864054 ) ) ;
#52343 = DIRECTION ( 'NONE',  ( 0.000000000000000000, 0.000000000000000000, 1.000000000000000000 ) ) ;
#52344 = EDGE_CURVE ( 'NONE', #69008, #8792, #49699, .T. ) ;
#52345 = AXIS2_PLACEMENT_3D ( 'NONE', #61270, #3400, #9015 ) ;
#52346 = DIRECTION ( 'NONE',  ( 0.000000000000000000, -0.9876883405951394357, 0.1564344650402205716 ) ) ;
#52347 = CARTESIAN_POINT ( 'NONE',  ( 95.00000000000000000, -206.9400435732949575, 76.50624999999999432 ) ) ;
#52348 = CARTESIAN_POINT ( 'NONE',  ( -94.99999999999997158, -207.3369185715606307, 85.67406250086715147 ) ) ;
#52349 = EDGE_CURVE ( 'NONE', #30795, #1255, #9862, .T. ) ;
#52350 = CARTESIAN_POINT ( 'NONE',  ( -96.15314808468751551, 88.00268892867056536, 81.01739583420049939 ) ) ;
#52351 = ORIENTED_EDGE ( 'NONE', *, *, #35542, .T. ) ;
#52352 = CIRCLE ( 'NONE', #31898, 31.99999999999998579 ) ;
#52353 = CARTESIAN_POINT ( 'NONE',  ( 92.69370383062498320, 88.66845928578037217, 83.34572916753380412 ) ) ;
#52354 = AXIS2_PLACEMENT_3D ( 'NONE', #6433, #58660, #7163 ) ;
#52355 = ORIENTED_EDGE ( 'NONE', *, *, #30457, .F. ) ;
#52356 = CARTESIAN_POINT ( 'NONE',  ( -92.35000000000005116, 88.47002178664754979, 78.91395833506763324 ) ) ;
#52357 = CARTESIAN_POINT ( 'NONE',  ( 12.00000000000000355, 0.000000000000000000, 0.000000000000000000 ) ) ;
#52358 = LINE ( 'NONE', #17047, #3157 ) ;
#52359 = CARTESIAN_POINT ( 'NONE',  ( 93.67500000000001137, -207.7050326799711968, 85.44916666666665606 ) ) ;
#52360 = CARTESIAN_POINT ( 'NONE',  ( -92.69370383062498320, -209.9999999999999716, 85.51531250086713953 ) ) ;
#52361 = CARTESIAN_POINT ( 'NONE',  ( -10.00000000000000000, 0.000000000000000000, 0.000000000000000000 ) ) ;
#52362 = EDGE_CURVE ( 'NONE', #1695, #53734, #29304, .T. ) ;
#52363 = DIRECTION ( 'NONE',  ( 0.000000000000000000, 0.000000000000000000, 1.000000000000000000 ) ) ;
#52364 = DIRECTION ( 'NONE',  ( -1.000000000000000000, 0.000000000000000000, 0.000000000000000000 ) ) ;
#52365 = DIRECTION ( 'NONE',  ( -1.000000000000000000, 0.000000000000000000, 0.000000000000000000 ) ) ;
#52366 = ORIENTED_EDGE ( 'NONE', *, *, #52982, .F. ) ;
#52367 = VECTOR ( 'NONE', #49257, 1000.000000000000114 ) ;
#52368 = ORIENTED_EDGE ( 'NONE', *, *, #32664, .F. ) ;
#52369 = CARTESIAN_POINT ( 'NONE',  ( -96.32500000000001705, 87.70503267997129626, 77.40583333333331950 ) ) ;
#52370 = CARTESIAN_POINT ( 'NONE',  ( -97.64999999999996305, -209.9999999999999716, 78.57000000000000739 ) ) ;
#52371 = CARTESIAN_POINT ( 'NONE',  ( -95.31113939543058677, -207.6265741463517998, 74.84415580543367241 ) ) ;
#52372 = FACE_OUTER_BOUND ( 'NONE', #18762, .T. ) ;
#52373 = CARTESIAN_POINT ( 'NONE',  ( 0.000000000000000000, -35.53030884539077050, -12.26510123303296851 ) ) ;
#52374 = CARTESIAN_POINT ( 'NONE',  ( 97.64999999946594755, -209.9999467985095976, 78.96687695417307395 ) ) ;
#52375 = EDGE_CURVE ( 'NONE', #60419, #23903, #39182, .T. ) ;
#52376 = ORIENTED_EDGE ( 'NONE', *, *, #56825, .T. ) ;
#52377 = CARTESIAN_POINT ( 'NONE',  ( -95.00000000000002842, 87.33691857156074434, 79.64156250086713840 ) ) ;
#52378 = PLANE ( 'NONE',  #72719 ) ;
#52379 = CARTESIAN_POINT ( 'NONE',  ( 0.000000000000000000, -27.74655509720726343, 77.16300072079651784 ) ) ;
#52380 = CARTESIAN_POINT ( 'NONE',  ( -7.670864526094549163, -97.73662565058241114, 5.500000000000000000 ) ) ;
#52381 = DIRECTION ( 'NONE',  ( -1.000000000000000000, 0.000000000000000000, 0.000000000000000000 ) ) ;
#52382 = CARTESIAN_POINT ( 'NONE',  ( 15.00000000000000000, 23.49999999999999645, 1.499999999999995337 ) ) ;
#52383 = CARTESIAN_POINT ( 'NONE',  ( -96.15314808468747287, -208.0026889286704943, 85.88572916753381037 ) ) ;
#52384 = SURFACE_STYLE_USAGE ( .BOTH. , #52014 ) ;
#52385 = ADVANCED_FACE ( 'NONE', ( #55726 ), #73746, .T. ) ;
#52386 = LINE ( 'NONE', #41125, #40836 ) ;
#52387 = EDGE_CURVE ( 'NONE', #17536, #51707, #19754, .T. ) ;
#52388 = CARTESIAN_POINT ( 'NONE',  ( 94.99999999999998579, 92.66308142843932671, 76.94281250086714863 ) ) ;
#52389 = CARTESIAN_POINT ( 'NONE',  ( -94.99999999999997158, -212.6630814284392557, 75.35531250086715715 ) ) ;
#52390 = CARTESIAN_POINT ( 'NONE',  ( 0.000000000000000000, 0.000000000000000000, 0.000000000000000000 ) ) ;
#52391 = ORIENTED_EDGE ( 'NONE', *, *, #26706, .F. ) ;
#52392 = CARTESIAN_POINT ( 'NONE',  ( -96.32500000000001705, 92.29496732002878900, 82.98854166840096980 ) ) ;
#52393 = CARTESIAN_POINT ( 'NONE',  ( 15.00000000000000000, -3.948201729842032215, 23.21447184625297666 ) ) ;
#52394 = CARTESIAN_POINT ( 'NONE',  ( 10.00000000000000000, -34.44570377933549565, -69.42325613327476219 ) ) ;
#52395 = AXIS2_PLACEMENT_3D ( 'NONE', #48559, #31626, #64750 ) ;
#52396 = CIRCLE ( 'NONE', #6791, 31.99999999999998579 ) ;
#52397 = LINE ( 'NONE', #5822, #48067 ) ;
#52398 = CARTESIAN_POINT ( 'NONE',  ( 97.30629616937498838, -209.9999999999999716, 75.35531250086714294 ) ) ;
#52399 = VERTEX_POINT ( 'NONE', #5357 ) ;
#52400 = CIRCLE ( 'NONE', #19981, 82.00000000000000000 ) ;
#52401 = LINE ( 'NONE', #42614, #37890 ) ;
#52402 = ORIENTED_EDGE ( 'NONE', *, *, #22798, .T. ) ;
#52403 = CARTESIAN_POINT ( 'NONE',  ( -92.34999999999999432, -209.9999999999999716, 90.00000000000000000 ) ) ;
#52404 = VERTEX_POINT ( 'NONE', #10229 ) ;
#52405 = DIRECTION ( 'NONE',  ( 0.000000000000000000, 0.000000000000000000, -1.000000000000000000 ) ) ;
#52406 = VERTEX_POINT ( 'NONE', #28256 ) ;
#52407 = VERTEX_POINT ( 'NONE', #33151 ) ;
#52408 = EDGE_LOOP ( 'NONE', ( #27999, #53597, #41506, #28575 ) ) ;
#52409 = CYLINDRICAL_SURFACE ( 'NONE', #63519, 31.99999999999999289 ) ;
#52410 = ORIENTED_EDGE ( 'NONE', *, *, #3675, .T. ) ;
#52411 = ORIENTED_EDGE ( 'NONE', *, *, #21395, .F. ) ;
#52412 = CARTESIAN_POINT ( 'NONE',  ( 97.30629616937498838, 90.00000000000002842, 85.03906250086714635 ) ) ;
#52413 = DIRECTION ( 'NONE',  ( 0.1276937514489679404, 0.9918136447140103451, -0.000000000000000000 ) ) ;
#52414 = DIRECTION ( 'NONE',  ( -0.000000000000000000, -0.000000000000000000, -1.000000000000000000 ) ) ;
#52415 = ORIENTED_EDGE ( 'NONE', *, *, #57164, .T. ) ;
#52416 = ORIENTED_EDGE ( 'NONE', *, *, #69928, .F. ) ;
#52417 = EDGE_CURVE ( 'NONE', #54022, #70837, #50944, .T. ) ;
#52418 = ORIENTED_EDGE ( 'NONE', *, *, #72027, .T. ) ;
#52419 = ORIENTED_EDGE ( 'NONE', *, *, #21793, .F. ) ;
#52420 = ORIENTED_EDGE ( 'NONE', *, *, #62481, .T. ) ;
#52421 = CIRCLE ( 'NONE', #20007, 16.00000000000000000 ) ;
#52422 = CARTESIAN_POINT ( 'NONE',  ( -92.35000000000005116, 88.47002178664753558, 87.72458333333332803 ) ) ;
#52423 = CARTESIAN_POINT ( 'NONE',  ( 10.00000000000000000, 65.59268652807263322, -36.72794159290169347 ) ) ;
#52424 = DIRECTION ( 'NONE',  ( 0.000000000000000000, 0.000000000000000000, -1.000000000000000000 ) ) ;
#52425 = DIRECTION ( 'NONE',  ( 0.000000000000000000, -0.9876883405951359940, -0.1564344650402420822 ) ) ;
#52426 = ADVANCED_FACE ( 'NONE', ( #51936 ), #30104, .T. ) ;
#52427 = DIRECTION ( 'NONE',  ( 1.000000000000000000, 0.000000000000000000, -0.000000000000000000 ) ) ;
#52428 = CARTESIAN_POINT ( 'NONE',  ( 10.00000000000000000, -22.74946021919153694, 29.81001611431000597 ) ) ;
#52429 = EDGE_LOOP ( 'NONE', ( #10943, #541, #73661, #41881 ) ) ;
#52430 = CARTESIAN_POINT ( 'NONE',  ( -97.64999999999994884, -211.5299782133524502, 78.06729166840096923 ) ) ;
#52431 = ORIENTED_EDGE ( 'NONE', *, *, #8247, .T. ) ;
#52432 = EDGE_CURVE ( 'NONE', #63446, #1614, #60564, .T. ) ;
#52433 = LINE ( 'NONE', #30607, #66323 ) ;
#52434 = ORIENTED_EDGE ( 'NONE', *, *, #18913, .F. ) ;
#52436 = CARTESIAN_POINT ( 'NONE',  ( -96.32500000000001705, 92.29496732002878900, 79.81354166840095843 ) ) ;
#52435 = CARTESIAN_POINT ( 'NONE',  ( 96.32499999999998863, 87.70503267997126784, 78.86104166840097207 ) ) ;
#52437 = EDGE_LOOP ( 'NONE', ( #30346, #69782, #9998, #34662 ) ) ;
#52438 = CARTESIAN_POINT ( 'NONE',  ( 93.84685191531248449, 88.00268892867053694, 80.38239583420048007 ) ) ;
#52439 = DIRECTION ( 'NONE',  ( 0.9580045777625456616, 0.2867529058022021404, 0.000000000000000000 ) ) ;
#52440 = DIRECTION ( 'NONE',  ( 0.000000000000000000, 0.000000000000000000, 1.000000000000000000 ) ) ;
#52441 = DIRECTION ( 'NONE',  ( -0.2867529058022035837, 0.9580045777625452175, 0.000000000000000000 ) ) ;
#52442 = AXIS2_PLACEMENT_3D ( 'NONE', #71455, #42913, #15817 ) ;
#52443 = DIRECTION ( 'NONE',  ( 0.000000000000000000, 0.9510565162951521989, 0.3090169943749515591 ) ) ;
#52444 = EDGE_CURVE ( 'NONE', #69078, #35859, #53055, .T. ) ;
#52445 = ORIENTED_EDGE ( 'NONE', *, *, #8147, .F. ) ;
#52446 = LINE ( 'NONE', #63031, #40942 ) ;
#52447 = CARTESIAN_POINT ( 'NONE',  ( -0.4079457818577069683, 5.537975084925943037, -5.689399939901069736 ) ) ;
#52448 = ORIENTED_EDGE ( 'NONE', *, *, #1854, .F. ) ;
#52449 = VECTOR ( 'NONE', #62939, 1000.000000000000000 ) ;
#52450 = VERTEX_POINT ( 'NONE', #64342 ) ;
#52451 = CIRCLE ( 'NONE', #59652, 16.00000000000000000 ) ;
#52452 = LINE ( 'NONE', #71866, #56499 ) ;
#52453 = CIRCLE ( 'NONE', #15218, 32.00000000000000000 ) ;
#52454 = EDGE_CURVE ( 'NONE', #68556, #16557, #850, .T. ) ;
#52455 = CARTESIAN_POINT ( 'NONE',  ( -4.084562121000262280, -3.415279651815011253, -1.156968425231159614 ) ) ;
#52456 = LINE ( 'NONE', #29517, #38971 ) ;
#52457 = CARTESIAN_POINT ( 'NONE',  ( -97.30629616937495996, -209.9999999999999716, 79.00656250086716170 ) ) ;
#52458 = ADVANCED_FACE ( 'NONE', ( #40291 ), #24121, .F. ) ;
#52459 = ORIENTED_EDGE ( 'NONE', *, *, #60635, .T. ) ;
#52460 = AXIS2_PLACEMENT_3D ( 'NONE', #44358, #10134, #56000 ) ;
#52461 = EDGE_CURVE ( 'NONE', #23684, #23048, #16124, .T. ) ;
#52462 = CYLINDRICAL_SURFACE ( 'NONE', #42697, 2.649999999999985700 ) ;
#52463 = DIRECTION ( 'NONE',  ( 0.000000000000000000, 0.000000000000000000, -1.000000000000000000 ) ) ;
#52464 = AXIS2_PLACEMENT_3D ( 'NONE', #39387, #62328, #45786 ) ;
#52465 =( NAMED_UNIT ( * ) SI_UNIT ( $, .STERADIAN. ) SOLID_ANGLE_UNIT ( ) );
#52466 = LINE ( 'NONE', #1017, #10487 ) ;
#52467 = DIRECTION ( 'NONE',  ( -0.000000000000000000, 0.3090169943749573878, 0.9510565162951503115 ) ) ;
#52468 = CYLINDRICAL_SURFACE ( 'NONE', #44460, 32.00000000000000000 ) ;
#52469 = CARTESIAN_POINT ( 'NONE',  ( 15.00000000000000000, -23.29833615347104470, 3.418703333116808629 ) ) ;
#52470 = CARTESIAN_POINT ( 'NONE',  ( 94.99999999999998579, 90.00000000000002842, 90.00000000000000000 ) ) ;
#52471 = DIRECTION ( 'NONE',  ( 0.000000000000000000, 0.7431448254773862505, 0.6691306063588672304 ) ) ;
#52472 = CIRCLE ( 'NONE', #28434, 31.99999999999998579 ) ;
#52473 = DIRECTION ( 'NONE',  ( 0.000000000000000000, 0.5000000000000003331, -0.8660254037844383745 ) ) ;
#52474 = EDGE_CURVE ( 'NONE', #66826, #21068, #12522, .T. ) ;
#52475 = ADVANCED_FACE ( 'NONE', ( #51569 ), #11337, .F. ) ;
#52476 = CARTESIAN_POINT ( 'NONE',  ( 92.69370383062498320, 90.00000000000002842, 88.53156250086716739 ) ) ;
#52477 = CARTESIAN_POINT ( 'NONE',  ( -97.30629616937497417, -211.3315407142195852, 87.31447916753381833 ) ) ;
#52478 = CARTESIAN_POINT ( 'NONE',  ( 97.64996928176852009, 91.52999594853174870, 79.01979289519825045 ) ) ;
#52479 = VERTEX_POINT ( 'NONE', #29727 ) ;
#52480 = DIRECTION ( 'NONE',  ( 0.000000000000000000, 0.000000000000000000, 1.000000000000000000 ) ) ;
#52481 = CARTESIAN_POINT ( 'NONE',  ( -92.34999999999999432, -209.9999999999999716, 82.69749999999999091 ) ) ;
#52482 = CARTESIAN_POINT ( 'NONE',  ( -93.84685191531254134, 91.99731107132950569, 74.82614583420047438 ) ) ;
#52483 = CARTESIAN_POINT ( 'NONE',  ( 97.30629616937498838, -208.6684592857803011, 86.83822916753381094 ) ) ;
#52484 = ORIENTED_EDGE ( 'NONE', *, *, #3402, .T. ) ;
#52485 = CARTESIAN_POINT ( 'NONE',  ( 10.00000000000000000, -36.73666225445940370, 65.58780272294062286 ) ) ;
#52486 = VECTOR ( 'NONE', #44624, 1000.000000000000000 ) ;
#52487 = EDGE_LOOP ( 'NONE', ( #13242, #16189, #17472, #64086 ) ) ;
#52488 = AXIS2_PLACEMENT_3D ( 'NONE', #53006, #68454, #12397 ) ;
#52489 = DIRECTION ( 'NONE',  ( 0.000000000000000000, 0.000000000000000000, 1.000000000000000000 ) ) ;
#52490 = CARTESIAN_POINT ( 'NONE',  ( 0.000000000000000000, 12.26510123303259725, 35.53030884539089840 ) ) ;
#52491 = VECTOR ( 'NONE', #32377, 1000.000000000000000 ) ;
#52492 = ORIENTED_EDGE ( 'NONE', *, *, #36408, .T. ) ;
#52493 = ORIENTED_EDGE ( 'NONE', *, *, #15714, .T. ) ;
#52494 = CARTESIAN_POINT ( 'NONE',  ( 96.15314808468750130, -211.9973110713294489, 81.12322916753382174 ) ) ;
#52495 = LINE ( 'NONE', #6293, #65684 ) ;
#52496 = DIRECTION ( 'NONE',  ( -1.000000000000000000, 0.000000000000000000, 0.000000000000000000 ) ) ;
#52497 =( BOUNDED_CURVE ( )  B_SPLINE_CURVE ( 2, ( #36486, #48515, #20310, #66189, #25582, #71428, #65084 ),
 .UNSPECIFIED., .F., .F. ) 
 B_SPLINE_CURVE_WITH_KNOTS ( ( 3, 2, 2, 3 ),
 ( 0.3333333333333333703, 0.3402777777777777901, 0.3472222222222221544, 0.3541666666666665741 ),
 .UNSPECIFIED. ) 
 CURVE ( )  GEOMETRIC_REPRESENTATION_ITEM ( )  RATIONAL_B_SPLINE_CURVE ( ( 0.9999999999999988898, 0.8660254037844398178, 1.000000000000000000, 0.8660254037844387076, 1.000000000000000000, 0.8660254037844408170, 0.9999999999999978906 ) ) 
 REPRESENTATION_ITEM ( '' )  );
#52498 = FACE_OUTER_BOUND ( 'NONE', #68512, .T. ) ;
#52499 = CARTESIAN_POINT ( 'NONE',  ( -92.35000000000003695, 89.99999998014077107, 85.95187500101400246 ) ) ;
#52500 = CARTESIAN_POINT ( 'NONE',  ( -10.00000000000000000, 0.000000000000000000, 0.000000000000000000 ) ) ;
#52501 = CARTESIAN_POINT ( 'NONE',  ( 96.32499999999998863, -207.7050326799711968, 84.70833333333332860 ) ) ;
#52502 = ADVANCED_FACE ( 'NONE', ( #1228 ), #23379, .T. ) ;
#52503 = VERTEX_POINT ( 'NONE', #35023 ) ;
#52504 = ORIENTED_EDGE ( 'NONE', *, *, #52210, .T. ) ;
#52505 = ORIENTED_EDGE ( 'NONE', *, *, #134, .F. ) ;
#52506 = ORIENTED_EDGE ( 'NONE', *, *, #44465, .T. ) ;
#52507 = DIRECTION ( 'NONE',  ( 0.000000000000000000, 0.000000000000000000, -1.000000000000000000 ) ) ;
#52508 = EDGE_CURVE ( 'NONE', #44376, #24421, #6097, .T. ) ;
#52509 = CIRCLE ( 'NONE', #8090, 42.00000000000000000 ) ;
#52510 = CARTESIAN_POINT ( 'NONE',  ( -95.00000000000002842, 87.33691857156074434, 86.78531250086716398 ) ) ;
#52511 = CARTESIAN_POINT ( 'NONE',  ( 0.000000000000000000, 0.000000000000000000, 52.00000000000002132 ) ) ;
#52512 = EDGE_CURVE ( 'NONE', #63103, #27431, #46306, .T. ) ;
#52513 = CARTESIAN_POINT ( 'NONE',  ( -3.000000000000000000, 16.83928648764945279, -16.46020748918028076 ) ) ;
#52514 = CARTESIAN_POINT ( 'NONE',  ( 95.00000000000000000, -206.9400435732949575, 76.58562500173430010 ) ) ;
#52515 = EDGE_CURVE ( 'NONE', #45539, #60065, #12084, .T. ) ;
#52516 = CARTESIAN_POINT ( 'NONE',  ( 93.67499999999999716, 87.70503267997126784, 78.67583333333332973 ) ) ;
#52517 = AXIS2_PLACEMENT_3D ( 'NONE', #5755, #30045, #51596 ) ;
#52518 = EDGE_LOOP ( 'NONE', ( #46157, #46489, #67143, #20822 ) ) ;
#52519 = CARTESIAN_POINT ( 'NONE',  ( 92.34999999999999432, 90.00000000000002842, 79.83999999999998920 ) ) ;
#52520 = VERTEX_POINT ( 'NONE', #41044 ) ;
#52521 = CARTESIAN_POINT ( 'NONE',  ( 0.000000000000000000, 41.19522573413732403, 65.64334221924923440 ) ) ;
#52522 = ORIENTED_EDGE ( 'NONE', *, *, #42222, .F. ) ;
#52523 = DIRECTION ( 'NONE',  ( -1.000000000000000000, 0.000000000000000000, 0.000000000000000000 ) ) ;
#52524 = EDGE_CURVE ( 'NONE', #49623, #35138, #118, .T. ) ;
#52525 = CARTESIAN_POINT ( 'NONE',  ( -93.84685191531252713, 88.00268892867056536, 80.48822916753381662 ) ) ;
#52526 = CARTESIAN_POINT ( 'NONE',  ( 96.15314808468748708, 88.00268892867053694, 76.51947916753380241 ) ) ;
#52527 = EDGE_LOOP ( 'NONE', ( #45423, #62905, #56459, #70787 ) ) ;
#52528 = CYLINDRICAL_SURFACE ( 'NONE', #48968, 16.00000000000000000 ) ;
#52529 = CARTESIAN_POINT ( 'NONE',  ( -7.500000000000014211, -69.70000000000003126, -255.0000000000000000 ) ) ;
#52530 = DIRECTION ( 'NONE',  ( 0.000000000000000000, 0.07845909572783793529, 0.9969173337331285190 ) ) ;
#52531 = EDGE_CURVE ( 'NONE', #25593, #70390, #2955, .T. ) ;
#52532 = CARTESIAN_POINT ( 'NONE',  ( 2.500000000000000444, 8.494897427831771708, -19.01812422950394676 ) ) ;
#52533 = ORIENTED_EDGE ( 'NONE', *, *, #42886, .F. ) ;
#52534 = CARTESIAN_POINT ( 'NONE',  ( 10.00000000000000000, 67.80270845531956070, -46.11716303203112943 ) ) ;
#52535 = CARTESIAN_POINT ( 'NONE',  ( -93.84685191531247028, -211.9973110713294489, 75.24947916753380639 ) ) ;
#52536 = ORIENTED_EDGE ( 'NONE', *, *, #44729, .F. ) ;
#52537 = ORIENTED_EDGE ( 'NONE', *, *, #35099, .F. ) ;
#52538 = DIRECTION ( 'NONE',  ( 0.000000000000000000, 0.000000000000000000, 1.000000000000000000 ) ) ;
#52539 = ORIENTED_EDGE ( 'NONE', *, *, #32311, .T. ) ;
#52540 = FACE_OUTER_BOUND ( 'NONE', #43917, .T. ) ;
#52541 = CARTESIAN_POINT ( 'NONE',  ( 10.00000000000000000, 16.23288003029543347, -33.80338159004267595 ) ) ;
#52542 = ORIENTED_EDGE ( 'NONE', *, *, #14283, .T. ) ;
#52543 = CARTESIAN_POINT ( 'NONE',  ( -97.30629616937497417, -208.6684592857803011, 87.84364583420048689 ) ) ;
#52544 = ORIENTED_EDGE ( 'NONE', *, *, #65343, .T. ) ;
#52545 = CARTESIAN_POINT ( 'NONE',  ( 97.65000000000000568, 91.52997821335252127, 88.54479166840097548 ) ) ;
#52546 = AXIS2_PLACEMENT_3D ( 'NONE', #32992, #49914, #15721 ) ;
#52547 = DIRECTION ( 'NONE',  ( 0.000000000000000000, 0.000000000000000000, 1.000000000000000000 ) ) ;
#52548 = EDGE_CURVE ( 'NONE', #37581, #13441, #62998, .T. ) ;
#52549 = ORIENTED_EDGE ( 'NONE', *, *, #43989, .F. ) ;
#52550 = EDGE_CURVE ( 'NONE', #18854, #61291, #63974, .T. ) ;
#52551 = CIRCLE ( 'NONE', #53730, 77.49899999999999523 ) ;
#52552 = VERTEX_POINT ( 'NONE', #29000 ) ;
#52553 = CARTESIAN_POINT ( 'NONE',  ( 10.00000000000000000, -18.89407956138203204, -75.16055320797050854 ) ) ;
#52554 = ADVANCED_FACE ( 'NONE', ( #23014 ), #45947, .T. ) ;
#52555 = ADVANCED_FACE ( 'NONE', ( #48152 ), #71063, .F. ) ;
#52556 = AXIS2_PLACEMENT_3D ( 'NONE', #18977, #60340, #48674 ) ;
#52557 = DIRECTION ( 'NONE',  ( 0.000000000000000000, 0.000000000000000000, -1.000000000000000000 ) ) ;
#52558 = CARTESIAN_POINT ( 'NONE',  ( 93.84685191531248449, 91.99731107132950569, 81.91697916753381037 ) ) ;
#52559 = VECTOR ( 'NONE', #110, 1000.000000000000000 ) ;
#52560 = DIRECTION ( 'NONE',  ( -1.000000000000000000, 0.000000000000000000, 0.000000000000000000 ) ) ;
#52561 = CARTESIAN_POINT ( 'NONE',  ( 10.00000000000000000, 51.02545421589402252, -55.20638768913705263 ) ) ;
#52562 = FACE_OUTER_BOUND ( 'NONE', #41969, .T. ) ;
#52563 = CARTESIAN_POINT ( 'NONE',  ( -42.50000000000000000, 0.000000000000000000, 0.000000000000000000 ) ) ;
#52564 = LINE ( 'NONE', #35634, #59660 ) ;
#52565 = LINE ( 'NONE', #1118, #26308 ) ;
#52566 = DIRECTION ( 'NONE',  ( 0.000000000000000000, 0.000000000000000000, 1.000000000000000000 ) ) ;
#52567 = EDGE_CURVE ( 'NONE', #58263, #14912, #32955, .T. ) ;
#52568 = FACE_OUTER_BOUND ( 'NONE', #33667, .T. ) ;
#52569 = DIRECTION ( 'NONE',  ( -1.000000000000000000, -0.000000000000000000, -0.000000000000000000 ) ) ;
#52570 = ADVANCED_BREP_SHAPE_REPRESENTATION ( '', ( #62892, #43395 ), #13531 ) ;
#52571 = CARTESIAN_POINT ( 'NONE',  ( -92.69370383062505425, 91.33154071421968467, 85.56822916753380071 ) ) ;
#52572 = DIRECTION ( 'NONE',  ( 2.603472992746261562E-14, 2.546204323184492723E-14, -1.000000000000000000 ) ) ;
#52573 = VECTOR ( 'NONE', #5107, 1000.000000000000000 ) ;
#52574 = CIRCLE ( 'NONE', #39385, 3.299999999999997158 ) ;
#52575 = VECTOR ( 'NONE', #13271, 1000.000000000000000 ) ;
#52576 = CARTESIAN_POINT ( 'NONE',  ( 0.000000000000000000, 0.000000000000000000, 0.000000000000000000 ) ) ;
#52577 = ORIENTED_EDGE ( 'NONE', *, *, #73086, .F. ) ;
#52578 = CIRCLE ( 'NONE', #23766, 42.00000000000000000 ) ;
#52579 = CARTESIAN_POINT ( 'NONE',  ( 0.000000000000000000, 51.03279382321166224, -55.19960302592011914 ) ) ;
#52580 = LINE ( 'NONE', #65360, #63605 ) ;
#52581 = CARTESIAN_POINT ( 'NONE',  ( 0.000000000000000000, 0.000000000000000000, 0.000000000000000000 ) ) ;
#52582 = CARTESIAN_POINT ( 'NONE',  ( 0.000000000000000000, -8.966570791700153364, -81.50828551894237251 ) ) ;
#52583 = CARTESIAN_POINT ( 'NONE',  ( 96.15314808468750130, -211.9973110713294489, 80.48822916753381662 ) ) ;
#52584 = ORIENTED_EDGE ( 'NONE', *, *, #2957, .F. ) ;
#52585 = VERTEX_POINT ( 'NONE', #9031 ) ;
#52586 = DIRECTION ( 'NONE',  ( 0.000000000000000000, 0.000000000000000000, 1.000000000000000000 ) ) ;
#52587 = ORIENTED_EDGE ( 'NONE', *, *, #11205, .T. ) ;
#52588 = DIRECTION ( 'NONE',  ( 0.6575728627325957421, -0.7533909544171993877, -1.230411769795008318E-16 ) ) ;
#52589 = CARTESIAN_POINT ( 'NONE',  ( 96.73972734126404305, -208.4859488783623362, 74.79348190356850523 ) ) ;
#52590 = AXIS2_PLACEMENT_3D ( 'NONE', #43847, #33657, #55483 ) ;
#52591 = EDGE_LOOP ( 'NONE', ( #69909, #45942, #61717, #38737 ) ) ;
#52592 = CARTESIAN_POINT ( 'NONE',  ( 92.69370383062501162, -208.6684592857803011, 78.95364583420048632 ) ) ;
#52593 = MECHANICAL_DESIGN_GEOMETRIC_PRESENTATION_REPRESENTATION (  '', ( #61027 ), #4598 ) ;
#52594 = AXIS2_PLACEMENT_3D ( 'NONE', #37878, #26208, #9290 ) ;
#52595 = ORIENTED_EDGE ( 'NONE', *, *, #15186, .F. ) ;
#52596 = ADVANCED_FACE ( 'NONE', ( #70687 ), #42889, .F. ) ;
#52597 = CARTESIAN_POINT ( 'NONE',  ( 96.32499999999997442, 92.29496732002878900, 80.34270833506762699 ) ) ;
#52598 = ORIENTED_EDGE ( 'NONE', *, *, #28095, .F. ) ;
#52599 = VERTEX_POINT ( 'NONE', #8672 ) ;
#52600 = CARTESIAN_POINT ( 'NONE',  ( 11.99999999999999822, 0.000000000000000000, 0.000000000000000000 ) ) ;
#52601 = CIRCLE ( 'NONE', #38229, 77.49899999999998101 ) ;
#52602 = EDGE_CURVE ( 'NONE', #10842, #10255, #31584, .T. ) ;
#52603 =( NAMED_UNIT ( * ) PLANE_ANGLE_UNIT ( ) SI_UNIT ( $, .RADIAN. ) );
#52604 = CARTESIAN_POINT ( 'NONE',  ( -10.00000000000000000, 0.000000000000000000, 0.000000000000000000 ) ) ;
#52605 = AXIS2_PLACEMENT_3D ( 'NONE', #48142, #70677, #61557 ) ;
#52606 = VERTEX_POINT ( 'NONE', #19203 ) ;
#52607 = DIRECTION ( 'NONE',  ( -1.000000000000000000, 0.000000000000000000, 0.000000000000000000 ) ) ;
#52608 = CARTESIAN_POINT ( 'NONE',  ( 95.00000000000000000, -213.0599564267049857, 86.42812500173430124 ) ) ;
#52609 = EDGE_CURVE ( 'NONE', #50553, #36680, #25950, .T. ) ;
#52610 = CARTESIAN_POINT ( 'NONE',  ( 97.64999999999997726, 88.47002178664753558, 87.72458333333332803 ) ) ;
#52611 = EDGE_CURVE ( 'NONE', #15234, #41319, #60552, .T. ) ;
#52612 = ORIENTED_EDGE ( 'NONE', *, *, #42342, .T. ) ;
#52613 = CARTESIAN_POINT ( 'NONE',  ( 92.35000000003287823, 90.00000839536618003, 84.99910573348789455 ) ) ;
#52614 = ORIENTED_EDGE ( 'NONE', *, *, #67019, .T. ) ;
#52615 = ORIENTED_EDGE ( 'NONE', *, *, #6983, .F. ) ;
#52616 = CARTESIAN_POINT ( 'NONE',  ( 0.000000000000000000, 55.20638768913831029, -51.02545421589267960 ) ) ;
#52617 = ORIENTED_EDGE ( 'NONE', *, *, #46631, .F. ) ;
#52618 = CARTESIAN_POINT ( 'NONE',  ( 96.32499999999997442, 92.29496732002878900, 86.69270833506763552 ) ) ;
#52619 = VECTOR ( 'NONE', #61081, 1000.000000000000000 ) ;
#52620 = ORIENTED_EDGE ( 'NONE', *, *, #56292, .F. ) ;
#52621 = VERTEX_POINT ( 'NONE', #2329 ) ;
#52622 = DIRECTION ( 'NONE',  ( -1.000000000000000000, 0.000000000000000000, 0.000000000000000000 ) ) ;
#52623 = CARTESIAN_POINT ( 'NONE',  ( -4.999999999999998224, -2.058885705017527989, -1.328630925609301183 ) ) ;
#52624 = VERTEX_POINT ( 'NONE', #48881 ) ;
#52625 = CIRCLE ( 'NONE', #11775, 16.00000000000000355 ) ;
#52626 = ORIENTED_EDGE ( 'NONE', *, *, #12659, .F. ) ;
#52627 = CIRCLE ( 'NONE', #71822, 77.49899999999999523 ) ;
#52628 = ORIENTED_EDGE ( 'NONE', *, *, #29505, .T. ) ;
#52629 = CARTESIAN_POINT ( 'NONE',  ( 11.99999999999999822, 72.35432306680455383, 20.40083707023012494 ) ) ;
#52630 = DIRECTION ( 'NONE',  ( 1.000000000000000000, 1.427937372958405461E-15, 7.962523111839130290E-16 ) ) ;
#52631 = CIRCLE ( 'NONE', #3441, 16.00000000000000355 ) ;
#52632 = ADVANCED_FACE ( 'NONE', ( #7923 ), #13918, .T. ) ;
#52633 = AXIS2_PLACEMENT_3D ( 'NONE', #44813, #39542, #67740 ) ;
#52634 = CARTESIAN_POINT ( 'NONE',  ( -96.32500000000001705, 87.70503267997129626, 86.29583333333333428 ) ) ;
#52635 = ORIENTED_EDGE ( 'NONE', *, *, #73273, .T. ) ;
#52636 = CARTESIAN_POINT ( 'NONE',  ( 92.34999999999999432, 90.00000000000002842, 81.74500000000000455 ) ) ;
#52637 = AXIS2_PLACEMENT_3D ( 'NONE', #14299, #8291, #3056 ) ;
#52638 = CARTESIAN_POINT ( 'NONE',  ( 10.00000000000000000, 21.53537804866081373, 30.80686688397018358 ) ) ;
#52639 = VERTEX_POINT ( 'NONE', #30839 ) ;
#52640 = DIRECTION ( 'NONE',  ( 0.000000000000000000, 0.000000000000000000, -1.000000000000000000 ) ) ;
#52641 = CARTESIAN_POINT ( 'NONE',  ( -97.30629616937497417, -211.3315407142195852, 81.44072916753381719 ) ) ;
#52642 = ORIENTED_EDGE ( 'NONE', *, *, #21212, .F. ) ;
#52643 = CARTESIAN_POINT ( 'NONE',  ( 10.00000000000000000, 0.000000000000000000, 0.000000000000000000 ) ) ;
#52644 = CARTESIAN_POINT ( 'NONE',  ( 92.49271422325850267, -210.3406226724007979, 74.92458348457969919 ) ) ;
#52645 = DIRECTION ( 'NONE',  ( -1.000000000000000000, 0.000000000000000000, 0.000000000000000000 ) ) ;
#52646 = CARTESIAN_POINT ( 'NONE',  ( -97.30629616937495996, -209.9999999999999716, 76.94281250086713442 ) ) ;
#52647 = CARTESIAN_POINT ( 'NONE',  ( 0.000000000000000000, 20.40083707022987625, -72.35432306680462489 ) ) ;
#52648 = EDGE_CURVE ( 'NONE', #48671, #24035, #13556, .T. ) ;
#52649 = ADVANCED_FACE ( 'NONE', ( #31955 ), #54170, .T. ) ;
#52650 = FACE_OUTER_BOUND ( 'NONE', #63994, .T. ) ;
#52651 = CARTESIAN_POINT ( 'NONE',  ( 0.000000000000000000, 37.01155633439068282, -6.555932627142014191 ) ) ;
#52652 = DIRECTION ( 'NONE',  ( 0.000000000000000000, -0.000000000000000000, -1.000000000000000000 ) ) ;
#52653 = CARTESIAN_POINT ( 'NONE',  ( 97.64999999999992042, 88.47002178664749295, 88.35958333333334735 ) ) ;
#52654 = CARTESIAN_POINT ( 'NONE',  ( -93.84685191531254134, 91.99731107132950569, 78.63614583420047666 ) ) ;
#52655 = DIRECTION ( 'NONE',  ( -0.000000000000000000, -0.000000000000000000, -1.000000000000000000 ) ) ;
#52656 = CARTESIAN_POINT ( 'NONE',  ( 5.000000000000000000, 33.71516098798740302, 74.74816331893443078 ) ) ;
#52657 = VECTOR ( 'NONE', #48999, 1000.000000000000000 ) ;
#52658 = ORIENTED_EDGE ( 'NONE', *, *, #42954, .T. ) ;
#52659 = CARTESIAN_POINT ( 'NONE',  ( 11.99999999999999822, -68.67312586194971402, -35.91791733033549860 ) ) ;
#52660 = CIRCLE ( 'NONE', #45490, 16.00000000000000355 ) ;
#52661 = CIRCLE ( 'NONE', #26238, 77.49899999999999523 ) ;
#52662 = CARTESIAN_POINT ( 'NONE',  ( 92.35000000005783249, -210.0000112241611703, 75.47473230081648410 ) ) ;
#52663 = CARTESIAN_POINT ( 'NONE',  ( -3.961125083139900749, -143.2122702051246677, -5.500000000000000000 ) ) ;
#52665 = AXIS2_PLACEMENT_3D ( 'NONE', #30453, #30090, #47395 ) ;
#52664 = CARTESIAN_POINT ( 'NONE',  ( -94.99999999999997158, -209.9999999999999716, 90.00000000000000000 ) ) ;
#52666 = CARTESIAN_POINT ( 'NONE',  ( -10.00000000000000000, 0.000000000000000000, 0.000000000000000000 ) ) ;
#52667 = CARTESIAN_POINT ( 'NONE',  ( -92.35000000000003695, 90.00000000000004263, 90.00000000000000000 ) ) ;
#52668 = CARTESIAN_POINT ( 'NONE',  ( -96.15314808468745866, -211.9973110713294489, 77.20739583420048291 ) ) ;
#52669 = VECTOR ( 'NONE', #65453, 1000.000000000000000 ) ;
#52670 = DIRECTION ( 'NONE',  ( -0.000000000000000000, -0.000000000000000000, 1.000000000000000000 ) ) ;
#52671 = ORIENTED_EDGE ( 'NONE', *, *, #55071, .F. ) ;
#52672 = CARTESIAN_POINT ( 'NONE',  ( -0.0004442498507136653329, 0.001194404164628348752, -70.59999999999999432 ) ) ;
#52673 = DIRECTION ( 'NONE',  ( 0.000000000000000000, 0.000000000000000000, 1.000000000000000000 ) ) ;
#52675 = SURFACE_STYLE_FILL_AREA ( #12445 ) ;
#52674 = AXIS2_PLACEMENT_3D ( 'NONE', #48580, #8360, #66253 ) ;
#52676 = DIRECTION ( 'NONE',  ( 0.000000000000000000, 0.5877852522924797984, -0.8090169943749426773 ) ) ;
#52677 = AXIS2_PLACEMENT_3D ( 'NONE', #59395, #70647, #19526 ) ;
#52678 = AXIS2_PLACEMENT_3D ( 'NONE', #13125, #69897, #1532 ) ;
#52680 = DIRECTION ( 'NONE',  ( 0.000000000000000000, -0.4539904997395541320, 0.8910065241883640130 ) ) ;
#52679 = AXIS2_PLACEMENT_3D ( 'NONE', #58706, #53070, #29380 ) ;
#52681 = ORIENTED_EDGE ( 'NONE', *, *, #34386, .F. ) ;
#52682 = AXIS2_PLACEMENT_3D ( 'NONE', #16240, #60988, #61375 ) ;
#52683 = DIRECTION ( 'NONE',  ( 0.000000000000000000, 0.000000000000000000, -1.000000000000000000 ) ) ;
#52684 = FACE_OUTER_BOUND ( 'NONE', #49180, .T. ) ;
#52685 = VERTEX_POINT ( 'NONE', #1958 ) ;
#52686 = APPLICATION_CONTEXT ( 'automotive_design' ) ;
#52687 = AXIS2_PLACEMENT_3D ( 'NONE', #17639, #2142, #36682 ) ;
#52688 = CARTESIAN_POINT ( 'NONE',  ( 96.15314808468750130, -211.9973110713294489, 86.67947916753381321 ) ) ;
#52689 = DIRECTION ( 'NONE',  ( 1.000000000000000000, 0.000000000000000000, 0.000000000000000000 ) ) ;
#52690 = ORIENTED_EDGE ( 'NONE', *, *, #27048, .F. ) ;
#52691 = PRODUCT_DEFINITION ( 'UNKNOWN', '', #62881, #72441 ) ;
#52692 = EDGE_CURVE ( 'NONE', #57437, #32439, #52497, .T. ) ;
#52693 = CARTESIAN_POINT ( 'NONE',  ( 95.00000000000000000, -212.6630814284392557, 89.32531250086715602 ) ) ;
#52694 = EDGE_LOOP ( 'NONE', ( #39590, #55380, #52997, #8865 ) ) ;
#52695 = CARTESIAN_POINT ( 'NONE',  ( 0.000000000000000000, -0.8299999999999999600, -1.199999999999999956 ) ) ;
#52696 = ORIENTED_EDGE ( 'NONE', *, *, #68496, .T. ) ;
#52697 = CARTESIAN_POINT ( 'NONE',  ( -97.30629616937501680, 91.33154071421968467, 82.12864583420048348 ) ) ;
#52698 = ORIENTED_EDGE ( 'NONE', *, *, #16325, .F. ) ;
#52699 = EDGE_CURVE ( 'NONE', #1386, #370, #19934, .T. ) ;
#52700 = ORIENTED_EDGE ( 'NONE', *, *, #55586, .F. ) ;
#52701 = CARTESIAN_POINT ( 'NONE',  ( 12.00000000000000000, -3.948201729842032215, 23.21447184625297666 ) ) ;
#52702 = ORIENTED_EDGE ( 'NONE', *, *, #17541, .F. ) ;
#52703 = DIRECTION ( 'NONE',  ( -0.000000000000000000, -0.000000000000000000, -1.000000000000000000 ) ) ;
#52704 = DIRECTION ( 'NONE',  ( -1.000000000000000000, 0.000000000000000000, -0.000000000000000000 ) ) ;
#52705 = EDGE_CURVE ( 'NONE', #39783, #62434, #70317, .T. ) ;
#52706 = ORIENTED_EDGE ( 'NONE', *, *, #43186, .F. ) ;
#52707 = DIRECTION ( 'NONE',  ( 1.000000000000000000, 0.000000000000000000, 0.000000000000000000 ) ) ;
#52708 = EDGE_LOOP ( 'NONE', ( #67306, #21855, #30481, #6026 ) ) ;
#52709 = CARTESIAN_POINT ( 'NONE',  ( 94.37155072198197558, 87.44368763736524386, 74.98613922222769190 ) ) ;
#52710 = EDGE_CURVE ( 'NONE', #35415, #26778, #36121, .T. ) ;
#52711 = AXIS2_PLACEMENT_3D ( 'NONE', #58747, #64760, #42202 ) ;
#52712 = CIRCLE ( 'NONE', #56314, 77.49899999999999523 ) ;
#52713 = ORIENTED_EDGE ( 'NONE', *, *, #11003, .T. ) ;
#52714 = VERTEX_POINT ( 'NONE', #13192 ) ;
#52715 = ORIENTED_EDGE ( 'NONE', *, *, #6385, .F. ) ;
#52716 = CARTESIAN_POINT ( 'NONE',  ( 93.84685191531251292, -211.9973110713294489, 80.85864583420047325 ) ) ;
#52717 = APPLICATION_PROTOCOL_DEFINITION ( 'draft international standard', 'automotive_design', 1998, #52245 ) ;
#52718 = CARTESIAN_POINT ( 'NONE',  ( -97.64999999999996305, -209.9999999999999716, 76.66499999999999204 ) ) ;
#52719 = CIRCLE ( 'NONE', #37113, 31.99999999999998934 ) ;
#52720 = CARTESIAN_POINT ( 'NONE',  ( -2.500000000000016431, -76.30000000000001137, -204.9999999999999716 ) ) ;
#52721 = AXIS2_PLACEMENT_3D ( 'NONE', #37896, #13467, #48060 ) ;
#52722 = DIRECTION ( 'NONE',  ( -1.000000000000000000, -0.000000000000000000, -0.000000000000000000 ) ) ;
#52723 = DIRECTION ( 'NONE',  ( 0.000000000000000000, 0.000000000000000000, 1.000000000000000000 ) ) ;
#52724 = CARTESIAN_POINT ( 'NONE',  ( -92.35000000000009379, 88.47002178664753558, 82.64458333333332973 ) ) ;
#52725 = CARTESIAN_POINT ( 'NONE',  ( -96.15314808468745866, -211.9973110713294489, 83.39864583420047950 ) ) ;
#52726 = EDGE_CURVE ( 'NONE', #69188, #55213, #59069, .T. ) ;
#52727 = CARTESIAN_POINT ( 'NONE',  ( -95.00000000000002842, 92.66308142843932671, 83.92781250086716227 ) ) ;
#52728 = EDGE_CURVE ( 'NONE', #73858, #9978, #71370, .T. ) ;
#52729 = ORIENTED_EDGE ( 'NONE', *, *, #60851, .F. ) ;
#52730 = CARTESIAN_POINT ( 'NONE',  ( 94.99999999999998579, 92.66308142843935514, 79.95906250086713385 ) ) ;
#52731 = ORIENTED_EDGE ( 'NONE', *, *, #58163, .T. ) ;
#52732 = DIRECTION ( 'NONE',  ( 0.000000000000000000, 0.000000000000000000, 1.000000000000000000 ) ) ;
#52733 = DIRECTION ( 'NONE',  ( 0.000000000000000000, 0.000000000000000000, 1.000000000000000000 ) ) ;
#52734 = CARTESIAN_POINT ( 'NONE',  ( 11.99999999999999822, 0.000000000000000000, 0.000000000000000000 ) ) ;
#52735 = DIRECTION ( 'NONE',  ( -0.9580045777625459946, -0.2867529058022011412, 0.000000000000000000 ) ) ;
#52736 = CARTESIAN_POINT ( 'NONE',  ( -5.000000000000000000, 1.947085426416883980, -5.800379292880308846 ) ) ;
#52737 = AXIS2_PLACEMENT_3D ( 'NONE', #56455, #50790, #73717 ) ;
#52738 = CARTESIAN_POINT ( 'NONE',  ( -96.15314808468745866, -211.9973110713294489, 87.84364583420047268 ) ) ;
#52739 = LINE ( 'NONE', #46363, #21056 ) ;
#52740 = CIRCLE ( 'NONE', #51490, 82.00000000000000000 ) ;
#52741 = CARTESIAN_POINT ( 'NONE',  ( 11.99999999999999822, 0.000000000000000000, 0.000000000000000000 ) ) ;
#52742 = CYLINDRICAL_SURFACE ( 'NONE', #10283, 31.99999999999998579 ) ;
#52743 = DIRECTION ( 'NONE',  ( 0.000000000000000000, -0.8526401643540970632, 0.5224985647159410274 ) ) ;
#52744 = ORIENTED_EDGE ( 'NONE', *, *, #6206, .T. ) ;
#52745 = CIRCLE ( 'NONE', #16733, 42.00000000000000000 ) ;
#52746 = EDGE_CURVE ( 'NONE', #32129, #21226, #4907, .T. ) ;
#52747 = AXIS2_PLACEMENT_3D ( 'NONE', #38663, #43939, #10080 ) ;
#52748 = VERTEX_POINT ( 'NONE', #49252 ) ;
#52749 = VECTOR ( 'NONE', #33746, 1000.000000000000000 ) ;
#52750 = CIRCLE ( 'NONE', #69540, 82.00000000000000000 ) ;
#52751 = CARTESIAN_POINT ( 'NONE',  ( -96.32500000000001705, 92.29496732002878900, 77.82916666666665151 ) ) ;
#52752 = CYLINDRICAL_SURFACE ( 'NONE', #4399, 82.00000000000000000 ) ;
#52753 = CYLINDRICAL_SURFACE ( 'NONE', #68117, 16.00000000000000000 ) ;
#52754 = DIRECTION ( 'NONE',  ( -0.000000000000000000, -0.000000000000000000, 1.000000000000000000 ) ) ;
#52755 = DIRECTION ( 'NONE',  ( -1.000000000000000000, 0.000000000000000000, -0.000000000000000000 ) ) ;
#52756 = DIRECTION ( 'NONE',  ( -1.000000000000000000, -0.000000000000000000, 0.000000000000000000 ) ) ;
#52757 = CARTESIAN_POINT ( 'NONE',  ( 10.00000000000000000, -30.00120703465189465, -22.64427369931201639 ) ) ;
#52758 = VECTOR ( 'NONE', #31777, 999.9999999999998863 ) ;
#52759 =( BOUNDED_CURVE ( )  B_SPLINE_CURVE ( 2, ( #12490, #13234, #35428, #23415, #18865, #58356, #6856 ),
 .UNSPECIFIED., .F., .F. ) 
 B_SPLINE_CURVE_WITH_KNOTS ( ( 3, 2, 2, 3 ),
 ( 0.3125000000000001665, 0.3194444444444445308, 0.3263888888888890061, 0.3333333333333333703 ),
 .UNSPECIFIED. ) 
 CURVE ( )  GEOMETRIC_REPRESENTATION_ITEM ( )  RATIONAL_B_SPLINE_CURVE ( ( 0.9999999999999967804, 0.8660254037844419273, 1.000000000000000000, 0.8660254037844387076, 1.000000000000000000, 0.8660254037844375974, 1.000000000000001110 ) ) 
 REPRESENTATION_ITEM ( '' )  );
#52760 = VERTEX_POINT ( 'NONE', #56393 ) ;
#52761 = CARTESIAN_POINT ( 'NONE',  ( -96.15314808468752972, 91.99731107132950569, 75.56697916753381605 ) ) ;
#52762 = DIRECTION ( 'NONE',  ( -0.000000000000000000, -0.000000000000000000, -1.000000000000000000 ) ) ;
#52763 = CARTESIAN_POINT ( 'NONE',  ( 92.35000000002597176, -210.0000000000000284, -64.99999999999356248 ) ) ;
#52764 = DIRECTION ( 'NONE',  ( -1.000000000000000000, -0.000000000000000000, -0.000000000000000000 ) ) ;
#52765 = FACE_OUTER_BOUND ( 'NONE', #52958, .T. ) ;
#52766 = CARTESIAN_POINT ( 'NONE',  ( -93.67500000000003979, 87.70503267997129626, 75.68604166840097491 ) ) ;
#52767 = CARTESIAN_POINT ( 'NONE',  ( -94.99999999999997158, -207.3369185715606307, 84.56281250086716739 ) ) ;
#52768 = CARTESIAN_POINT ( 'NONE',  ( 0.000000000000000000, 0.000000000000000000, -275.0000000000000000 ) ) ;
#52769 = CIRCLE ( 'NONE', #1236, 31.99999999999998579 ) ;
#52770 = CARTESIAN_POINT ( 'NONE',  ( 10.00000000000000000, 0.000000000000000000, 0.000000000000000000 ) ) ;
#52771 = AXIS2_PLACEMENT_3D ( 'NONE', #55752, #27543, #72646 ) ;
#52772 = ADVANCED_FACE ( 'NONE', ( #9772 ), #56767, .T. ) ;
#52773 = CIRCLE ( 'NONE', #21514, 31.99999999999999289 ) ;
#52774 = CARTESIAN_POINT ( 'NONE',  ( -93.84685191531247028, -211.9973110713294489, 76.67822916753381435 ) ) ;
#52775 = FACE_OUTER_BOUND ( 'NONE', #69438, .T. ) ;
#52776 = ORIENTED_EDGE ( 'NONE', *, *, #64982, .T. ) ;
#52777 = LINE ( 'NONE', #210, #29259 ) ;
#52778 = CARTESIAN_POINT ( 'NONE',  ( 10.00000000000000000, -35.95386929396264009, 10.96151621346475658 ) ) ;
#52779 = VECTOR ( 'NONE', #15840, 1000.000000000000227 ) ;
#52780 = CARTESIAN_POINT ( 'NONE',  ( -92.35000982492222477, 88.47001611422608391, 88.43895794268867405 ) ) ;
#52781 = AXIS2_PLACEMENT_3D ( 'NONE', #50521, #73068, #34997 ) ;
#52782 = EDGE_CURVE ( 'NONE', #62190, #70424, #72539, .T. ) ;
#52783 = CARTESIAN_POINT ( 'NONE',  ( -92.69370383062505425, 88.66845928578038638, 76.09614583420048461 ) ) ;
#52784 = CARTESIAN_POINT ( 'NONE',  ( 92.69370383062501162, -208.6684592857803011, 76.88989583420047325 ) ) ;
#52785 = ORIENTED_EDGE ( 'NONE', *, *, #52791, .F. ) ;
#52786 = EDGE_CURVE ( 'NONE', #48148, #39717, #63055, .T. ) ;
#52787 = DIRECTION ( 'NONE',  ( -1.000000000000000000, 0.000000000000000000, -0.000000000000000000 ) ) ;
#52788 = VERTEX_POINT ( 'NONE', #32321 ) ;
#52789 = DIRECTION ( 'NONE',  ( 0.000000000000000000, 0.000000000000000000, 1.000000000000000000 ) ) ;
#52790 = VERTEX_POINT ( 'NONE', #50360 ) ;
#52791 = EDGE_CURVE ( 'NONE', #30232, #59737, #24591, .T. ) ;
#52792 = AXIS2_PLACEMENT_3D ( 'NONE', #1186, #13877, #12408 ) ;
#52793 = DIRECTION ( 'NONE',  ( 0.000000000000000000, 0.000000000000000000, 1.000000000000000000 ) ) ;
#52794 = VECTOR ( 'NONE', #21186, 1000.000000000000227 ) ;
#52795 = ORIENTED_EDGE ( 'NONE', *, *, #11275, .F. ) ;
#52796 = ORIENTED_EDGE ( 'NONE', *, *, #7906, .T. ) ;
#52797 = VERTEX_POINT ( 'NONE', #49982 ) ;
#52798 = AXIS2_PLACEMENT_3D ( 'NONE', #30382, #53328, #1129 ) ;
#52799 = DIRECTION ( 'NONE',  ( 0.000000000000000000, 0.5877852522924743583, -0.8090169943749466741 ) ) ;
#52800 = ORIENTED_EDGE ( 'NONE', *, *, #51461, .T. ) ;
#52801 = EDGE_LOOP ( 'NONE', ( #60128, #1172, #66035, #56587 ) ) ;
#52802 = CARTESIAN_POINT ( 'NONE',  ( 94.99999999999998579, 87.33691857156068750, 84.88031250086714863 ) ) ;
#52803 = CARTESIAN_POINT ( 'NONE',  ( 15.00000000000000000, -22.32062822937469093, 14.36278369418830181 ) ) ;
#52804 = EDGE_CURVE ( 'NONE', #23577, #19685, #33060, .T. ) ;
#52805 = DIRECTION ( 'NONE',  ( -0.000000000000000000, -0.000000000000000000, 1.000000000000000000 ) ) ;
#52806 = VERTEX_POINT ( 'NONE', #4526 ) ;
#52807 = ORIENTED_EDGE ( 'NONE', *, *, #48286, .T. ) ;
#52808 = ORIENTED_EDGE ( 'NONE', *, *, #45070, .T. ) ;
#52809 = CARTESIAN_POINT ( 'NONE',  ( 10.00000000000000000, -8.966570791700142706, -81.50828551894234408 ) ) ;
#52810 = VERTEX_POINT ( 'NONE', #20682 ) ;
#52811 = DIRECTION ( 'NONE',  ( 1.000000000000000000, 0.000000000000000000, 0.000000000000000000 ) ) ;
#52812 = CARTESIAN_POINT ( 'NONE',  ( -94.99999999999997158, -206.9400435732949575, 75.31562500173430408 ) ) ;
#52813 = CARTESIAN_POINT ( 'NONE',  ( 92.34999999999999432, 90.00000000000002842, 83.65000000000000568 ) ) ;
#52814 = CARTESIAN_POINT ( 'NONE',  ( 26.47460221209471598, -121.8961639463267090, -5.500000000000000000 ) ) ;
#52815 = DIRECTION ( 'NONE',  ( 0.000000000000000000, 0.000000000000000000, 1.000000000000000000 ) ) ;
#52816 = CARTESIAN_POINT ( 'NONE',  ( 10.00000000000000000, 31.46837873495072913, -68.27212725128242710 ) ) ;
#52817 = CARTESIAN_POINT ( 'NONE',  ( 0.000000000000000000, 0.8828120875900632436, 37.48860685352291000 ) ) ;
#52818 = CARTESIAN_POINT ( 'NONE',  ( -93.67499999999998295, -212.2949673200287179, 78.86104166840097207 ) ) ;
#52820 = ORIENTED_EDGE ( 'NONE', *, *, #43218, .F. ) ;
#52819 = EDGE_CURVE ( 'NONE', #9978, #73858, #30589, .T. ) ;
#52821 = LINE ( 'NONE', #36260, #9851 ) ;
#52822 = EDGE_CURVE ( 'NONE', #3895, #55045, #22172, .T. ) ;
#52823 = ORIENTED_EDGE ( 'NONE', *, *, #24362, .F. ) ;
#52825 = CARTESIAN_POINT ( 'NONE',  ( -96.32500000000001705, 87.70503267997129626, 75.58020833506763836 ) ) ;
#52824 = CARTESIAN_POINT ( 'NONE',  ( 93.67499999999999716, 87.70503267997126784, 78.75520833506763552 ) ) ;
#52826 = VECTOR ( 'NONE', #18784, 1000.000000000000000 ) ;
#52828 = EDGE_CURVE ( 'NONE', #53528, #39808, #49805, .T. ) ;
#52827 = VERTEX_POINT ( 'NONE', #73287 ) ;
#52829 = CARTESIAN_POINT ( 'NONE',  ( 92.69370383062498320, 91.33154071421968467, 79.58864583420047722 ) ) ;
#52830 = DIRECTION ( 'NONE',  ( -1.000000000000000000, -0.000000000000000000, 0.000000000000000000 ) ) ;
#52831 = DIRECTION ( 'NONE',  ( 0.000000000000000000, 0.000000000000000000, 1.000000000000000000 ) ) ;
#52832 = CIRCLE ( 'NONE', #9570, 82.00000000000000000 ) ;
#52833 = DIRECTION ( 'NONE',  ( 0.000000000000000000, 0.000000000000000000, 1.000000000000000000 ) ) ;
#52834 = CARTESIAN_POINT ( 'NONE',  ( -10.00000000000000000, 0.000000000000000000, 0.000000000000000000 ) ) ;
#52835 = AXIS2_PLACEMENT_3D ( 'NONE', #21957, #62576, #32854 ) ;
#52836 = ORIENTED_EDGE ( 'NONE', *, *, #62980, .T. ) ;
#52837 = DIRECTION ( 'NONE',  ( -7.945298363252408085E-16, -1.065814103640131188E-14, -1.000000000000000000 ) ) ;
#52838 = CARTESIAN_POINT ( 'NONE',  ( 10.00000000000000000, -37.58145647212455032, 16.68533520207890319 ) ) ;
#52839 = ORIENTED_EDGE ( 'NONE', *, *, #58838, .T. ) ;
#52840 = ORIENTED_EDGE ( 'NONE', *, *, #70421, .F. ) ;
#52841 = CIRCLE ( 'NONE', #39642, 31.99999999999998579 ) ;
#52842 = DIRECTION ( 'NONE',  ( -1.000000000000000000, -0.000000000000000000, -0.000000000000000000 ) ) ;
#52843 = CARTESIAN_POINT ( 'NONE',  ( 0.000000000000000000, 0.000000000000000000, 0.000000000000000000 ) ) ;
#52844 = CARTESIAN_POINT ( 'NONE',  ( 11.99999999999999822, -11.30684508768284680, -76.66974797899850103 ) ) ;
#52845 = CARTESIAN_POINT ( 'NONE',  ( -92.69370383062498320, -208.6684592857803011, 78.74197916753382742 ) ) ;
#52846 = ORIENTED_EDGE ( 'NONE', *, *, #73074, .F. ) ;
#52847 = AXIS2_PLACEMENT_3D ( 'NONE', #62277, #4781, #55885 ) ;
#52848 = DIRECTION ( 'NONE',  ( 0.000000000000000000, 0.000000000000000000, 1.000000000000000000 ) ) ;
#52849 = AXIS2_PLACEMENT_3D ( 'NONE', #62780, #62018, #11246 ) ;
#52850 = VECTOR ( 'NONE', #45628, 1000.000000000000114 ) ;
#52851 = CIRCLE ( 'NONE', #4838, 77.49900000000000944 ) ;
#52852 = CYLINDRICAL_SURFACE ( 'NONE', #72628, 2.649999999999985700 ) ;
#52853 = CARTESIAN_POINT ( 'NONE',  ( -92.35000000000003695, 90.00000000000004263, 83.96750000000000114 ) ) ;
#52854 = CARTESIAN_POINT ( 'NONE',  ( -99.99999999999997158, -214.9999999999999716, -90.00000000000000000 ) ) ;
#52855 = DIRECTION ( 'NONE',  ( -1.000000000000000000, -0.000000000000000000, -0.000000000000000000 ) ) ;
#52856 = DIRECTION ( 'NONE',  ( -1.000000000000000000, 0.000000000000000000, 0.000000000000000000 ) ) ;
#52857 = AXIS2_PLACEMENT_3D ( 'NONE', #58262, #23678, #12390 ) ;
#52858 = DIRECTION ( 'NONE',  ( -1.000000000000000000, 0.000000000000000000, 0.000000000000000000 ) ) ;
#52859 = AXIS2_PLACEMENT_3D ( 'NONE', #68877, #23384, #46310 ) ;
#52860 = CARTESIAN_POINT ( 'NONE',  ( -89.99999999999998579, -124.0000000000000142, 39.99999999999996447 ) ) ;
#52861 = DIRECTION ( 'NONE',  ( 1.000000000000000000, 0.000000000000000000, 0.000000000000000000 ) ) ;
#52862 = CARTESIAN_POINT ( 'NONE',  ( 94.99999999999998579, 92.66308142843932671, 87.10281250086715943 ) ) ;
#52863 = CARTESIAN_POINT ( 'NONE',  ( -97.30629616937495996, -209.9999999999999716, 85.99156250086716113 ) ) ;
#52864 = CARTESIAN_POINT ( 'NONE',  ( 19.29194287201271862, -133.5026271600380880, 5.500000000000000000 ) ) ;
#52866 = EDGE_CURVE ( 'NONE', #22274, #27546, #10210, .T. ) ;
#52865 = ORIENTED_EDGE ( 'NONE', *, *, #25951, .T. ) ;
#52867 = CARTESIAN_POINT ( 'NONE',  ( 97.64999999999999147, -209.9999999999999716, 83.41187500173430180 ) ) ;
#52868 = CARTESIAN_POINT ( 'NONE',  ( -94.99999999999997158, -206.9400435732949575, 79.68124999999999147 ) ) ;
#52869 = CARTESIAN_POINT ( 'NONE',  ( -95.00000000000002842, 92.66308142843932671, 76.78406250086712248 ) ) ;
#52870 = EDGE_CURVE ( 'NONE', #27007, #44712, #55267, .T. ) ;
#52871 = CARTESIAN_POINT ( 'NONE',  ( 92.69370383062501162, -208.6684592857803011, 86.41489583420047893 ) ) ;
#52872 = ORIENTED_EDGE ( 'NONE', *, *, #40178, .T. ) ;
#52873 = ADVANCED_FACE ( 'NONE', ( #61655 ), #56007, .F. ) ;
#52874 = VERTEX_POINT ( 'NONE', #49609 ) ;
#52875 = VERTEX_POINT ( 'NONE', #10510 ) ;
#52876 = ADVANCED_FACE ( 'NONE', ( #27804 ), #50730, .T. ) ;
#52877 = VECTOR ( 'NONE', #65522, 1000.000000000000000 ) ;
#52879 = VECTOR ( 'NONE', #63402, 1000.000000000000000 ) ;
#52878 = LINE ( 'NONE', #29184, #33345 ) ;
#52880 = CARTESIAN_POINT ( 'NONE',  ( 10.00000000000000000, 35.38097989696512968, 12.42422080174651100 ) ) ;
#52881 = ORIENTED_EDGE ( 'NONE', *, *, #20303, .T. ) ;
#52882 = EDGE_LOOP ( 'NONE', ( #25221, #48, #57088, #44089 ) ) ;
#52883 = CARTESIAN_POINT ( 'NONE',  ( 92.69370383062501162, -208.6684592857803295, 83.39864583420049371 ) ) ;
#52884 = DIRECTION ( 'NONE',  ( 0.000000000000000000, 0.000000000000000000, 1.000000000000000000 ) ) ;
#52885 = CARTESIAN_POINT ( 'NONE',  ( 100.0010000000000190, -123.9999999999999858, -40.00000000000002132 ) ) ;
#52886 = CARTESIAN_POINT ( 'NONE',  ( 97.64999999999999147, 90.00000000000002842, 82.69749999999999091 ) ) ;
#52887 = CARTESIAN_POINT ( 'NONE',  ( 0.000000000000000000, 0.6853352020790449695, 37.58145647212454321 ) ) ;
#52888 = ADVANCED_FACE ( 'NONE', ( #10897 ), #15404, .T. ) ;
#52889 = DIRECTION ( 'NONE',  ( -1.000000000000000000, 0.000000000000000000, 0.000000000000000000 ) ) ;
#52890 = CARTESIAN_POINT ( 'NONE',  ( 95.00000000000000000, -206.9400435732949575, 85.39624999999998067 ) ) ;
#52891 = VECTOR ( 'NONE', #10203, 1000.000000000000000 ) ;
#52892 = VERTEX_POINT ( 'NONE', #12359 ) ;
#52893 = ORIENTED_EDGE ( 'NONE', *, *, #5792, .T. ) ;
#52894 = EDGE_LOOP ( 'NONE', ( #2634, #68350, #36402, #4557 ) ) ;
#52895 = ORIENTED_EDGE ( 'NONE', *, *, #5820, .F. ) ;
#52896 = CARTESIAN_POINT ( 'NONE',  ( -12.49999999999999645, 0.000000000000000000, 125.0000000000000000 ) ) ;
#52897 = AXIS2_PLACEMENT_3D ( 'NONE', #54938, #63195, #436 ) ;
#52898 = VECTOR ( 'NONE', #66513, 1000.000000000000000 ) ;
#52899 = CARTESIAN_POINT ( 'NONE',  ( -97.30629616937501680, 91.33154071421968467, 87.84364583420048689 ) ) ;
#52900 = DIRECTION ( 'NONE',  ( -1.000000000000000000, 0.000000000000000000, 0.000000000000000000 ) ) ;
#52901 = CIRCLE ( 'NONE', #57745, 32.00000000000000000 ) ;
#52902 = DIRECTION ( 'NONE',  ( 0.000000000000000000, 0.8910065241883691201, -0.4539904997395446951 ) ) ;
#52903 = CARTESIAN_POINT ( 'NONE',  ( 97.30629616937498838, -208.6684592857803011, 88.74322916753379786 ) ) ;
#52904 = CARTESIAN_POINT ( 'NONE',  ( 96.32499999999997442, 92.29496732002878900, 78.35833333333333428 ) ) ;
#52905 = ORIENTED_EDGE ( 'NONE', *, *, #73163, .F. ) ;
#52906 = FACE_OUTER_BOUND ( 'NONE', #26883, .T. ) ;
#52907 = ORIENTED_EDGE ( 'NONE', *, *, #54428, .T. ) ;
#52908 = EDGE_CURVE ( 'NONE', #48244, #54357, #5643, .T. ) ;
#52909 = CARTESIAN_POINT ( 'NONE',  ( 93.67500000000001137, -212.2949673200287179, 79.94583333333332575 ) ) ;
#52910 = EDGE_CURVE ( 'NONE', #28632, #21312, #57868, .T. ) ;
#52911 = ORIENTED_EDGE ( 'NONE', *, *, #11159, .T. ) ;
#52912 = CARTESIAN_POINT ( 'NONE',  ( -96.32500000000001705, 87.70503267997129626, 87.01020833506763097 ) ) ;
#52913 = CARTESIAN_POINT ( 'NONE',  ( 97.30629616937498838, 90.00000000000002842, 89.48406250086715374 ) ) ;
#52914 = VERTEX_POINT ( 'NONE', #29638 ) ;
#52915 = CARTESIAN_POINT ( 'NONE',  ( 10.00000000000000000, -33.79645857604525361, 16.45098606841114730 ) ) ;
#52916 = CARTESIAN_POINT ( 'NONE',  ( -2.500000000000020428, -90.00000000000000000, -90.00000000000000000 ) ) ;
#52917 = DIRECTION ( 'NONE',  ( 1.000000000000000000, 0.000000000000000000, 0.000000000000000000 ) ) ;
#52918 = CARTESIAN_POINT ( 'NONE',  ( 0.000000000000000000, -62.20884554313985149, -46.21855187248698371 ) ) ;
#52919 = ORIENTED_EDGE ( 'NONE', *, *, #41692, .T. ) ;
#52920 = CARTESIAN_POINT ( 'NONE',  ( -92.35000000000003695, 90.00000000000004263, 89.04749999999999943 ) ) ;
#52921 = CARTESIAN_POINT ( 'NONE',  ( -97.30629616937497417, -208.6684592857803011, 75.61989583420047722 ) ) ;
#52922 = EDGE_LOOP ( 'NONE', ( #4481, #58336, #12376, #9887 ) ) ;
#52923 = ORIENTED_EDGE ( 'NONE', *, *, #20727, .T. ) ;
#52924 = CYLINDRICAL_SURFACE ( 'NONE', #38569, 31.99999999999998579 ) ;
#52925 = DIRECTION ( 'NONE',  ( -0.000000000000000000, -0.000000000000000000, -1.000000000000000000 ) ) ;
#52926 = CYLINDRICAL_SURFACE ( 'NONE', #68969, 0.9999999999999991118 ) ;
#52927 = ORIENTED_EDGE ( 'NONE', *, *, #12080, .T. ) ;
#52928 = CARTESIAN_POINT ( 'NONE',  ( -92.69370383062498320, -208.6684592857803011, 87.63197916753382799 ) ) ;
#52929 = EDGE_LOOP ( 'NONE', ( #53816, #30966, #52324, #56738 ) ) ;
#52930 = CARTESIAN_POINT ( 'NONE',  ( 0.000000000000000000, -77.16300072079681627, 27.74655509720641433 ) ) ;
#52931 = ORIENTED_EDGE ( 'NONE', *, *, #60584, .T. ) ;
#52932 = ORIENTED_EDGE ( 'NONE', *, *, #70592, .T. ) ;
#52933 = VECTOR ( 'NONE', #64143, 1000.000000000000000 ) ;
#52934 = AXIS2_PLACEMENT_3D ( 'NONE', #56997, #5501, #28398 ) ;
#52935 = CARTESIAN_POINT ( 'NONE',  ( -97.65000000000001990, 91.52997821335253548, 83.67645833506763609 ) ) ;
#52936 = AXIS2_PLACEMENT_3D ( 'NONE', #36651, #60712, #9191 ) ;
#52937 = CYLINDRICAL_SURFACE ( 'NONE', #69345, 16.00000000000000000 ) ;
#52938 = CARTESIAN_POINT ( 'NONE',  ( 96.15314808468748708, 88.00268892867053694, 82.23447916753380582 ) ) ;
#52939 = DIRECTION ( 'NONE',  ( 0.000000000000000000, 0.000000000000000000, 1.000000000000000000 ) ) ;
#52940 = LINE ( 'NONE', #1481, #63844 ) ;
#52941 = DIRECTION ( 'NONE',  ( -1.000000000000000000, 0.000000000000000000, 0.000000000000000000 ) ) ;
#52942 = CYLINDRICAL_SURFACE ( 'NONE', #7597, 31.99999999999999289 ) ;
#52943 = DIRECTION ( 'NONE',  ( 1.000000000000000000, 0.000000000000000000, 0.000000000000000000 ) ) ;
#52944 = DIRECTION ( 'NONE',  ( 0.000000000000000000, -0.9876883405951394357, 0.1564344650402205716 ) ) ;
#52945 = DIRECTION ( 'NONE',  ( -1.000000000000000000, -0.000000000000000000, -0.000000000000000000 ) ) ;
#52946 = ADVANCED_FACE ( 'NONE', ( #6728 ), #68788, .T. ) ;
#52947 = DIRECTION ( 'NONE',  ( 1.000000000000000000, 1.427937372958405461E-15, 7.962523111839130290E-16 ) ) ;
#52948 = EDGE_CURVE ( 'NONE', #17753, #68977, #42630, .T. ) ;
#52949 =( GEOMETRIC_REPRESENTATION_CONTEXT ( 3 ) GLOBAL_UNCERTAINTY_ASSIGNED_CONTEXT ( ( #39866 ) ) GLOBAL_UNIT_ASSIGNED_CONTEXT ( ( #7166, #59044, #47745 ) ) REPRESENTATION_CONTEXT ( 'NONE', 'WORKASPACE' ) );
#52950 = DIRECTION ( 'NONE',  ( 0.000000000000000000, 0.000000000000000000, 1.000000000000000000 ) ) ;
#52951 = CARTESIAN_POINT ( 'NONE',  ( -97.30629616937501680, 91.33154071421968467, 87.04989583420046984 ) ) ;
#52952 = AXIS2_PLACEMENT_3D ( 'NONE', #55041, #3570, #42302 ) ;
#52953 = CARTESIAN_POINT ( 'NONE',  ( 5.000000000000000000, 39.04073710021366139, -15.48615015657542138 ) ) ;
#52954 = ADVANCED_FACE ( 'NONE', ( #23290 ), #28917, .F. ) ;
#52955 = CIRCLE ( 'NONE', #45739, 77.49900000000000944 ) ;
#52956 = EDGE_CURVE ( 'NONE', #8743, #31993, #72604, .T. ) ;
#52957 = CARTESIAN_POINT ( 'NONE',  ( 3.000000000000000000, -1.467624384280032501, -2.541999999999998039 ) ) ;
#52958 = EDGE_LOOP ( 'NONE', ( #39948, #70640, #4467, #21728 ) ) ;
#52959 =( BOUNDED_CURVE ( )  B_SPLINE_CURVE ( 2, ( #19624, #42570, #8358, #31278, #39150, #54951, #15465 ),
 .UNSPECIFIED., .F., .F. ) 
 B_SPLINE_CURVE_WITH_KNOTS ( ( 3, 2, 2, 3 ),
 ( 0.1874999999999999167, 0.1944444444444443365, 0.2013888888888887285, 0.2083333333333331483 ),
 .UNSPECIFIED. ) 
 CURVE ( )  GEOMETRIC_REPRESENTATION_ITEM ( )  RATIONAL_B_SPLINE_CURVE ( ( 1.000000000000001554, 0.8660254037844371533, 1.000000000000000000, 0.8660254037844387076, 1.000000000000000000, 0.8660254037844424824, 0.9999999999999962252 ) ) 
 REPRESENTATION_ITEM ( '' )  );
#52960 = DIRECTION ( 'NONE',  ( -1.000000000000000000, -0.000000000000000000, 0.000000000000000000 ) ) ;
#52961 = CARTESIAN_POINT ( 'NONE',  ( 10.00000000000000000, -11.30684508768284680, -76.66974797899850103 ) ) ;
#52962 = DIRECTION ( 'NONE',  ( 0.000000000000000000, 0.000000000000000000, 1.000000000000000000 ) ) ;
#52963 = EDGE_CURVE ( 'NONE', #43951, #9784, #29408, .T. ) ;
#52964 = CARTESIAN_POINT ( 'NONE',  ( 10.00000000000000000, -15.48615015657610883, 39.04073710021339139 ) ) ;
#52965 = CARTESIAN_POINT ( 'NONE',  ( 93.84685191531249870, -208.0026889286704943, 83.34572916753383254 ) ) ;
#52966 = ORIENTED_EDGE ( 'NONE', *, *, #3921, .T. ) ;
#52967 = ORIENTED_EDGE ( 'NONE', *, *, #14373, .T. ) ;
#52968 = CYLINDRICAL_SURFACE ( 'NONE', #5646, 12.74999999999999822 ) ;
#52969 = VERTEX_POINT ( 'NONE', #5273 ) ;
#52970 = ADVANCED_FACE ( 'NONE', ( #74036 ), #52215, .F. ) ;
#52971 = CARTESIAN_POINT ( 'NONE',  ( 92.34999999999993747, -208.4700217866474929, 88.67708333333332860 ) ) ;
#52972 = CARTESIAN_POINT ( 'NONE',  ( 96.15314808468748708, -208.0026889286704943, 74.82614583420047438 ) ) ;
#52974 = ORIENTED_EDGE ( 'NONE', *, *, #57960, .T. ) ;
#52973 = EDGE_CURVE ( 'NONE', #37710, #31522, #69047, .T. ) ;
#52975 = CARTESIAN_POINT ( 'NONE',  ( 92.69370383062501162, -209.9999999999999716, 78.37156250086715659 ) ) ;
#52976 = PRESENTATION_LAYER_ASSIGNMENT (  '', '', ( #54171 ) ) ;
#52977 = AXIS2_PLACEMENT_3D ( 'NONE', #24261, #41541, #63749 ) ;
#52978 = ORIENTED_EDGE ( 'NONE', *, *, #20356, .F. ) ;
#52979 = LINE ( 'NONE', #43195, #37138 ) ;
#52980 = ORIENTED_EDGE ( 'NONE', *, *, #12496, .T. ) ;
#52981 = AXIS2_PLACEMENT_3D ( 'NONE', #56748, #40188, #12339 ) ;
#52982 = EDGE_CURVE ( 'NONE', #44827, #49630, #33008, .T. ) ;
#52983 = ORIENTED_EDGE ( 'NONE', *, *, #55762, .F. ) ;
#52984 = LINE ( 'NONE', #34573, #5720 ) ;
#52985 = CIRCLE ( 'NONE', #26726, 77.49900000000002365 ) ;
#52986 = FILL_AREA_STYLE_COLOUR ( '', #38710 ) ;
#52987 = LINE ( 'NONE', #69535, #72503 ) ;
#52988 = ORIENTED_EDGE ( 'NONE', *, *, #39813, .F. ) ;
#52989 = DIRECTION ( 'NONE',  ( -1.000000000000000000, 0.000000000000000000, 0.000000000000000000 ) ) ;
#52990 = CARTESIAN_POINT ( 'NONE',  ( 93.67500000000001137, -207.7050326799711968, 84.89354166840095672 ) ) ;
#52991 = CARTESIAN_POINT ( 'NONE',  ( 92.34999999999999432, 91.52997821335252127, 88.04208333333332348 ) ) ;
#52992 = ORIENTED_EDGE ( 'NONE', *, *, #36221, .F. ) ;
#52993 = CYLINDRICAL_SURFACE ( 'NONE', #21487, 82.00000000000000000 ) ;
#52994 = AXIS2_PLACEMENT_3D ( 'NONE', #8536, #60053, #71291 ) ;
#52995 = EDGE_CURVE ( 'NONE', #69189, #35387, #57792, .T. ) ;
#52996 = CARTESIAN_POINT ( 'NONE',  ( 0.000000000000000000, 0.000000000000000000, 53.20000000000001705 ) ) ;
#52997 = ORIENTED_EDGE ( 'NONE', *, *, #59072, .F. ) ;
#52998 = ORIENTED_EDGE ( 'NONE', *, *, #26287, .T. ) ;
#52999 = CARTESIAN_POINT ( 'NONE',  ( 5.000000000000000000, -0.5603747650654238299, -0.5678343202077608121 ) ) ;
#53000 = EDGE_LOOP ( 'NONE', ( #20420, #9155, #35688, #9216 ) ) ;
#53001 = CARTESIAN_POINT ( 'NONE',  ( 94.99999999999998579, 93.05995642670504253, 87.38062500173430180 ) ) ;
#53002 = EDGE_CURVE ( 'NONE', #63923, #68344, #652, .T. ) ;
#53003 = EDGE_LOOP ( 'NONE', ( #63818, #8045, #2363, #53569 ) ) ;
#53004 = FILL_AREA_STYLE ('',( #58267 ) ) ;
#53005 = ORIENTED_EDGE ( 'NONE', *, *, #62075, .T. ) ;
#53006 = CARTESIAN_POINT ( 'NONE',  ( 10.00000000000000000, -0.6853352020793173072, 37.58145647212453611 ) ) ;
#53007 = VECTOR ( 'NONE', #58376, 1000.000000000000000 ) ;
#53008 = CARTESIAN_POINT ( 'NONE',  ( -92.34999999999999432, -209.9999999999999716, 75.07749999999998636 ) ) ;
#53009 = VERTEX_POINT ( 'NONE', #51477 ) ;
#53010 = AXIS2_PLACEMENT_3D ( 'NONE', #23988, #69114, #40911 ) ;
#53011 = VERTEX_POINT ( 'NONE', #62796 ) ;
#53012 = VERTEX_POINT ( 'NONE', #16911 ) ;
#53013 = DIRECTION ( 'NONE',  ( 7.571541139946887334E-15, -1.000000000000000000, -2.546204323184473159E-14 ) ) ;
#53014 = CARTESIAN_POINT ( 'NONE',  ( -21.33958957442910886, -129.9559990355020034, 5.500000000000000000 ) ) ;
#53015 = CARTESIAN_POINT ( 'NONE',  ( -97.65000000000001990, 88.47002178664754979, 86.24291666666665890 ) ) ;
#53016 = ORIENTED_EDGE ( 'NONE', *, *, #35414, .F. ) ;
#53017 = DIRECTION ( 'NONE',  ( -1.000000000000000000, 0.000000000000000000, 0.000000000000000000 ) ) ;
#53018 = CIRCLE ( 'NONE', #47008, 12.49999999999999645 ) ;
#53019 = DIRECTION ( 'NONE',  ( -1.000000000000000000, 0.000000000000000000, 0.000000000000000000 ) ) ;
#53020 = ORIENTED_EDGE ( 'NONE', *, *, #71887, .F. ) ;
#53021 = FACE_OUTER_BOUND ( 'NONE', #26652, .T. ) ;
#53022 = CARTESIAN_POINT ( 'NONE',  ( -94.99999999999997158, -207.3369185715606307, 83.76906250086713612 ) ) ;
#53023 = ORIENTED_EDGE ( 'NONE', *, *, #60886, .T. ) ;
#53024 = DIRECTION ( 'NONE',  ( -1.000000000000000000, -0.000000000000000000, 0.000000000000000000 ) ) ;
#53025 = DIRECTION ( 'NONE',  ( -1.000000000000000000, -0.000000000000000000, -0.000000000000000000 ) ) ;
#53026 = CARTESIAN_POINT ( 'NONE',  ( -23.97194136764370498, -131.3950000906648938, -5.500000000000000000 ) ) ;
#53027 = PLANE ( 'NONE',  #59061 ) ;
#53028 = DIRECTION ( 'NONE',  ( -0.000000000000000000, -0.3090169943749573878, 0.9510565162951503115 ) ) ;
#53029 = CARTESIAN_POINT ( 'NONE',  ( 0.000000000000000000, 0.000000000000000000, 0.000000000000000000 ) ) ;
#53030 = LINE ( 'NONE', #58662, #6054 ) ;
#53031 = CARTESIAN_POINT ( 'NONE',  ( 7.400000000000003908, 1.056673655987569448E-14, 5.892267102770835596E-15 ) ) ;
#53032 = CARTESIAN_POINT ( 'NONE',  ( 97.64999999999999147, 90.00000000000002842, 82.77687500173431090 ) ) ;
#53033 = LINE ( 'NONE', #13538, #18743 ) ;
#53034 = CARTESIAN_POINT ( 'NONE',  ( -97.30629616937501680, 90.00000000000004263, 78.21281250086714465 ) ) ;
#53035 = DIRECTION ( 'NONE',  ( 1.000000000000000000, 0.000000000000000000, 0.000000000000000000 ) ) ;
#53036 = CARTESIAN_POINT ( 'NONE',  ( 96.32499999999998863, 87.70503267997126784, 76.24166666666666003 ) ) ;
#53037 = DIRECTION ( 'NONE',  ( 0.000000000000000000, 0.000000000000000000, -1.000000000000000000 ) ) ;
#53038 = CIRCLE ( 'NONE', #61411, 21.00000000000000000 ) ;
#53039 = EDGE_CURVE ( 'NONE', #1337, #19859, #70198, .T. ) ;
#53040 = FACE_OUTER_BOUND ( 'NONE', #63804, .T. ) ;
#53041 = CARTESIAN_POINT ( 'NONE',  ( 0.000000000000000000, 29.01471420065564644, 76.69515212746026123 ) ) ;
#53042 = LINE ( 'NONE', #20298, #2313 ) ;
#53043 = EDGE_CURVE ( 'NONE', #21151, #61705, #61804, .T. ) ;
#53044 = CARTESIAN_POINT ( 'NONE',  ( 0.000000000000000000, 0.000000000000000000, 0.000000000000000000 ) ) ;
#53045 = LINE ( 'NONE', #35731, #6427 ) ;
#53046 = CARTESIAN_POINT ( 'NONE',  ( -92.69370383062498320, -209.9999999999999716, 76.78406250086715090 ) ) ;
#53047 = ADVANCED_FACE ( 'NONE', ( #62278 ), #67913, .T. ) ;
#53048 = EDGE_CURVE ( 'NONE', #32074, #44409, #56052, .T. ) ;
#53049 = VECTOR ( 'NONE', #26466, 1000.000000000000000 ) ;
#53050 = DIRECTION ( 'NONE',  ( 0.000000000000000000, 0.000000000000000000, 1.000000000000000000 ) ) ;
#53051 = AXIS2_PLACEMENT_3D ( 'NONE', #1358, #35147, #52424 ) ;
#53052 = ORIENTED_EDGE ( 'NONE', *, *, #27655, .T. ) ;
#53053 = DIRECTION ( 'NONE',  ( 0.000000000000000000, 0.000000000000000000, 1.000000000000000000 ) ) ;
#53054 = CARTESIAN_POINT ( 'NONE',  ( 11.99999999999999822, -29.01471420065616513, 76.69515212746006227 ) ) ;
#53055 = LINE ( 'NONE', #1591, #71321 ) ;
#53056 = CIRCLE ( 'NONE', #62695, 31.99999999999998224 ) ;
#53057 = CIRCLE ( 'NONE', #71015, 62.50000000000000000 ) ;
#53058 = AXIS2_PLACEMENT_3D ( 'NONE', #21595, #44550, #67469 ) ;
#53059 = CARTESIAN_POINT ( 'NONE',  ( 96.32499999999998863, 87.70503267997126784, 83.30604166840096525 ) ) ;
#53060 = EDGE_CURVE ( 'NONE', #34583, #17670, #48593, .T. ) ;
#53061 = EDGE_LOOP ( 'NONE', ( #28021, #8638 ) ) ;
#53062 = CARTESIAN_POINT ( 'NONE',  ( -92.35000000000003695, 90.00000000000004263, 90.00000000000000000 ) ) ;
#53063 = CYLINDRICAL_SURFACE ( 'NONE', #47539, 31.99999999999998579 ) ;
#53064 = VERTEX_POINT ( 'NONE', #72423 ) ;
#53065 = CARTESIAN_POINT ( 'NONE',  ( 95.00000000000000000, -207.3369185715606307, 84.40406250086714124 ) ) ;
#53066 = CARTESIAN_POINT ( 'NONE',  ( 93.84685191531251292, -211.9973110713294489, 88.00239583420048461 ) ) ;
#53067 = VERTEX_POINT ( 'NONE', #50986 ) ;
#53068 = DIRECTION ( 'NONE',  ( -1.000000000000000000, 0.000000000000000000, 0.000000000000000000 ) ) ;
#53069 = ORIENTED_EDGE ( 'NONE', *, *, #30696, .T. ) ;
#53070 = DIRECTION ( 'NONE',  ( -1.000000000000000000, 0.000000000000000000, 0.000000000000000000 ) ) ;
#53071 = EDGE_LOOP ( 'NONE', ( #13315, #16532, #28692, #20529 ) ) ;
#53072 = ADVANCED_FACE ( 'NONE', ( #28418 ), #4035, .T. ) ;
#53073 = EDGE_CURVE ( 'NONE', #32793, #38655, #3001, .T. ) ;
#53074 = CARTESIAN_POINT ( 'NONE',  ( -95.00000000000002842, 92.66308142843932671, 80.11781250086714579 ) ) ;
#53075 = VERTEX_POINT ( 'NONE', #56645 ) ;
#53076 = VERTEX_POINT ( 'NONE', #32569 ) ;
#53077 = LINE ( 'NONE', #65106, #64113 ) ;
#53078 = ORIENTED_EDGE ( 'NONE', *, *, #72236, .F. ) ;
#53079 = DIRECTION ( 'NONE',  ( -1.000000000000000000, 0.000000000000000000, -0.000000000000000000 ) ) ;
#53080 = ORIENTED_EDGE ( 'NONE', *, *, #53945, .F. ) ;
#53081 = CARTESIAN_POINT ( 'NONE',  ( 0.000000000000000000, -55.20638768913797634, 51.02545421589302777 ) ) ;
#53082 = VERTEX_POINT ( 'NONE', #22044 ) ;
#53083 = FACE_OUTER_BOUND ( 'NONE', #59352, .T. ) ;
#53084 = VERTEX_POINT ( 'NONE', #73909 ) ;
#53085 = CIRCLE ( 'NONE', #62719, 37.49900000000001654 ) ;
#53086 = ORIENTED_EDGE ( 'NONE', *, *, #50319, .T. ) ;
#53087 = ORIENTED_EDGE ( 'NONE', *, *, #5057, .F. ) ;
#53088 = CARTESIAN_POINT ( 'NONE',  ( 97.30629616937498838, -209.9999999999999716, 82.97531250086714749 ) ) ;
#53089 = DIRECTION ( 'NONE',  ( -1.000000000000000000, -0.000000000000000000, 0.000000000000000000 ) ) ;
#53090 = APPLICATION_PROTOCOL_DEFINITION ( 'draft international standard', 'automotive_design', 1998, #15240 ) ;
#53091 = DIRECTION ( 'NONE',  ( 0.000000000000000000, 0.000000000000000000, 1.000000000000000000 ) ) ;
#53093 = CYLINDRICAL_SURFACE ( 'NONE', #46100, 16.00000000000000000 ) ;
#53092 = AXIS2_PLACEMENT_3D ( 'NONE', #28156, #69140, #40553 ) ;
#53094 = FACE_OUTER_BOUND ( 'NONE', #50089, .T. ) ;
#53095 = CARTESIAN_POINT ( 'NONE',  ( -93.67499999999998295, -212.2949673200287179, 75.60666666666665492 ) ) ;
#53096 = CARTESIAN_POINT ( 'NONE',  ( -97.64999999954989107, -210.0000310946949753, 88.81037122969127040 ) ) ;
#53097 = CYLINDRICAL_SURFACE ( 'NONE', #49102, 37.49900000000000233 ) ;
#53098 = CARTESIAN_POINT ( 'NONE',  ( -94.99999999999997158, -207.3369185715606307, 83.13406250086714522 ) ) ;
#53099 = CARTESIAN_POINT ( 'NONE',  ( -95.00000000000002842, 87.33691857156074434, 82.97531250086716170 ) ) ;
#53100 = CIRCLE ( 'NONE', #61532, 31.99999999999998579 ) ;
#53101 = ORIENTED_EDGE ( 'NONE', *, *, #47763, .F. ) ;
#53102 = CARTESIAN_POINT ( 'NONE',  ( 92.69370383062498320, 88.66845928578037217, 81.44072916753381719 ) ) ;
#53103 = AXIS2_PLACEMENT_3D ( 'NONE', #25453, #13786, #19799 ) ;
#53104 = VERTEX_POINT ( 'NONE', #44987 ) ;
#53105 = CARTESIAN_POINT ( 'NONE',  ( -2.500000000000011990, -62.44997998398397954, -189.9999999999999147 ) ) ;
#53106 = FACE_OUTER_BOUND ( 'NONE', #28112, .T. ) ;
#53107 = DIRECTION ( 'NONE',  ( -1.000000000000000000, -0.000000000000000000, -0.000000000000000000 ) ) ;
#53108 = CARTESIAN_POINT ( 'NONE',  ( 23.11608002360578240, -124.4885236261218182, -5.500000000000000000 ) ) ;
#53109 = DIRECTION ( 'NONE',  ( 1.000000000000000000, 0.000000000000000000, 0.000000000000000000 ) ) ;
#53110 = CARTESIAN_POINT ( 'NONE',  ( -92.69370383062498320, -211.3315407142195852, 84.82739583420048746 ) ) ;
#53111 = CARTESIAN_POINT ( 'NONE',  ( 10.00000000000000000, 27.75498641678742473, 31.52238457039609898 ) ) ;
#53112 = CARTESIAN_POINT ( 'NONE',  ( -96.32499999999996021, -212.2949673200287179, 89.47083333333333144 ) ) ;
#53113 = CARTESIAN_POINT ( 'NONE',  ( -17.26469406256017791, -140.1601175325492648, 5.500000000000000000 ) ) ;
#53114 = VECTOR ( 'NONE', #25788, 1000.000000000000000 ) ;
#53115 = CARTESIAN_POINT ( 'NONE',  ( 96.32499999999997442, 92.29496732002878900, 80.26333333333332121 ) ) ;
#53116 = ORIENTED_EDGE ( 'NONE', *, *, #73234, .T. ) ;
#53117 = CIRCLE ( 'NONE', #14672, 15.99999999999999822 ) ;
#53118 = ORIENTED_EDGE ( 'NONE', *, *, #43828, .T. ) ;
#53119 = DIRECTION ( 'NONE',  ( -1.000000000000000000, -0.000000000000000000, -0.000000000000000000 ) ) ;
#53120 = FACE_OUTER_BOUND ( 'NONE', #7567, .T. ) ;
#53121 = CARTESIAN_POINT ( 'NONE',  ( -97.30629616937501680, 88.66845928578038638, 89.06072916753379332 ) ) ;
#53122 = DIRECTION ( 'NONE',  ( 0.000000000000000000, 0.000000000000000000, 1.000000000000000000 ) ) ;
#53123 = LINE ( 'NONE', #17788, #15792 ) ;
#53124 = DIRECTION ( 'NONE',  ( 1.000000000000000000, -0.000000000000000000, -0.000000000000000000 ) ) ;
#53125 = CARTESIAN_POINT ( 'NONE',  ( 0.000000000000000000, 0.000000000000000000, 0.000000000000000000 ) ) ;
#53126 = ORIENTED_EDGE ( 'NONE', *, *, #45099, .T. ) ;
#53127 = CARTESIAN_POINT ( 'NONE',  ( -93.84685191531252713, 88.00268892867056536, 75.88447916753381151 ) ) ;
#53128 = EDGE_CURVE ( 'NONE', #14021, #11081, #16030, .T. ) ;
#53129 = FACE_OUTER_BOUND ( 'NONE', #66062, .T. ) ;
#53130 = DIRECTION ( 'NONE',  ( 0.000000000000000000, -0.7071067811865389130, -0.7071067811865561215 ) ) ;
#53131 = EDGE_CURVE ( 'NONE', #24073, #18738, #44238, .T. ) ;
#53132 = CARTESIAN_POINT ( 'NONE',  ( 15.00000000000000000, 22.07842321921492612, 8.187992925817123790 ) ) ;
#53133 = LINE ( 'NONE', #68954, #70104 ) ;
#53134 = CARTESIAN_POINT ( 'NONE',  ( -93.84685191531248449, -208.0026889286704943, 87.04989583420048405 ) ) ;
#53135 = EDGE_CURVE ( 'NONE', #29022, #70651, #59766, .T. ) ;
#53136 = DIRECTION ( 'NONE',  ( -2.628368902995175337E-16, -1.000000000000000000, 0.000000000000000000 ) ) ;
#53137 = EDGE_CURVE ( 'NONE', #21499, #64024, #21669, .T. ) ;
#53138 = CARTESIAN_POINT ( 'NONE',  ( 96.15314808468748708, 91.99731107132950569, 74.98489583420048632 ) ) ;
#53139 = CARTESIAN_POINT ( 'NONE',  ( -93.33920801875063944, -211.6002412367801071, 74.80065669543250806 ) ) ;
#53140 = CARTESIAN_POINT ( 'NONE',  ( 10.00000000000000000, 0.000000000000000000, 0.000000000000000000 ) ) ;
#53141 = VERTEX_POINT ( 'NONE', #68288 ) ;
#53142 = MECHANICAL_DESIGN_GEOMETRIC_PRESENTATION_REPRESENTATION (  '', ( #1561 ), #46018 ) ;
#53143 = CARTESIAN_POINT ( 'NONE',  ( 10.00000000000000000, -22.74946021919110706, -29.81001611431033282 ) ) ;
#53144 = DIRECTION ( 'NONE',  ( -1.000000000000000000, -0.000000000000000000, -0.000000000000000000 ) ) ;
#53145 = CARTESIAN_POINT ( 'NONE',  ( -96.32500000000001705, 87.70503267997129626, 88.28020833506764120 ) ) ;
#53146 = ADVANCED_FACE ( 'NONE', ( #72779 ), #49862, .F. ) ;
#53147 = AXIS2_PLACEMENT_3D ( 'NONE', #28363, #33253, #40773 ) ;
#53148 = CARTESIAN_POINT ( 'NONE',  ( -97.30629616937501680, 90.00000000000004263, 75.83156250086716454 ) ) ;
#53150 = ADVANCED_FACE ( 'NONE', ( #34065 ), #5515, .T. ) ;
#53149 = CARTESIAN_POINT ( 'NONE',  ( 93.84685191531251292, -211.9973110713294489, 77.68364583420047609 ) ) ;
#53151 = EDGE_LOOP ( 'NONE', ( #19663, #54577, #61009, #62985, #65752, #10057, #29827, #47231 ) ) ;
#53152 = AXIS2_PLACEMENT_3D ( 'NONE', #66884, #15004, #60882 ) ;
#53153 = EDGE_CURVE ( 'NONE', #4121, #6916, #38218, .T. ) ;
#53154 = DIRECTION ( 'NONE',  ( -1.000000000000000000, 0.000000000000000000, 0.000000000000000000 ) ) ;
#53155 = CARTESIAN_POINT ( 'NONE',  ( 10.00000000000000000, -33.17418723428319538, 17.67226234102814431 ) ) ;
#53156 = EDGE_LOOP ( 'NONE', ( #52445, #59658, #60397, #1381 ) ) ;
#53157 = LINE ( 'NONE', #24580, #65177 ) ;
#53158 = EDGE_LOOP ( 'NONE', ( #40473, #23130, #69422, #13765 ) ) ;
#53159 = AXIS2_PLACEMENT_3D ( 'NONE', #17430, #30448, #34719 ) ;
#53160 = DIRECTION ( 'NONE',  ( 0.000000000000000000, -0.4539904997395352027, -0.8910065241883737830 ) ) ;
#53161 = EDGE_CURVE ( 'NONE', #42454, #27599, #38599, .T. ) ;
#53163 = EDGE_CURVE ( 'NONE', #30036, #68106, #47464, .T. ) ;
#53162 = AXIS2_PLACEMENT_3D ( 'NONE', #34249, #57194, #63951 ) ;
#53164 = ORIENTED_EDGE ( 'NONE', *, *, #34535, .T. ) ;
#53165 = ORIENTED_EDGE ( 'NONE', *, *, #41126, .T. ) ;
#53166 = ORIENTED_EDGE ( 'NONE', *, *, #63704, .F. ) ;
#53167 = DIRECTION ( 'NONE',  ( 1.000000000000000000, 1.427937372958405461E-15, 7.962523111839130290E-16 ) ) ;
#53168 = ORIENTED_EDGE ( 'NONE', *, *, #33153, .T. ) ;
#53169 = EDGE_LOOP ( 'NONE', ( #7939, #45963, #1250, #8605, #38460, #51143 ) ) ;
#53170 = CARTESIAN_POINT ( 'NONE',  ( 93.84685191531248449, 88.00268892867053694, 78.47739583420049314 ) ) ;
#53171 = FACE_OUTER_BOUND ( 'NONE', #47368, .T. ) ;
#53172 = CARTESIAN_POINT ( 'NONE',  ( 92.35000000000002274, -211.5299782133524502, 75.44791666666667140 ) ) ;
#53173 = EDGE_LOOP ( 'NONE', ( #42992, #74158, #13571, #35210 ) ) ;
#53174 = VERTEX_POINT ( 'NONE', #51350 ) ;
#53175 = EDGE_LOOP ( 'NONE', ( #43305, #20905, #12471, #28957 ) ) ;
#53176 = DIRECTION ( 'NONE',  ( 0.000000000000000000, 0.000000000000000000, 1.000000000000000000 ) ) ;
#53177 = VERTEX_POINT ( 'NONE', #18251 ) ;
#53178 = DIRECTION ( 'NONE',  ( -0.7533909544171997208, -0.6575728627325955200, 0.000000000000000000 ) ) ;
#53179 = CARTESIAN_POINT ( 'NONE',  ( -97.65000000000000568, 88.47002178664756400, 87.51291666666666913 ) ) ;
#53180 = CARTESIAN_POINT ( 'NONE',  ( -95.43397055421762332, 92.35870626171013953, 74.84690984288799598 ) ) ;
#53181 = FACE_OUTER_BOUND ( 'NONE', #68741, .T. ) ;
#53182 = CARTESIAN_POINT ( 'NONE',  ( 0.000000000000000000, 5.256550761632864166, 77.32052557432842832 ) ) ;
#53183 = DIRECTION ( 'NONE',  ( 0.000000000000000000, -0.8910065241883627918, -0.4539904997395569630 ) ) ;
#53184 = CARTESIAN_POINT ( 'NONE',  ( 93.67499999999998295, 92.29496732002878900, 77.82916666666665151 ) ) ;
#53185 = CARTESIAN_POINT ( 'NONE',  ( -92.34999999999999432, -209.9999999999999716, 78.33187500173430351 ) ) ;
#53186 = PLANE ( 'NONE',  #56728 ) ;
#53187 = VERTEX_POINT ( 'NONE', #40445 ) ;
#53189 = CARTESIAN_POINT ( 'NONE',  ( -92.35000000000005116, 91.52997821335253548, 75.84479166840098685 ) ) ;
#53188 = CARTESIAN_POINT ( 'NONE',  ( 97.64999999999999147, 90.00000000000002842, 74.52187500173430124 ) ) ;
#53190 =( BOUNDED_CURVE ( )  B_SPLINE_CURVE ( 2, ( #33222, #70388, #18892, #11767, #58021, #29429, #41470, #922, #46013 ),
 .UNSPECIFIED., .F., .F. ) 
 B_SPLINE_CURVE_WITH_KNOTS ( ( 3, 2, 2, 2, 3 ),
 ( 0.7620226289464459013, 0.7620226784152965838, 0.7690784439561786368, 0.7761342094970606897, 0.7831899741065915244 ),
 .UNSPECIFIED. ) 
 CURVE ( )  GEOMETRIC_REPRESENTATION_ITEM ( )  RATIONAL_B_SPLINE_CURVE ( ( 0.9999981213880242414, 0.9999990606874264998, 1.000000000000000000, 0.8660254037844387076, 1.000000000000000000, 0.8660254037844387076, 1.000000000000000000, 0.8660254037844387076, 1.000000000000000000 ) ) 
 REPRESENTATION_ITEM ( '' )  );
#53191 = ORIENTED_EDGE ( 'NONE', *, *, #67931, .F. ) ;
#53192 = CARTESIAN_POINT ( 'NONE',  ( 97.30629616937498838, 88.66845928578037217, 80.54114583420049200 ) ) ;
#53193 = DIRECTION ( 'NONE',  ( 0.000000000000000000, 0.3090169943749442316, 0.9510565162951545304 ) ) ;
#53194 = LINE ( 'NONE', #28779, #70299 ) ;
#53195 = DIRECTION ( 'NONE',  ( 0.000000000000000000, -0.9510565162951565288, 0.3090169943749384029 ) ) ;
#53196 = CARTESIAN_POINT ( 'NONE',  ( 10.00000000000000000, -38.55633173626998911, -16.65560815589452304 ) ) ;
#53197 = DIRECTION ( 'NONE',  ( -1.000000000000000000, 0.000000000000000000, 0.000000000000000000 ) ) ;
#53198 = AXIS2_PLACEMENT_3D ( 'NONE', #8793, #48277, #43014 ) ;
#53199 = ORIENTED_EDGE ( 'NONE', *, *, #54267, .F. ) ;
#53200 = CARTESIAN_POINT ( 'NONE',  ( 10.00000000000000000, 0.000000000000000000, 0.000000000000000000 ) ) ;
#53201 = CARTESIAN_POINT ( 'NONE',  ( -1.653121499799246497, 4.819072548984005167, -5.948595712916174172 ) ) ;
#53202 = ORIENTED_EDGE ( 'NONE', *, *, #20818, .T. ) ;
#53203 = VERTEX_POINT ( 'NONE', #51732 ) ;
#53204 = EDGE_CURVE ( 'NONE', #47718, #38512, #64922, .T. ) ;
#53205 = ADVANCED_FACE ( 'NONE', ( #636 ), #1383, .F. ) ;
#53206 = CARTESIAN_POINT ( 'NONE',  ( 11.99999999999999822, -81.50828551894234408, 8.966570791700414489 ) ) ;
#53207 = CARTESIAN_POINT ( 'NONE',  ( 0.000000000000000000, -76.66974797899844418, 11.30684508768314522 ) ) ;
#53208 = EDGE_CURVE ( 'NONE', #17471, #48180, #69098, .T. ) ;
#53209 = DIRECTION ( 'NONE',  ( 0.000000000000000000, 0.000000000000000000, 1.000000000000000000 ) ) ;
#53210 = FACE_OUTER_BOUND ( 'NONE', #6367, .T. ) ;
#53211 = AXIS2_PLACEMENT_3D ( 'NONE', #56218, #9970, #32889 ) ;
#53212 = CARTESIAN_POINT ( 'NONE',  ( -92.69370383062498320, -211.3315407142195852, 78.00114583420049996 ) ) ;
#53213 = CIRCLE ( 'NONE', #56975, 82.00000000000000000 ) ;
#53214 = ORIENTED_EDGE ( 'NONE', *, *, #26743, .T. ) ;
#53215 = EDGE_CURVE ( 'NONE', #9807, #51953, #29516, .T. ) ;
#53216 = DIRECTION ( 'NONE',  ( -1.000000000000000000, 0.000000000000000000, -0.000000000000000000 ) ) ;
#53217 = CIRCLE ( 'NONE', #8774, 31.99999999999999289 ) ;
#53218 = AXIS2_PLACEMENT_3D ( 'NONE', #33043, #67273, #43249 ) ;
#53219 = CARTESIAN_POINT ( 'NONE',  ( -32.50000000000000000, -120.0000000000000000, -2.500000000000000000 ) ) ;
#53220 = FACE_OUTER_BOUND ( 'NONE', #67683, .T. ) ;
#53221 = EDGE_CURVE ( 'NONE', #47617, #68616, #41552, .T. ) ;
#53222 = CARTESIAN_POINT ( 'NONE',  ( 8.700667342345820288, -98.11853780484867116, 5.500000000000000000 ) ) ;
#53223 = CARTESIAN_POINT ( 'NONE',  ( 0.000000000000000000, 23.50000000000000000, -1.500000000000001332 ) ) ;
#53224 = DIRECTION ( 'NONE',  ( -1.000000000000000000, -0.000000000000000000, 0.000000000000000000 ) ) ;
#53225 = PLANE ( 'NONE',  #42151 ) ;
#53226 = CARTESIAN_POINT ( 'NONE',  ( 97.65000000000000568, 91.52997821335252127, 86.00479166840096923 ) ) ;
#53227 = DIRECTION ( 'NONE',  ( -1.000000000000000000, 0.000000000000000000, -0.000000000000000000 ) ) ;
#53228 = DIRECTION ( 'NONE',  ( -1.000000000000000000, -0.000000000000000000, 0.000000000000000000 ) ) ;
#53229 = ADVANCED_FACE ( 'NONE', ( #22804 ), #69385, .T. ) ;
#53230 = CARTESIAN_POINT ( 'NONE',  ( 97.30629616937498838, 88.66845928578035796, 82.44614583420049314 ) ) ;
#53231 = CARTESIAN_POINT ( 'NONE',  ( -92.69370383062498320, -209.9999999999999716, 85.67406250086715147 ) ) ;
#53232 = CARTESIAN_POINT ( 'NONE',  ( 97.64999999946594755, 90.00005320149050192, 78.96687695417308817 ) ) ;
#53233 = ORIENTED_EDGE ( 'NONE', *, *, #37035, .F. ) ;
#53234 = CARTESIAN_POINT ( 'NONE',  ( 12.50000000000000000, -132.5000000000000000, 2.500000000000000000 ) ) ;
#53235 = CARTESIAN_POINT ( 'NONE',  ( -92.34999999999999432, -208.4700217866474645, 82.11541666666666117 ) ) ;
#53236 = CARTESIAN_POINT ( 'NONE',  ( -95.00000000000002842, 92.66308142843932671, 77.41906250086714181 ) ) ;
#53238 = EDGE_CURVE ( 'NONE', #27772, #50461, #58242, .T. ) ;
#53237 = CARTESIAN_POINT ( 'NONE',  ( 92.69370383062501162, -209.9999999999999716, 87.10281250086714522 ) ) ;
#53239 = ORIENTED_EDGE ( 'NONE', *, *, #43886, .T. ) ;
#53240 = EDGE_CURVE ( 'NONE', #24576, #855, #17149, .T. ) ;
#53241 = APPLICATION_CONTEXT ( 'automotive_design' ) ;
#53242 = VECTOR ( 'NONE', #68305, 1000.000000000000000 ) ;
#53243 = ORIENTED_EDGE ( 'NONE', *, *, #9921, .F. ) ;
#53244 = ORIENTED_EDGE ( 'NONE', *, *, #10264, .T. ) ;
#53245 = CARTESIAN_POINT ( 'NONE',  ( 93.67500000000001137, -212.2949673200287179, 75.50083333333331836 ) ) ;
#53246 = FACE_OUTER_BOUND ( 'NONE', #54714, .T. ) ;
#53247 = VECTOR ( 'NONE', #55475, 1000.000000000000114 ) ;
#53248 = ORIENTED_EDGE ( 'NONE', *, *, #71466, .F. ) ;
#53249 = VERTEX_POINT ( 'NONE', #23168 ) ;
#53250 = DIRECTION ( 'NONE',  ( -0.000000000000000000, 1.000000000000000000, -0.000000000000000000 ) ) ;
#53251 = CARTESIAN_POINT ( 'NONE',  ( 92.69370383062501162, -209.9999999999999716, 82.18156250086715886 ) ) ;
#53252 = FACE_OUTER_BOUND ( 'NONE', #32429, .T. ) ;
#53253 = DIRECTION ( 'NONE',  ( -1.000000000000000000, 0.000000000000000000, 0.000000000000000000 ) ) ;
#53254 = PLANE ( 'NONE',  #34030 ) ;
#53255 = CARTESIAN_POINT ( 'NONE',  ( 0.000000000000000000, -11.30684508768284680, -76.66974797899850103 ) ) ;
#53256 = CIRCLE ( 'NONE', #1677, 5.000000000000000000 ) ;
#53257 = DIRECTION ( 'NONE',  ( -1.000000000000000000, 0.000000000000000000, -0.000000000000000000 ) ) ;
#53258 = CARTESIAN_POINT ( 'NONE',  ( 92.35000000000002274, -208.4700217866474645, 86.13708333333332234 ) ) ;
#53259 = ORIENTED_EDGE ( 'NONE', *, *, #10890, .T. ) ;
#53260 = ORIENTED_EDGE ( 'NONE', *, *, #24386, .T. ) ;
#53261 = EDGE_LOOP ( 'NONE', ( #34988, #2180, #71833, #40497 ) ) ;
#53262 = VECTOR ( 'NONE', #65337, 1000.000000000000000 ) ;
#53263 = EDGE_LOOP ( 'NONE', ( #39367, #26461, #16433, #33248 ) ) ;
#53264 = DIRECTION ( 'NONE',  ( -1.000000000000000000, -0.000000000000000000, -0.000000000000000000 ) ) ;
#53265 = AXIS2_PLACEMENT_3D ( 'NONE', #35921, #43349, #6267 ) ;
#53266 = CARTESIAN_POINT ( 'NONE',  ( -95.00000000000002842, 92.66308142843932671, 89.00781250086716057 ) ) ;
#53267 = DIRECTION ( 'NONE',  ( 1.000000000000000000, 0.000000000000000000, 0.000000000000000000 ) ) ;
#53268 = CARTESIAN_POINT ( 'NONE',  ( 0.000000000000000000, 0.000000000000000000, 0.000000000000000000 ) ) ;
#53269 = CARTESIAN_POINT ( 'NONE',  ( 92.35000000000002274, -211.5299782133524502, 74.89229166840097207 ) ) ;
#53270 = CARTESIAN_POINT ( 'NONE',  ( 97.64999999999999147, 90.00000000000002842, 76.98250000000000171 ) ) ;
#53271 = ORIENTED_EDGE ( 'NONE', *, *, #6451, .F. ) ;
#53272 = CARTESIAN_POINT ( 'NONE',  ( -93.67499999999998295, -212.2949673200287179, 87.75104166840095843 ) ) ;
#53273 = ADVANCED_FACE ( 'NONE', ( #5884 ), #28795, .F. ) ;
#53274 = VERTEX_POINT ( 'NONE', #63392 ) ;
#53275 = CARTESIAN_POINT ( 'NONE',  ( 15.00000000000000000, 0.000000000000000000, 0.000000000000000000 ) ) ;
#53276 = ORIENTED_EDGE ( 'NONE', *, *, #45860, .F. ) ;
#53277 = CARTESIAN_POINT ( 'NONE',  ( -92.35000000000003695, 90.00000000000004263, 86.58687500173429896 ) ) ;
#53278 = CARTESIAN_POINT ( 'NONE',  ( 96.15314808468748708, 88.00268892867053694, 75.88447916753381151 ) ) ;
#53279 = VERTEX_POINT ( 'NONE', #34811 ) ;
#53280 = CARTESIAN_POINT ( 'NONE',  ( 11.99999999999999822, 0.000000000000000000, 0.000000000000000000 ) ) ;
#53281 = CARTESIAN_POINT ( 'NONE',  ( 2.500000000000031530, 80.00000000000000000, -90.00000000000000000 ) ) ;
#53282 = CARTESIAN_POINT ( 'NONE',  ( -92.35000000018064270, -210.0000309433161476, 78.33187387208045038 ) ) ;
#53283 = CARTESIAN_POINT ( 'NONE',  ( 5.000000000000002665, -76.69515212745996280, -29.01471420065644580 ) ) ;
#53284 = ORIENTED_EDGE ( 'NONE', *, *, #2584, .T. ) ;
#53285 = CYLINDRICAL_SURFACE ( 'NONE', #31504, 31.99999999999999289 ) ;
#53286 = CARTESIAN_POINT ( 'NONE',  ( -97.65000000000001990, 90.00000000000004263, 79.83999999999998920 ) ) ;
#53287 = VERTEX_POINT ( 'NONE', #57749 ) ;
#53288 = ORIENTED_EDGE ( 'NONE', *, *, #38353, .F. ) ;
#53289 = EDGE_CURVE ( 'NONE', #39053, #54369, #21037, .T. ) ;
#53290 = FACE_OUTER_BOUND ( 'NONE', #62801, .T. ) ;
#53291 = ADVANCED_FACE ( 'NONE', ( #12641 ), #69788, .F. ) ;
#53292 = DIRECTION ( 'NONE',  ( 0.000000000000000000, 0.000000000000000000, 1.000000000000000000 ) ) ;
#53293 = VECTOR ( 'NONE', #26861, 1000.000000000000000 ) ;
#53294 = CARTESIAN_POINT ( 'NONE',  ( 10.00000000000000000, -39.78640506895653317, 66.50666863321987421 ) ) ;
#53295 = CARTESIAN_POINT ( 'NONE',  ( -92.69370383062498320, -209.9999999999999716, 88.21406250086714351 ) ) ;
#53296 = EDGE_LOOP ( 'NONE', ( #4395, #35736, #29606, #34565 ) ) ;
#53297 = CARTESIAN_POINT ( 'NONE',  ( -94.99999999999997158, -213.0599564267049857, 82.53874999999999318 ) ) ;
#53298 = ORIENTED_EDGE ( 'NONE', *, *, #42883, .F. ) ;
#53299 = ADVANCED_FACE ( 'NONE', ( #70147 ), #18647, .F. ) ;
#53300 = ADVANCED_FACE ( 'NONE', ( #53246 ), #35574, .T. ) ;
#53301 = ORIENTED_EDGE ( 'NONE', *, *, #7634, .T. ) ;
#53302 = DIRECTION ( 'NONE',  ( 2.603472992746261562E-14, 2.546204323184492723E-14, -1.000000000000000000 ) ) ;
#53303 = CIRCLE ( 'NONE', #6518, 31.99999999999999289 ) ;
#53304 = DIRECTION ( 'NONE',  ( 0.4796670183876317051, -0.8774505977381971134, 0.000000000000000000 ) ) ;
#53305 = DIRECTION ( 'NONE',  ( 0.000000000000000000, 0.000000000000000000, 1.000000000000000000 ) ) ;
#53306 = CARTESIAN_POINT ( 'NONE',  ( 92.69370383062498320, 88.66845928578035796, 80.17072916753380696 ) ) ;
#53307 = DIRECTION ( 'NONE',  ( 0.000000000000000000, 0.000000000000000000, 1.000000000000000000 ) ) ;
#53308 = FACE_OUTER_BOUND ( 'NONE', #71094, .T. ) ;
#53309 = CARTESIAN_POINT ( 'NONE',  ( -97.65000000000001990, 90.00000000000004263, 85.55499999999999261 ) ) ;
#53310 = LINE ( 'NONE', #36375, #21980 ) ;
#53311 = DIRECTION ( 'NONE',  ( -1.000000000000000000, -0.000000000000000000, -0.000000000000000000 ) ) ;
#53312 = CARTESIAN_POINT ( 'NONE',  ( 95.00000000000000000, -209.9999999999999716, 90.00000000000000000 ) ) ;
#53313 = CARTESIAN_POINT ( 'NONE',  ( 10.00000000000000000, 2.956366410621684260, -75.11725578898465017 ) ) ;
#53314 = VECTOR ( 'NONE', #26618, 1000.000000000000000 ) ;
#53315 = AXIS2_PLACEMENT_3D ( 'NONE', #23831, #70048, #12173 ) ;
#53316 = EDGE_CURVE ( 'NONE', #19317, #28874, #69065, .T. ) ;
#53317 = CARTESIAN_POINT ( 'NONE',  ( 0.000000000000000000, -39.47590169984898978, 71.87247863392400404 ) ) ;
#53318 = CARTESIAN_POINT ( 'NONE',  ( 97.64999999999999147, -209.9999999999999716, 86.50750000000000739 ) ) ;
#53319 = VECTOR ( 'NONE', #40750, 1000.000000000000000 ) ;
#53320 = CARTESIAN_POINT ( 'NONE',  ( -93.84685191531252713, 88.00268892867056536, 87.31447916753380412 ) ) ;
#53321 = AXIS2_PLACEMENT_3D ( 'NONE', #47035, #63963, #6801 ) ;
#53322 = LINE ( 'NONE', #24744, #37158 ) ;
#53324 = EDGE_CURVE ( 'NONE', #61596, #68440, #13385, .T. ) ;
#53323 = CARTESIAN_POINT ( 'NONE',  ( -3.000000000000000000, 23.50000000000000000, 1.499999999999997780 ) ) ;
#53325 = ORIENTED_EDGE ( 'NONE', *, *, #7805, .T. ) ;
#53326 = DIRECTION ( 'NONE',  ( 0.000000000000000000, -0.4067366430757887730, 0.9135454576426059736 ) ) ;
#53327 = ADVANCED_FACE ( 'NONE', ( #17550 ), #13008, .T. ) ;
#53328 = DIRECTION ( 'NONE',  ( -1.000000000000000000, 0.000000000000000000, 0.000000000000000000 ) ) ;
#53329 = CARTESIAN_POINT ( 'NONE',  ( 12.00000000000000000, -19.89357724625003598, -12.59942793731059041 ) ) ;
#53330 = AXIS2_PLACEMENT_3D ( 'NONE', #61421, #15546, #61791 ) ;
#53331 = LINE ( 'NONE', #32139, #10425 ) ;
#53332 = CARTESIAN_POINT ( 'NONE',  ( 92.69370383062501162, -209.9999999999999716, 82.81656250086714977 ) ) ;
#53333 = ORIENTED_EDGE ( 'NONE', *, *, #55522, .T. ) ;
#53334 = ORIENTED_EDGE ( 'NONE', *, *, #46177, .T. ) ;
#53335 = DIRECTION ( 'NONE',  ( 0.000000000000000000, 0.5877852522924684742, 0.8090169943749506709 ) ) ;
#53336 = ORIENTED_EDGE ( 'NONE', *, *, #23015, .T. ) ;
#53337 = VECTOR ( 'NONE', #37862, 1000.000000000000000 ) ;
#53338 = CARTESIAN_POINT ( 'NONE',  ( 10.00000000000000000, 0.000000000000000000, 0.000000000000000000 ) ) ;
#53339 = CARTESIAN_POINT ( 'NONE',  ( 93.84685191531251292, -211.9973110713294489, 76.41364583420048007 ) ) ;
#53340 = ORIENTED_EDGE ( 'NONE', *, *, #38308, .F. ) ;
#53341 = CARTESIAN_POINT ( 'NONE',  ( 97.30629616937498838, -209.9999999999999716, 79.32406250086715715 ) ) ;
#53342 = VERTEX_POINT ( 'NONE', #36316 ) ;
#53343 = DIRECTION ( 'NONE',  ( -0.000000000000000000, -0.000000000000000000, 1.000000000000000000 ) ) ;
#53344 = ORIENTED_EDGE ( 'NONE', *, *, #37887, .F. ) ;
#53345 = VERTEX_POINT ( 'NONE', #52880 ) ;
#53346 = CARTESIAN_POINT ( 'NONE',  ( 96.32499999999998863, -207.7050326799711968, 86.69270833506763552 ) ) ;
#53347 = AXIS2_PLACEMENT_3D ( 'NONE', #29297, #24777, #784 ) ;
#53348 = CARTESIAN_POINT ( 'NONE',  ( -2.500000000000017319, -80.00000000000001421, -269.9999999999999432 ) ) ;
#53349 = ORIENTED_EDGE ( 'NONE', *, *, #42854, .F. ) ;
#53350 = DIRECTION ( 'NONE',  ( -1.000000000000000000, -0.000000000000000000, 0.000000000000000000 ) ) ;
#53351 = CARTESIAN_POINT ( 'NONE',  ( 93.67500000000001137, -212.2949673200287179, 84.47020833506762472 ) ) ;
#53352 = CARTESIAN_POINT ( 'NONE',  ( 96.32499999999997442, 92.29496732002878900, 89.78833333333332689 ) ) ;
#53353 = ORIENTED_EDGE ( 'NONE', *, *, #13477, .F. ) ;
#53354 = CARTESIAN_POINT ( 'NONE',  ( 0.000000000000000000, 27.13269053701132094, -25.88420570971372570 ) ) ;
#53355 = DIRECTION ( 'NONE',  ( 1.000000000000000000, 0.000000000000000000, 0.000000000000000000 ) ) ;
#53356 = AXIS2_PLACEMENT_3D ( 'NONE', #58529, #41994, #64930 ) ;
#53357 = ORIENTED_EDGE ( 'NONE', *, *, #60046, .F. ) ;
#53358 = VERTEX_POINT ( 'NONE', #70507 ) ;
#53359 = CARTESIAN_POINT ( 'NONE',  ( -93.84685191531252713, 88.00268892867056536, 86.83822916753382515 ) ) ;
#53360 = AXIS2_PLACEMENT_3D ( 'NONE', #62882, #18457, #17719 ) ;
#53361 = CARTESIAN_POINT ( 'NONE',  ( 93.84685191531248449, 91.99731107132950569, 86.36197916753381776 ) ) ;
#53362 = ORIENTED_EDGE ( 'NONE', *, *, #33916, .T. ) ;
#53363 = CARTESIAN_POINT ( 'NONE',  ( 96.32499999999997442, 92.29496732002878900, 86.05770833506763040 ) ) ;
#53364 = CIRCLE ( 'NONE', #22144, 77.49899999999999523 ) ;
#53365 = ORIENTED_EDGE ( 'NONE', *, *, #73483, .F. ) ;
#53366 = CYLINDRICAL_SURFACE ( 'NONE', #39307, 77.49899999999999523 ) ;
#53367 = AXIS2_PLACEMENT_3D ( 'NONE', #57860, #39460, #68025 ) ;
#53368 = LINE ( 'NONE', #61151, #55831 ) ;
#53370 = EDGE_CURVE ( 'NONE', #27662, #47563, #58893, .T. ) ;
#53369 = EDGE_LOOP ( 'NONE', ( #41510, #6407, #63699, #13401 ) ) ;
#53371 = ORIENTED_EDGE ( 'NONE', *, *, #62590, .T. ) ;
#53372 = ORIENTED_EDGE ( 'NONE', *, *, #73915, .F. ) ;
#53373 = CARTESIAN_POINT ( 'NONE',  ( -92.35000000000002274, 90.00000000000004263, 75.00000000000000000 ) ) ;
#53374 = EDGE_CURVE ( 'NONE', #19936, #44954, #29928, .T. ) ;
#53376 = CIRCLE ( 'NONE', #17360, 82.00000000000000000 ) ;
#53375 = CARTESIAN_POINT ( 'NONE',  ( 10.00000000000000000, -50.23322058963393033, 64.81221759200326460 ) ) ;
#53377 = CARTESIAN_POINT ( 'NONE',  ( -92.35000000000005116, 88.47002178664754979, 85.18458333333332178 ) ) ;
#53378 = EDGE_CURVE ( 'NONE', #28922, #45162, #64528, .T. ) ;
#53379 = ORIENTED_EDGE ( 'NONE', *, *, #26845, .F. ) ;
#53380 = DIRECTION ( 'NONE',  ( 0.000000000000000000, 0.000000000000000000, 1.000000000000000000 ) ) ;
#53381 = CIRCLE ( 'NONE', #42539, 3.299999999999997158 ) ;
#53382 = CARTESIAN_POINT ( 'NONE',  ( 95.00000000000000000, -209.9999999999999716, 90.00000000000000000 ) ) ;
#53383 = VERTEX_POINT ( 'NONE', #34846 ) ;
#53384 = DIRECTION ( 'NONE',  ( 2.603472992746261562E-14, 2.546204323184492723E-14, -1.000000000000000000 ) ) ;
#53385 = CARTESIAN_POINT ( 'NONE',  ( -96.15314808468747287, -208.0026889286704943, 81.91697916753381037 ) ) ;
#53386 = VERTEX_POINT ( 'NONE', #7389 ) ;
#53387 = FACE_OUTER_BOUND ( 'NONE', #28320, .T. ) ;
#53388 = PLANE ( 'NONE',  #48845 ) ;
#53389 = CARTESIAN_POINT ( 'NONE',  ( 11.99999999999999822, 14.66109333815460225, 73.73191006444577056 ) ) ;
#53390 = FACE_OUTER_BOUND ( 'NONE', #45419, .T. ) ;
#53391 = CIRCLE ( 'NONE', #20959, 37.49900000000000944 ) ;
#53392 = EDGE_CURVE ( 'NONE', #47001, #6488, #35439, .T. ) ;
#53393 = DIRECTION ( 'NONE',  ( -1.000000000000000000, -0.000000000000000000, -0.000000000000000000 ) ) ;
#53394 = CARTESIAN_POINT ( 'NONE',  ( 5.000000000000002665, -22.90783923731686045, 78.73519480814945837 ) ) ;
#53395 = DIRECTION ( 'NONE',  ( -1.000000000000000000, 0.000000000000000000, -0.000000000000000000 ) ) ;
#53396 = DIRECTION ( 'NONE',  ( -0.000000000000000000, -0.000000000000000000, 1.000000000000000000 ) ) ;
#53397 = DIRECTION ( 'NONE',  ( -1.000000000000000000, 0.000000000000000000, 0.000000000000000000 ) ) ;
#53398 = LINE ( 'NONE', #60169, #47632 ) ;
#53399 = CARTESIAN_POINT ( 'NONE',  ( -92.69370383062502583, 91.33154071421968467, 75.40822916753381833 ) ) ;
#53400 = CYLINDRICAL_SURFACE ( 'NONE', #43081, 77.49899999999999523 ) ;
#53401 = LINE ( 'NONE', #3041, #33821 ) ;
#53402 = ADVANCED_FACE ( 'NONE', ( #17921 ), #23939, .F. ) ;
#53403 =( BOUNDED_CURVE ( )  B_SPLINE_CURVE ( 2, ( #50161, #61840, #10323, #56193, #62974, #16337, #62595 ),
 .UNSPECIFIED., .F., .F. ) 
 B_SPLINE_CURVE_WITH_KNOTS ( ( 3, 2, 2, 3 ),
 ( 0.5503499107226622611, 0.5574054777297072771, 0.5644612432705896632, 0.5715170088666295944 ),
 .UNSPECIFIED. ) 
 CURVE ( )  GEOMETRIC_REPRESENTATION_ITEM ( )  RATIONAL_B_SPLINE_CURVE ( ( 0.9999924607068835236, 0.8660291735370695410, 1.000000000000000000, 0.8660254037844387076, 1.000000000000000000, 0.8660254037844387076, 1.000000000000000000 ) ) 
 REPRESENTATION_ITEM ( '' )  );
#53404 = EDGE_CURVE ( 'NONE', #53605, #46835, #23205, .T. ) ;
#53405 = DIRECTION ( 'NONE',  ( -1.000000000000000000, -0.000000000000000000, 0.000000000000000000 ) ) ;
#53406 = EDGE_CURVE ( 'NONE', #9362, #31085, #59485, .T. ) ;
#53407 = CARTESIAN_POINT ( 'NONE',  ( -15.44521549751111422, -137.7748507232956001, 5.500000000000000000 ) ) ;
#53408 = DIRECTION ( 'NONE',  ( 0.000000000000000000, 0.000000000000000000, 1.000000000000000000 ) ) ;
#53409 = CARTESIAN_POINT ( 'NONE',  ( -12.50000000000000000, -132.5000000000000000, 40.00000000000000000 ) ) ;
#53410 = DIRECTION ( 'NONE',  ( 0.000000000000000000, -0.9135454576426059736, 0.4067366430757887730 ) ) ;
#53411 = DIRECTION ( 'NONE',  ( 0.000000000000000000, 0.1045284632676436315, 0.9945218953682742891 ) ) ;
#53412 = CARTESIAN_POINT ( 'NONE',  ( -94.99999999999997158, -207.3369185715606307, 76.94281250086714863 ) ) ;
#53413 = CYLINDRICAL_SURFACE ( 'NONE', #72206, 3.299999999999969624 ) ;
#53414 = ADVANCED_FACE ( 'NONE', ( #7002 ), #23561, .F. ) ;
#53415 = ORIENTED_EDGE ( 'NONE', *, *, #60997, .T. ) ;
#53416 = VECTOR ( 'NONE', #32, 1000.000000000000114 ) ;
#53417 = LINE ( 'NONE', #63972, #46744 ) ;
#53418 = CIRCLE ( 'NONE', #25775, 42.00000000000000000 ) ;
#53419 = CARTESIAN_POINT ( 'NONE',  ( 5.000000000000000000, -32.34446384429989507, 26.79245525562703278 ) ) ;
#53420 = CARTESIAN_POINT ( 'NONE',  ( 11.99999999999999822, -72.35432306680498016, 20.40083707022857951 ) ) ;
#53421 = AXIS2_PLACEMENT_3D ( 'NONE', #21501, #44459, #45582 ) ;
#53422 = VECTOR ( 'NONE', #49954, 1000.000000000000000 ) ;
#53423 = DIRECTION ( 'NONE',  ( 0.000000000000000000, 0.000000000000000000, 1.000000000000000000 ) ) ;
#53424 = EDGE_LOOP ( 'NONE', ( #50503, #72405, #22127, #46781 ) ) ;
#53425 = CARTESIAN_POINT ( 'NONE',  ( 10.00000000000000000, -12.93880638057259169, -76.41127070299286572 ) ) ;
#53426 = CARTESIAN_POINT ( 'NONE',  ( 0.000000000000000000, 0.000000000000000000, 42.00000000000001421 ) ) ;
#53427 = ORIENTED_EDGE ( 'NONE', *, *, #16114, .F. ) ;
#53428 = CARTESIAN_POINT ( 'NONE',  ( 96.15314808468750130, -211.9973110713294489, 84.77447916753381207 ) ) ;
#53429 = DIRECTION ( 'NONE',  ( 0.000000000000000000, 0.000000000000000000, 1.000000000000000000 ) ) ;
#53430 = ORIENTED_EDGE ( 'NONE', *, *, #61564, .F. ) ;
#53431 = CIRCLE ( 'NONE', #42658, 82.00000000000000000 ) ;
#53432 = CARTESIAN_POINT ( 'NONE',  ( 12.00000000000000000, -10.45096189432314127, 21.10159698893440350 ) ) ;
#53433 = ORIENTED_EDGE ( 'NONE', *, *, #35414, .T. ) ;
#53434 = DIRECTION ( 'NONE',  ( -1.000000000000000000, 0.000000000000000000, -0.000000000000000000 ) ) ;
#53435 = VERTEX_POINT ( 'NONE', #58145 ) ;
#53436 = CARTESIAN_POINT ( 'NONE',  ( -93.84685191531252713, 88.00268892867056536, 79.21822916753382060 ) ) ;
#53437 = VERTEX_POINT ( 'NONE', #6643 ) ;
#53438 = CIRCLE ( 'NONE', #9050, 11.59999999999999964 ) ;
#53439 = ORIENTED_EDGE ( 'NONE', *, *, #68628, .T. ) ;
#53440 = CARTESIAN_POINT ( 'NONE',  ( 11.99999999999999822, 0.000000000000000000, 0.000000000000000000 ) ) ;
#53441 = ORIENTED_EDGE ( 'NONE', *, *, #29877, .F. ) ;
#53442 = CARTESIAN_POINT ( 'NONE',  ( 0.000000000000000000, -8.830959090341869100, -74.65491531819127147 ) ) ;
#53443 = DIRECTION ( 'NONE',  ( 0.2867529058022035837, -0.9580045777625452175, 0.000000000000000000 ) ) ;
#53444 = ORIENTED_EDGE ( 'NONE', *, *, #64443, .T. ) ;
#53445 = DIRECTION ( 'NONE',  ( -1.000000000000000000, -0.000000000000000000, -0.000000000000000000 ) ) ;
#53446 = ORIENTED_EDGE ( 'NONE', *, *, #59020, .F. ) ;
#53447 = DIRECTION ( 'NONE',  ( 1.000000000000000000, 0.000000000000000000, 0.000000000000000000 ) ) ;
#53448 = ORIENTED_EDGE ( 'NONE', *, *, #31911, .F. ) ;
#53449 = EDGE_CURVE ( 'NONE', #5103, #50093, #65505, .T. ) ;
#53450 = ORIENTED_EDGE ( 'NONE', *, *, #48893, .T. ) ;
#53451 = ORIENTED_EDGE ( 'NONE', *, *, #40248, .T. ) ;
#53452 = CARTESIAN_POINT ( 'NONE',  ( 95.00000000000000000, -212.6630814284392557, 77.10156250086711793 ) ) ;
#53453 = DIRECTION ( 'NONE',  ( -1.000000000000000000, 0.000000000000000000, -0.000000000000000000 ) ) ;
#53454 = CIRCLE ( 'NONE', #73902, 77.49899999999999523 ) ;
#53455 = ITEM_DEFINED_TRANSFORMATION ( 'NONE', 'NONE', #18356,  #43395 ) ;
#53456 = CARTESIAN_POINT ( 'NONE',  ( -97.64995850909662067, -211.5300021681366047, 85.68729332542763188 ) ) ;
#53457 = ADVANCED_FACE ( 'NONE', ( #42341 ), #70893, .F. ) ;
#53458 = DIRECTION ( 'NONE',  ( -1.000000000000000000, 0.000000000000000000, 0.000000000000000000 ) ) ;
#53459 = DIRECTION ( 'NONE',  ( -1.000000000000000000, -0.000000000000000000, 0.000000000000000000 ) ) ;
#53460 = ADVANCED_FACE ( 'NONE', ( #20784 ), #43738, .F. ) ;
#53461 = CARTESIAN_POINT ( 'NONE',  ( 0.000000000000000000, -55.38113227695743745, -54.21277698773734244 ) ) ;
#53462 = CARTESIAN_POINT ( 'NONE',  ( 23.30762065077924916, -123.0008031590507329, -2.500000000000000000 ) ) ;
#53463 = ADVANCED_FACE ( 'NONE', ( #8112 ), #61393, .T. ) ;
#53464 = CYLINDRICAL_SURFACE ( 'NONE', #38328, 77.49899999999999523 ) ;
#53465 = CARTESIAN_POINT ( 'NONE',  ( -93.84685191531247028, -211.9973110713294489, 80.32947916753380468 ) ) ;
#53466 = CARTESIAN_POINT ( 'NONE',  ( -92.69370383062502583, 91.33154071421968467, 81.91697916753381037 ) ) ;
#53467 = ORIENTED_EDGE ( 'NONE', *, *, #50823, .T. ) ;
#53468 = CARTESIAN_POINT ( 'NONE',  ( 96.15314808468748708, 91.99731107132950569, 82.44614583420046472 ) ) ;
#53469 = ADVANCED_FACE ( 'NONE', ( #49715 ), #27148, .F. ) ;
#53470 = EDGE_LOOP ( 'NONE', ( #42759, #31344, #8695, #68250 ) ) ;
#53471 = PLANE ( 'NONE',  #38332 ) ;
#53473 = VECTOR ( 'NONE', #41192, 1000.000000000000000 ) ;
#53472 = CARTESIAN_POINT ( 'NONE',  ( 5.000000000000002665, -29.01471420065617224, 76.69515212746007649 ) ) ;
#53474 = LINE ( 'NONE', #54583, #14593 ) ;
#53475 = AXIS2_PLACEMENT_3D ( 'NONE', #12398, #68070, #22582 ) ;
#53476 = CARTESIAN_POINT ( 'NONE',  ( 10.00000000000000000, -46.54456581323762521, -59.03342792756313884 ) ) ;
#53477 = CARTESIAN_POINT ( 'NONE',  ( -2.500000000000012879, -65.00000000000000000, -90.00000000000000000 ) ) ;
#53478 = CARTESIAN_POINT ( 'NONE',  ( -94.99999999999997158, -212.6630814284392557, 82.18156250086715886 ) ) ;
#53479 = ADVANCED_FACE ( 'NONE', ( #38078 ), #44474, .F. ) ;
#53480 = CARTESIAN_POINT ( 'NONE',  ( -92.34999999999996589, -211.5299782133524502, 89.62958333333334338 ) ) ;
#53481 = CARTESIAN_POINT ( 'NONE',  ( 0.000000000000000000, 0.000000000000000000, 125.0000000000000000 ) ) ;
#53482 = AXIS2_PLACEMENT_3D ( 'NONE', #50194, #22386, #15637 ) ;
#53483 = DIRECTION ( 'NONE',  ( -0.000000000000000000, -0.000000000000000000, 1.000000000000000000 ) ) ;
#53484 = ORIENTED_EDGE ( 'NONE', *, *, #68856, .F. ) ;
#53485 = VERTEX_POINT ( 'NONE', #65279 ) ;
#53486 = CIRCLE ( 'NONE', #28298, 32.00000000000000000 ) ;
#53487 = LINE ( 'NONE', #14371, #25472 ) ;
#53488 = DIRECTION ( 'NONE',  ( 0.000000000000000000, 0.000000000000000000, 1.000000000000000000 ) ) ;
#53489 = CARTESIAN_POINT ( 'NONE',  ( -92.69370383062502583, 88.66845928578038638, 84.19239583420046813 ) ) ;
#53490 = LINE ( 'NONE', #70386, #10584 ) ;
#53491 = DIRECTION ( 'NONE',  ( -0.000000000000000000, -0.000000000000000000, -1.000000000000000000 ) ) ;
#53492 = LINE ( 'NONE', #18169, #26519 ) ;
#53493 = CARTESIAN_POINT ( 'NONE',  ( 2.459674775249762302, 2.188067104722127970E-13, 20.20000000000039009 ) ) ;
#53494 = ORIENTED_EDGE ( 'NONE', *, *, #50045, .T. ) ;
#53495 = EDGE_CURVE ( 'NONE', #31458, #23125, #67390, .T. ) ;
#53496 = CARTESIAN_POINT ( 'NONE',  ( -93.84685191531254134, 91.99731107132950569, 74.82614583420047438 ) ) ;
#53497 = VECTOR ( 'NONE', #50122, 1000.000000000000000 ) ;
#53498 = EDGE_CURVE ( 'NONE', #913, #49620, #27043, .T. ) ;
#53499 = EDGE_CURVE ( 'NONE', #63816, #71661, #55890, .T. ) ;
#53500 = CARTESIAN_POINT ( 'NONE',  ( 5.000000000000000000, -50.23322058963298531, -64.81221759200398935 ) ) ;
#53501 = DIRECTION ( 'NONE',  ( -0.000000000000000000, -0.000000000000000000, -1.000000000000000000 ) ) ;
#53502 = DIRECTION ( 'NONE',  ( -0.8225049752423791993, -0.5687579148473745905, 0.000000000000000000 ) ) ;
#53503 = COLOUR_RGB ( '', 0.08235294, 0.09019608, 0.10196078) ;
#53504 = DIRECTION ( 'NONE',  ( -1.000000000000000000, 0.000000000000000000, 0.000000000000000000 ) ) ;
#53505 = CARTESIAN_POINT ( 'NONE',  ( -96.15314808468745866, -211.9973110713294489, 85.46239583420047836 ) ) ;
#53506 = FACE_OUTER_BOUND ( 'NONE', #31877, .T. ) ;
#53507 = EDGE_CURVE ( 'NONE', #28753, #57811, #29460, .T. ) ;
#53508 = DIRECTION ( 'NONE',  ( 0.000000000000000000, 0.000000000000000000, 1.000000000000000000 ) ) ;
#53509 = CARTESIAN_POINT ( 'NONE',  ( -92.69370383062498320, -209.9999999999999716, 76.78406250086715090 ) ) ;
#53510 = CARTESIAN_POINT ( 'NONE',  ( 0.000000000000000000, 33.00180498840046539, 17.80606268964551120 ) ) ;
#53511 = ORIENTED_EDGE ( 'NONE', *, *, #72401, .T. ) ;
#53512 = CARTESIAN_POINT ( 'NONE',  ( -94.99999999999997158, -213.0599564267049857, 81.98312500173430806 ) ) ;
#53513 = CARTESIAN_POINT ( 'NONE',  ( 10.00000000000000178, 0.000000000000000000, 0.000000000000000000 ) ) ;
#53514 = DIRECTION ( 'NONE',  ( -1.000000000000000000, 5.236901059551556403E-15, 2.618450529775778123E-14 ) ) ;
#53515 = DIRECTION ( 'NONE',  ( -7.945298363252408085E-16, -1.065814103640131188E-14, -1.000000000000000000 ) ) ;
#53516 = CARTESIAN_POINT ( 'NONE',  ( 95.00000000000000000, -212.6630814284392557, 77.10156250086711793 ) ) ;
#53517 = ORIENTED_EDGE ( 'NONE', *, *, #68768, .T. ) ;
#53518 = DIRECTION ( 'NONE',  ( 0.000000000000000000, -0.3090169943749563330, 0.9510565162951507556 ) ) ;
#53519 = DIRECTION ( 'NONE',  ( 0.000000000000000000, 0.9876883405951382144, -0.1564344650402276493 ) ) ;
#53520 = VERTEX_POINT ( 'NONE', #10241 ) ;
#53521 = CARTESIAN_POINT ( 'NONE',  ( -3.000000000000002665, 0.000000000000000000, -19.21700905503013601 ) ) ;
#53522 = AXIS2_PLACEMENT_3D ( 'NONE', #46081, #12953, #35891 ) ;
#53523 = ORIENTED_EDGE ( 'NONE', *, *, #18997, .T. ) ;
#53524 = CARTESIAN_POINT ( 'NONE',  ( 10.00000000000000000, 70.52718814184260054, 26.02418014898334420 ) ) ;
#53525 = AXIS2_PLACEMENT_3D ( 'NONE', #5850, #28759, #7322 ) ;
#53526 = ORIENTED_EDGE ( 'NONE', *, *, #45576, .T. ) ;
#53527 = AXIS2_PLACEMENT_3D ( 'NONE', #4250, #27139, #50821 ) ;
#53528 = VERTEX_POINT ( 'NONE', #33165 ) ;
#53529 = TOROIDAL_SURFACE ( 'NONE', #63159, 3.250000000000001332, 0.2500000000000000000 ) ;
#53530 = ORIENTED_EDGE ( 'NONE', *, *, #56690, .F. ) ;
#53531 = DIRECTION ( 'NONE',  ( 0.000000000000000000, 0.000000000000000000, 1.000000000000000000 ) ) ;
#53532 = ORIENTED_EDGE ( 'NONE', *, *, #44985, .T. ) ;
#53533 = VECTOR ( 'NONE', #34716, 1000.000000000000000 ) ;
#53534 = VECTOR ( 'NONE', #19991, 1000.000000000000000 ) ;
#53535 = ORIENTED_EDGE ( 'NONE', *, *, #15776, .F. ) ;
#53536 = CARTESIAN_POINT ( 'NONE',  ( 92.69370383062498320, 91.33154071421968467, 80.22364583420048234 ) ) ;
#53537 = CARTESIAN_POINT ( 'NONE',  ( -96.32500000000001705, 87.70503267997129626, 81.29520833506762756 ) ) ;
#53538 = CARTESIAN_POINT ( 'NONE',  ( 0.000000000000000000, 75.11764819372142199, 2.946379043147685728 ) ) ;
#53539 = ORIENTED_EDGE ( 'NONE', *, *, #27471, .T. ) ;
#53540 = ORIENTED_EDGE ( 'NONE', *, *, #6363, .T. ) ;
#53541 = ORIENTED_EDGE ( 'NONE', *, *, #10382, .T. ) ;
#53542 = CARTESIAN_POINT ( 'NONE',  ( -2.500000000000017319, -80.00000000000001421, -269.9999999999999432 ) ) ;
#53543 = ORIENTED_EDGE ( 'NONE', *, *, #9319, .F. ) ;
#53544 = DIRECTION ( 'NONE',  ( 0.000000000000000000, -2.775557561562891351E-17, 1.000000000000000000 ) ) ;
#53545 = LINE ( 'NONE', #2084, #60736 ) ;
#53546 = EDGE_CURVE ( 'NONE', #14214, #49169, #32792, .T. ) ;
#53547 = AXIS2_PLACEMENT_3D ( 'NONE', #10903, #6022, #44 ) ;
#53548 = CARTESIAN_POINT ( 'NONE',  ( -94.00680085345865677, 92.13398380010822564, 74.81432998548486069 ) ) ;
#53549 = DIRECTION ( 'NONE',  ( -1.000000000000000000, -0.000000000000000000, -0.000000000000000000 ) ) ;
#53550 = DIRECTION ( 'NONE',  ( -1.000000000000000000, -0.000000000000000000, -0.000000000000000000 ) ) ;
#53551 = CYLINDRICAL_SURFACE ( 'NONE', #43260, 2.649999999999985700 ) ;
#53552 = CARTESIAN_POINT ( 'NONE',  ( 10.00000000000000000, 4.992566952385523393, -37.16516213103272293 ) ) ;
#53553 = ADVANCED_FACE ( 'NONE', ( #55372 ), #21144, .T. ) ;
#53554 = CARTESIAN_POINT ( 'NONE',  ( -92.34999999999999432, -211.5299782133524502, 79.54895833506762415 ) ) ;
#53555 = DIRECTION ( 'NONE',  ( -0.000000000000000000, -0.000000000000000000, 1.000000000000000000 ) ) ;
#53557 = CARTESIAN_POINT ( 'NONE',  ( -92.35000000000005116, 88.47002178664754979, 76.37395833506761278 ) ) ;
#53556 = CARTESIAN_POINT ( 'NONE',  ( 93.67499999999998295, 92.29496732002878900, 76.00354166840097037 ) ) ;
#53558 = ORIENTED_EDGE ( 'NONE', *, *, #60951, .F. ) ;
#53559 = CARTESIAN_POINT ( 'NONE',  ( 97.30629616937498838, 91.33154071421968467, 75.56697916753383026 ) ) ;
#53560 = LINE ( 'NONE', #24984, #25346 ) ;
#53561 = DIRECTION ( 'NONE',  ( -1.000000000000000000, 0.000000000000000000, 0.000000000000000000 ) ) ;
#53562 = DIRECTION ( 'NONE',  ( 0.000000000000000000, 0.1564344650402243742, 0.9876883405951387696 ) ) ;
#53563 = CARTESIAN_POINT ( 'NONE',  ( 11.99999999999999822, 73.44644590900061587, 24.73286445877730699 ) ) ;
#53564 = FACE_OUTER_BOUND ( 'NONE', #7412, .T. ) ;
#53565 = ORIENTED_EDGE ( 'NONE', *, *, #17000, .F. ) ;
#53566 = CARTESIAN_POINT ( 'NONE',  ( 10.00000000000000000, 37.22597642581158084, -5.202137450156524068 ) ) ;
#53567 = DIRECTION ( 'NONE',  ( -1.000000000000000000, -0.000000000000000000, 0.000000000000000000 ) ) ;
#53568 = ORIENTED_EDGE ( 'NONE', *, *, #58305, .T. ) ;
#53569 = ORIENTED_EDGE ( 'NONE', *, *, #28711, .T. ) ;
#53570 = EDGE_CURVE ( 'NONE', #17509, #64359, #15516, .T. ) ;
#53571 = EDGE_CURVE ( 'NONE', #19421, #53274, #3052, .T. ) ;
#53572 = CARTESIAN_POINT ( 'NONE',  ( 10.00000000000000000, 40.98264845739763018, -9.188173127306866306 ) ) ;
#53573 = CARTESIAN_POINT ( 'NONE',  ( 97.64999999999993463, -208.4700217866474077, 81.48041666666665606 ) ) ;
#53574 = DIRECTION ( 'NONE',  ( 1.000000000000000000, 0.000000000000000000, 0.000000000000000000 ) ) ;
#53575 = CARTESIAN_POINT ( 'NONE',  ( -0.0004442498525516064278, 0.001194404164626844313, -64.00000000000000000 ) ) ;
#53576 = CARTESIAN_POINT ( 'NONE',  ( -92.69370383062498320, -208.6684592857803011, 76.83697916753382628 ) ) ;
#53577 = CIRCLE ( 'NONE', #16332, 16.00000000000000000 ) ;
#53578 = ORIENTED_EDGE ( 'NONE', *, *, #71520, .F. ) ;
#53579 = DIRECTION ( 'NONE',  ( -0.000000000000000000, -0.000000000000000000, 1.000000000000000000 ) ) ;
#53580 = EDGE_CURVE ( 'NONE', #58797, #67105, #65688, .T. ) ;
#53581 = EDGE_CURVE ( 'NONE', #37368, #67705, #21227, .T. ) ;
#53582 = DIRECTION ( 'NONE',  ( -1.000000000000000000, 0.000000000000000000, 0.000000000000000000 ) ) ;
#53583 = DIRECTION ( 'NONE',  ( 0.000000000000000000, 0.8910065241883655673, 0.4539904997395510233 ) ) ;
#53584 = DIRECTION ( 'NONE',  ( -0.2867529058022035837, 0.9580045777625452175, 0.000000000000000000 ) ) ;
#53585 = DIRECTION ( 'NONE',  ( -0.8774505977381971134, -0.4796670183876317051, 0.000000000000000000 ) ) ;
#53586 = DIRECTION ( 'NONE',  ( 0.000000000000000000, 0.000000000000000000, -1.000000000000000000 ) ) ;
#53587 = VECTOR ( 'NONE', #61136, 1000.000000000000000 ) ;
#53588 = CARTESIAN_POINT ( 'NONE',  ( 19.29194287201271862, -133.5026271600380880, 5.500000000000000000 ) ) ;
#53589 = DIRECTION ( 'NONE',  ( 0.000000000000000000, 0.000000000000000000, 1.000000000000000000 ) ) ;
#53590 = CARTESIAN_POINT ( 'NONE',  ( 10.00000000000000000, -27.05870788708250885, 26.08949754953014022 ) ) ;
#53591 = DIRECTION ( 'NONE',  ( -1.000000000000000000, 3.061616997868383141E-16, -0.000000000000000000 ) ) ;
#53592 = VECTOR ( 'NONE', #49676, 1000.000000000000000 ) ;
#53593 = AXIS2_PLACEMENT_3D ( 'NONE', #52278, #12423, #18430 ) ;
#53594 = CARTESIAN_POINT ( 'NONE',  ( 94.99999999999998579, 92.66308142843932671, 84.56281250086716739 ) ) ;
#53595 = CARTESIAN_POINT ( 'NONE',  ( -92.69370383062498320, -209.9999999999999716, 85.03906250086714635 ) ) ;
#53596 = CARTESIAN_POINT ( 'NONE',  ( 0.000000000000000000, 0.000000000000000000, 0.000000000000000000 ) ) ;
#53597 = ORIENTED_EDGE ( 'NONE', *, *, #8419, .F. ) ;
#53598 = CARTESIAN_POINT ( 'NONE',  ( 15.00000000000000000, -14.54903810567676636, -22.19967320028755964 ) ) ;
#53599 = CARTESIAN_POINT ( 'NONE',  ( -93.67499999999998295, -207.7050326799711968, 80.26333333333332121 ) ) ;
#53600 = CARTESIAN_POINT ( 'NONE',  ( -97.30629616937501680, 90.00000000000004263, 75.67281250086713840 ) ) ;
#53601 = CARTESIAN_POINT ( 'NONE',  ( 97.30629616937498838, -209.9999999999999716, 86.15031250086714465 ) ) ;
#53602 = VERTEX_POINT ( 'NONE', #49356 ) ;
#53603 = CYLINDRICAL_SURFACE ( 'NONE', #52687, 31.99999999999998579 ) ;
#53604 = ORIENTED_EDGE ( 'NONE', *, *, #42703, .T. ) ;
#53605 = VERTEX_POINT ( 'NONE', #15138 ) ;
#53606 = DIRECTION ( 'NONE',  ( 0.000000000000000000, -0.3090169943749548342, 0.9510565162951510887 ) ) ;
#53608 = CLOSED_SHELL ( 'NONE', ( #6901, #28194, #36732, #43320, #26989, #33155, #31410, #13169, #51491, #69752, #55435, #36005, #36995, #392, #26635, #624, #54987, #67671, #41024, #68169, #7022, #48982, #12731, #57816, #55099, #51166, #32745, #4425 ) ) ;
#53607 = CARTESIAN_POINT ( 'NONE',  ( 10.00000000000000000, 27.05870788708267582, -26.08949754952995903 ) ) ;
#53609 = ORIENTED_EDGE ( 'NONE', *, *, #25199, .F. ) ;
#53610 = VERTEX_POINT ( 'NONE', #39196 ) ;
#53611 = CARTESIAN_POINT ( 'NONE',  ( -1.200000000000000030E-05, 0.9569279952884557350, -2.499999999999984457 ) ) ;
#53612 = CARTESIAN_POINT ( 'NONE',  ( 92.69370383062501162, -209.9999999999999716, 79.00656250086716170 ) ) ;
#53613 = CARTESIAN_POINT ( 'NONE',  ( -94.99999999999997158, -206.9400435732949575, 80.95125000000000171 ) ) ;
#53614 = DIRECTION ( 'NONE',  ( 1.000000000000000000, 0.000000000000000000, -0.000000000000000000 ) ) ;
#53615 = DIRECTION ( 'NONE',  ( -1.000000000000000000, 0.000000000000000000, 0.000000000000000000 ) ) ;
#53616 =( BOUNDED_CURVE ( )  B_SPLINE_CURVE ( 2, ( #58206, #36750, #48402, #18346, #6708, #41648, #48037 ),
 .UNSPECIFIED., .F., .F. ) 
 B_SPLINE_CURVE_WITH_KNOTS ( ( 3, 2, 2, 3 ),
 ( 0.5926843883797354717, 0.5997400709749998171, 0.6067958365158829803, 0.6138516023186938453 ),
 .UNSPECIFIED. ) 
 CURVE ( )  GEOMETRIC_REPRESENTATION_ITEM ( )  RATIONAL_B_SPLINE_CURVE ( ( 0.9999968501007930888, 0.8660269787525570750, 1.000000000000000000, 0.8660254037844387076, 1.000000000000000000, 0.8660254037844387076, 1.000000000000000000 ) ) 
 REPRESENTATION_ITEM ( '' )  );
#53617 = DIRECTION ( 'NONE',  ( -0.6862798483830544471, -0.7273375899149802093, 0.000000000000000000 ) ) ;
#53618 = CIRCLE ( 'NONE', #2042, 16.00000000000000000 ) ;
#53619 = DIRECTION ( 'NONE',  ( 0.000000000000000000, -6.982962677686266711E-15, 1.000000000000000000 ) ) ;
#53620 = CARTESIAN_POINT ( 'NONE',  ( 93.67500000000001137, -207.7050326799711968, 84.81416666666666515 ) ) ;
#53621 = PRODUCT_DEFINITION ( 'UNKNOWN', '', #36381, #66452 ) ;
#53622 = EDGE_CURVE ( 'NONE', #14085, #3697, #52472, .T. ) ;
#53623 = VECTOR ( 'NONE', #30499, 1000.000000000000000 ) ;
#53624 = ORIENTED_EDGE ( 'NONE', *, *, #19671, .T. ) ;
#53625 = ORIENTED_EDGE ( 'NONE', *, *, #26665, .T. ) ;
#53626 = ORIENTED_EDGE ( 'NONE', *, *, #51458, .T. ) ;
#53627 = EDGE_LOOP ( 'NONE', ( #72994, #4016, #45525, #46623 ) ) ;
#53628 = CARTESIAN_POINT ( 'NONE',  ( -92.35000000000000853, -210.0000001051137701, 86.58687499784845443 ) ) ;
#53629 = SHAPE_REPRESENTATION_RELATIONSHIP ( 'NONE' , 'NONE' ,  #10045, #72270 ) ;
#53630 = CARTESIAN_POINT ( 'NONE',  ( -97.30629616937501680, 88.66845928578038638, 83.50447916753383026 ) ) ;
#53631 = VECTOR ( 'NONE', #41455, 1000.000000000000000 ) ;
#53632 = EDGE_CURVE ( 'NONE', #2660, #21827, #64509, .T. ) ;
#53633 = LINE ( 'NONE', #59280, #12520 ) ;
#53634 = AXIS2_PLACEMENT_3D ( 'NONE', #11506, #16418, #51359 ) ;
#53635 = CARTESIAN_POINT ( 'NONE',  ( 10.00000000000000000, 44.88180994100468268, -63.18004540532978552 ) ) ;
#53636 = CARTESIAN_POINT ( 'NONE',  ( 97.30629616937498838, -208.6684592857803011, 87.47322916753381605 ) ) ;
#53637 = CARTESIAN_POINT ( 'NONE',  ( 93.67499999999998295, 92.29496732002878900, 76.55916666666666970 ) ) ;
#53639 = ORIENTED_EDGE ( 'NONE', *, *, #32771, .T. ) ;
#53638 = EDGE_CURVE ( 'NONE', #52121, #70257, #16468, .T. ) ;
#53640 = CYLINDRICAL_SURFACE ( 'NONE', #34761, 82.00000000000000000 ) ;
#53641 = ORIENTED_EDGE ( 'NONE', *, *, #73405, .F. ) ;
#53642 = CARTESIAN_POINT ( 'NONE',  ( -92.35000000000002274, -211.5299782133524786, 85.18458333333332178 ) ) ;
#53643 = CIRCLE ( 'NONE', #25998, 32.00000000000000000 ) ;
#53644 = VERTEX_POINT ( 'NONE', #22647 ) ;
#53645 = CARTESIAN_POINT ( 'NONE',  ( -97.65000000000001990, 90.00000000000004263, 86.26937500173430351 ) ) ;
#53646 = EDGE_CURVE ( 'NONE', #8512, #27109, #23655, .T. ) ;
#53647 = CARTESIAN_POINT ( 'NONE',  ( 96.15314808468748708, 91.99731107132950569, 85.77989583420048803 ) ) ;
#53648 = DIRECTION ( 'NONE',  ( -1.000000000000000000, -0.000000000000000000, -0.000000000000000000 ) ) ;
#53649 = DIRECTION ( 'NONE',  ( 0.000000000000000000, -0.9945218953682740670, -0.1045284632676459352 ) ) ;
#53650 = CARTESIAN_POINT ( 'NONE',  ( -92.34999999999999432, -209.9999999999999716, 78.33187500173430351 ) ) ;
#53651 = DIRECTION ( 'NONE',  ( 2.603472992746261562E-14, 2.546204323184492723E-14, -1.000000000000000000 ) ) ;
#53652 = ORIENTED_EDGE ( 'NONE', *, *, #32179, .F. ) ;
#53653 = DIRECTION ( 'NONE',  ( -0.000000000000000000, -0.000000000000000000, 1.000000000000000000 ) ) ;
#53654 = LINE ( 'NONE', #65320, #2396 ) ;
#53655 = EDGE_LOOP ( 'NONE', ( #40616, #45052, #12718 ) ) ;
#53656 = AXIS2_PLACEMENT_3D ( 'NONE', #22090, #56684, #32979 ) ;
#53657 = ORIENTED_EDGE ( 'NONE', *, *, #6785, .T. ) ;
#53658 = DIRECTION ( 'NONE',  ( 0.000000000000000000, 0.9135454576426003115, 0.4067366430758017071 ) ) ;
#53659 = EDGE_CURVE ( 'NONE', #21226, #56853, #50044, .T. ) ;
#53660 = AXIS2_PLACEMENT_3D ( 'NONE', #966, #51689, #236 ) ;
#53661 = EDGE_CURVE ( 'NONE', #67107, #48097, #17371, .T. ) ;
#53662 = CARTESIAN_POINT ( 'NONE',  ( 0.000000000000000000, 0.000000000000000000, 0.000000000000000000 ) ) ;
#53663 = CARTESIAN_POINT ( 'NONE',  ( -97.64999999994218172, 89.99998877583867340, 75.47473230081648410 ) ) ;
#53664 = CARTESIAN_POINT ( 'NONE',  ( -96.15314808468745866, -211.9973110713294489, 88.63739583420048973 ) ) ;
#53665 = ORIENTED_EDGE ( 'NONE', *, *, #15302, .F. ) ;
#53666 = CARTESIAN_POINT ( 'NONE',  ( 0.000000000000000000, 0.000000000000000000, 0.000000000000000000 ) ) ;
#53667 = VERTEX_POINT ( 'NONE', #63249 ) ;
#53668 = EDGE_LOOP ( 'NONE', ( #68443, #14317, #31910, #48990 ) ) ;
#53669 = CARTESIAN_POINT ( 'NONE',  ( 10.00000000000000000, -5.202137450156655518, 37.22597642581156663 ) ) ;
#53670 = CARTESIAN_POINT ( 'NONE',  ( 10.00000000000000000, -63.18004540532994184, -44.88180994100446952 ) ) ;
#53671 = CARTESIAN_POINT ( 'NONE',  ( 5.000000000000000000, 36.13751322684419165, 21.40280677340384585 ) ) ;
#53672 = CARTESIAN_POINT ( 'NONE',  ( 96.15314808468748708, 91.99731107132950569, 82.44614583420046472 ) ) ;
#53673 = DIRECTION ( 'NONE',  ( 0.000000000000000000, 0.000000000000000000, 1.000000000000000000 ) ) ;
#53674 = CARTESIAN_POINT ( 'NONE',  ( 10.00000000000000000, -30.80686688397025108, 21.53537804866070715 ) ) ;
#53675 = CARTESIAN_POINT ( 'NONE',  ( -96.32500000000001705, 92.29496732002878900, 81.00416666666666288 ) ) ;
#53676 = LINE ( 'NONE', #59695, #30386 ) ;
#53677 = DIRECTION ( 'NONE',  ( 1.000000000000000000, -0.000000000000000000, -0.000000000000000000 ) ) ;
#53678 = CARTESIAN_POINT ( 'NONE',  ( 2.499999999999983569, -80.00000000000000000, -90.00000000000000000 ) ) ;
#53679 = DIRECTION ( 'NONE',  ( -1.000000000000000000, -0.000000000000000000, 0.000000000000000000 ) ) ;
#53680 = CARTESIAN_POINT ( 'NONE',  ( -10.00000000000000000, 0.000000000000000000, 0.000000000000000000 ) ) ;
#53681 = AXIS2_PLACEMENT_3D ( 'NONE', #67323, #27085, #15827 ) ;
#53682 = PLANE ( 'NONE',  #19353 ) ;
#53683 = ORIENTED_EDGE ( 'NONE', *, *, #1325, .F. ) ;
#53684 = CARTESIAN_POINT ( 'NONE',  ( -96.15314808468752972, 91.99731107132950569, 86.99697916753380866 ) ) ;
#53685 = DIRECTION ( 'NONE',  ( 1.000000000000000000, -0.000000000000000000, -0.000000000000000000 ) ) ;
#53686 = CIRCLE ( 'NONE', #23689, 31.99999999999998934 ) ;
#53687 = AXIS2_PLACEMENT_3D ( 'NONE', #61459, #9941, #54698 ) ;
#53688 = CARTESIAN_POINT ( 'NONE',  ( 97.64999999999999147, 90.00000000000002842, 90.00000000000000000 ) ) ;
#53689 = PRODUCT_DEFINITION_SHAPE ( 'NONE', 'NONE',  #74361 ) ;
#53690 = VECTOR ( 'NONE', #12441, 1000.000000000000000 ) ;
#53691 = EDGE_LOOP ( 'NONE', ( #37380, #43587, #70079, #72203 ) ) ;
#53692 = CARTESIAN_POINT ( 'NONE',  ( -235.0000123116479926, -117.0000000000000142, 2.500000000000000000 ) ) ;
#53693 = CARTESIAN_POINT ( 'NONE',  ( 92.35000000000000853, -209.9999999999999716, 77.93499999999998806 ) ) ;
#53694 = DIRECTION ( 'NONE',  ( 0.000000000000000000, 0.000000000000000000, -1.000000000000000000 ) ) ;
#53695 = EDGE_CURVE ( 'NONE', #69733, #68386, #39286, .T. ) ;
#53696 = CARTESIAN_POINT ( 'NONE',  ( 95.00000000000000000, -207.3369185715606307, 81.38781250086715602 ) ) ;
#53697 = VECTOR ( 'NONE', #33743, 1000.000000000000000 ) ;
#53698 = ORIENTED_EDGE ( 'NONE', *, *, #60199, .F. ) ;
#53699 = ADVANCED_FACE ( 'NONE', ( #56865 ), #6110, .T. ) ;
#53700 = ORIENTED_EDGE ( 'NONE', *, *, #72893, .T. ) ;
#53702 = EDGE_CURVE ( 'NONE', #21621, #72558, #29644, .T. ) ;
#53701 = VECTOR ( 'NONE', #14234, 1000.000000000000000 ) ;
#53703 = PLANE ( 'NONE',  #15226 ) ;
#53704 = EDGE_LOOP ( 'NONE', ( #59202, #15420, #66240, #31618 ) ) ;
#53705 = DIRECTION ( 'NONE',  ( 0.000000000000000000, 0.000000000000000000, 1.000000000000000000 ) ) ;
#53706 = DIRECTION ( 'NONE',  ( 0.000000000000000000, 0.000000000000000000, 1.000000000000000000 ) ) ;
#53707 = ORIENTED_EDGE ( 'NONE', *, *, #28113, .F. ) ;
#53708 = CARTESIAN_POINT ( 'NONE',  ( 97.30629616937498838, -211.3315407142195852, 80.54114583420049200 ) ) ;
#53709 = EDGE_CURVE ( 'NONE', #48987, #41411, #29012, .T. ) ;
#53710 = ORIENTED_EDGE ( 'NONE', *, *, #43186, .T. ) ;
#53711 = CARTESIAN_POINT ( 'NONE',  ( -7.499999999999973355, 62.04836822995428491, -275.0000000000000000 ) ) ;
#53712 = ORIENTED_EDGE ( 'NONE', *, *, #38527, .F. ) ;
#53713 = EDGE_LOOP ( 'NONE', ( #42003, #6879, #66483, #7936 ) ) ;
#53714 = CARTESIAN_POINT ( 'NONE',  ( 10.00000000000000000, -17.67226234102849958, 33.17418723428301774 ) ) ;
#53715 = DIRECTION ( 'NONE',  ( 0.000000000000000000, 0.000000000000000000, 1.000000000000000000 ) ) ;
#53716 = ORIENTED_EDGE ( 'NONE', *, *, #42295, .F. ) ;
#53717 = LINE ( 'NONE', #13120, #5345 ) ;
#53718 = CARTESIAN_POINT ( 'NONE',  ( 93.67500000000001137, -212.2949673200287179, 83.83520833506763381 ) ) ;
#53719 = CARTESIAN_POINT ( 'NONE',  ( 93.67499999999998295, 92.29496732002878900, 84.17916666666666003 ) ) ;
#53720 = ORIENTED_EDGE ( 'NONE', *, *, #47750, .T. ) ;
#53721 = CARTESIAN_POINT ( 'NONE',  ( 10.00000000000000000, -10.74501242461308159, 35.92658777277507909 ) ) ;
#53722 = LINE ( 'NONE', #2641, #11676 ) ;
#53723 = ORIENTED_EDGE ( 'NONE', *, *, #42173, .F. ) ;
#53724 = ORIENTED_EDGE ( 'NONE', *, *, #537, .T. ) ;
#53725 = CARTESIAN_POINT ( 'NONE',  ( -97.30629616937501680, 90.00000000000004263, 87.89656250086714806 ) ) ;
#53726 = EDGE_CURVE ( 'NONE', #44676, #105, #34286, .T. ) ;
#53727 = VECTOR ( 'NONE', #19073, 1000.000000000000000 ) ;
#53728 = CARTESIAN_POINT ( 'NONE',  ( 97.30629616937498838, 88.66845928578037217, 85.46239583420047836 ) ) ;
#53729 = ORIENTED_EDGE ( 'NONE', *, *, #67831, .T. ) ;
#53731 = CARTESIAN_POINT ( 'NONE',  ( 92.34999999999999432, 91.52997821335252127, 87.48645833506763836 ) ) ;
#53730 = AXIS2_PLACEMENT_3D ( 'NONE', #3678, #66808, #55529 ) ;
#53732 = EDGE_LOOP ( 'NONE', ( #53260, #18766, #1751, #65374 ) ) ;
#53733 = DIRECTION ( 'NONE',  ( -0.000000000000000000, -0.000000000000000000, 1.000000000000000000 ) ) ;
#53734 = VERTEX_POINT ( 'NONE', #40681 ) ;
#53735 = EDGE_LOOP ( 'NONE', ( #71905, #45038, #60119, #33282 ) ) ;
#53736 = CIRCLE ( 'NONE', #17721, 1.500000000000000000 ) ;
#53737 = EDGE_LOOP ( 'NONE', ( #25055, #29649, #66571, #68898 ) ) ;
#53738 = AXIS2_PLACEMENT_3D ( 'NONE', #40749, #12160, #59145 ) ;
#53739 = DIRECTION ( 'NONE',  ( 0.000000000000000000, -0.4999999999999930611, 0.8660254037844425934 ) ) ;
#53740 = CARTESIAN_POINT ( 'NONE',  ( 21.85433023846371370, -135.0628101570779620, 5.500000000000000000 ) ) ;
#53741 = CARTESIAN_POINT ( 'NONE',  ( -96.32500000000001705, 92.29496732002878900, 83.54416666666666913 ) ) ;
#53742 = ADVANCED_FACE ( 'NONE', ( #57230 ), #16629, .F. ) ;
#53743 = ORIENTED_EDGE ( 'NONE', *, *, #64698, .T. ) ;
#53744 = ADVANCED_FACE ( 'NONE', ( #63627 ), #51580, .T. ) ;
#53745 = CARTESIAN_POINT ( 'NONE',  ( 96.92110976540138267, 91.30563282057313756, 74.79348190356853365 ) ) ;
#53746 = FACE_OUTER_BOUND ( 'NONE', #44369, .T. ) ;
#53747 = ORIENTED_EDGE ( 'NONE', *, *, #29627, .F. ) ;
#53748 = DIRECTION ( 'NONE',  ( 0.000000000000000000, 0.000000000000000000, 1.000000000000000000 ) ) ;
#53749 = CARTESIAN_POINT ( 'NONE',  ( -94.99999999999997158, -212.6630814284392557, 83.45156250086714067 ) ) ;
#53750 = ORIENTED_EDGE ( 'NONE', *, *, #30011, .T. ) ;
#53751 = EDGE_CURVE ( 'NONE', #43669, #71014, #23027, .T. ) ;
#53752 = CARTESIAN_POINT ( 'NONE',  ( 0.000000000000000000, -71.27951684758045303, 30.41916302227090085 ) ) ;
#53753 = DIRECTION ( 'NONE',  ( 1.000000000000000000, 0.000000000000000000, 0.000000000000000000 ) ) ;
#53754 = CARTESIAN_POINT ( 'NONE',  ( 4.250000000000000000, -13.95926121303099343, -1.199999999999999956 ) ) ;
#53755 = DIRECTION ( 'NONE',  ( 0.000000000000000000, 0.000000000000000000, 1.000000000000000000 ) ) ;
#53756 = DIRECTION ( 'NONE',  ( 0.000000000000000000, 0.4539904997395414754, 0.8910065241883706744 ) ) ;
#53757 = AXIS2_PLACEMENT_3D ( 'NONE', #30676, #6298, #1434 ) ;
#53759 = VECTOR ( 'NONE', #46531, 999.9999999999998863 ) ;
#53758 = CARTESIAN_POINT ( 'NONE',  ( -2.499999999999969802, 76.30000000000001137, -204.9999999999999716 ) ) ;
#53760 = CARTESIAN_POINT ( 'NONE',  ( -94.99999999999997158, -206.9400435732949575, 89.84125000000000227 ) ) ;
#53761 = LINE ( 'NONE', #25198, #29106 ) ;
#53762 = CIRCLE ( 'NONE', #71777, 82.00000000000000000 ) ;
#53763 = DIRECTION ( 'NONE',  ( -1.000000000000000000, 0.000000000000000000, 0.000000000000000000 ) ) ;
#53764 = CARTESIAN_POINT ( 'NONE',  ( -95.00000000000002842, 87.33691857156074434, 75.19656250086714522 ) ) ;
#53765 = CARTESIAN_POINT ( 'NONE',  ( 15.00000000000000000, -13.04903810567646971, 19.60159698893442481 ) ) ;
#53766 = LINE ( 'NONE', #43254, #20618 ) ;
#53767 = CIRCLE ( 'NONE', #12971, 31.99999999999999289 ) ;
#53768 = DIRECTION ( 'NONE',  ( -1.000000000000000000, 0.000000000000000000, 0.000000000000000000 ) ) ;
#53769 = CARTESIAN_POINT ( 'NONE',  ( 10.00000000000000000, -55.20638768913797634, 51.02545421589302777 ) ) ;
#53770 = CARTESIAN_POINT ( 'NONE',  ( 5.000000000000002665, 81.50828551894240093, -8.966570791699803422 ) ) ;
#53771 = FACE_OUTER_BOUND ( 'NONE', #73672, .T. ) ;
#53772 = CARTESIAN_POINT ( 'NONE',  ( 11.99999999999999822, 0.000000000000000000, 0.000000000000000000 ) ) ;
#53773 = CARTESIAN_POINT ( 'NONE',  ( -96.32499999999996021, -207.7050326799711968, 86.71916666666666629 ) ) ;
#53774 = FACE_OUTER_BOUND ( 'NONE', #72205, .T. ) ;
#53775 = VERTEX_POINT ( 'NONE', #23747 ) ;
#53776 = CIRCLE ( 'NONE', #52546, 31.99999999999998579 ) ;
#53777 = CARTESIAN_POINT ( 'NONE',  ( 5.000000000000000000, -39.04073710021356192, 15.48615015657568073 ) ) ;
#53778 = CARTESIAN_POINT ( 'NONE',  ( 93.67500000000001137, -212.2949673200287179, 78.12020833506763040 ) ) ;
#53779 = DIRECTION ( 'NONE',  ( -1.427937372958396784E-15, 1.000000000000000000, -1.078060571631604545E-14 ) ) ;
#53780 = CIRCLE ( 'NONE', #67029, 42.00000000000000000 ) ;
#53781 = CIRCLE ( 'NONE', #38166, 77.49899999999999523 ) ;
#53782 = DIRECTION ( 'NONE',  ( -7.632783294297813165E-16, -1.065814103640131188E-14, -1.000000000000000000 ) ) ;
#53783 = ADVANCED_FACE ( 'NONE', ( #5002 ), #27904, .F. ) ;
#53784 = CIRCLE ( 'NONE', #30971, 16.00000000000000000 ) ;
#53785 = CIRCLE ( 'NONE', #8114, 37.49900000000000944 ) ;
#53786 = EDGE_CURVE ( 'NONE', #40782, #11821, #34735, .T. ) ;
#53787 = ORIENTED_EDGE ( 'NONE', *, *, #50938, .F. ) ;
#53789 = EDGE_CURVE ( 'NONE', #46404, #11277, #53795, .T. ) ;
#53788 = CARTESIAN_POINT ( 'NONE',  ( 0.000000000000000000, -44.99326035066006568, -68.55367621811190304 ) ) ;
#53790 = CARTESIAN_POINT ( 'NONE',  ( 20.10151712711562766, -102.7321394148470830, -2.500000000000000000 ) ) ;
#53791 = VERTEX_POINT ( 'NONE', #13567 ) ;
#53792 = CARTESIAN_POINT ( 'NONE',  ( 96.15314808468750130, -211.9973110713294489, 86.04447916753380809 ) ) ;
#53793 = CARTESIAN_POINT ( 'NONE',  ( 96.15314808468750130, -211.9973110713294489, 88.10822916753382117 ) ) ;
#53794 = ORIENTED_EDGE ( 'NONE', *, *, #73915, .T. ) ;
#53795 = LINE ( 'NONE', #2710, #35662 ) ;
#53796 = EDGE_CURVE ( 'NONE', #23489, #40541, #10450, .T. ) ;
#53797 = VERTEX_POINT ( 'NONE', #70705 ) ;
#53798 = CARTESIAN_POINT ( 'NONE',  ( 10.00000000000000000, 10.74501242461333028, -35.92658777277499382 ) ) ;
#53799 = EDGE_LOOP ( 'NONE', ( #34977, #71714, #12320, #32372 ) ) ;
#53800 = CARTESIAN_POINT ( 'NONE',  ( -95.00000000000002842, 87.33691857156074434, 78.53031250086715431 ) ) ;
#53801 = AXIS2_PLACEMENT_3D ( 'NONE', #42538, #13944, #58719 ) ;
#53802 = ORIENTED_EDGE ( 'NONE', *, *, #6525, .T. ) ;
#53803 = ORIENTED_EDGE ( 'NONE', *, *, #34875, .T. ) ;
#53804 = DIRECTION ( 'NONE',  ( 0.000000000000000000, 0.000000000000000000, -1.000000000000000000 ) ) ;
#53805 = CIRCLE ( 'NONE', #33408, 15.99999999999999822 ) ;
#53806 = ORIENTED_EDGE ( 'NONE', *, *, #46619, .F. ) ;
#53807 = DIRECTION ( 'NONE',  ( 0.000000000000000000, 0.7604059656000322631, -0.6494480483301821039 ) ) ;
#53808 = CARTESIAN_POINT ( 'NONE',  ( 25.38712131070745315, -112.4010479962415872, -2.500000000000000000 ) ) ;
#53809 = AXIS2_PLACEMENT_3D ( 'NONE', #52770, #30928, #48241 ) ;
#53810 = VERTEX_POINT ( 'NONE', #36498 ) ;
#53811 = CYLINDRICAL_SURFACE ( 'NONE', #49028, 2.649999999999999467 ) ;
#53812 = VERTEX_POINT ( 'NONE', #53432 ) ;
#53813 = MECHANICAL_DESIGN_GEOMETRIC_PRESENTATION_REPRESENTATION (  '', ( #58649 ), #2233 ) ;
#53814 = CARTESIAN_POINT ( 'NONE',  ( 0.000000000000000000, 20.41045688087824317, 72.35160999960824313 ) ) ;
#53815 = EDGE_CURVE ( 'NONE', #1543, #29672, #54886, .T. ) ;
#53816 = ORIENTED_EDGE ( 'NONE', *, *, #42039, .T. ) ;
#53817 = ORIENTED_EDGE ( 'NONE', *, *, #38896, .T. ) ;
#53818 = VERTEX_POINT ( 'NONE', #1603 ) ;
#53819 = CARTESIAN_POINT ( 'NONE',  ( 97.30629616937498838, -211.3315407142195852, 77.84239583420045960 ) ) ;
#53820 = CARTESIAN_POINT ( 'NONE',  ( -99.99999999999997158, -214.9999999999999716, 90.00000000000000000 ) ) ;
#53821 = ITEM_DEFINED_TRANSFORMATION ( 'NONE', 'NONE', #14758,  #43395 ) ;
#53822 = LINE ( 'NONE', #41802, #10152 ) ;
#53823 = ORIENTED_EDGE ( 'NONE', *, *, #72883, .T. ) ;
#53824 = DIRECTION ( 'NONE',  ( -1.000000000000000000, 0.000000000000000000, -0.000000000000000000 ) ) ;
#53825 = DIRECTION ( 'NONE',  ( 0.000000000000000000, 0.000000000000000000, 1.000000000000000000 ) ) ;
#53826 = CARTESIAN_POINT ( 'NONE',  ( 11.99999999999999822, 76.41127070299273782, 12.93880638057342836 ) ) ;
#53827 = DIRECTION ( 'NONE',  ( -1.000000000000000000, 0.000000000000000000, -0.000000000000000000 ) ) ;
#53828 = DIRECTION ( 'NONE',  ( -0.000000000000000000, 0.000000000000000000, 1.000000000000000000 ) ) ;
#53829 = CARTESIAN_POINT ( 'NONE',  ( -92.69370383062498320, -211.3315407142195852, 81.01739583420048518 ) ) ;
#53830 = CARTESIAN_POINT ( 'NONE',  ( -92.69370383062502583, 88.66845928578038638, 79.90614583420048689 ) ) ;
#53831 = EDGE_CURVE ( 'NONE', #53610, #60557, #26061, .T. ) ;
#53832 = ORIENTED_EDGE ( 'NONE', *, *, #29283, .T. ) ;
#53833 = EDGE_CURVE ( 'NONE', #72774, #34470, #68099, .T. ) ;
#53834 = CARTESIAN_POINT ( 'NONE',  ( 92.69370383062498320, 91.33154071421968467, 80.69989583420048973 ) ) ;
#53835 =( BOUNDED_CURVE ( )  B_SPLINE_CURVE ( 2, ( #29652, #53, #17285, #18381, #22944, #23305, #46233 ),
 .UNSPECIFIED., .F., .F. ) 
 B_SPLINE_CURVE_WITH_KNOTS ( ( 3, 2, 2, 3 ),
 ( 0.1041666666666670182, 0.1111111111111114103, 0.1180555555555558161, 0.1250000000000002220 ),
 .UNSPECIFIED. ) 
 CURVE ( )  GEOMETRIC_REPRESENTATION_ITEM ( )  RATIONAL_B_SPLINE_CURVE ( ( 0.9999999999999933387, 0.8660254037844453689, 1.000000000000000000, 0.8660254037844387076, 1.000000000000000000, 0.8660254037844343777, 1.000000000000004219 ) ) 
 REPRESENTATION_ITEM ( '' )  );
#53836 = ORIENTED_EDGE ( 'NONE', *, *, #21023, .F. ) ;
#53837 = DIRECTION ( 'NONE',  ( -0.000000000000000000, -0.9135454576426006446, 0.4067366430758008744 ) ) ;
#53838 = DIRECTION ( 'NONE',  ( 0.000000000000000000, 0.5877852522924696954, 0.8090169943749498938 ) ) ;
#53839 = DIRECTION ( 'NONE',  ( 0.000000000000000000, 0.000000000000000000, 1.000000000000000000 ) ) ;
#53840 = DIRECTION ( 'NONE',  ( 1.000000000000000000, -0.000000000000000000, 0.000000000000000000 ) ) ;
#53841 = CARTESIAN_POINT ( 'NONE',  ( 6.000000000000000000, 71.87247863392471459, -39.47590169984771080 ) ) ;
#53842 = CARTESIAN_POINT ( 'NONE',  ( -97.30629616937497417, -211.3315407142195852, 83.34572916753381833 ) ) ;
#53843 = AXIS2_PLACEMENT_3D ( 'NONE', #64418, #58029, #46383 ) ;
#53844 = VECTOR ( 'NONE', #1399, 1000.000000000000000 ) ;
#53845 = CARTESIAN_POINT ( 'NONE',  ( 6.000000000000000000, 8.966570791701871102, -81.50828551894218776 ) ) ;
#53846 = DIRECTION ( 'NONE',  ( -0.000000000000000000, -0.000000000000000000, -1.000000000000000000 ) ) ;
#53847 = DIRECTION ( 'NONE',  ( 0.000000000000000000, 0.000000000000000000, 1.000000000000000000 ) ) ;
#53848 = VERTEX_POINT ( 'NONE', #2345 ) ;
#53849 = AXIS2_PLACEMENT_3D ( 'NONE', #27497, #21108, #61357 ) ;
#53850 = ORIENTED_EDGE ( 'NONE', *, *, #73086, .T. ) ;
#53851 = CARTESIAN_POINT ( 'NONE',  ( 10.00000000000000000, -62.50884508063395373, -41.76106447765554464 ) ) ;
#53852 = AXIS2_PLACEMENT_3D ( 'NONE', #2317, #59422, #19191 ) ;
#53853 = CARTESIAN_POINT ( 'NONE',  ( -95.00000000000002842, 93.05995642670501411, 75.23624999999999829 ) ) ;
#53854 = CARTESIAN_POINT ( 'NONE',  ( 0.000000000000000000, 0.000000000000000000, 0.000000000000000000 ) ) ;
#53855 = CARTESIAN_POINT ( 'NONE',  ( -97.30629616937501680, 90.00000000000004263, 83.92781250086714806 ) ) ;
#53856 = DIRECTION ( 'NONE',  ( 0.000000000000000000, -0.07845909572783055230, -0.9969173337331290741 ) ) ;
#53857 = DIRECTION ( 'NONE',  ( -1.000000000000000000, 0.000000000000000000, 0.000000000000000000 ) ) ;
#53858 = CARTESIAN_POINT ( 'NONE',  ( -0.2999999999999964362, 0.000000000000000000, 0.000000000000000000 ) ) ;
#53859 = VERTEX_POINT ( 'NONE', #63985 ) ;
#53860 = CARTESIAN_POINT ( 'NONE',  ( -97.30629616937501680, 88.66845928578038638, 75.09072916753382287 ) ) ;
#53861 = AXIS2_PLACEMENT_3D ( 'NONE', #14473, #3226, #25394 ) ;
#53862 = DIRECTION ( 'NONE',  ( -1.000000000000000000, -0.000000000000000000, -0.000000000000000000 ) ) ;
#53863 = AXIS2_PLACEMENT_3D ( 'NONE', #6041, #52244, #27832 ) ;
#53864 = DIRECTION ( 'NONE',  ( 0.000000000000000000, 0.000000000000000000, -1.000000000000000000 ) ) ;
#53865 = CARTESIAN_POINT ( 'NONE',  ( 0.000000000000000000, -62.50329211542465657, 41.76937507738766442 ) ) ;
#53866 = CARTESIAN_POINT ( 'NONE',  ( 22.94323693612312809, -114.6983135802921083, 5.500000000000000000 ) ) ;
#53867 = DIRECTION ( 'NONE',  ( -1.000000000000000000, -0.000000000000000000, -0.000000000000000000 ) ) ;
#53868 = CARTESIAN_POINT ( 'NONE',  ( -96.15314808468747287, -208.0026889286704943, 83.34572916753383254 ) ) ;
#53869 = SURFACE_STYLE_USAGE ( .BOTH. , #72260 ) ;
#53870 = AXIS2_PLACEMENT_3D ( 'NONE', #41416, #499, #57970 ) ;
#53871 = AXIS2_PLACEMENT_3D ( 'NONE', #26407, #66639, #20762 ) ;
#53872 = CARTESIAN_POINT ( 'NONE',  ( -10.00000000000000000, 0.000000000000000000, 0.000000000000000000 ) ) ;
#53873 = ADVANCED_FACE ( 'NONE', ( #12462 ), #34281, .F. ) ;
#53874 = AXIS2_PLACEMENT_3D ( 'NONE', #47973, #9217, #8859 ) ;
#53875 = CARTESIAN_POINT ( 'NONE',  ( 2.500000000000004441, -90.00000000000000000, -279.9999999999999432 ) ) ;
#53876 = EDGE_CURVE ( 'NONE', #46530, #3129, #42881, .T. ) ;
#53877 = CARTESIAN_POINT ( 'NONE',  ( -93.84685191531248449, -208.0026889286704943, 76.25489583420049655 ) ) ;
#53878 = DIRECTION ( 'NONE',  ( -1.000000000000000000, 0.000000000000000000, 0.000000000000000000 ) ) ;
#53879 = VERTEX_POINT ( 'NONE', #41887 ) ;
#53880 = FACE_OUTER_BOUND ( 'NONE', #7928, .T. ) ;
#53881 = DIRECTION ( 'NONE',  ( 1.000000000000000000, 0.000000000000000000, -0.000000000000000000 ) ) ;
#53882 = CARTESIAN_POINT ( 'NONE',  ( 0.000000000000000000, -68.27212725128254078, -31.46837873495049465 ) ) ;
#53883 = EDGE_CURVE ( 'NONE', #27833, #38563, #69344, .T. ) ;
#53884 = EDGE_CURVE ( 'NONE', #48148, #48900, #58432, .T. ) ;
#53885 = CARTESIAN_POINT ( 'NONE',  ( -6.880223345695647197, -142.5202692415819854, 2.500000000000000000 ) ) ;
#53886 = CARTESIAN_POINT ( 'NONE',  ( 93.84685191531249870, -208.0026889286704943, 89.06072916753382174 ) ) ;
#53887 = ORIENTED_EDGE ( 'NONE', *, *, #42339, .F. ) ;
#53888 = AXIS2_PLACEMENT_3D ( 'NONE', #26819, #54302, #33572 ) ;
#53889 = FACE_OUTER_BOUND ( 'NONE', #17179, .T. ) ;
#53890 = DIRECTION ( 'NONE',  ( 0.000000000000000000, 0.000000000000000000, 1.000000000000000000 ) ) ;
#53891 = PRESENTATION_STYLE_ASSIGNMENT (( #71160 ) ) ;
#53892 = ORIENTED_EDGE ( 'NONE', *, *, #14922, .F. ) ;
#53893 = AXIS2_PLACEMENT_3D ( 'NONE', #21536, #16276, #38099 ) ;
#53894 = CARTESIAN_POINT ( 'NONE',  ( 2.874421927457452952, -143.3717286177755739, 5.500000000000000000 ) ) ;
#53895 = EDGE_LOOP ( 'NONE', ( #32990, #29680, #45954 ) ) ;
#53896 = CIRCLE ( 'NONE', #62335, 16.00000000000000000 ) ;
#53897 = AXIS2_PLACEMENT_3D ( 'NONE', #70304, #18808, #36113 ) ;
#53898 = EDGE_CURVE ( 'NONE', #28347, #39126, #13308, .T. ) ;
#53899 = PLANE ( 'NONE',  #29816 ) ;
#53900 = VECTOR ( 'NONE', #26297, 1000.000000000000114 ) ;
#53901 = VERTEX_POINT ( 'NONE', #46055 ) ;
#53902 = VERTEX_POINT ( 'NONE', #7674 ) ;
#53903 = VECTOR ( 'NONE', #9770, 1000.000000000000000 ) ;
#53904 = ORIENTED_EDGE ( 'NONE', *, *, #50860, .F. ) ;
#53905 = DIRECTION ( 'NONE',  ( 1.000000000000000000, 0.000000000000000000, 0.000000000000000000 ) ) ;
#53906 = ORIENTED_EDGE ( 'NONE', *, *, #69096, .F. ) ;
#53907 = EDGE_CURVE ( 'NONE', #69802, #49839, #12858, .T. ) ;
#53908 = EDGE_LOOP ( 'NONE', ( #63987, #4025, #59756, #3427 ) ) ;
#53909 = CARTESIAN_POINT ( 'NONE',  ( 93.84685191531248449, 88.00268892867053694, 80.38239583420048007 ) ) ;
#53910 = FACE_OUTER_BOUND ( 'NONE', #5601, .T. ) ;
#53911 = EDGE_CURVE ( 'NONE', #55837, #5520, #70073, .T. ) ;
#53912 = DIRECTION ( 'NONE',  ( 0.000000000000000000, 0.000000000000000000, 1.000000000000000000 ) ) ;
#53913 = AXIS2_PLACEMENT_3D ( 'NONE', #7985, #25285, #13980 ) ;
#53914 = EDGE_LOOP ( 'NONE', ( #60076, #44483, #12476, #71374 ) ) ;
#53916 = ORIENTED_EDGE ( 'NONE', *, *, #34135, .F. ) ;
#53915 = AXIS2_PLACEMENT_3D ( 'NONE', #71759, #26275, #55598 ) ;
#53917 = ORIENTED_EDGE ( 'NONE', *, *, #49389, .T. ) ;
#53918 = DIRECTION ( 'NONE',  ( 0.000000000000000000, 0.000000000000000000, 1.000000000000000000 ) ) ;
#53920 = ADVANCED_FACE ( 'NONE', ( #29848 ), #47165, .T. ) ;
#53919 = ORIENTED_EDGE ( 'NONE', *, *, #47430, .F. ) ;
#53921 = ADVANCED_FACE ( 'NONE', ( #18577 ), #40790, .F. ) ;
#53922 = VECTOR ( 'NONE', #1596, 1000.000000000000000 ) ;
#53923 = CIRCLE ( 'NONE', #41896, 5.000000000000000000 ) ;
#53924 = DIRECTION ( 'NONE',  ( 0.000000000000000000, 0.000000000000000000, 1.000000000000000000 ) ) ;
#53925 = CARTESIAN_POINT ( 'NONE',  ( -21.33958957442910886, -129.9559990355020034, 5.500000000000000000 ) ) ;
#53926 = CARTESIAN_POINT ( 'NONE',  ( -0.0004442498512760095037, 0.001194404164628348752, -49.00000000000000000 ) ) ;
#53927 = CARTESIAN_POINT ( 'NONE',  ( -10.00000000000000000, 0.000000000000000000, 0.000000000000000000 ) ) ;
#53928 = DIRECTION ( 'NONE',  ( -1.000000000000000000, -0.000000000000000000, 0.000000000000000000 ) ) ;
#53929 = LINE ( 'NONE', #41902, #9532 ) ;
#53930 = CIRCLE ( 'NONE', #10719, 32.00000000000000000 ) ;
#53931 = DIRECTION ( 'NONE',  ( 0.000000000000000000, 0.000000000000000000, 1.000000000000000000 ) ) ;
#53932 = AXIS2_PLACEMENT_3D ( 'NONE', #71060, #19200, #59805 ) ;
#53933 = CARTESIAN_POINT ( 'NONE',  ( -92.34999999999999432, -209.9999999999999716, 74.52187500173430124 ) ) ;
#53934 = DIRECTION ( 'NONE',  ( 1.000000000000000000, 0.000000000000000000, 0.000000000000000000 ) ) ;
#53935 = ADVANCED_FACE ( 'NONE', ( #64456 ), #17840, .T. ) ;
#53937 = CARTESIAN_POINT ( 'NONE',  ( -95.00000000000002842, 93.05995642670501411, 76.58562500173430010 ) ) ;
#53936 = CARTESIAN_POINT ( 'NONE',  ( 96.32499999999998863, 87.70503267997126784, 76.95604166840095672 ) ) ;
#53938 = AXIS2_PLACEMENT_3D ( 'NONE', #7388, #24667, #36315 ) ;
#53939 = EDGE_LOOP ( 'NONE', ( #60312, #18320, #20159, #18125 ) ) ;
#53940 = CARTESIAN_POINT ( 'NONE',  ( 96.15314808468748708, 88.00268892867053694, 76.67822916753381435 ) ) ;
#53941 = CARTESIAN_POINT ( 'NONE',  ( 92.34999999999999432, 91.52997821335252127, 82.32708333333334849 ) ) ;
#53942 = DIRECTION ( 'NONE',  ( 1.000000000000000000, 0.000000000000000000, 0.000000000000000000 ) ) ;
#53943 = DIRECTION ( 'NONE',  ( -1.000000000000000000, 0.000000000000000000, 0.000000000000000000 ) ) ;
#53944 = DIRECTION ( 'NONE',  ( -1.000000000000000000, -0.000000000000000000, -0.000000000000000000 ) ) ;
#53945 = EDGE_CURVE ( 'NONE', #47197, #62527, #14035, .T. ) ;
#53946 = CARTESIAN_POINT ( 'NONE',  ( -13.05994868825747446, -139.5943292883446532, 5.500000000000000000 ) ) ;
#53947 = ORIENTED_EDGE ( 'NONE', *, *, #8909, .F. ) ;
#53948 = CARTESIAN_POINT ( 'NONE',  ( 10.00000000000000000, 0.000000000000000000, 0.000000000000000000 ) ) ;
#53949 = CARTESIAN_POINT ( 'NONE',  ( 1.560000000000000053, 0.000000000000000000, 2.999999999999998668 ) ) ;
#53950 = ORIENTED_EDGE ( 'NONE', *, *, #54236, .F. ) ;
#53951 = EDGE_LOOP ( 'NONE', ( #52076, #30507, #47892, #40567 ) ) ;
#53952 = VECTOR ( 'NONE', #25995, 1000.000000000000000 ) ;
#53953 = DIRECTION ( 'NONE',  ( 0.000000000000000000, 0.000000000000000000, 1.000000000000000000 ) ) ;
#53954 = CARTESIAN_POINT ( 'NONE',  ( 92.35000000000000853, -209.9999999999999716, 83.01499999999998636 ) ) ;
#53955 = DIRECTION ( 'NONE',  ( 0.000000000000000000, 0.000000000000000000, -1.000000000000000000 ) ) ;
#53956 = DIRECTION ( 'NONE',  ( -1.000000000000000000, -0.000000000000000000, -0.000000000000000000 ) ) ;
#53957 = DIRECTION ( 'NONE',  ( 0.000000000000000000, 0.4539904997395413089, 0.8910065241883705633 ) ) ;
#53958 = CARTESIAN_POINT ( 'NONE',  ( -97.30629616937497417, -208.6684592857803011, 75.14364583420049826 ) ) ;
#53959 = CIRCLE ( 'NONE', #3518, 16.00000000000000000 ) ;
#53960 = ORIENTED_EDGE ( 'NONE', *, *, #9131, .F. ) ;
#53961 = VECTOR ( 'NONE', #27248, 1000.000000000000000 ) ;
#53962 = AXIS2_PLACEMENT_3D ( 'NONE', #69861, #11602, #57861 ) ;
#53963 = CARTESIAN_POINT ( 'NONE',  ( 10.00000000000000000, 41.91543099594818500, -2.663952781846293139 ) ) ;
#53964 = DIRECTION ( 'NONE',  ( 1.000000000000000000, 0.000000000000000000, -0.000000000000000000 ) ) ;
#53965 = VECTOR ( 'NONE', #33709, 1000.000000000000000 ) ;
#53966 = CARTESIAN_POINT ( 'NONE',  ( 0.000000000000000000, -35.91791733033427647, -68.67312586195032509 ) ) ;
#53967 = CARTESIAN_POINT ( 'NONE',  ( -92.35000000000000853, -210.0000001051137701, 86.58687499784845443 ) ) ;
#53968 = CIRCLE ( 'NONE', #71915, 16.00000000000000000 ) ;
#53969 = DIRECTION ( 'NONE',  ( 1.000000000000000000, -0.000000000000000000, -0.000000000000000000 ) ) ;
#53970 = FACE_OUTER_BOUND ( 'NONE', #21345, .T. ) ;
#53971 = DIRECTION ( 'NONE',  ( -1.000000000000000000, -0.000000000000000000, -0.000000000000000000 ) ) ;
#53972 = DIRECTION ( 'NONE',  ( -1.000000000000000000, -0.000000000000000000, 0.000000000000000000 ) ) ;
#53973 = CARTESIAN_POINT ( 'NONE',  ( 96.15314808468748708, 88.00268892867053694, 84.29822916753381890 ) ) ;
#53974 = CARTESIAN_POINT ( 'NONE',  ( -97.30629616937497417, -211.3315407142195852, 87.94947916753382344 ) ) ;
#53975 = DIRECTION ( 'NONE',  ( 0.5200609990133008287, 0.8541291221503266584, -0.000000000000000000 ) ) ;
#53976 = AXIS2_PLACEMENT_3D ( 'NONE', #29234, #73619, #16118 ) ;
#53977 = ORIENTED_EDGE ( 'NONE', *, *, #67461, .T. ) ;
#53978 = LINE ( 'NONE', #2522, #32893 ) ;
#53979 = CARTESIAN_POINT ( 'NONE',  ( -92.34999999999999432, -211.5299782133524502, 82.00958333333332462 ) ) ;
#53980 = ADVANCED_FACE ( 'NONE', ( #19684 ), #2460, .T. ) ;
#53981 = CARTESIAN_POINT ( 'NONE',  ( -93.84685191531252713, 88.00268892867056536, 76.51947916753380241 ) ) ;
#53982 = VECTOR ( 'NONE', #25716, 1000.000000000000000 ) ;
#53983 = CIRCLE ( 'NONE', #5970, 37.49900000000000233 ) ;
#53984 = ADVANCED_FACE ( 'NONE', ( #2077 ), #3540, .T. ) ;
#53985 = VECTOR ( 'NONE', #1346, 1000.000000000000000 ) ;
#53986 = EDGE_CURVE ( 'NONE', #58705, #2902, #71557, .T. ) ;
#53987 = AXIS2_PLACEMENT_3D ( 'NONE', #33728, #22453, #40475 ) ;
#53988 = EDGE_CURVE ( 'NONE', #23400, #57437, #67451, .T. ) ;
#53989 = CARTESIAN_POINT ( 'NONE',  ( 93.84685191531249870, -208.0026889286704943, 85.09197916753380753 ) ) ;
#53990 = EDGE_LOOP ( 'NONE', ( #44513, #5459, #49299 ) ) ;
#53991 = ORIENTED_EDGE ( 'NONE', *, *, #58678, .T. ) ;
#53992 = ORIENTED_EDGE ( 'NONE', *, *, #10696, .F. ) ;
#53993 = DIRECTION ( 'NONE',  ( 0.000000000000000000, 0.3090169943749482839, -0.9510565162951533091 ) ) ;
#53994 = CARTESIAN_POINT ( 'NONE',  ( 1.560000000000000053, 0.000000000000000000, 0.000000000000000000 ) ) ;
#53995 = EDGE_CURVE ( 'NONE', #22794, #58538, #31861, .T. ) ;
#53996 = ORIENTED_EDGE ( 'NONE', *, *, #1091, .F. ) ;
#53997 = ADVANCED_FACE ( 'NONE', ( #2812 ), #54288, .F. ) ;
#53998 = CYLINDRICAL_SURFACE ( 'NONE', #43236, 16.00000000000000000 ) ;
#53999 = CARTESIAN_POINT ( 'NONE',  ( 92.69370383062501162, -209.9999999999999716, 79.64156250086715261 ) ) ;
#54000 = FACE_OUTER_BOUND ( 'NONE', #21062, .T. ) ;
#54001 = DIRECTION ( 'NONE',  ( -0.5200609990132993854, -0.8541291221503274356, 0.000000000000000000 ) ) ;
#54002 = DIRECTION ( 'NONE',  ( -1.000000000000000000, 0.000000000000000000, -0.000000000000000000 ) ) ;
#54003 = DIRECTION ( 'NONE',  ( -1.000000000000000000, 0.000000000000000000, -0.000000000000000000 ) ) ;
#54004 = CYLINDRICAL_SURFACE ( 'NONE', #67000, 2.649999999999985700 ) ;
#54005 = CARTESIAN_POINT ( 'NONE',  ( 97.64999999999999147, -209.9999999999999716, 80.15749999999999886 ) ) ;
#54006 = VECTOR ( 'NONE', #49348, 1000.000000000000000 ) ;
#54007 = VERTEX_POINT ( 'NONE', #48640 ) ;
#54008 = ORIENTED_EDGE ( 'NONE', *, *, #28445, .F. ) ;
#54009 = AXIS2_PLACEMENT_3D ( 'NONE', #24548, #23086, #51644 ) ;
#54010 = ORIENTED_EDGE ( 'NONE', *, *, #303, .F. ) ;
#54011 = ORIENTED_EDGE ( 'NONE', *, *, #31422, .F. ) ;
#54012 = EDGE_CURVE ( 'NONE', #25891, #31993, #66855, .T. ) ;
#54013 = EDGE_CURVE ( 'NONE', #13090, #9512, #43392, .T. ) ;
#54014 = SURFACE_SIDE_STYLE ('',( #14132 ) ) ;
#54015 = CARTESIAN_POINT ( 'NONE',  ( -97.30629616937501680, 90.00000000000004263, 84.08656250086716000 ) ) ;
#54016 = CARTESIAN_POINT ( 'NONE',  ( -97.64999999999996305, -209.9999999999999716, 77.29999999999999716 ) ) ;
#54017 = AXIS2_PLACEMENT_3D ( 'NONE', #21699, #39754, #33337 ) ;
#54018 = CARTESIAN_POINT ( 'NONE',  ( 10.00000000000000000, 75.11764819372149304, -2.946379043146603482 ) ) ;
#54019 = CARTESIAN_POINT ( 'NONE',  ( 93.67499999999998295, 92.29496732002878900, 75.92416666666666458 ) ) ;
#54020 = ORIENTED_EDGE ( 'NONE', *, *, #28605, .T. ) ;
#54021 = CARTESIAN_POINT ( 'NONE',  ( -97.64999999999996305, -209.9999999999999716, 84.99937500173429328 ) ) ;
#54022 = VERTEX_POINT ( 'NONE', #47895 ) ;
#54023 = CARTESIAN_POINT ( 'NONE',  ( 10.00000000000000000, -37.58145647212455032, 0.6853352020789044152 ) ) ;
#54024 = ORIENTED_EDGE ( 'NONE', *, *, #50339, .T. ) ;
#54025 = CARTESIAN_POINT ( 'NONE',  ( -93.67500000000003979, 92.29496732002878900, 87.32770833506762642 ) ) ;
#54026 = CARTESIAN_POINT ( 'NONE',  ( 97.30629616937498838, 90.00000000000002842, 86.30906250086715659 ) ) ;
#54027 = CARTESIAN_POINT ( 'NONE',  ( -7.500000000000016875, -80.00000000000001421, -269.9999999999999432 ) ) ;
#54028 = LINE ( 'NONE', #13782, #73426 ) ;
#54029 = VECTOR ( 'NONE', #73995, 1000.000000000000000 ) ;
#54030 = CARTESIAN_POINT ( 'NONE',  ( 10.00000000000000000, -65.64334221924939072, 41.19522573413710376 ) ) ;
#54031 = CARTESIAN_POINT ( 'NONE',  ( 10.00000000000000000, 6.555932627142952995, -37.01155633439051940 ) ) ;
#54032 = ORIENTED_EDGE ( 'NONE', *, *, #55945, .T. ) ;
#54033 = CARTESIAN_POINT ( 'NONE',  ( 10.00000000000000000, 16.23288003029497162, 33.80338159004289622 ) ) ;
#54034 = CIRCLE ( 'NONE', #66064, 42.00000000000000000 ) ;
#54035 = AXIS2_PLACEMENT_3D ( 'NONE', #44119, #27179, #38485 ) ;
#54037 = CARTESIAN_POINT ( 'NONE',  ( 0.000000000000000000, -120.0000000000000000, -2.500000000000000000 ) ) ;
#54036 = AXIS2_PLACEMENT_3D ( 'NONE', #59972, #44139, #9919 ) ;
#54038 = ORIENTED_EDGE ( 'NONE', *, *, #55264, .F. ) ;
#54039 = VERTEX_POINT ( 'NONE', #36611 ) ;
#54040 = PLANE ( 'NONE',  #62583 ) ;
#54041 = AXIS2_PLACEMENT_3D ( 'NONE', #34651, #6464, #17727 ) ;
#54042 = CARTESIAN_POINT ( 'NONE',  ( 2.500000000000000000, 16.00000000000000000, -10.00000000000000178 ) ) ;
#54043 = CARTESIAN_POINT ( 'NONE',  ( -94.99999999999997158, -209.9999999999999716, 90.00000000000000000 ) ) ;
#54044 = CARTESIAN_POINT ( 'NONE',  ( -92.69370383062498320, -208.6684592857803011, 83.82197916753382572 ) ) ;
#54045 = EDGE_LOOP ( 'NONE', ( #55942, #18912, #33957, #30865, #24403, #67249, #68540, #21537, #57912, #57908, #59017, #62919, #12836, #70141, #36311, #63463, #59103, #38583, #49254, #46798, #22286, #22800, #63254, #62136, #28677, #10707, #13301, #1403, #48270, #47234, #58174, #20431, #34788, #70625, #13051, #4265, #22867, #61052, #48091, #54425, #68059, #35789, #19491, #24104, #60233, #9792, #60671, #46222, #18371, #57733, #63546, #56049, #74317, #40391, #41218, #72605, #32733, #20700, #54190, #24746, #3485, #42469, #30587, #3560, #54752, #73934, #57323, #51386, #15740, #28410, #15139, #21270, #45900, #48107, #42895, #59439, #51205, #9795, #13022, #17056, #13566, #49265, #48833, #43369, #58651, #40909, #65380, #14405, #33836, #70905, #31817, #72134, #54011, #23250, #42722, #45704, #48110, #23164, #64772, #56490, #14070, #62612, #9819, #6193, #32335, #19066, #71910, #34654, #52319, #34505, #17841, #68872, #9126, #39805, #40434, #11620, #47101, #71161, #37082, #65035, #26541, #40417, #46665, #65665, #12041, #72595, #55481, #50285, #47879, #9599, #1898, #45972, #22285, #4693, #65611, #19719, #10568, #27349, #9836, #1527, #12243, #30201, #10718, #27476, #3452, #15534, #505, #2666, #44024, #72623, #38474, #60029, #23853, #55005, #46807, #7103, #66315, #54848, #5484, #25157, #31395, #66937, #16932, #13750, #44407 ) ) ;
#54046 = DIRECTION ( 'NONE',  ( -1.000000000000000000, -0.000000000000000000, 0.000000000000000000 ) ) ;
#54047 = VERTEX_POINT ( 'NONE', #43006 ) ;
#54048 = VERTEX_POINT ( 'NONE', #65942 ) ;
#54049 = DIRECTION ( 'NONE',  ( -0.000000000000000000, -0.000000000000000000, 1.000000000000000000 ) ) ;
#54050 = CARTESIAN_POINT ( 'NONE',  ( 96.15314808468748708, 88.00268892867053694, 88.74322916753382628 ) ) ;
#54051 = SURFACE_STYLE_USAGE ( .BOTH. , #31100 ) ;
#54052 = CARTESIAN_POINT ( 'NONE',  ( 93.84685191531248449, 88.00268892867053694, 82.76364583420047438 ) ) ;
#54053 = CARTESIAN_POINT ( 'NONE',  ( -0.1915406271734583221, -121.4877204670710427, -2.500000000000000000 ) ) ;
#54054 = DIRECTION ( 'NONE',  ( -0.8541291221503261033, 0.5200609990133016058, 0.000000000000000000 ) ) ;
#54055 = CARTESIAN_POINT ( 'NONE',  ( 10.00000000000000000, 0.000000000000000000, 0.000000000000000000 ) ) ;
#54056 = DIRECTION ( 'NONE',  ( 0.000000000000000000, 0.000000000000000000, 1.000000000000000000 ) ) ;
#54057 = CARTESIAN_POINT ( 'NONE',  ( 0.000000000000000000, 0.000000000000000000, 0.000000000000000000 ) ) ;
#54058 = LINE ( 'NONE', #65342, #57505 ) ;
#54059 = SHAPE_REPRESENTATION ( 'Shift Fork Lever Arm', ( #43395 ), #45865 ) ;
#54060 = DIRECTION ( 'NONE',  ( -0.000000000000000000, -0.000000000000000000, -1.000000000000000000 ) ) ;
#54061 = EDGE_CURVE ( 'NONE', #29988, #71738, #72841, .T. ) ;
#54062 = CARTESIAN_POINT ( 'NONE',  ( 10.00000000000000000, 0.000000000000000000, 0.000000000000000000 ) ) ;
#54063 = ORIENTED_EDGE ( 'NONE', *, *, #7147, .F. ) ;
#54064 = CIRCLE ( 'NONE', #6098, 31.99999999999998579 ) ;
#54065 = EDGE_CURVE ( 'NONE', #27808, #53848, #69327, .T. ) ;
#54066 = CARTESIAN_POINT ( 'NONE',  ( -93.84685191531254134, 91.99731107132950569, 86.25614583420048120 ) ) ;
#54067 = AXIS2_PLACEMENT_3D ( 'NONE', #70867, #24287, #69765 ) ;
#54068 = CARTESIAN_POINT ( 'NONE',  ( 0.000000000000000000, -16.45098606841102651, -33.79645857604531045 ) ) ;
#54069 = EDGE_CURVE ( 'NONE', #63900, #7213, #45363, .T. ) ;
#54070 = AXIS2_PLACEMENT_3D ( 'NONE', #13892, #65786, #19175 ) ;
#54071 = ADVANCED_FACE ( 'NONE', ( #72302 ), #20801, .T. ) ;
#54072 = DIRECTION ( 'NONE',  ( -1.000000000000000000, 7.619177619974977057E-15, 2.612289469705706555E-14 ) ) ;
#54073 = ORIENTED_EDGE ( 'NONE', *, *, #45872, .F. ) ;
#54074 = EDGE_CURVE ( 'NONE', #33637, #24497, #72655, .T. ) ;
#54075 = LINE ( 'NONE', #58593, #59494 ) ;
#54076 = FACE_OUTER_BOUND ( 'NONE', #12924, .T. ) ;
#54077 = CARTESIAN_POINT ( 'NONE',  ( 0.000000000000000000, 0.000000000000000000, 0.000000000000000000 ) ) ;
#54078 = CIRCLE ( 'NONE', #18070, 32.00000000000000000 ) ;
#54079 = AXIS2_PLACEMENT_3D ( 'NONE', #44728, #45478, #63143 ) ;
#54080 = CIRCLE ( 'NONE', #21661, 12.74999999999999822 ) ;
#54081 = CARTESIAN_POINT ( 'NONE',  ( 93.84685191531249870, -208.0026889286704943, 80.80572916753382628 ) ) ;
#54082 = ORIENTED_EDGE ( 'NONE', *, *, #9614, .T. ) ;
#54083 = CIRCLE ( 'NONE', #73282, 82.00000000000000000 ) ;
#54084 = EDGE_LOOP ( 'NONE', ( #5065, #66018, #38287, #49190 ) ) ;
#54085 = CIRCLE ( 'NONE', #21665, 77.49900000000000944 ) ;
#54086 = ADVANCED_FACE ( 'NONE', ( #73777 ), #21160, .T. ) ;
#54087 = ADVANCED_FACE ( 'NONE', ( #21915 ), #51224, .T. ) ;
#54088 = DIRECTION ( 'NONE',  ( -1.000000000000000000, 0.000000000000000000, 0.000000000000000000 ) ) ;
#54089 = VERTEX_POINT ( 'NONE', #39216 ) ;
#54090 = CARTESIAN_POINT ( 'NONE',  ( 10.00000000000000000, 37.48860685352291000, -0.8828120875901940279 ) ) ;
#54091 = CARTESIAN_POINT ( 'NONE',  ( 5.999999999999999112, -50.23322058963393744, 64.81221759200325039 ) ) ;
#54092 = VERTEX_POINT ( 'NONE', #10261 ) ;
#54093 = CARTESIAN_POINT ( 'NONE',  ( 4.999999999999999112, 40.98264845739749518, 9.188173127307448951 ) ) ;
#54094 = CARTESIAN_POINT ( 'NONE',  ( 97.30629616937498838, -211.3315407142195852, 75.46114583420049371 ) ) ;
#54095 = ORIENTED_EDGE ( 'NONE', *, *, #54343, .F. ) ;
#54096 = CARTESIAN_POINT ( 'NONE',  ( -19.27444613274700913, -101.8135840178490668, 2.500000000000000000 ) ) ;
#54097 = VERTEX_POINT ( 'NONE', #56883 ) ;
#54098 = ORIENTED_EDGE ( 'NONE', *, *, #19018, .F. ) ;
#54099 = LINE ( 'NONE', #65741, #70558 ) ;
#54100 = EDGE_CURVE ( 'NONE', #24060, #63369, #29704, .T. ) ;
#54101 = ADVANCED_FACE ( 'NONE', ( #55385 ), #56130, .T. ) ;
#54102 = CARTESIAN_POINT ( 'NONE',  ( -92.35000000000003695, 90.00000000000004263, 82.69749999999999091 ) ) ;
#54103 = ORIENTED_EDGE ( 'NONE', *, *, #2741, .F. ) ;
#54104 = DIRECTION ( 'NONE',  ( -1.000000000000000000, 0.000000000000000000, 0.000000000000000000 ) ) ;
#54105 = CARTESIAN_POINT ( 'NONE',  ( 92.35000000000002274, -208.4700217866474645, 84.31145833506762699 ) ) ;
#54106 = CARTESIAN_POINT ( 'NONE',  ( 92.34999999999999432, 88.47002178664753558, 83.70291666666668107 ) ) ;
#54107 = ORIENTED_EDGE ( 'NONE', *, *, #5186, .T. ) ;
#54108 = DIRECTION ( 'NONE',  ( 0.000000000000000000, 0.000000000000000000, 1.000000000000000000 ) ) ;
#54109 = DIRECTION ( 'NONE',  ( -1.000000000000000000, -0.000000000000000000, -0.000000000000000000 ) ) ;
#54110 = VERTEX_POINT ( 'NONE', #33184 ) ;
#54111 = ORIENTED_EDGE ( 'NONE', *, *, #65954, .T. ) ;
#54112 = CARTESIAN_POINT ( 'NONE',  ( -95.00000000000002842, 87.33691857156074434, 86.78531250086713555 ) ) ;
#54113 = CARTESIAN_POINT ( 'NONE',  ( 92.69370383062498320, 91.33154071421968467, 80.69989583420048973 ) ) ;
#54114 = VERTEX_POINT ( 'NONE', #28285 ) ;
#54115 = CARTESIAN_POINT ( 'NONE',  ( 96.32499999999997442, 92.29496732002878900, 82.88270833506763324 ) ) ;
#54116 = CIRCLE ( 'NONE', #30105, 31.99999999999998934 ) ;
#54117 = CYLINDRICAL_SURFACE ( 'NONE', #44462, 77.49899999999999523 ) ;
#54118 = EDGE_LOOP ( 'NONE', ( #41988, #69900, #55016, #54360 ) ) ;
#54119 = DIRECTION ( 'NONE',  ( 1.000000000000000000, 0.000000000000000000, -0.000000000000000000 ) ) ;
#54120 = VECTOR ( 'NONE', #30267, 1000.000000000000000 ) ;
#54121 = VERTEX_POINT ( 'NONE', #15533 ) ;
#54122 = ORIENTED_EDGE ( 'NONE', *, *, #39482, .T. ) ;
#54123 = ORIENTED_EDGE ( 'NONE', *, *, #30213, .T. ) ;
#54124 = DIRECTION ( 'NONE',  ( -1.000000000000000000, 0.000000000000000000, 0.000000000000000000 ) ) ;
#54125 = DIRECTION ( 'NONE',  ( -1.000000000000000000, -0.000000000000000000, -0.000000000000000000 ) ) ;
#54126 = CARTESIAN_POINT ( 'NONE',  ( -92.35000000000003695, 90.00000000000004263, 83.96750000000000114 ) ) ;
#54127 = EDGE_LOOP ( 'NONE', ( #50591, #70743, #20954, #6929 ) ) ;
#54128 = CARTESIAN_POINT ( 'NONE',  ( 97.64999999999999147, 90.00000000000002842, 82.06250000000000000 ) ) ;
#54129 = LINE ( 'NONE', #69919, #35865 ) ;
#54130 = ORIENTED_EDGE ( 'NONE', *, *, #53221, .T. ) ;
#54131 = CYLINDRICAL_SURFACE ( 'NONE', #60024, 31.99999999999999289 ) ;
#54132 = CARTESIAN_POINT ( 'NONE',  ( -94.99999999999997158, -207.3369185715606307, 81.22906250086715829 ) ) ;
#54133 = ORIENTED_EDGE ( 'NONE', *, *, #64006, .F. ) ;
#54134 = CARTESIAN_POINT ( 'NONE',  ( 10.00000000000000000, -24.73286445877757345, 73.44644590900053061 ) ) ;
#54135 = DIRECTION ( 'NONE',  ( -0.8090169943749504489, 0.5877852522924689183, 0.000000000000000000 ) ) ;
#54136 = CYLINDRICAL_SURFACE ( 'NONE', #20128, 16.00000000000000000 ) ;
#54137 = DIRECTION ( 'NONE',  ( -1.000000000000000000, 0.000000000000000000, 0.000000000000000000 ) ) ;
#54138 = VECTOR ( 'NONE', #28978, 1000.000000000000000 ) ;
#54139 = CARTESIAN_POINT ( 'NONE',  ( 92.35000000000000853, -209.9999999999999716, 83.72937500173429726 ) ) ;
#54140 = AXIS2_PLACEMENT_3D ( 'NONE', #41000, #63931, #30065 ) ;
#54141 = CARTESIAN_POINT ( 'NONE',  ( 0.000000000000000000, -30.84782396557201878, -21.32104025579148399 ) ) ;
#54142 = LINE ( 'NONE', #70658, #16821 ) ;
#54143 = EDGE_CURVE ( 'NONE', #59084, #40700, #54940, .T. ) ;
#54144 = DIRECTION ( 'NONE',  ( -1.000000000000000000, 0.000000000000000000, -0.000000000000000000 ) ) ;
#54145 = AXIS2_PLACEMENT_3D ( 'NONE', #37514, #54792, #3688 ) ;
#54146 = CARTESIAN_POINT ( 'NONE',  ( 97.64999999999999147, 89.99999413691126904, 82.77687479895028844 ) ) ;
#54147 = EDGE_CURVE ( 'NONE', #1246, #73701, #27549, .T. ) ;
#54148 = CARTESIAN_POINT ( 'NONE',  ( -93.84685191531254134, 91.99731107132950569, 76.73114583420047552 ) ) ;
#54149 = CARTESIAN_POINT ( 'NONE',  ( 0.000000000000000000, 0.8660254037844389297, 1.500000000000000000 ) ) ;
#54150 = CARTESIAN_POINT ( 'NONE',  ( -7.400000000000022560, -2.610330509153157305E-13, -23.50000000000042633 ) ) ;
#54151 = ADVANCED_FACE ( 'NONE', ( #68152 ), #68538, .F. ) ;
#54152 = DIRECTION ( 'NONE',  ( 0.000000000000000000, 0.000000000000000000, 1.000000000000000000 ) ) ;
#54153 = UNCERTAINTY_MEASURE_WITH_UNIT (LENGTH_MEASURE( 1.000000000000000082E-05 ), #10159, 'distance_accuracy_value', 'NONE');
#54154 = CARTESIAN_POINT ( 'NONE',  ( 92.35000000000000853, -209.9999999999999716, 90.00000000000000000 ) ) ;
#54155 = EDGE_CURVE ( 'NONE', #44097, #6594, #67405, .T. ) ;
#54156 = DIRECTION ( 'NONE',  ( 0.000000000000000000, -0.1564344650402170189, -0.9876883405951399908 ) ) ;
#54157 = CYLINDRICAL_SURFACE ( 'NONE', #40622, 31.99999999999999289 ) ;
#54158 = LINE ( 'NONE', #2689, #15464 ) ;
#54159 = CARTESIAN_POINT ( 'NONE',  ( -12.00000000000000000, 0.000000000000000000, -17.30399999999999849 ) ) ;
#54160 = ADVANCED_FACE ( 'NONE', ( #16646 ), #33936, .T. ) ;
#54161 = DIRECTION ( 'NONE',  ( -1.000000000000000000, -0.000000000000000000, -0.000000000000000000 ) ) ;
#54162 = CARTESIAN_POINT ( 'NONE',  ( -97.64999999999994884, -211.5299782133524502, 88.78291666666667936 ) ) ;
#54163 = CARTESIAN_POINT ( 'NONE',  ( 10.00000000000000000, -65.59268652807183742, -36.72794159290312166 ) ) ;
#54164 = PRODUCT_DEFINITION_SHAPE ( 'NONE', 'NONE',  #74347 ) ;
#54165 = ORIENTED_EDGE ( 'NONE', *, *, #29671, .T. ) ;
#54166 = EDGE_CURVE ( 'NONE', #44200, #30664, #74152, .T. ) ;
#54167 = DIRECTION ( 'NONE',  ( 0.000000000000000000, 0.000000000000000000, 1.000000000000000000 ) ) ;
#54168 = CARTESIAN_POINT ( 'NONE',  ( 0.000000000000000000, -75.16055320797016748, -18.89407956138335365 ) ) ;
#54169 = CARTESIAN_POINT ( 'NONE',  ( 0.000000000000000000, -40.65526001592664329, 71.21200624218782593 ) ) ;
#54170 = CYLINDRICAL_SURFACE ( 'NONE', #4224, 16.00000000000000000 ) ;
#54171 = STYLED_ITEM ( 'NONE', ( #203 ), #7701 ) ;
#54172 = CIRCLE ( 'NONE', #52934, 14.09999999999999964 ) ;
#54173 = AXIS2_PLACEMENT_3D ( 'NONE', #15382, #59508, #9008 ) ;
#54174 = ORIENTED_EDGE ( 'NONE', *, *, #21571, .F. ) ;
#54175 = EDGE_CURVE ( 'NONE', #35072, #54619, #45612, .T. ) ;
#54176 = DIRECTION ( 'NONE',  ( -1.000000000000000000, -0.000000000000000000, 0.000000000000000000 ) ) ;
#54177 = ADVANCED_FACE ( 'NONE', ( #38839 ), #67783, .T. ) ;
#54178 = FACE_OUTER_BOUND ( 'NONE', #4264, .T. ) ;
#54179 = ORIENTED_EDGE ( 'NONE', *, *, #23800, .F. ) ;
#54180 = CARTESIAN_POINT ( 'NONE',  ( 92.69370383062501162, -211.3315407142195852, 80.80572916753379786 ) ) ;
#54181 = DIRECTION ( 'NONE',  ( 0.000000000000000000, -0.1564344650402382242, 0.9876883405951366601 ) ) ;
#54182 = ORIENTED_EDGE ( 'NONE', *, *, #37621, .T. ) ;
#54183 = DIRECTION ( 'NONE',  ( -0.000000000000000000, -0.000000000000000000, 1.000000000000000000 ) ) ;
#54184 = EDGE_LOOP ( 'NONE', ( #29025, #58822, #47487, #59258 ) ) ;
#54185 = DIRECTION ( 'NONE',  ( -1.000000000000000000, -0.000000000000000000, 0.000000000000000000 ) ) ;
#54186 = VERTEX_POINT ( 'NONE', #27166 ) ;
#54187 = AXIS2_PLACEMENT_3D ( 'NONE', #52741, #11756, #64033 ) ;
#54188 = CARTESIAN_POINT ( 'NONE',  ( -97.30629616937501680, 88.66845928578038638, 75.88447916753382572 ) ) ;
#54189 = VECTOR ( 'NONE', #65687, 1000.000000000000114 ) ;
#54190 = ORIENTED_EDGE ( 'NONE', *, *, #19683, .F. ) ;
#54191 = ORIENTED_EDGE ( 'NONE', *, *, #10898, .T. ) ;
#54192 = DIRECTION ( 'NONE',  ( 0.000000000000000000, 0.000000000000000000, 1.000000000000000000 ) ) ;
#54193 = VECTOR ( 'NONE', #61091, 1000.000000000000000 ) ;
#54194 = ORIENTED_EDGE ( 'NONE', *, *, #64193, .T. ) ;
#54195 = DIRECTION ( 'NONE',  ( 0.000000000000000000, 0.5877852522924684742, 0.8090169943749507819 ) ) ;
#54196 = CARTESIAN_POINT ( 'NONE',  ( 92.35000000003287823, -209.9999916080746516, 86.90410584365268676 ) ) ;
#54197 = EDGE_LOOP ( 'NONE', ( #62692, #866, #69012, #38467 ) ) ;
#54198 = CARTESIAN_POINT ( 'NONE',  ( 0.000000000000000000, 0.000000000000000000, -310.0000000000000000 ) ) ;
#54199 = ORIENTED_EDGE ( 'NONE', *, *, #30298, .F. ) ;
#54200 = DIRECTION ( 'NONE',  ( 0.000000000000000000, -1.000000000000000000, -1.047444401652940007E-14 ) ) ;
#54201 = ORIENTED_EDGE ( 'NONE', *, *, #18899, .F. ) ;
#54202 = ORIENTED_EDGE ( 'NONE', *, *, #11930, .F. ) ;
#54203 = ORIENTED_EDGE ( 'NONE', *, *, #54804, .T. ) ;
#54204 = CARTESIAN_POINT ( 'NONE',  ( 93.84685191531251292, -211.9973110713294489, 78.31864583420048120 ) ) ;
#54205 = CARTESIAN_POINT ( 'NONE',  ( 10.00000000000000000, 35.53030884539084866, 12.26510123303271982 ) ) ;
#54206 = ITEM_DEFINED_TRANSFORMATION ( 'NONE', 'NONE', #47190,  #43395 ) ;
#54207 = CARTESIAN_POINT ( 'NONE',  ( -97.65000000000001990, 90.00000000000004263, 88.09499999999999886 ) ) ;
#54208 = ORIENTED_EDGE ( 'NONE', *, *, #68865, .T. ) ;
#54209 = LINE ( 'NONE', #13601, #37675 ) ;
#54210 = ORIENTED_EDGE ( 'NONE', *, *, #49036, .T. ) ;
#54211 = CARTESIAN_POINT ( 'NONE',  ( -21.67772167707813935, -110.8034581014852762, 5.500000000000000000 ) ) ;
#54212 = CARTESIAN_POINT ( 'NONE',  ( 0.000000000000000000, -21.53537804866058991, -30.80686688397033635 ) ) ;
#54213 = CARTESIAN_POINT ( 'NONE',  ( -97.64999999999996305, -208.4700217866474645, 88.75645833506762017 ) ) ;
#54214 = CARTESIAN_POINT ( 'NONE',  ( 22.75000000000000000, 0.000000000000000000, 0.000000000000000000 ) ) ;
#54215 = CARTESIAN_POINT ( 'NONE',  ( -94.99999999999997158, -212.6630814284392557, 82.18156250086714465 ) ) ;
#54216 = CARTESIAN_POINT ( 'NONE',  ( -97.30629616937501680, 90.00000000000004263, 77.73656250086715147 ) ) ;
#54217 = ADVANCED_FACE ( 'NONE', ( #5018, #26805 ), #15905, .T. ) ;
#54218 = ORIENTED_EDGE ( 'NONE', *, *, #7331, .F. ) ;
#54219 = CARTESIAN_POINT ( 'NONE',  ( 94.99999999999998579, 87.33691857156068750, 82.18156250086714465 ) ) ;
#54220 = VERTEX_POINT ( 'NONE', #1896 ) ;
#54221 = CARTESIAN_POINT ( 'NONE',  ( 26.00000000000000355, 0.000000000000000000, 0.000000000000000000 ) ) ;
#54222 = LINE ( 'NONE', #47103, #14336 ) ;
#54223 = CARTESIAN_POINT ( 'NONE',  ( -93.67499999999998295, -212.2949673200287179, 76.87666666666666515 ) ) ;
#54224 = DIRECTION ( 'NONE',  ( 1.000000000000000000, -0.000000000000000000, 0.000000000000000000 ) ) ;
#54225 = CARTESIAN_POINT ( 'NONE',  ( 0.000000000000000000, -74.65491531819111515, -8.830959090343204920 ) ) ;
#54226 = CARTESIAN_POINT ( 'NONE',  ( -94.99999999999997158, -212.6630814284392557, 82.81656250086712134 ) ) ;
#54227 =( GEOMETRIC_REPRESENTATION_CONTEXT ( 3 ) GLOBAL_UNCERTAINTY_ASSIGNED_CONTEXT ( ( #3927 ) ) GLOBAL_UNIT_ASSIGNED_CONTEXT ( ( #1311, #70039, #34731 ) ) REPRESENTATION_CONTEXT ( 'NONE', 'WORKASPACE' ) );
#54228 = VECTOR ( 'NONE', #12418, 1000.000000000000000 ) ;
#54229 = CARTESIAN_POINT ( 'NONE',  ( 10.00000000000000000, 37.48860685352291000, 0.8828120875901893649 ) ) ;
#54230 = CARTESIAN_POINT ( 'NONE',  ( 5.000000000000000000, -44.99326035066101781, 68.55367621811127776 ) ) ;
#54231 = CIRCLE ( 'NONE', #31402, 31.99999999999998579 ) ;
#54232 = PLANE ( 'NONE',  #17901 ) ;
#54233 = ORIENTED_EDGE ( 'NONE', *, *, #42681, .T. ) ;
#54234 = ORIENTED_EDGE ( 'NONE', *, *, #8498, .F. ) ;
#54235 = CARTESIAN_POINT ( 'NONE',  ( -8.637688417678527131, 13.69818742750669394, 52.00000000000002132 ) ) ;
#54236 = EDGE_CURVE ( 'NONE', #27007, #31458, #71003, .T. ) ;
#54237 = CARTESIAN_POINT ( 'NONE',  ( 0.000000000000000000, -120.0000000000000000, -40.00000000000000711 ) ) ;
#54238 = ADVANCED_FACE ( 'NONE', ( #59744 ), #7501, .T. ) ;
#54239 = DIRECTION ( 'NONE',  ( -0.000000000000000000, 0.000000000000000000, 1.000000000000000000 ) ) ;
#54240 = CARTESIAN_POINT ( 'NONE',  ( -95.00000000000002842, 92.66308142843932671, 83.76906250086713612 ) ) ;
#54241 = CARTESIAN_POINT ( 'NONE',  ( -96.01774234934295293, -207.8046129959941197, 74.85985921673513133 ) ) ;
#54242 = CARTESIAN_POINT ( 'NONE',  ( 26.00000000000000355, 0.000000000000000000, 0.000000000000000000 ) ) ;
#54243 = CARTESIAN_POINT ( 'NONE',  ( 12.00000000000000000, -1.278221433540145391, 26.51162292216073979 ) ) ;
#54244 = ORIENTED_EDGE ( 'NONE', *, *, #46000, .F. ) ;
#54245 = CARTESIAN_POINT ( 'NONE',  ( -92.69370383062502583, 91.33154071421968467, 74.77322916753379900 ) ) ;
#54246 = ADVANCED_FACE ( 'NONE', ( #64641 ), #31159, .T. ) ;
#54247 = EDGE_CURVE ( 'NONE', #73160, #59759, #26120, .T. ) ;
#54248 = AXIS2_PLACEMENT_3D ( 'NONE', #5331, #68474, #51908 ) ;
#54249 = DIRECTION ( 'NONE',  ( 0.000000000000000000, -1.000000000000000000, -1.040834085586084257E-14 ) ) ;
#54250 = VECTOR ( 'NONE', #51414, 1000.000000000000000 ) ;
#54251 = CARTESIAN_POINT ( 'NONE',  ( -3.453178355211937944, 3.779809238954856099, -0.7375898304884446199 ) ) ;
#54252 = CARTESIAN_POINT ( 'NONE',  ( 93.67500000000001137, -207.7050326799711968, 84.81416666666666515 ) ) ;
#54253 = CARTESIAN_POINT ( 'NONE',  ( -10.00000000000000000, 0.000000000000000000, 0.000000000000000000 ) ) ;
#54254 = CARTESIAN_POINT ( 'NONE',  ( -97.30629616937495996, -209.9999999999999716, 82.18156250086715886 ) ) ;
#54255 = AXIS2_PLACEMENT_3D ( 'NONE', #62972, #69318, #11428 ) ;
#54256 = DIRECTION ( 'NONE',  ( 0.000000000000000000, 0.000000000000000000, 1.000000000000000000 ) ) ;
#54257 = EDGE_CURVE ( 'NONE', #4558, #30043, #53722, .T. ) ;
#54258 = CARTESIAN_POINT ( 'NONE',  ( 11.99999999999999822, -39.78640506895559525, -66.50666863322042843 ) ) ;
#54259 = CARTESIAN_POINT ( 'NONE',  ( 9.984461079971730157, -95.40710393340121698, -2.500000000000000000 ) ) ;
#54260 = DIRECTION ( 'NONE',  ( 0.000000000000000000, 0.000000000000000000, 1.000000000000000000 ) ) ;
#54261 = ORIENTED_EDGE ( 'NONE', *, *, #41501, .F. ) ;
#54262 = DIRECTION ( 'NONE',  ( -1.000000000000000000, -0.000000000000000000, 0.000000000000000000 ) ) ;
#54263 = DIRECTION ( 'NONE',  ( 0.000000000000000000, 0.000000000000000000, 1.000000000000000000 ) ) ;
#54264 = DIRECTION ( 'NONE',  ( -1.000000000000000000, -0.000000000000000000, 0.000000000000000000 ) ) ;
#54265 = CARTESIAN_POINT ( 'NONE',  ( 97.30629616937498838, -211.3315407142195852, 89.43114583420049257 ) ) ;
#54266 = ORIENTED_EDGE ( 'NONE', *, *, #915, .T. ) ;
#54267 = EDGE_CURVE ( 'NONE', #25004, #28623, #25163, .T. ) ;
#54268 = EDGE_CURVE ( 'NONE', #60480, #35604, #70256, .T. ) ;
#54269 = LINE ( 'NONE', #42991, #57691 ) ;
#54270 = CARTESIAN_POINT ( 'NONE',  ( -0.9774260708577104939, -118.8621782758236378, -2.500000000000000000 ) ) ;
#54271 = ORIENTED_EDGE ( 'NONE', *, *, #20796, .F. ) ;
#54272 = CARTESIAN_POINT ( 'NONE',  ( -10.00000000000000000, 0.000000000000000000, 0.000000000000000000 ) ) ;
#54273 = EDGE_CURVE ( 'NONE', #4807, #51310, #60904, .T. ) ;
#54274 = EDGE_LOOP ( 'NONE', ( #40218, #67065, #27637, #73914 ) ) ;
#54275 = VECTOR ( 'NONE', #68002, 1000.000000000000000 ) ;
#54276 = FACE_OUTER_BOUND ( 'NONE', #48723, .T. ) ;
#54277 = ORIENTED_EDGE ( 'NONE', *, *, #4681, .T. ) ;
#54278 = ORIENTED_EDGE ( 'NONE', *, *, #49162, .T. ) ;
#54279 = ORIENTED_EDGE ( 'NONE', *, *, #14075, .F. ) ;
#54280 = CARTESIAN_POINT ( 'NONE',  ( 11.99999999999999822, 0.000000000000000000, 0.000000000000000000 ) ) ;
#54281 = AXIS2_PLACEMENT_3D ( 'NONE', #49218, #61625, #38319 ) ;
#54282 = VERTEX_POINT ( 'NONE', #59372 ) ;
#54283 = VECTOR ( 'NONE', #61504, 1000.000000000000000 ) ;
#54284 = EDGE_LOOP ( 'NONE', ( #6530, #37150, #54562, #64558 ) ) ;
#54285 =( BOUNDED_CURVE ( )  B_SPLINE_CURVE ( 2, ( #67189, #73190, #67563, #37884, #26211, #60814, #15686 ),
 .UNSPECIFIED., .F., .F. ) 
 B_SPLINE_CURVE_WITH_KNOTS ( ( 3, 2, 2, 3 ),
 ( 0.7408554641864648627, 0.7479111473335299243, 0.7549669128744133095, 0.7620226289464454572 ),
 .UNSPECIFIED. ) 
 CURVE ( )  GEOMETRIC_REPRESENTATION_ITEM ( )  RATIONAL_B_SPLINE_CURVE ( ( 0.9999968710554256734, 0.8660269682749952569, 1.000000000000000000, 0.8660254037844387076, 1.000000000000000000, 0.8660263430970250864, 0.9999981213879984843 ) ) 
 REPRESENTATION_ITEM ( '' )  );
#54286 = CARTESIAN_POINT ( 'NONE',  ( 92.69370383062498320, 90.00000000000002842, 80.91156250086716284 ) ) ;
#54287 = FACE_BOUND ( 'NONE', #42158, .T. ) ;
#54288 = PLANE ( 'NONE',  #17649 ) ;
#54289 = VERTEX_POINT ( 'NONE', #18765 ) ;
#54290 = ORIENTED_EDGE ( 'NONE', *, *, #73314, .T. ) ;
#54291 = VERTEX_POINT ( 'NONE', #1533 ) ;
#54292 = CARTESIAN_POINT ( 'NONE',  ( 9.984461079971730157, -95.40710393340120277, -5.500000000000000000 ) ) ;
#54293 = AXIS2_PLACEMENT_3D ( 'NONE', #5192, #51032, #45411 ) ;
#54294 = EDGE_LOOP ( 'NONE', ( #46891, #20702, #33866, #21334 ) ) ;
#54295 = VECTOR ( 'NONE', #6234, 1000.000000000000000 ) ;
#54296 = CARTESIAN_POINT ( 'NONE',  ( 1.498801083244105440E-11, -120.0000000000024727, 24.99999999999850786 ) ) ;
#54297 = LINE ( 'NONE', #60678, #72717 ) ;
#54298 = DIRECTION ( 'NONE',  ( -1.000000000000000000, -0.000000000000000000, 0.000000000000000000 ) ) ;
#54299 = CARTESIAN_POINT ( 'NONE',  ( 92.35000000003357457, 89.99999234487445676, 78.01464417100922333 ) ) ;
#54300 = DIRECTION ( 'NONE',  ( 0.000000000000000000, -0.8090169943749426773, -0.5877852522924797984 ) ) ;
#54301 = CARTESIAN_POINT ( 'NONE',  ( -96.32500000000001705, 87.70503267997129626, 78.04083333333333883 ) ) ;
#54302 = DIRECTION ( 'NONE',  ( -1.000000000000000000, -0.000000000000000000, -0.000000000000000000 ) ) ;
#54303 = CARTESIAN_POINT ( 'NONE',  ( -97.64999999999994884, -211.5299782133524502, 75.52729166840099140 ) ) ;
#54304 = CARTESIAN_POINT ( 'NONE',  ( -95.00000000000002842, 87.33691857156074434, 88.69031250086716511 ) ) ;
#54305 = EDGE_CURVE ( 'NONE', #9979, #17228, #48453, .T. ) ;
#54307 = CARTESIAN_POINT ( 'NONE',  ( -93.67500000000003979, 92.29496732002878900, 77.80270833506763495 ) ) ;
#54306 = CARTESIAN_POINT ( 'NONE',  ( 93.67499999999999716, 87.70503267997126784, 75.58020833506763836 ) ) ;
#54308 = ORIENTED_EDGE ( 'NONE', *, *, #3696, .F. ) ;
#54309 = CARTESIAN_POINT ( 'NONE',  ( 97.30629616937498838, 90.00000000000002842, 76.14906250086716000 ) ) ;
#54310 = CARTESIAN_POINT ( 'NONE',  ( 10.00000000000000000, 32.34446384430010113, -26.79245525562679831 ) ) ;
#54311 = CARTESIAN_POINT ( 'NONE',  ( 7.999999999999974243, 2.611051703902955430E-13, 22.90000000000000924 ) ) ;
#54312 = CYLINDRICAL_SURFACE ( 'NONE', #28720, 31.99999999999999289 ) ;
#54313 = DIRECTION ( 'NONE',  ( 0.000000000000000000, 0.000000000000000000, -1.000000000000000000 ) ) ;
#54314 = EDGE_LOOP ( 'NONE', ( #55141, #59983, #10924, #38476 ) ) ;
#54315 = CARTESIAN_POINT ( 'NONE',  ( -12.49999999999999645, 0.000000000000000000, 42.00000000000001421 ) ) ;
#54316 = CARTESIAN_POINT ( 'NONE',  ( 92.35000000000000853, -209.9999999999999716, 89.36499999999999488 ) ) ;
#54317 = ORIENTED_EDGE ( 'NONE', *, *, #29959, .F. ) ;
#54318 = EDGE_CURVE ( 'NONE', #5972, #37629, #31424, .T. ) ;
#54319 = ORIENTED_EDGE ( 'NONE', *, *, #39974, .T. ) ;
#54320 = ADVANCED_FACE ( 'NONE', ( #19873 ), #41701, .T. ) ;
#54321 = DIRECTION ( 'NONE',  ( -1.000000000000000000, 0.000000000000000000, 0.000000000000000000 ) ) ;
#54322 = DIRECTION ( 'NONE',  ( -1.000000000000000000, -0.000000000000000000, -0.000000000000000000 ) ) ;
#54323 = FACE_OUTER_BOUND ( 'NONE', #45740, .T. ) ;
#54324 = FACE_OUTER_BOUND ( 'NONE', #59938, .T. ) ;
#54325 = CARTESIAN_POINT ( 'NONE',  ( 11.99999999999999822, -36.73666225445845157, -65.58780272294114866 ) ) ;
#54326 = CARTESIAN_POINT ( 'NONE',  ( -94.99999999999997158, -207.3369185715606307, 75.67281250086716682 ) ) ;
#54327 = VERTEX_POINT ( 'NONE', #12755 ) ;
#54328 = EDGE_CURVE ( 'NONE', #60196, #40964, #27293, .T. ) ;
#54329 = CARTESIAN_POINT ( 'NONE',  ( 11.99999999999999822, -76.41127070299262414, -12.93880638057396304 ) ) ;
#54330 = DIRECTION ( 'NONE',  ( 1.000000000000000000, 0.000000000000000000, 0.000000000000000000 ) ) ;
#54331 = AXIS2_PLACEMENT_3D ( 'NONE', #34920, #5623, #29620 ) ;
#54332 = DIRECTION ( 'NONE',  ( 0.000000000000000000, 0.8910065241883656784, 0.4539904997395511344 ) ) ;
#54333 = DIRECTION ( 'NONE',  ( 0.9730327541852497042, -0.2306669878475622604, 0.000000000000000000 ) ) ;
#54334 = CARTESIAN_POINT ( 'NONE',  ( 4.755015822784811164, -4.336808689942017736E-16, 0.000000000000000000 ) ) ;
#54335 = CARTESIAN_POINT ( 'NONE',  ( 95.00000000000000000, -206.9400435732949575, 80.39562500173430237 ) ) ;
#54336 = UNCERTAINTY_MEASURE_WITH_UNIT (LENGTH_MEASURE( 1.000000000000000082E-05 ), #33659, 'distance_accuracy_value', 'NONE');
#54337 = LINE ( 'NONE', #26118, #22996 ) ;
#54338 = CARTESIAN_POINT ( 'NONE',  ( 5.000000000000002665, -3.894527615417340272, -81.90746397400393164 ) ) ;
#54339 = DIRECTION ( 'NONE',  ( 0.000000000000000000, 0.7604059656000323741, -0.6494480483301819929 ) ) ;
#54340 = VECTOR ( 'NONE', #49772, 999.9999999999998863 ) ;
#54341 = EDGE_CURVE ( 'NONE', #69810, #44748, #24063, .T. ) ;
#54342 = VECTOR ( 'NONE', #28126, 1000.000000000000114 ) ;
#54343 = EDGE_CURVE ( 'NONE', #45782, #16094, #20108, .T. ) ;
#54344 = CARTESIAN_POINT ( 'NONE',  ( 93.84685191531248449, 91.99731107132950569, 84.61572916753381435 ) ) ;
#54345 = CARTESIAN_POINT ( 'NONE',  ( -97.30629616937497417, -211.3315407142195852, 83.50447916753383026 ) ) ;
#54346 = CYLINDRICAL_SURFACE ( 'NONE', #73378, 30.50000000000000000 ) ;
#54347 = ORIENTED_EDGE ( 'NONE', *, *, #37772, .F. ) ;
#54348 = DIRECTION ( 'NONE',  ( -8.332732854036912157E-16, -1.065814103640131031E-14, -1.000000000000000000 ) ) ;
#54349 = CARTESIAN_POINT ( 'NONE',  ( -97.64999999999996305, -209.9999999999999716, 77.29999999999999716 ) ) ;
#54350 = DIRECTION ( 'NONE',  ( -1.000000000000000000, -0.000000000000000000, -0.000000000000000000 ) ) ;
#54351 = ADVANCED_FACE ( 'NONE', ( #59008, #47352 ), #41340, .T. ) ;
#54352 = CIRCLE ( 'NONE', #5156, 42.00000000000000000 ) ;
#54353 = CARTESIAN_POINT ( 'NONE',  ( 97.30629616937498838, -209.9999999999999716, 82.97531250086714749 ) ) ;
#54354 = ORIENTED_EDGE ( 'NONE', *, *, #7311, .T. ) ;
#54355 = EDGE_CURVE ( 'NONE', #7925, #15992, #47713, .T. ) ;
#54356 = CYLINDRICAL_SURFACE ( 'NONE', #41911, 37.49900000000000233 ) ;
#54357 = VERTEX_POINT ( 'NONE', #9333 ) ;
#54358 = ORIENTED_EDGE ( 'NONE', *, *, #42713, .F. ) ;
#54359 = FACE_OUTER_BOUND ( 'NONE', #49279, .T. ) ;
#54360 = ORIENTED_EDGE ( 'NONE', *, *, #73188, .T. ) ;
#54361 = FACE_OUTER_BOUND ( 'NONE', #35683, .T. ) ;
#54362 = CARTESIAN_POINT ( 'NONE',  ( 92.69370383062501162, -211.3315407142195852, 78.42447916753380355 ) ) ;
#54363 = DIRECTION ( 'NONE',  ( -1.000000000000000000, 0.000000000000000000, 0.000000000000000000 ) ) ;
#54364 = CARTESIAN_POINT ( 'NONE',  ( -3.000000000000000000, 23.50000000000000000, -1.500000000000001332 ) ) ;
#54365 = CARTESIAN_POINT ( 'NONE',  ( -10.00000000000000000, 0.000000000000000000, 0.000000000000000000 ) ) ;
#54366 = DIRECTION ( 'NONE',  ( 0.000000000000000000, 0.000000000000000000, 1.000000000000000000 ) ) ;
#54367 = CARTESIAN_POINT ( 'NONE',  ( 10.00000000000000000, 17.80606268964585226, -33.00180498840028775 ) ) ;
#54368 = CARTESIAN_POINT ( 'NONE',  ( 96.32499999999998863, -207.7050326799711968, 82.16833333333332234 ) ) ;
#54369 = VERTEX_POINT ( 'NONE', #71737 ) ;
#54370 = ORIENTED_EDGE ( 'NONE', *, *, #12537, .T. ) ;
#54371 = ORIENTED_EDGE ( 'NONE', *, *, #42184, .F. ) ;
#54372 = VERTEX_POINT ( 'NONE', #33004 ) ;
#54373 = CARTESIAN_POINT ( 'NONE',  ( -96.32499999999996021, -212.2949673200287179, 86.37520833506764006 ) ) ;
#54374 = AXIS2_PLACEMENT_3D ( 'NONE', #53926, #47540, #2468 ) ;
#54375 = CARTESIAN_POINT ( 'NONE',  ( -92.69370383062502583, 91.33154071421968467, 82.55197916753382970 ) ) ;
#54376 = DIRECTION ( 'NONE',  ( 0.000000000000000000, 0.000000000000000000, 1.000000000000000000 ) ) ;
#54377 = CARTESIAN_POINT ( 'NONE',  ( 0.000000000000000000, 0.000000000000000000, -56.19999999999998863 ) ) ;
#54378 = CARTESIAN_POINT ( 'NONE',  ( 10.00000000000000000, -22.90783923731575911, -78.73519480814978522 ) ) ;
#54379 = CARTESIAN_POINT ( 'NONE',  ( 10.00000000000000000, 0.000000000000000000, 0.000000000000000000 ) ) ;
#54380 = EDGE_LOOP ( 'NONE', ( #70064, #8627, #61170, #64635 ) ) ;
#54381 = CARTESIAN_POINT ( 'NONE',  ( -92.34999999999999432, -209.9999999999999716, 84.68187500173429783 ) ) ;
#54382 = ORIENTED_EDGE ( 'NONE', *, *, #39471, .T. ) ;
#54383 = CARTESIAN_POINT ( 'NONE',  ( 25.81725066941077529, -113.8380548628854854, 5.500000000000000000 ) ) ;
#54384 = ORIENTED_EDGE ( 'NONE', *, *, #44482, .F. ) ;
#54385 = CARTESIAN_POINT ( 'NONE',  ( -92.35000000000003695, 90.00000000000004263, 87.85687500173429498 ) ) ;
#54386 = AXIS2_PLACEMENT_3D ( 'NONE', #34054, #63381, #17505 ) ;
#54387 = EDGE_LOOP ( 'NONE', ( #59618, #32198, #34878, #41556 ) ) ;
#54388 = CARTESIAN_POINT ( 'NONE',  ( 93.84685191531248449, 91.99731107132950569, 87.15572916753382060 ) ) ;
#54389 = CARTESIAN_POINT ( 'NONE',  ( 0.000000000000000000, 8.688484142254221609, -21.88630264137359660 ) ) ;
#54390 = DIRECTION ( 'NONE',  ( -1.000000000000000000, 0.000000000000000000, -0.000000000000000000 ) ) ;
#54391 = CARTESIAN_POINT ( 'NONE',  ( 92.34999999999999432, 90.00000000000002842, 88.73000000000000398 ) ) ;
#54392 = ADVANCED_FACE ( 'NONE', ( #55950 ), #26628, .T. ) ;
#54393 = FACE_OUTER_BOUND ( 'NONE', #66301, .T. ) ;
#54394 = ORIENTED_EDGE ( 'NONE', *, *, #39408, .F. ) ;
#54395 = DIRECTION ( 'NONE',  ( 0.000000000000000000, 0.000000000000000000, 1.000000000000000000 ) ) ;
#54396 = AXIS2_PLACEMENT_3D ( 'NONE', #29616, #12341, #42038 ) ;
#54397 = CARTESIAN_POINT ( 'NONE',  ( 0.000000000000000000, 0.000000000000000000, 0.000000000000000000 ) ) ;
#54398 = ORIENTED_EDGE ( 'NONE', *, *, #27583, .F. ) ;
#54399 = EDGE_CURVE ( 'NONE', #26840, #8961, #70278, .T. ) ;
#54400 = ORIENTED_EDGE ( 'NONE', *, *, #1175, .T. ) ;
#54401 = CARTESIAN_POINT ( 'NONE',  ( 92.35000000010803944, 90.00001510551041406, 78.64888723592453346 ) ) ;
#54402 = EDGE_CURVE ( 'NONE', #65764, #42628, #26286, .T. ) ;
#54403 = DIRECTION ( 'NONE',  ( 1.000000000000000000, 0.000000000000000000, 0.000000000000000000 ) ) ;
#54404 = CARTESIAN_POINT ( 'NONE',  ( 11.99999999999999822, 5.256550761632864166, 77.32052557432842832 ) ) ;
#54405 = EDGE_CURVE ( 'NONE', #19072, #69267, #23714, .T. ) ;
#54406 = CARTESIAN_POINT ( 'NONE',  ( -92.69370383062498320, -211.3315407142195852, 83.71614583420050337 ) ) ;
#54407 = ORIENTED_EDGE ( 'NONE', *, *, #66902, .T. ) ;
#54408 = CARTESIAN_POINT ( 'NONE',  ( 11.99999999999999822, 44.88180994100376608, 63.18004540533043922 ) ) ;
#54409 = VERTEX_POINT ( 'NONE', #37560 ) ;
#54410 = CARTESIAN_POINT ( 'NONE',  ( 10.00000000000000000, 0.000000000000000000, 0.000000000000000000 ) ) ;
#54411 = LINE ( 'NONE', #53670, #73108 ) ;
#54412 = DIRECTION ( 'NONE',  ( 1.000000000000000000, 0.000000000000000000, 0.000000000000000000 ) ) ;
#54413 = CARTESIAN_POINT ( 'NONE',  ( 94.99999999999998579, 87.33691857156068750, 77.10156250086711793 ) ) ;
#54414 = CARTESIAN_POINT ( 'NONE',  ( 10.00000000000000000, 33.00180498840046539, 17.80606268964551120 ) ) ;
#54415 = FACE_OUTER_BOUND ( 'NONE', #67725, .T. ) ;
#54416 = CARTESIAN_POINT ( 'NONE',  ( 10.00000000000000000, 0.000000000000000000, 0.000000000000000000 ) ) ;
#54417 = CARTESIAN_POINT ( 'NONE',  ( -3.000000000000000000, 14.60985201121729737, -18.46759930825687945 ) ) ;
#54418 = DIRECTION ( 'NONE',  ( 0.000000000000000000, 0.6494480483301849905, -0.7604059656000298206 ) ) ;
#54419 = CARTESIAN_POINT ( 'NONE',  ( 22.30499999999999972, 0.000000000000000000, 0.000000000000000000 ) ) ;
#54420 = AXIS2_PLACEMENT_3D ( 'NONE', #17897, #5533, #5901 ) ;
#54421 = CARTESIAN_POINT ( 'NONE',  ( 3.000000000000000000, -2.201436576420043867, 1.271000000000003904 ) ) ;
#54422 = PRODUCT_DEFINITION_CONTEXT ( 'detailed design', #40737, 'design' ) ;
#54423 = AXIS2_PLACEMENT_3D ( 'NONE', #246, #23139, #29123 ) ;
#54424 = LINE ( 'NONE', #1857, #25320 ) ;
#54425 = ORIENTED_EDGE ( 'NONE', *, *, #47480, .F. ) ;
#54426 = CARTESIAN_POINT ( 'NONE',  ( -92.69370383062505425, 91.33154071421968467, 84.29822916753380468 ) ) ;
#54427 = EDGE_CURVE ( 'NONE', #71014, #67963, #55580, .T. ) ;
#54428 = EDGE_CURVE ( 'NONE', #24421, #9962, #60492, .T. ) ;
#54429 = CYLINDRICAL_SURFACE ( 'NONE', #50347, 2.649999999999985700 ) ;
#54430 = AXIS2_PLACEMENT_3D ( 'NONE', #9127, #14026, #54629 ) ;
#54431 = DIRECTION ( 'NONE',  ( 0.000000000000000000, 0.000000000000000000, 1.000000000000000000 ) ) ;
#54432 = ADVANCED_FACE ( 'NONE', ( #55208 ), #44303, .T. ) ;
#54433 = ORIENTED_EDGE ( 'NONE', *, *, #49716, .F. ) ;
#54434 = AXIS2_PLACEMENT_3D ( 'NONE', #45318, #27638, #68244 ) ;
#54435 = CARTESIAN_POINT ( 'NONE',  ( 10.00000000000000000, -46.21855187248673502, 62.20884554314003623 ) ) ;
#54437 = DIRECTION ( 'NONE',  ( -1.000000000000000000, 0.000000000000000000, 0.000000000000000000 ) ) ;
#54436 = AXIS2_PLACEMENT_3D ( 'NONE', #31944, #28441, #45390 ) ;
#54438 = CARTESIAN_POINT ( 'NONE',  ( 11.99999999999999822, 14.67089635893713684, 73.72996012237443608 ) ) ;
#54439 = CIRCLE ( 'NONE', #18431, 31.99999999999999289 ) ;
#54440 = AXIS2_PLACEMENT_3D ( 'NONE', #19185, #24461, #69942 ) ;
#54441 = CARTESIAN_POINT ( 'NONE',  ( 96.15314808468748708, -208.0026889286704943, 79.42989583420049371 ) ) ;
#54442 = VERTEX_POINT ( 'NONE', #38666 ) ;
#54443 = ORIENTED_EDGE ( 'NONE', *, *, #55880, .T. ) ;
#54444 = DIRECTION ( 'NONE',  ( 1.000000000000000000, 0.000000000000000000, 0.000000000000000000 ) ) ;
#54445 = DIRECTION ( 'NONE',  ( 0.000000000000000000, 0.000000000000000000, -1.000000000000000000 ) ) ;
#54446 = DIRECTION ( 'NONE',  ( -1.000000000000000000, 0.000000000000000000, 0.000000000000000000 ) ) ;
#54447 = EDGE_LOOP ( 'NONE', ( #66959, #33016, #37352, #4771, #55656, #63806 ) ) ;
#54448 = FACE_OUTER_BOUND ( 'NONE', #62347, .T. ) ;
#54449 = CARTESIAN_POINT ( 'NONE',  ( 93.84685191531249870, -208.0026889286704943, 77.63072916753381492 ) ) ;
#54450 = AXIS2_PLACEMENT_3D ( 'NONE', #50683, #27757, #57448 ) ;
#54451 = ORIENTED_EDGE ( 'NONE', *, *, #18591, .T. ) ;
#54452 = CARTESIAN_POINT ( 'NONE',  ( 0.000000000000000000, 0.000000000000000000, 0.000000000000000000 ) ) ;
#54453 = ORIENTED_EDGE ( 'NONE', *, *, #47393, .T. ) ;
#54454 = VERTEX_POINT ( 'NONE', #26253 ) ;
#54455 = DIRECTION ( 'NONE',  ( -0.000000000000000000, -0.000000000000000000, 1.000000000000000000 ) ) ;
#54456 = ORIENTED_EDGE ( 'NONE', *, *, #62145, .T. ) ;
#54457 = DIRECTION ( 'NONE',  ( -1.000000000000000000, 0.000000000000000000, 0.000000000000000000 ) ) ;
#54458 = CARTESIAN_POINT ( 'NONE',  ( 97.64999999999997726, -211.5299782133524502, 82.08895833506764461 ) ) ;
#54459 = CARTESIAN_POINT ( 'NONE',  ( 94.99999999999998579, 86.94004357329500010, 84.44375000000000853 ) ) ;
#54460 = ORIENTED_EDGE ( 'NONE', *, *, #39826, .T. ) ;
#54461 = CARTESIAN_POINT ( 'NONE',  ( 96.73972734126401463, 91.51405112163766375, 74.79348190356853365 ) ) ;
#54462 = DIRECTION ( 'NONE',  ( 0.000000000000000000, 0.7071067811865439090, 0.7071067811865512365 ) ) ;
#54463 = VECTOR ( 'NONE', #8477, 1000.000000000000114 ) ;
#54464 = EDGE_LOOP ( 'NONE', ( #14333, #50490, #60665, #30128 ) ) ;
#54465 = ORIENTED_EDGE ( 'NONE', *, *, #5274, .T. ) ;
#54466 = CARTESIAN_POINT ( 'NONE',  ( -95.00000000000002842, 87.33691857156074434, 89.32531250086715602 ) ) ;
#54467 = CARTESIAN_POINT ( 'NONE',  ( 96.15314808468748708, 88.00268892867053694, 82.86947916753379673 ) ) ;
#54468 = VERTEX_POINT ( 'NONE', #37922 ) ;
#54469 = CARTESIAN_POINT ( 'NONE',  ( 92.34999999999999432, 88.47002178664753558, 81.24229166840098060 ) ) ;
#54470 = CARTESIAN_POINT ( 'NONE',  ( 92.34999999999999432, 90.00000000000002842, 80.47499999999999432 ) ) ;
#54471 = FACE_OUTER_BOUND ( 'NONE', #19378, .T. ) ;
#54472 = ORIENTED_EDGE ( 'NONE', *, *, #68671, .F. ) ;
#54473 = DIRECTION ( 'NONE',  ( 0.6691306063588569053, 0.7431448254773954654, 0.000000000000000000 ) ) ;
#54474 = ORIENTED_EDGE ( 'NONE', *, *, #24802, .F. ) ;
#54475 = CIRCLE ( 'NONE', #73679, 16.00000000000000000 ) ;
#54476 = VERTEX_POINT ( 'NONE', #60131 ) ;
#54477 = EDGE_CURVE ( 'NONE', #26154, #8157, #32260, .T. ) ;
#54478 = VERTEX_POINT ( 'NONE', #48820 ) ;
#54479 = CARTESIAN_POINT ( 'NONE',  ( 0.000000000000000000, 0.000000000000000000, 0.000000000000000000 ) ) ;
#54480 = DIRECTION ( 'NONE',  ( 0.000000000000000000, 0.5877852522924797984, 0.8090169943749426773 ) ) ;
#54481 = EDGE_CURVE ( 'NONE', #31307, #27645, #3581, .T. ) ;
#54482 = CARTESIAN_POINT ( 'NONE',  ( -93.67500000000003979, 92.29496732002878900, 84.70833333333332860 ) ) ;
#54483 = VERTEX_POINT ( 'NONE', #10082 ) ;
#54484 = DIRECTION ( 'NONE',  ( -1.000000000000000000, 0.000000000000000000, 0.000000000000000000 ) ) ;
#54485 = AXIS2_PLACEMENT_3D ( 'NONE', #53440, #71080, #54192 ) ;
#54486 =( BOUNDED_CURVE ( )  B_SPLINE_CURVE ( 2, ( #4020, #30059, #38206, #46997, #59022, #35691, #53008 ),
 .UNSPECIFIED., .F., .T. ) 
 B_SPLINE_CURVE_WITH_KNOTS ( ( 3, 2, 2, 3 ),
 ( 0.9583333333333337034, 0.9652777777777781232, 0.9722222222222225430, 0.9791666666666669627 ),
 .UNSPECIFIED. ) 
 CURVE ( )  GEOMETRIC_REPRESENTATION_ITEM ( )  RATIONAL_B_SPLINE_CURVE ( ( 0.9999999999999935607, 0.8660254037844451469, 1.000000000000000000, 0.8660254037844387076, 1.000000000000000000, 0.8660254037844322683, 1.000000000000006439 ) ) 
 REPRESENTATION_ITEM ( '' )  );
#54487 = DIRECTION ( 'NONE',  ( 1.000000000000000000, -0.000000000000000000, 0.000000000000000000 ) ) ;
#54488 = VERTEX_POINT ( 'NONE', #8973 ) ;
#54489 = CARTESIAN_POINT ( 'NONE',  ( 0.000000000000000000, 0.000000000000000000, 0.000000000000000000 ) ) ;
#54490 = CARTESIAN_POINT ( 'NONE',  ( -97.30629616937497417, -211.3315407142195852, 78.90072916753381094 ) ) ;
#54492 = VERTEX_POINT ( 'NONE', #15344 ) ;
#54491 = EDGE_CURVE ( 'NONE', #35768, #12556, #20240, .T. ) ;
#54493 = VECTOR ( 'NONE', #44925, 999.9999999999998863 ) ;
#54494 = DIRECTION ( 'NONE',  ( 1.000000000000000000, 0.000000000000000000, 0.000000000000000000 ) ) ;
#54495 = DIRECTION ( 'NONE',  ( 0.000000000000000000, 0.000000000000000000, 1.000000000000000000 ) ) ;
#54496 = CARTESIAN_POINT ( 'NONE',  ( 0.000000000000000000, -1.467624384280027838, 2.542000000000001592 ) ) ;
#54497 = CARTESIAN_POINT ( 'NONE',  ( -2.500000000000015543, -73.00000000000001421, -204.9999999999999716 ) ) ;
#54498 = EDGE_CURVE ( 'NONE', #72643, #50746, #72693, .T. ) ;
#54499 = CARTESIAN_POINT ( 'NONE',  ( 10.00000000000000000, -6.555932627142676772, 37.01155633439056203 ) ) ;
#54500 = AXIS2_PLACEMENT_3D ( 'NONE', #45289, #27970, #73081 ) ;
#54501 = AXIS2_PLACEMENT_3D ( 'NONE', #53769, #59055, #13175 ) ;
#54502 = DIRECTION ( 'NONE',  ( -0.000000000000000000, -0.000000000000000000, 1.000000000000000000 ) ) ;
#54503 = DIRECTION ( 'NONE',  ( -0.02332147558787930897, -0.9997280174009348652, 0.000000000000000000 ) ) ;
#54504 = DIRECTION ( 'NONE',  ( 1.000000000000000000, 0.000000000000000000, -0.000000000000000000 ) ) ;
#54505 = CARTESIAN_POINT ( 'NONE',  ( 0.000000000000000000, 36.13751322684419165, 21.40280677340384585 ) ) ;
#54506 = ADVANCED_FACE ( 'NONE', ( #10455 ), #29218, .T. ) ;
#54507 = DIRECTION ( 'NONE',  ( 0.7585478161175716050, 0.6516173805718067369, 0.000000000000000000 ) ) ;
#54508 = EDGE_CURVE ( 'NONE', #60065, #61902, #38088, .T. ) ;
#54509 = CARTESIAN_POINT ( 'NONE',  ( -97.30629616937501680, 90.00000000000004263, 75.03781250086713328 ) ) ;
#54510 = CARTESIAN_POINT ( 'NONE',  ( 11.99999999999999822, 0.000000000000000000, 0.000000000000000000 ) ) ;
#54511 = CARTESIAN_POINT ( 'NONE',  ( 5.822613034544236399, -142.8165987265839760, -5.500000000000000000 ) ) ;
#54512 =( BOUNDED_CURVE ( )  B_SPLINE_CURVE ( 2, ( #38956, #68273, #67898, #26917, #44607, #67149, #73520 ),
 .UNSPECIFIED., .F., .F. ) 
 B_SPLINE_CURVE_WITH_KNOTS ( ( 3, 2, 2, 3 ),
 ( 0.8958333333333331483, 0.9027777777777775681, 0.9097222222222218768, 0.9166666666666662966 ),
 .UNSPECIFIED. ) 
 CURVE ( )  GEOMETRIC_REPRESENTATION_ITEM ( )  RATIONAL_B_SPLINE_CURVE ( ( 1.000000000000004219, 0.8660254037844343777, 1.000000000000000000, 0.8660254037844387076, 1.000000000000000000, 0.8660254037844451469, 0.9999999999999935607 ) ) 
 REPRESENTATION_ITEM ( '' )  );
#54513 = FACE_OUTER_BOUND ( 'NONE', #4194, .T. ) ;
#54514 = FACE_OUTER_BOUND ( 'NONE', #63222, .T. ) ;
#54515 = CONICAL_SURFACE ( 'NONE', #28098, 17.30399999999999849, 0.2094395102393129815 ) ;
#54516 = CARTESIAN_POINT ( 'NONE',  ( 0.000000000000000000, 40.68715046381943523, -10.41901085202036370 ) ) ;
#54517 = CARTESIAN_POINT ( 'NONE',  ( -9.055038557894883766, -98.31460683512894150, -2.500000000000000000 ) ) ;
#54518 = EDGE_CURVE ( 'NONE', #13842, #68033, #62354, .T. ) ;
#54519 = EDGE_CURVE ( 'NONE', #61799, #70823, #44688, .T. ) ;
#54520 = CARTESIAN_POINT ( 'NONE',  ( -22.53294031248082163, -134.0273518838794757, 5.500000000000000000 ) ) ;
#54521 = CARTESIAN_POINT ( 'NONE',  ( 6.000000000000000000, 40.65526001592611749, 71.21200624218811015 ) ) ;
#54522 = CARTESIAN_POINT ( 'NONE',  ( -96.32499999999996021, -207.7050326799711968, 89.25916666666667254 ) ) ;
#54523 = LINE ( 'NONE', #25941, #56627 ) ;
#54524 = EDGE_LOOP ( 'NONE', ( #13492, #69169, #64665, #20732 ) ) ;
#54525 = DIRECTION ( 'NONE',  ( -1.000000000000000000, 0.000000000000000000, 0.000000000000000000 ) ) ;
#54526 = FACE_OUTER_BOUND ( 'NONE', #583, .T. ) ;
#54527 = CARTESIAN_POINT ( 'NONE',  ( 95.00000000000000000, -206.9400435732949575, 81.66562500173431260 ) ) ;
#54528 = DIRECTION ( 'NONE',  ( 0.3311129884571281101, 0.9435911131814402886, 0.000000000000000000 ) ) ;
#54529 = AXIS2_PLACEMENT_3D ( 'NONE', #20334, #14691, #54918 ) ;
#54530 = EDGE_LOOP ( 'NONE', ( #18775, #5187, #59187, #17017 ) ) ;
#54531 = CARTESIAN_POINT ( 'NONE',  ( -97.65000000000001990, 90.00000000000004263, 81.10999999999999943 ) ) ;
#54532 = DIRECTION ( 'NONE',  ( 1.000000000000000000, 0.000000000000000000, 0.000000000000000000 ) ) ;
#54533 = ORIENTED_EDGE ( 'NONE', *, *, #27792, .T. ) ;
#54534 = CIRCLE ( 'NONE', #26888, 82.00000000000000000 ) ;
#54535 = CARTESIAN_POINT ( 'NONE',  ( 96.15314808468750130, -211.9973110713294489, 81.59947916753381492 ) ) ;
#54536 = CARTESIAN_POINT ( 'NONE',  ( 95.00000000000000000, -212.6630814284392557, 89.32531250086715602 ) ) ;
#54537 = AXIS2_PLACEMENT_3D ( 'NONE', #7561, #59810, #54528 ) ;
#54538 = VERTEX_POINT ( 'NONE', #46160 ) ;
#54539 = CARTESIAN_POINT ( 'NONE',  ( 95.00000000000000000, -207.3369185715606307, 87.10281250086715943 ) ) ;
#54540 = ORIENTED_EDGE ( 'NONE', *, *, #56809, .T. ) ;
#54541 = AXIS2_PLACEMENT_3D ( 'NONE', #18990, #1018, #46106 ) ;
#54542 = CARTESIAN_POINT ( 'NONE',  ( 0.000000000000000000, -120.0000000000000000, 2.500000000000000000 ) ) ;
#54543 = ORIENTED_EDGE ( 'NONE', *, *, #45434, .T. ) ;
#54544 = AXIS2_PLACEMENT_3D ( 'NONE', #11077, #57688, #68965 ) ;
#54545 = CARTESIAN_POINT ( 'NONE',  ( -97.30629616937501680, 88.66845928578038638, 77.78947916753381264 ) ) ;
#54546 = ORIENTED_EDGE ( 'NONE', *, *, #57536, .T. ) ;
#54547 = ORIENTED_EDGE ( 'NONE', *, *, #33106, .T. ) ;
#54548 = DIRECTION ( 'NONE',  ( -1.000000000000000000, 0.000000000000000000, 0.000000000000000000 ) ) ;
#54549 = ORIENTED_EDGE ( 'NONE', *, *, #56857, .T. ) ;
#54550 = CARTESIAN_POINT ( 'NONE',  ( -12.40464318976452596, 10.41032311384371489, 42.00000000000001421 ) ) ;
#54551 = LINE ( 'NONE', #24501, #10422 ) ;
#54552 = EDGE_CURVE ( 'NONE', #26000, #48188, #38630, .T. ) ;
#54553 = VERTEX_POINT ( 'NONE', #45051 ) ;
#54554 = DIRECTION ( 'NONE',  ( 0.000000000000000000, -1.000000000000000000, -1.040834085586084730E-14 ) ) ;
#54555 = EDGE_CURVE ( 'NONE', #68902, #46309, #11932, .T. ) ;
#54556 = ORIENTED_EDGE ( 'NONE', *, *, #30736, .T. ) ;
#54557 = CARTESIAN_POINT ( 'NONE',  ( 10.00000000000000000, 81.90746397400388901, 3.894527615418187150 ) ) ;
#54558 = PRODUCT_RELATED_PRODUCT_CATEGORY ( 'part', '', ( #14543 ) ) ;
#54559 = ORIENTED_EDGE ( 'NONE', *, *, #64917, .T. ) ;
#54560 = CIRCLE ( 'NONE', #36577, 21.00000000000000000 ) ;
#54561 = EDGE_CURVE ( 'NONE', #68066, #61610, #16854, .T. ) ;
#54562 = ORIENTED_EDGE ( 'NONE', *, *, #11109, .T. ) ;
#54563 = ORIENTED_EDGE ( 'NONE', *, *, #63957, .T. ) ;
#54564 = CARTESIAN_POINT ( 'NONE',  ( 93.84685191531249870, -208.0026889286704943, 80.01197916753380923 ) ) ;
#54565 = DIRECTION ( 'NONE',  ( -1.000000000000000000, 0.000000000000000000, 0.000000000000000000 ) ) ;
#54566 = CONTEXT_DEPENDENT_SHAPE_REPRESENTATION ( #22509, #6841 ) ;
#54567 = CARTESIAN_POINT ( 'NONE',  ( 0.3000000000000016542, 0.000000000000000000, 5.000000000000000000 ) ) ;
#54568 = ORIENTED_EDGE ( 'NONE', *, *, #47349, .T. ) ;
#54569 = ORIENTED_EDGE ( 'NONE', *, *, #2905, .F. ) ;
#54570 = CARTESIAN_POINT ( 'NONE',  ( 10.00000000000000000, -67.80270845531855173, -46.11716303203261447 ) ) ;
#54571 = EDGE_CURVE ( 'NONE', #13817, #2580, #65036, .T. ) ;
#54572 = ORIENTED_EDGE ( 'NONE', *, *, #16751, .F. ) ;
#54573 = CARTESIAN_POINT ( 'NONE',  ( -235.0000123116479926, -123.0000000000000284, -2.500000000000000000 ) ) ;
#54574 = DIRECTION ( 'NONE',  ( -1.000000000000000000, 0.000000000000000000, 0.000000000000000000 ) ) ;
#54575 = ADVANCED_FACE ( 'NONE', ( #48462 ), #5955, .F. ) ;
#54576 = CARTESIAN_POINT ( 'NONE',  ( -95.00000000000002842, 87.33691857156074434, 79.16531250086715943 ) ) ;
#54577 = ORIENTED_EDGE ( 'NONE', *, *, #35333, .F. ) ;
#54578 = CARTESIAN_POINT ( 'NONE',  ( 93.84685191531248449, 88.00268892867053694, 78.95364583420047211 ) ) ;
#54579 = VERTEX_POINT ( 'NONE', #27749 ) ;
#54580 = CARTESIAN_POINT ( 'NONE',  ( 15.00000000000000000, 22.07842321921480888, -8.187992925817425771 ) ) ;
#54581 = DIRECTION ( 'NONE',  ( 0.000000000000000000, -0.5224985647159559043, 0.8526401643540879594 ) ) ;
#54582 = EDGE_CURVE ( 'NONE', #54579, #70, #35024, .T. ) ;
#54583 = CARTESIAN_POINT ( 'NONE',  ( 6.000000000000000000, 8.966570791700705811, 81.50828551894228724 ) ) ;
#54584 = CARTESIAN_POINT ( 'NONE',  ( -26.53422223201112828, -120.6595836127786043, 5.500000000000000000 ) ) ;
#54585 = DIRECTION ( 'NONE',  ( -1.000000000000000000, -0.000000000000000000, 0.000000000000000000 ) ) ;
#54586 = VECTOR ( 'NONE', #37877, 1000.000000000000000 ) ;
#54587 = CARTESIAN_POINT ( 'NONE',  ( -92.69370383062498320, -208.6684592857803295, 84.29822916753380468 ) ) ;
#54588 = CARTESIAN_POINT ( 'NONE',  ( -2.977765906491215642, 0.000000000000000000, 0.000000000000000000 ) ) ;
#54589 = CARTESIAN_POINT ( 'NONE',  ( 10.00000000000000000, 0.000000000000000000, 0.000000000000000000 ) ) ;
#54590 = DIRECTION ( 'NONE',  ( 1.000000000000000000, 0.000000000000000000, -0.000000000000000000 ) ) ;
#54591 = ORIENTED_EDGE ( 'NONE', *, *, #28612, .T. ) ;
#54592 = VECTOR ( 'NONE', #32628, 1000.000000000000000 ) ;
#54593 = VERTEX_POINT ( 'NONE', #28863 ) ;
#54594 = DIRECTION ( 'NONE',  ( -1.000000000000000000, 0.000000000000000000, 0.000000000000000000 ) ) ;
#54595 = CARTESIAN_POINT ( 'NONE',  ( -96.32500000000001705, 87.70503267997129626, 76.13583333333333769 ) ) ;
#54596 = ADVANCED_FACE ( 'NONE', ( #39784, #5213 ), #33758, .T. ) ;
#54597 = CARTESIAN_POINT ( 'NONE',  ( -97.64999999980591383, 89.99998015682162134, 84.36502760998403971 ) ) ;
#54598 = EDGE_CURVE ( 'NONE', #2735, #16527, #66270, .T. ) ;
#54599 = CARTESIAN_POINT ( 'NONE',  ( -95.00000000000002842, 87.33691857156074434, 84.72156250086713669 ) ) ;
#54600 = CARTESIAN_POINT ( 'NONE',  ( 10.00000000000000000, 0.000000000000000000, 0.000000000000000000 ) ) ;
#54601 = CARTESIAN_POINT ( 'NONE',  ( 5.000000000000002665, -71.21200624218825226, 40.65526001592589722 ) ) ;
#54602 = CYLINDRICAL_SURFACE ( 'NONE', #73201, 3.299999999999969624 ) ;
#54603 = VECTOR ( 'NONE', #15787, 1000.000000000000000 ) ;
#54604 = VERTEX_POINT ( 'NONE', #56712 ) ;
#54605 = VECTOR ( 'NONE', #41436, 1000.000000000000000 ) ;
#54606 = DIRECTION ( 'NONE',  ( -1.000000000000000000, 0.000000000000000000, 0.000000000000000000 ) ) ;
#54607 = LINE ( 'NONE', #62490, #27341 ) ;
#54608 = DIRECTION ( 'NONE',  ( 0.000000000000000000, 0.000000000000000000, 1.000000000000000000 ) ) ;
#54609 = DIRECTION ( 'NONE',  ( -1.000000000000000000, 7.571544473058805744E-15, 2.612289469705706870E-14 ) ) ;
#54610 = DIRECTION ( 'NONE',  ( 0.000000000000000000, -0.9876883405951359940, -0.1564344650402420545 ) ) ;
#54611 = CARTESIAN_POINT ( 'NONE',  ( 96.32499999999998863, 87.70503267997126784, 86.40166666666667084 ) ) ;
#54612 = CARTESIAN_POINT ( 'NONE',  ( -94.99999999999997158, -212.6630814284392557, 83.61031250086716682 ) ) ;
#54613 = CARTESIAN_POINT ( 'NONE',  ( 0.000000000000000000, 0.000000000000000000, 0.000000000000000000 ) ) ;
#54614 = AXIS2_PLACEMENT_3D ( 'NONE', #49741, #39227, #20811 ) ;
#54615 = CARTESIAN_POINT ( 'NONE',  ( -10.90076147243505211, 0.000000000000000000, 0.000000000000000000 ) ) ;
#54616 = VECTOR ( 'NONE', #41919, 1000.000000000000000 ) ;
#54617 = CARTESIAN_POINT ( 'NONE',  ( 0.000000000000000000, 0.000000000000000000, 0.000000000000000000 ) ) ;
#54618 = CYLINDRICAL_SURFACE ( 'NONE', #69388, 37.49900000000000233 ) ;
#54619 = VERTEX_POINT ( 'NONE', #22490 ) ;
#54620 = DIRECTION ( 'NONE',  ( 0.000000000000000000, 0.000000000000000000, 1.000000000000000000 ) ) ;
#54621 = CARTESIAN_POINT ( 'NONE',  ( -92.35000000000003695, 90.00000000000004263, 78.25249999999999773 ) ) ;
#54622 = DIRECTION ( 'NONE',  ( 0.000000000000000000, -0.000000000000000000, -1.000000000000000000 ) ) ;
#54623 =( BOUNDED_CURVE ( )  B_SPLINE_CURVE ( 2, ( #49965, #33417, #33047, #55988, #5624, #68020, #72886 ),
 .UNSPECIFIED., .F., .F. ) 
 B_SPLINE_CURVE_WITH_KNOTS ( ( 3, 2, 2, 3 ),
 ( 0.9166666666666662966, 0.9236111111111108274, 0.9305555555555551361, 0.9374999999999995559 ),
 .UNSPECIFIED. ) 
 CURVE ( )  GEOMETRIC_REPRESENTATION_ITEM ( )  RATIONAL_B_SPLINE_CURVE ( ( 1.000000000000006439, 0.8660254037844322683, 1.000000000000000000, 0.8660254037844387076, 1.000000000000000000, 0.8660254037844472563, 0.9999999999999914513 ) ) 
 REPRESENTATION_ITEM ( '' )  );
#54624 = DIRECTION ( 'NONE',  ( 0.000000000000000000, -0.9876883405951358830, -0.1564344650402420822 ) ) ;
#54625 = ORIENTED_EDGE ( 'NONE', *, *, #23838, .F. ) ;
#54626 = CARTESIAN_POINT ( 'NONE',  ( 10.00000000000000000, -14.66109333815513160, 73.73191006444567108 ) ) ;
#54627 =( NAMED_UNIT ( * ) PLANE_ANGLE_UNIT ( ) SI_UNIT ( $, .RADIAN. ) );
#54628 = EDGE_LOOP ( 'NONE', ( #26381, #18024, #41074, #70195 ) ) ;
#54629 = DIRECTION ( 'NONE',  ( 0.000000000000000000, 0.000000000000000000, 1.000000000000000000 ) ) ;
#54630 = EDGE_LOOP ( 'NONE', ( #70603, #2762, #51196, #52459 ) ) ;
#54631 = EDGE_CURVE ( 'NONE', #42391, #68050, #45430, .T. ) ;
#54632 = DIRECTION ( 'NONE',  ( -1.000000000000000000, 0.000000000000000000, -0.000000000000000000 ) ) ;
#54633 = VECTOR ( 'NONE', #14516, 1000.000000000000227 ) ;
#54634 = VERTEX_POINT ( 'NONE', #57076 ) ;
#54635 = VERTEX_POINT ( 'NONE', #23970 ) ;
#54636 = EDGE_CURVE ( 'NONE', #1681, #2580, #58925, .T. ) ;
#54637 = VERTEX_POINT ( 'NONE', #25067 ) ;
#54638 = ORIENTED_EDGE ( 'NONE', *, *, #2815, .F. ) ;
#54639 = CARTESIAN_POINT ( 'NONE',  ( 10.00000000000000000, -16.65560815589383381, -38.55633173627028754 ) ) ;
#54640 = EDGE_CURVE ( 'NONE', #15499, #19508, #39816, .T. ) ;
#54641 = VERTEX_POINT ( 'NONE', #2182 ) ;
#54642 = ORIENTED_EDGE ( 'NONE', *, *, #10933, .T. ) ;
#54643 = CARTESIAN_POINT ( 'NONE',  ( 97.30629616937498838, 90.00000000000002842, 81.22906250086715829 ) ) ;
#54644 = VECTOR ( 'NONE', #40482, 1000.000000000000000 ) ;
#54645 = CARTESIAN_POINT ( 'NONE',  ( 11.99999999999999822, -14.67089635893658794, -73.72996012237454977 ) ) ;
#54647 = DIRECTION ( 'NONE',  ( -1.000000000000000000, -0.000000000000000000, -0.000000000000000000 ) ) ;
#54646 = CIRCLE ( 'NONE', #3054, 77.49900000000000944 ) ;
#54648 = ORIENTED_EDGE ( 'NONE', *, *, #67246, .F. ) ;
#54649 = EDGE_CURVE ( 'NONE', #1126, #2080, #60220, .T. ) ;
#54650 = ORIENTED_EDGE ( 'NONE', *, *, #19748, .T. ) ;
#54651 = ORIENTED_EDGE ( 'NONE', *, *, #47294, .T. ) ;
#54652 = LINE ( 'NONE', #24966, #52657 ) ;
#54653 = ORIENTED_EDGE ( 'NONE', *, *, #35702, .T. ) ;
#54654 = AXIS2_PLACEMENT_3D ( 'NONE', #5358, #51191, #74125 ) ;
#54655 = DIRECTION ( 'NONE',  ( 0.9634709561335031980, -0.2678128389140318477, 0.000000000000000000 ) ) ;
#54656 = DIRECTION ( 'NONE',  ( -0.000000000000000000, -0.3090169943749448977, -0.9510565162951543083 ) ) ;
#54657 = DIRECTION ( 'NONE',  ( 0.000000000000000000, -0.9876883405951394357, 0.1564344650402205716 ) ) ;
#54658 = DIRECTION ( 'NONE',  ( -0.000000000000000000, -0.000000000000000000, 1.000000000000000000 ) ) ;
#54659 = DIRECTION ( 'NONE',  ( 0.000000000000000000, 1.224646799147351482E-16, 1.000000000000000000 ) ) ;
#54660 = VECTOR ( 'NONE', #27779, 1000.000000000000000 ) ;
#54661 = CARTESIAN_POINT ( 'NONE',  ( 10.00000000000000000, 30.00120703465236716, -22.64427369931138756 ) ) ;
#54662 = FACE_OUTER_BOUND ( 'NONE', #37909, .T. ) ;
#54663 = CARTESIAN_POINT ( 'NONE',  ( -96.15314808468747287, -208.0026889286704943, 89.53697916753381492 ) ) ;
#54664 = DIRECTION ( 'NONE',  ( 0.000000000000000000, 0.8090169943749486725, -0.5877852522924713607 ) ) ;
#54665 = ORIENTED_EDGE ( 'NONE', *, *, #28509, .F. ) ;
#54666 =( REPRESENTATION_RELATIONSHIP ('NONE','NONE', #31117, #23018 ) REPRESENTATION_RELATIONSHIP_WITH_TRANSFORMATION ( #55676 )SHAPE_REPRESENTATION_RELATIONSHIP( ) );
#54668 = CARTESIAN_POINT ( 'NONE',  ( -97.30629616937501680, 88.66845928578038638, 87.79072916753381151 ) ) ;
#54667 = CARTESIAN_POINT ( 'NONE',  ( 96.32499999999997442, 92.29496732002878900, 75.89770833506763381 ) ) ;
#54669 = ORIENTED_EDGE ( 'NONE', *, *, #5947, .T. ) ;
#54670 = CARTESIAN_POINT ( 'NONE',  ( 92.69370383062498320, 90.00000000000002842, 75.19656250086714522 ) ) ;
#54671 = EDGE_CURVE ( 'NONE', #8248, #53177, #63863, .T. ) ;
#54672 = DIRECTION ( 'NONE',  ( 0.000000000000000000, 0.000000000000000000, 1.000000000000000000 ) ) ;
#54673 = CARTESIAN_POINT ( 'NONE',  ( 96.32499999999998863, -212.2949673200287179, 87.67166666666666686 ) ) ;
#54674 = DIRECTION ( 'NONE',  ( 0.000000000000000000, 0.000000000000000000, 1.000000000000000000 ) ) ;
#54675 = AXIS2_PLACEMENT_3D ( 'NONE', #16679, #39616, #27581 ) ;
#54676 = CARTESIAN_POINT ( 'NONE',  ( -92.35000000000005116, 91.52997821335253548, 78.38479166840096468 ) ) ;
#54677 = DIRECTION ( 'NONE',  ( -1.000000000000000000, -0.000000000000000000, 0.000000000000000000 ) ) ;
#54678 = CARTESIAN_POINT ( 'NONE',  ( 25.44550000000002399, 0.000000000000000000, 3.000000000000000444 ) ) ;
#54679 = FACE_OUTER_BOUND ( 'NONE', #40694, .T. ) ;
#54680 = VERTEX_POINT ( 'NONE', #46905 ) ;
#54681 = VECTOR ( 'NONE', #66359, 1000.000000000000000 ) ;
#54682 = VERTEX_POINT ( 'NONE', #13413 ) ;
#54683 = ADVANCED_FACE ( 'NONE', ( #36344 ), #59287, .F. ) ;
#54684 = DIRECTION ( 'NONE',  ( 0.000000000000000000, 0.000000000000000000, 1.000000000000000000 ) ) ;
#54685 = EDGE_CURVE ( 'NONE', #62821, #51135, #7780, .T. ) ;
#54686 = DIRECTION ( 'NONE',  ( 0.000000000000000000, 0.000000000000000000, 1.000000000000000000 ) ) ;
#54687 = DIRECTION ( 'NONE',  ( -1.000000000000000000, -0.000000000000000000, 0.000000000000000000 ) ) ;
#54688 = DIRECTION ( 'NONE',  ( -0.9966891607226786576, -0.08130631524009861166, 0.000000000000000000 ) ) ;
#54689 = LINE ( 'NONE', #26105, #56548 ) ;
#54690 = DIRECTION ( 'NONE',  ( 0.000000000000000000, 0.000000000000000000, 1.000000000000000000 ) ) ;
#54691 = ADVANCED_FACE ( 'NONE', ( #70920 ), #46523, .F. ) ;
#54692 = ORIENTED_EDGE ( 'NONE', *, *, #1973, .T. ) ;
#54693 = CARTESIAN_POINT ( 'NONE',  ( -96.15314808468752972, 91.99731107132950569, 83.18697916753382060 ) ) ;
#54694 = CARTESIAN_POINT ( 'NONE',  ( -6.782329983125270800, 10.49999999999999467, -125.0000000000000000 ) ) ;
#54695 = CIRCLE ( 'NONE', #25858, 15.69999999999999929 ) ;
#54696 = DIRECTION ( 'NONE',  ( -0.000000000000000000, -0.000000000000000000, 1.000000000000000000 ) ) ;
#54697 = LINE ( 'NONE', #38143, #2206 ) ;
#54698 = DIRECTION ( 'NONE',  ( 0.000000000000000000, 0.000000000000000000, -1.000000000000000000 ) ) ;
#54699 = CARTESIAN_POINT ( 'NONE',  ( 6.000000000000000000, 78.73519480814955784, 22.90783923731656557 ) ) ;
#54700 = CARTESIAN_POINT ( 'NONE',  ( 0.000000000000000000, -41.19522573413780009, 65.64334221924896440 ) ) ;
#54701 = LINE ( 'NONE', #67087, #64090 ) ;
#54702 = FACE_OUTER_BOUND ( 'NONE', #36776, .T. ) ;
#54703 = VECTOR ( 'NONE', #44516, 1000.000000000000000 ) ;
#54704 = CARTESIAN_POINT ( 'NONE',  ( 92.69370383062498320, 90.00000000000002842, 82.81656250086714977 ) ) ;
#54705 = CARTESIAN_POINT ( 'NONE',  ( -97.30629616937497417, -211.3315407142195852, 81.59947916753382913 ) ) ;
#54706 = CARTESIAN_POINT ( 'NONE',  ( 15.87720740287354459, 0.000000000000000000, 0.000000000000000000 ) ) ;
#54707 = EDGE_LOOP ( 'NONE', ( #50669, #25682, #31171, #43319 ) ) ;
#54708 = CARTESIAN_POINT ( 'NONE',  ( -93.67499999999998295, -212.2949673200287179, 81.32166666666667254 ) ) ;
#54709 = CARTESIAN_POINT ( 'NONE',  ( -92.34999999999999432, -209.9999999999999716, 77.61749999999999261 ) ) ;
#54710 = CARTESIAN_POINT ( 'NONE',  ( 10.00000000000000000, -37.01155633439063308, 6.555932627142289526 ) ) ;
#54711 = VECTOR ( 'NONE', #65579, 1000.000000000000114 ) ;
#54712 = AXIS2_PLACEMENT_3D ( 'NONE', #39728, #73916, #15291 ) ;
#54713 = CARTESIAN_POINT ( 'NONE',  ( 96.15314808468748708, -208.0026889286704943, 83.71614583420047495 ) ) ;
#54714 = EDGE_LOOP ( 'NONE', ( #19969, #24240, #71583, #35692 ) ) ;
#54715 = CIRCLE ( 'NONE', #22308, 2.650000000000540812 ) ;
#54716 = FACE_OUTER_BOUND ( 'NONE', #58728, .T. ) ;
#54717 = ORIENTED_EDGE ( 'NONE', *, *, #34797, .T. ) ;
#54718 = VECTOR ( 'NONE', #3474, 1000.000000000000000 ) ;
#54719 =( BOUNDED_CURVE ( )  B_SPLINE_CURVE ( 2, ( #14533, #8899, #61154, #60781, #42742, #60417, #54391 ),
 .UNSPECIFIED., .F., .F. ) 
 B_SPLINE_CURVE_WITH_KNOTS ( ( 3, 2, 2, 3 ),
 ( 0.06249999999999966693, 0.06944444444444407283, 0.07638888888888849260, 0.08333333333333288462 ),
 .UNSPECIFIED. ) 
 CURVE ( )  GEOMETRIC_REPRESENTATION_ITEM ( )  RATIONAL_B_SPLINE_CURVE ( ( 1.000000000000006439, 0.8660254037844322683, 1.000000000000000000, 0.8660254037844387076, 1.000000000000000000, 0.8660254037844472563, 0.9999999999999914513 ) ) 
 REPRESENTATION_ITEM ( '' )  );
#54720 = CARTESIAN_POINT ( 'NONE',  ( -92.34999999999999432, -208.4700217866474645, 75.84479166840098685 ) ) ;
#54721 = ORIENTED_EDGE ( 'NONE', *, *, #7118, .T. ) ;
#54722 = EDGE_CURVE ( 'NONE', #71560, #10365, #37450, .T. ) ;
#54723 = DIRECTION ( 'NONE',  ( 1.000000000000000000, 0.000000000000000000, 0.000000000000000000 ) ) ;
#54724 = AXIS2_PLACEMENT_3D ( 'NONE', #20419, #21138, #49351 ) ;
#54725 = EDGE_CURVE ( 'NONE', #68556, #59175, #53057, .T. ) ;
#54726 = ORIENTED_EDGE ( 'NONE', *, *, #8804, .T. ) ;
#54727 = CARTESIAN_POINT ( 'NONE',  ( 93.84685191531251292, -211.9973110713294489, 79.11239583420048405 ) ) ;
#54728 = ADVANCED_FACE ( 'NONE', ( #41258 ), #13777, .T. ) ;
#54729 = DIRECTION ( 'NONE',  ( -1.000000000000000000, -0.000000000000000000, 0.000000000000000000 ) ) ;
#54730 = CARTESIAN_POINT ( 'NONE',  ( -97.64996284860750109, 91.52999966271900689, 76.69145685134847668 ) ) ;
#54731 = DIRECTION ( 'NONE',  ( 0.000000000000000000, 0.8526401643540936215, -0.5224985647159469115 ) ) ;
#54732 = CARTESIAN_POINT ( 'NONE',  ( 5.999999999999999112, 59.75363087400076267, 56.15606465354979093 ) ) ;
#54733 = DIRECTION ( 'NONE',  ( -0.000000000000000000, -0.000000000000000000, 1.000000000000000000 ) ) ;
#54734 = CARTESIAN_POINT ( 'NONE',  ( 92.35000000000002274, -208.4700217866474645, 81.69208333333332916 ) ) ;
#54735 = ORIENTED_EDGE ( 'NONE', *, *, #55330, .F. ) ;
#54736 = EDGE_CURVE ( 'NONE', #18846, #23196, #63830, .T. ) ;
#54737 = ORIENTED_EDGE ( 'NONE', *, *, #38543, .T. ) ;
#54738 = ORIENTED_EDGE ( 'NONE', *, *, #24554, .F. ) ;
#54739 = ORIENTED_EDGE ( 'NONE', *, *, #21457, .F. ) ;
#54740 = CARTESIAN_POINT ( 'NONE',  ( -94.99999999999997158, -213.0599564267049857, 86.42812500173430124 ) ) ;
#54741 =( NAMED_UNIT ( * ) SI_UNIT ( $, .STERADIAN. ) SOLID_ANGLE_UNIT ( ) );
#54742 = CARTESIAN_POINT ( 'NONE',  ( -97.30629616937501680, 88.66845928578038638, 84.13947916753383538 ) ) ;
#54743 = CARTESIAN_POINT ( 'NONE',  ( 93.67499999999999716, 87.70503267997126784, 88.28020833506764120 ) ) ;
#54744 = DIRECTION ( 'NONE',  ( -1.000000000000000000, -0.000000000000000000, -0.000000000000000000 ) ) ;
#54745 = CARTESIAN_POINT ( 'NONE',  ( 94.99999999999998579, 93.05995642670504253, 76.50624999999999432 ) ) ;
#54746 = CARTESIAN_POINT ( 'NONE',  ( 0.000000000000000000, 65.58780272294129077, -36.73666225445822420 ) ) ;
#54747 = ORIENTED_EDGE ( 'NONE', *, *, #213, .F. ) ;
#54748 = CARTESIAN_POINT ( 'NONE',  ( -92.34999999999999432, -209.9999999999999716, 85.31687500173428873 ) ) ;
#54749 = ORIENTED_EDGE ( 'NONE', *, *, #58716, .T. ) ;
#54750 = LINE ( 'NONE', #72758, #11049 ) ;
#54751 = EDGE_CURVE ( 'NONE', #42459, #38362, #33838, .T. ) ;
#54752 = ORIENTED_EDGE ( 'NONE', *, *, #39423, .F. ) ;
#54753 = CARTESIAN_POINT ( 'NONE',  ( -97.65000000000001990, 88.47002178664754979, 84.41729166840097776 ) ) ;
#54754 = VERTEX_POINT ( 'NONE', #52521 ) ;
#54755 = CARTESIAN_POINT ( 'NONE',  ( 92.69370383062498320, 91.33154071421968467, 88.47864583420047779 ) ) ;
#54756 = EDGE_CURVE ( 'NONE', #47170, #37739, #36695, .T. ) ;
#54757 = CIRCLE ( 'NONE', #7903, 31.99999999999998579 ) ;
#54758 = DIRECTION ( 'NONE',  ( -1.000000000000000000, -0.000000000000000000, -0.000000000000000000 ) ) ;
#54759 = FACE_OUTER_BOUND ( 'NONE', #37642, .T. ) ;
#54760 = CARTESIAN_POINT ( 'NONE',  ( -93.23660927304929658, 88.50623689698963403, 74.79348190356844839 ) ) ;
#54761 = CARTESIAN_POINT ( 'NONE',  ( -3.360000000000002096, 2.571758278209441661E-15, 21.00000000000000000 ) ) ;
#54762 = CYLINDRICAL_SURFACE ( 'NONE', #121, 42.00000000000000000 ) ;
#54763 = EDGE_LOOP ( 'NONE', ( #35770, #52846, #7222, #55934 ) ) ;
#54764 = DIRECTION ( 'NONE',  ( -1.000000000000000000, 0.000000000000000000, -0.000000000000000000 ) ) ;
#54765 = ORIENTED_EDGE ( 'NONE', *, *, #15779, .T. ) ;
#54766 = AXIS2_PLACEMENT_3D ( 'NONE', #14956, #65087, #26227 ) ;
#54767 = VERTEX_POINT ( 'NONE', #7417 ) ;
#54769 = DIRECTION ( 'NONE',  ( 0.000000000000000000, -0.07845909572783053842, -0.9969173337331290741 ) ) ;
#54768 = VECTOR ( 'NONE', #59226, 1000.000000000000000 ) ;
#54770 = ADVANCED_FACE ( 'NONE', ( #47631 ), #70539, .T. ) ;
#54771 = PRODUCT_DEFINITION_SHAPE ( 'NONE', 'NONE',  #53621 ) ;
#54772 = CARTESIAN_POINT ( 'NONE',  ( -2.977765906491215642, 0.000000000000000000, 0.000000000000000000 ) ) ;
#54773 = EDGE_CURVE ( 'NONE', #21073, #27990, #20906, .T. ) ;
#54774 = CIRCLE ( 'NONE', #24762, 19.21700905503013601 ) ;
#54775 = VECTOR ( 'NONE', #39529, 1000.000000000000000 ) ;
#54776 = DIRECTION ( 'NONE',  ( 0.000000000000000000, 0.000000000000000000, 1.000000000000000000 ) ) ;
#54777 = CARTESIAN_POINT ( 'NONE',  ( -97.30629616937497417, -211.3315407142195852, 86.04447916753382231 ) ) ;
#54778 = VERTEX_POINT ( 'NONE', #37096 ) ;
#54779 = PLANE ( 'NONE',  #21299 ) ;
#54780 = EDGE_LOOP ( 'NONE', ( #22070, #16636, #25905, #39950, #11283 ) ) ;
#54781 = DIRECTION ( 'NONE',  ( 1.000000000000000000, -0.000000000000000000, -0.000000000000000000 ) ) ;
#54782 = CARTESIAN_POINT ( 'NONE',  ( 0.000000000000000000, 0.000000000000000000, 0.000000000000000000 ) ) ;
#54783 = CARTESIAN_POINT ( 'NONE',  ( -97.64999999999996305, -209.9999872707217037, 76.10937456147250657 ) ) ;
#54784 = CARTESIAN_POINT ( 'NONE',  ( 92.69370383062498320, 90.00000000000002842, 77.57781250086713953 ) ) ;
#54785 = DIRECTION ( 'NONE',  ( -1.000000000000000000, -0.000000000000000000, 0.000000000000000000 ) ) ;
#54786 = CARTESIAN_POINT ( 'NONE',  ( -97.65000000000001990, 90.00000000000004263, 89.36499999999999488 ) ) ;
#54787 = DIRECTION ( 'NONE',  ( 0.000000000000000000, 0.000000000000000000, -1.000000000000000000 ) ) ;
#54788 = DIRECTION ( 'NONE',  ( -1.000000000000000000, 0.000000000000000000, -0.000000000000000000 ) ) ;
#54789 = LINE ( 'NONE', #73551, #14808 ) ;
#54790 = DIRECTION ( 'NONE',  ( 0.000000000000000000, 0.000000000000000000, -1.000000000000000000 ) ) ;
#54791 = FACE_OUTER_BOUND ( 'NONE', #58759, .T. ) ;
#54792 = DIRECTION ( 'NONE',  ( 0.000000000000000000, 0.8660254037844380415, -0.5000000000000009992 ) ) ;
#54793 = ORIENTED_EDGE ( 'NONE', *, *, #46008, .F. ) ;
#54794 = CARTESIAN_POINT ( 'NONE',  ( -93.84685191531254134, 91.99731107132950569, 82.44614583420046472 ) ) ;
#54795 = B_SPLINE_CURVE_WITH_KNOTS ( 'NONE', 3,
 ( #58517, #7012, #17557, #40874, #28840, #18657, #51776, #24316, #320, #29559 ),
 .UNSPECIFIED., .F., .F.,
 ( 4, 2, 2, 2, 4 ),
 ( 0.01815567983891738443, 0.01899359644517026671, 0.01983151305142315246, 0.02066942965767603474, 0.02150734626392891702 ),
 .UNSPECIFIED. ) ;
#54796 = DIRECTION ( 'NONE',  ( 0.000000000000000000, 1.000000000000000000, -1.181994176819165452E-15 ) ) ;
#54797 = CLOSED_SHELL ( 'NONE', ( #31643, #23434, #33850, #25464, #59164, #25324, #33331, #68065, #52039, #63609, #51287, #47948, #28667, #53146, #26500, #10787, #20197, #18821, #29747, #35294, #41406, #7461, #26474, #45346, #50130, #22438, #31577 ) ) ;
#54798 = CARTESIAN_POINT ( 'NONE',  ( 11.99999999999999822, 0.000000000000000000, 0.000000000000000000 ) ) ;
#54799 = ORIENTED_EDGE ( 'NONE', *, *, #5812, .T. ) ;
#54800 = CARTESIAN_POINT ( 'NONE',  ( 0.000000000000000000, 17.67226234102826510, 33.17418723428314564 ) ) ;
#54801 = CARTESIAN_POINT ( 'NONE',  ( 0.000000000000000000, -2.935248768560059673, 2.602085213965210642E-15 ) ) ;
#54802 = AXIS2_PLACEMENT_3D ( 'NONE', #8259, #37583, #30076 ) ;
#54803 = DIRECTION ( 'NONE',  ( -1.000000000000000000, 0.000000000000000000, 0.000000000000000000 ) ) ;
#54804 = EDGE_CURVE ( 'NONE', #73248, #43631, #60772, .T. ) ;
#54805 = CARTESIAN_POINT ( 'NONE',  ( 0.000000000000000000, -30.00120703465222149, 22.64427369931158296 ) ) ;
#54806 = CARTESIAN_POINT ( 'NONE',  ( 97.30629616937498838, -209.9999999999999716, 78.05406250086716113 ) ) ;
#54807 = EDGE_CURVE ( 'NONE', #49292, #59685, #15267, .T. ) ;
#54808 = AXIS2_PLACEMENT_3D ( 'NONE', #57995, #6139, #40709 ) ;
#54809 = EDGE_CURVE ( 'NONE', #2347, #57306, #29003, .T. ) ;
#54810 = ORIENTED_EDGE ( 'NONE', *, *, #47308, .F. ) ;
#54811 = AXIS2_PLACEMENT_3D ( 'NONE', #72161, #72524, #13900 ) ;
#54812 = EDGE_CURVE ( 'NONE', #52552, #57541, #25805, .T. ) ;
#54813 = ORIENTED_EDGE ( 'NONE', *, *, #52956, .T. ) ;
#54814 = DIRECTION ( 'NONE',  ( 2.603472992746261562E-14, 2.546204323184492723E-14, -1.000000000000000000 ) ) ;
#54815 = CIRCLE ( 'NONE', #36841, 31.99999999999998934 ) ;
#54816 = CARTESIAN_POINT ( 'NONE',  ( 0.000000000000000000, 0.000000000000000000, 0.000000000000000000 ) ) ;
#54817 = DIRECTION ( 'NONE',  ( 0.000000000000000000, -0.9945218953682730678, 0.1045284632676569680 ) ) ;
#54818 = ORIENTED_EDGE ( 'NONE', *, *, #64858, .F. ) ;
#54819 = FACE_OUTER_BOUND ( 'NONE', #55760, .T. ) ;
#54820 = CARTESIAN_POINT ( 'NONE',  ( 92.69370383062501162, -209.9999999999999716, 75.83156250086716454 ) ) ;
#54821 = EDGE_CURVE ( 'NONE', #64729, #20698, #37477, .T. ) ;
#54822 = ORIENTED_EDGE ( 'NONE', *, *, #67370, .T. ) ;
#54823 = DIRECTION ( 'NONE',  ( -1.000000000000000000, 0.000000000000000000, 0.000000000000000000 ) ) ;
#54824 = VERTEX_POINT ( 'NONE', #48736 ) ;
#54825 = ORIENTED_EDGE ( 'NONE', *, *, #29444, .T. ) ;
#54826 = CARTESIAN_POINT ( 'NONE',  ( -92.34999999999999432, -208.4700217866474645, 82.19479166840095274 ) ) ;
#54827 = CIRCLE ( 'NONE', #24774, 37.49900000000000944 ) ;
#54828 = PLANE ( 'NONE',  #28134 ) ;
#54829 = ORIENTED_EDGE ( 'NONE', *, *, #67416, .T. ) ;
#54830 = LINE ( 'NONE', #55573, #40163 ) ;
#54831 = CARTESIAN_POINT ( 'NONE',  ( 95.00000000000000000, -206.9400435732949575, 79.12562500173429214 ) ) ;
#54832 = CARTESIAN_POINT ( 'NONE',  ( 93.67499999999998295, 92.29496732002878900, 84.81416666666666515 ) ) ;
#54833 = ORIENTED_EDGE ( 'NONE', *, *, #17051, .F. ) ;
#54834 = LINE ( 'NONE', #4096, #63491 ) ;
#54835 = CARTESIAN_POINT ( 'NONE',  ( -92.69370383062501162, -210.2956651733040303, 74.79348190356850523 ) ) ;
#54836 = EDGE_CURVE ( 'NONE', #51720, #21751, #54750, .T. ) ;
#54837 = ORIENTED_EDGE ( 'NONE', *, *, #68016, .T. ) ;
#54838 = ORIENTED_EDGE ( 'NONE', *, *, #34026, .F. ) ;
#54839 = CARTESIAN_POINT ( 'NONE',  ( -96.15314808468752972, 91.99731107132950569, 87.79072916753381151 ) ) ;
#54840 = CARTESIAN_POINT ( 'NONE',  ( 93.84685191531248449, 91.99731107132950569, 81.28197916753380525 ) ) ;
#54841 = EDGE_CURVE ( 'NONE', #72954, #67569, #55117, .T. ) ;
#54842 = ORIENTED_EDGE ( 'NONE', *, *, #632, .T. ) ;
#54843 = CARTESIAN_POINT ( 'NONE',  ( 11.99999999999999822, 0.000000000000000000, 0.000000000000000000 ) ) ;
#54844 = ORIENTED_EDGE ( 'NONE', *, *, #41249, .T. ) ;
#54845 = FACE_BOUND ( 'NONE', #38654, .T. ) ;
#54846 = EDGE_CURVE ( 'NONE', #15838, #41508, #67142, .T. ) ;
#54847 = EDGE_CURVE ( 'NONE', #70771, #63454, #60408, .T. ) ;
#54848 = ORIENTED_EDGE ( 'NONE', *, *, #52288, .F. ) ;
#54849 = VERTEX_POINT ( 'NONE', #31806 ) ;
#54850 = ORIENTED_EDGE ( 'NONE', *, *, #25570, .F. ) ;
#54851 = DIRECTION ( 'NONE',  ( 0.000000000000000000, -0.8090169943749402348, -0.5877852522924830181 ) ) ;
#54852 = EDGE_LOOP ( 'NONE', ( #27992, #22215, #41178, #71957 ) ) ;
#54853 = ADVANCED_FACE ( 'NONE', ( #49477 ), #31442, .T. ) ;
#54854 = DIRECTION ( 'NONE',  ( 0.000000000000000000, 0.000000000000000000, 1.000000000000000000 ) ) ;
#54855 = CARTESIAN_POINT ( 'NONE',  ( 97.64999999999999147, 90.00000000000002842, 89.12687500173430521 ) ) ;
#54856 = ORIENTED_EDGE ( 'NONE', *, *, #63442, .F. ) ;
#54857 = CARTESIAN_POINT ( 'NONE',  ( -92.34999999999999432, -210.0000000024460576, 75.15687493084206494 ) ) ;
#54858 = CARTESIAN_POINT ( 'NONE',  ( -96.15314808468745866, -211.9973110713294489, 78.95364583420047211 ) ) ;
#54859 = ORIENTED_EDGE ( 'NONE', *, *, #55741, .T. ) ;
#54860 = DIRECTION ( 'NONE',  ( 0.000000000000000000, -0.8910065241883722287, 0.4539904997395382558 ) ) ;
#54861 = AXIS2_PLACEMENT_3D ( 'NONE', #27018, #43604, #10110 ) ;
#54862 = CARTESIAN_POINT ( 'NONE',  ( 15.00000000000000000, -10.45096189432314127, 21.10159698893440350 ) ) ;
#54863 = CARTESIAN_POINT ( 'NONE',  ( 94.99999999999998579, 90.00000000000002842, 90.00000000000000000 ) ) ;
#54864 = DIRECTION ( 'NONE',  ( -1.000000000000000000, -0.000000000000000000, -0.000000000000000000 ) ) ;
#54865 = EDGE_CURVE ( 'NONE', #68424, #16094, #8889, .T. ) ;
#54866 = PLANE ( 'NONE',  #42802 ) ;
#54867 = AXIS2_PLACEMENT_3D ( 'NONE', #51247, #63292, #68178 ) ;
#54868 = LINE ( 'NONE', #25923, #63754 ) ;
#54869 = CARTESIAN_POINT ( 'NONE',  ( 96.15314808468748708, 91.99731107132950569, 88.16114583420046813 ) ) ;
#54870 = CARTESIAN_POINT ( 'NONE',  ( -93.67499999999998295, -212.2949673200287179, 85.76666666666665151 ) ) ;
#54871 = CARTESIAN_POINT ( 'NONE',  ( 97.65000000000000568, 88.47002178664752137, 81.45395833506763950 ) ) ;
#54872 = CARTESIAN_POINT ( 'NONE',  ( 11.99999999999999822, -16.65972982744876774, -80.28980883073775487 ) ) ;
#54873 = DIRECTION ( 'NONE',  ( 0.000000000000000000, 0.000000000000000000, 1.000000000000000000 ) ) ;
#54874 = CARTESIAN_POINT ( 'NONE',  ( -10.00000000000000000, 0.000000000000000000, 0.000000000000000000 ) ) ;
#54875 = AXIS2_PLACEMENT_3D ( 'NONE', #14187, #14561, #7816 ) ;
#54876 = AXIS2_PLACEMENT_3D ( 'NONE', #65078, #36480, #1223 ) ;
#54877 = CARTESIAN_POINT ( 'NONE',  ( 0.000000000000000000, 0.000000000000000000, 0.000000000000000000 ) ) ;
#54878 = CARTESIAN_POINT ( 'NONE',  ( -95.00000000000002842, 90.00000000000004263, 90.00000000000000000 ) ) ;
#54879 = VECTOR ( 'NONE', #21398, 1000.000000000000000 ) ;
#54880 = CARTESIAN_POINT ( 'NONE',  ( 15.00000000000000000, 22.07842321921480888, -8.187992925817425771 ) ) ;
#54881 = CYLINDRICAL_SURFACE ( 'NONE', #39451, 31.99999999999998579 ) ;
#54882 = CARTESIAN_POINT ( 'NONE',  ( 0.000000000000000000, -28.89263327155693517, -71.91182617369219088 ) ) ;
#54883 = CIRCLE ( 'NONE', #34436, 37.49900000000000233 ) ;
#54884 = CARTESIAN_POINT ( 'NONE',  ( 15.00000000000000000, -22.67460108101782978, -6.353146135317906840 ) ) ;
#54885 = CARTESIAN_POINT ( 'NONE',  ( -96.32499999999996021, -212.2949673200287179, 88.20083333333332121 ) ) ;
#54886 = CIRCLE ( 'NONE', #69280, 82.00000000000000000 ) ;
#54887 = DIRECTION ( 'NONE',  ( 0.000000000000000000, -0.5877852522924802425, 0.8090169943749422332 ) ) ;
#54888 = EDGE_LOOP ( 'NONE', ( #20045, #69988, #45701, #67256 ) ) ;
#54889 = FACE_OUTER_BOUND ( 'NONE', #51139, .T. ) ;
#54890 = CARTESIAN_POINT ( 'NONE',  ( 96.32499999999998863, -212.2949673200287179, 78.22604166840096696 ) ) ;
#54891 = CYLINDRICAL_SURFACE ( 'NONE', #26222, 77.49899999999999523 ) ;
#54892 = DIRECTION ( 'NONE',  ( -1.000000000000000000, -0.000000000000000000, 0.000000000000000000 ) ) ;
#54893 = ADVANCED_FACE ( 'NONE', ( #72402 ), #56674, .T. ) ;
#54894 = ADVANCED_FACE ( 'NONE', ( #43118 ), #37841, .T. ) ;
#54895 = ORIENTED_EDGE ( 'NONE', *, *, #42945, .F. ) ;
#54896 = EDGE_CURVE ( 'NONE', #73780, #7680, #2561, .T. ) ;
#54897 = VERTEX_POINT ( 'NONE', #26169 ) ;
#54898 = ADVANCED_FACE ( 'NONE', ( #32174 ), #71281, .T. ) ;
#54899 = CARTESIAN_POINT ( 'NONE',  ( 0.000000000000000000, -74.65491531819124305, 8.830959090342128448 ) ) ;
#54900 = CARTESIAN_POINT ( 'NONE',  ( 10.00000000000000000, -65.59268652807237743, 36.72794159290217664 ) ) ;
#54901 = ORIENTED_EDGE ( 'NONE', *, *, #44346, .F. ) ;
#54902 = CARTESIAN_POINT ( 'NONE',  ( 93.84685191531249870, -208.0026889286704943, 80.01197916753380923 ) ) ;
#54903 = CARTESIAN_POINT ( 'NONE',  ( 97.30629616937498838, -209.9999999999999716, 86.30906250086715659 ) ) ;
#54904 = AXIS2_PLACEMENT_3D ( 'NONE', #15810, #62812, #22948 ) ;
#54905 = VERTEX_POINT ( 'NONE', #66772 ) ;
#54906 = CARTESIAN_POINT ( 'NONE',  ( 96.15314808468750130, -211.9973110713294489, 87.47322916753381605 ) ) ;
#54907 = CIRCLE ( 'NONE', #18897, 12.50000000000000000 ) ;
#54908 = ORIENTED_EDGE ( 'NONE', *, *, #16892, .F. ) ;
#54909 = DIRECTION ( 'NONE',  ( 1.000000000000000000, 0.000000000000000000, 0.000000000000000000 ) ) ;
#54910 = ORIENTED_EDGE ( 'NONE', *, *, #48237, .F. ) ;
#54911 = CARTESIAN_POINT ( 'NONE',  ( -97.30629616937501680, 88.66845928578038638, 78.42447916753380355 ) ) ;
#54912 = ORIENTED_EDGE ( 'NONE', *, *, #18761, .F. ) ;
#54913 = AXIS2_PLACEMENT_3D ( 'NONE', #72960, #20370, #43329 ) ;
#54914 = VERTEX_POINT ( 'NONE', #14146 ) ;
#54915 = DIRECTION ( 'NONE',  ( 0.000000000000000000, 0.000000000000000000, 1.000000000000000000 ) ) ;
#54916 = AXIS2_PLACEMENT_3D ( 'NONE', #33611, #67458, #45663 ) ;
#54917 = VERTEX_POINT ( 'NONE', #28770 ) ;
#54918 = DIRECTION ( 'NONE',  ( 0.000000000000000000, 0.000000000000000000, 1.000000000000000000 ) ) ;
#54919 = DIRECTION ( 'NONE',  ( 0.000000000000000000, 0.5224985647159500202, -0.8526401643540915121 ) ) ;
#54920 = ADVANCED_FACE ( 'NONE', ( #17126 ), #68633, .F. ) ;
#54921 = ORIENTED_EDGE ( 'NONE', *, *, #56177, .T. ) ;
#54922 = DIRECTION ( 'NONE',  ( -1.000000000000000000, -0.000000000000000000, 0.000000000000000000 ) ) ;
#54923 = ORIENTED_EDGE ( 'NONE', *, *, #69676, .F. ) ;
#54924 =( BOUNDED_CURVE ( )  B_SPLINE_CURVE ( 2, ( #52718, #41078, #62922, #40327, #12488, #5762, #51973 ),
 .UNSPECIFIED., .F., .F. ) 
 B_SPLINE_CURVE_WITH_KNOTS ( ( 3, 2, 2, 3 ),
 ( 0.8749999999999997780, 0.8819444444444441977, 0.8888888888888886175, 0.8958333333333331483 ),
 .UNSPECIFIED. ) 
 CURVE ( )  GEOMETRIC_REPRESENTATION_ITEM ( )  RATIONAL_B_SPLINE_CURVE ( ( 1.000000000000004219, 0.8660254037844343777, 1.000000000000000000, 0.8660254037844387076, 1.000000000000000000, 0.8660254037844430375, 0.9999999999999956701 ) ) 
 REPRESENTATION_ITEM ( '' )  );
#54925 = DIRECTION ( 'NONE',  ( 0.000000000000000000, 0.000000000000000000, 1.000000000000000000 ) ) ;
#54926 = ORIENTED_EDGE ( 'NONE', *, *, #1585, .F. ) ;
#54927 = ORIENTED_EDGE ( 'NONE', *, *, #7892, .F. ) ;
#54928 = VERTEX_POINT ( 'NONE', #23149 ) ;
#54929 = CARTESIAN_POINT ( 'NONE',  ( 96.15314808468750130, -211.9973110713294489, 79.05947916753380866 ) ) ;
#54931 = ADVANCED_FACE ( 'NONE', ( #63370 ), #5861, .T. ) ;
#54930 = CARTESIAN_POINT ( 'NONE',  ( -7.500000000000015099, -73.00000000000001421, -255.0000000000000000 ) ) ;
#54932 = EDGE_CURVE ( 'NONE', #49170, #15332, #25419, .T. ) ;
#54933 = CARTESIAN_POINT ( 'NONE',  ( 5.000000000000002665, -10.30890764327323872, -81.34940948281348483 ) ) ;
#54934 = ORIENTED_EDGE ( 'NONE', *, *, #2004, .F. ) ;
#54935 = VECTOR ( 'NONE', #15239, 1000.000000000000000 ) ;
#54936 = ORIENTED_EDGE ( 'NONE', *, *, #65104, .F. ) ;
#54937 = ORIENTED_EDGE ( 'NONE', *, *, #26485, .T. ) ;
#54938 = CARTESIAN_POINT ( 'NONE',  ( -10.00000000000000000, 0.000000000000000000, 0.000000000000000000 ) ) ;
#54939 = DIRECTION ( 'NONE',  ( 0.7273375899149812085, -0.6862798483830533369, 0.000000000000000000 ) ) ;
#54940 = CIRCLE ( 'NONE', #4520, 20.20000000000036522 ) ;
#54941 = CARTESIAN_POINT ( 'NONE',  ( -93.84685191531252713, 88.00268892867056536, 79.85322916753381151 ) ) ;
#54942 = VERTEX_POINT ( 'NONE', #33668 ) ;
#54943 = CARTESIAN_POINT ( 'NONE',  ( 94.99999999999998579, 92.66308142843935514, 76.14906250086716000 ) ) ;
#54944 = ORIENTED_EDGE ( 'NONE', *, *, #8201, .T. ) ;
#54945 = CARTESIAN_POINT ( 'NONE',  ( 2.949999999999999734, 0.000000000000000000, 0.000000000000000000 ) ) ;
#54946 = DIRECTION ( 'NONE',  ( 0.000000000000000000, 0.000000000000000000, 1.000000000000000000 ) ) ;
#54947 = CARTESIAN_POINT ( 'NONE',  ( -97.64999999999990621, -211.5299782133524786, 76.71791666666666742 ) ) ;
#54948 = DIRECTION ( 'NONE',  ( 0.000000000000000000, 0.000000000000000000, 1.000000000000000000 ) ) ;
#54949 = DIRECTION ( 'NONE',  ( -1.000000000000000000, -0.000000000000000000, 0.000000000000000000 ) ) ;
#54950 = CARTESIAN_POINT ( 'NONE',  ( -96.15314808468747287, -208.0026889286704943, 80.01197916753380923 ) ) ;
#54951 = CARTESIAN_POINT ( 'NONE',  ( 92.35000000000002274, 88.47002178664750716, 86.87791666666664980 ) ) ;
#54952 = DIRECTION ( 'NONE',  ( 0.000000000000000000, 0.000000000000000000, -1.000000000000000000 ) ) ;
#54953 = DIRECTION ( 'NONE',  ( 0.000000000000000000, -0.4539904997395350916, -0.8910065241883738940 ) ) ;
#54954 = VERTEX_POINT ( 'NONE', #74263 ) ;
#54955 = ORIENTED_EDGE ( 'NONE', *, *, #40770, .T. ) ;
#54956 = CARTESIAN_POINT ( 'NONE',  ( -95.00000000000002842, 90.00000000000004263, 90.00000000000000000 ) ) ;
#54957 = DIRECTION ( 'NONE',  ( -1.000000000000000000, -0.000000000000000000, -0.000000000000000000 ) ) ;
#54958 = DIRECTION ( 'NONE',  ( -1.000000000000000000, -0.000000000000000000, -0.000000000000000000 ) ) ;
#54959 = CARTESIAN_POINT ( 'NONE',  ( -92.69370383062502583, 91.33154071421968467, 85.56822916753380071 ) ) ;
#54960 = DIRECTION ( 'NONE',  ( -1.000000000000000000, -0.000000000000000000, -0.000000000000000000 ) ) ;
#54961 = DIRECTION ( 'NONE',  ( 0.000000000000000000, -0.4539904997395352027, -0.8910065241883737830 ) ) ;
#54962 = AXIS2_PLACEMENT_3D ( 'NONE', #15333, #61220, #51041 ) ;
#54963 = ORIENTED_EDGE ( 'NONE', *, *, #20030, .F. ) ;
#54964 = DIRECTION ( 'NONE',  ( 2.628368902995164490E-16, 1.000000000000000000, 0.000000000000000000 ) ) ;
#54965 = PRESENTATION_LAYER_ASSIGNMENT (  '', '', ( #50121 ) ) ;
#54966 = CARTESIAN_POINT ( 'NONE',  ( 11.99999999999999822, -5.256550761632340141, -77.32052557432847095 ) ) ;
#54967 = LINE ( 'NONE', #3490, #56186 ) ;
#54968 = FACE_OUTER_BOUND ( 'NONE', #52311, .T. ) ;
#54969 = AXIS2_PLACEMENT_3D ( 'NONE', #18614, #24272, #64489 ) ;
#54970 = DIRECTION ( 'NONE',  ( -1.000000000000000000, 0.000000000000000000, -0.000000000000000000 ) ) ;
#54971 = CARTESIAN_POINT ( 'NONE',  ( 92.35000000000000853, -208.4700217866474645, 88.75645833506762017 ) ) ;
#54972 = CARTESIAN_POINT ( 'NONE',  ( -92.69370383062498320, -209.9999999999999716, 83.13406250086715943 ) ) ;
#54973 = VECTOR ( 'NONE', #39172, 1000.000000000000000 ) ;
#54974 = DIRECTION ( 'NONE',  ( -1.000000000000000000, -0.000000000000000000, -0.000000000000000000 ) ) ;
#54975 = EDGE_CURVE ( 'NONE', #27662, #55952, #21814, .T. ) ;
#54976 = DIRECTION ( 'NONE',  ( -1.000000000000000000, 0.000000000000000000, 0.000000000000000000 ) ) ;
#54977 = DIRECTION ( 'NONE',  ( -1.000000000000000000, 0.000000000000000000, 0.000000000000000000 ) ) ;
#54978 = ORIENTED_EDGE ( 'NONE', *, *, #11716, .T. ) ;
#54979 = CARTESIAN_POINT ( 'NONE',  ( 92.35000000002544596, 90.00000000000008527, -74.99999999999992895 ) ) ;
#54980 = DIRECTION ( 'NONE',  ( -1.000000000000000000, 0.000000000000000000, -0.000000000000000000 ) ) ;
#54981 = DIRECTION ( 'NONE',  ( -1.000000000000000000, -0.000000000000000000, 0.000000000000000000 ) ) ;
#54982 = AXIS2_PLACEMENT_3D ( 'NONE', #26150, #48719, #60390 ) ;
#54983 = ADVANCED_FACE ( 'NONE', ( #55865 ), #11477, .T. ) ;
#54984 = VECTOR ( 'NONE', #39790, 1000.000000000000114 ) ;
#54985 = CARTESIAN_POINT ( 'NONE',  ( -94.99999999999997158, -209.9999999999999716, 90.00000000000000000 ) ) ;
#54986 = VERTEX_POINT ( 'NONE', #44964 ) ;
#54987 = ADVANCED_FACE ( 'NONE', ( #39700 ), #42281, .T. ) ;
#54988 = DIRECTION ( 'NONE',  ( -1.000000000000000000, 0.000000000000000000, 0.000000000000000000 ) ) ;
#54989 = CARTESIAN_POINT ( 'NONE',  ( 0.000000000000000000, -17.67226234102801286, -33.17418723428327354 ) ) ;
#54990 = ORIENTED_EDGE ( 'NONE', *, *, #58136, .F. ) ;
#54991 = CIRCLE ( 'NONE', #56187, 42.00000000000000000 ) ;
#54992 = EDGE_CURVE ( 'NONE', #7579, #50776, #65086, .T. ) ;
#54993 = LINE ( 'NONE', #21509, #20772 ) ;
#54994 = CARTESIAN_POINT ( 'NONE',  ( 5.000000000000000000, -15.48615015657555993, -39.04073710021360455 ) ) ;
#54995 = ORIENTED_EDGE ( 'NONE', *, *, #16116, .F. ) ;
#54996 = ORIENTED_EDGE ( 'NONE', *, *, #22326, .F. ) ;
#54997 = DIRECTION ( 'NONE',  ( 1.000000000000000000, 0.000000000000000000, 0.000000000000000000 ) ) ;
#54998 = ORIENTED_EDGE ( 'NONE', *, *, #66704, .T. ) ;
#54999 = ORIENTED_EDGE ( 'NONE', *, *, #14319, .F. ) ;
#55000 = VERTEX_POINT ( 'NONE', #50205 ) ;
#55001 = VERTEX_POINT ( 'NONE', #45721 ) ;
#55002 = CARTESIAN_POINT ( 'NONE',  ( 11.99999999999999822, 0.000000000000000000, 0.000000000000000000 ) ) ;
#55003 = ADVANCED_FACE ( 'NONE', ( #28022 ), #4755, .T. ) ;
#55004 = ADVANCED_FACE ( 'NONE', ( #73139 ), #57349, .T. ) ;
#55005 = ORIENTED_EDGE ( 'NONE', *, *, #16455, .F. ) ;
#55006 = VERTEX_POINT ( 'NONE', #62258 ) ;
#55007 = CARTESIAN_POINT ( 'NONE',  ( 94.99999999999998579, 92.66308142843935514, 75.03781250086714749 ) ) ;
#55008 = FACE_OUTER_BOUND ( 'NONE', #68319, .T. ) ;
#55009 = AXIS2_PLACEMENT_3D ( 'NONE', #61873, #72749, #49827 ) ;
#55010 = AXIS2_PLACEMENT_3D ( 'NONE', #55437, #49047, #71599 ) ;
#55011 = ORIENTED_EDGE ( 'NONE', *, *, #25911, .F. ) ;
#55012 = CIRCLE ( 'NONE', #56267, 31.99999999999998224 ) ;
#55013 = ORIENTED_EDGE ( 'NONE', *, *, #19628, .F. ) ;
#55014 = ORIENTED_EDGE ( 'NONE', *, *, #26510, .T. ) ;
#55015 = CARTESIAN_POINT ( 'NONE',  ( 93.84685191531248449, 91.99731107132950569, 88.26697916753380468 ) ) ;
#55016 = ORIENTED_EDGE ( 'NONE', *, *, #57213, .F. ) ;
#55017 = CARTESIAN_POINT ( 'NONE',  ( 97.30629616937498838, -211.3315407142195852, 89.27239583420048064 ) ) ;
#55018 = EDGE_CURVE ( 'NONE', #66019, #18578, #39867, .T. ) ;
#55019 = EDGE_CURVE ( 'NONE', #42393, #23530, #31471, .T. ) ;
#55020 = DIRECTION ( 'NONE',  ( 0.9937460003578419965, -0.1116641696014989971, 2.775557561562891351E-17 ) ) ;
#55021 = DIRECTION ( 'NONE',  ( -1.000000000000000000, 0.000000000000000000, 0.000000000000000000 ) ) ;
#55022 = CARTESIAN_POINT ( 'NONE',  ( 10.00000000000000000, -10.30890764327441822, 81.34940948281332851 ) ) ;
#55023 = CARTESIAN_POINT ( 'NONE',  ( 5.000000000000000000, 32.34446384429971744, 26.79245525562726016 ) ) ;
#55024 = AXIS2_PLACEMENT_3D ( 'NONE', #42877, #65444, #71053 ) ;
#55025 = CARTESIAN_POINT ( 'NONE',  ( -97.64999999999996305, -208.4700217866474645, 84.31145833506762699 ) ) ;
#55026 = CARTESIAN_POINT ( 'NONE',  ( -42.50000000000000000, 0.000000000000000000, 0.000000000000000000 ) ) ;
#55027 = DIRECTION ( 'NONE',  ( -0.000000000000000000, -0.000000000000000000, 1.000000000000000000 ) ) ;
#55028 = CARTESIAN_POINT ( 'NONE',  ( -97.64999999999996305, -209.9999999999999716, 77.37937500173428873 ) ) ;
#55029 = CARTESIAN_POINT ( 'NONE',  ( -96.15314808468752972, 91.99731107132950569, 89.69572916753382685 ) ) ;
#55030 = ORIENTED_EDGE ( 'NONE', *, *, #67118, .T. ) ;
#55031 = UNCERTAINTY_MEASURE_WITH_UNIT (LENGTH_MEASURE( 1.000000000000000082E-05 ), #38147, 'distance_accuracy_value', 'NONE');
#55033 = CARTESIAN_POINT ( 'NONE',  ( -96.15314808468751551, 88.00268892867056536, 87.20864583420046756 ) ) ;
#55032 = CARTESIAN_POINT ( 'NONE',  ( 97.30629616937498838, 91.33154071421968467, 86.20322916753382003 ) ) ;
#55034 = VERTEX_POINT ( 'NONE', #61886 ) ;
#55035 = CARTESIAN_POINT ( 'NONE',  ( 94.99999999999998579, 92.66308142843935514, 78.21281250086717307 ) ) ;
#55036 = DIRECTION ( 'NONE',  ( 0.000000000000000000, -0.4067366430757989315, -0.9135454576426015327 ) ) ;
#55037 = PLANE ( 'NONE',  #58303 ) ;
#55038 = CARTESIAN_POINT ( 'NONE',  ( 0.000000000000000000, 21.40280677340371795, 36.13751322684426270 ) ) ;
#55039 = LINE ( 'NONE', #3568, #53049 ) ;
#55040 = CARTESIAN_POINT ( 'NONE',  ( -96.32500000000001705, 92.29496732002878900, 89.25916666666667254 ) ) ;
#55041 = CARTESIAN_POINT ( 'NONE',  ( 0.000000000000000000, 0.000000000000000000, 0.000000000000000000 ) ) ;
#55042 = DIRECTION ( 'NONE',  ( 1.000000000000000000, 0.000000000000000000, 0.000000000000000000 ) ) ;
#55043 = ORIENTED_EDGE ( 'NONE', *, *, #6366, .F. ) ;
#55044 = CIRCLE ( 'NONE', #44266, 77.49900000000000944 ) ;
#55045 = VERTEX_POINT ( 'NONE', #10366 ) ;
#55046 = AXIS2_PLACEMENT_3D ( 'NONE', #36874, #31235, #14316 ) ;
#55047 = CARTESIAN_POINT ( 'NONE',  ( -93.67500000000003979, 87.70503267997129626, 80.05166666666666231 ) ) ;
#55048 = LINE ( 'NONE', #19354, #59101 ) ;
#55049 = DIRECTION ( 'NONE',  ( -1.000000000000000000, 0.000000000000000000, -0.000000000000000000 ) ) ;
#55050 = DIRECTION ( 'NONE',  ( -1.000000000000000000, 3.061616997868382648E-16, 0.000000000000000000 ) ) ;
#55051 = CARTESIAN_POINT ( 'NONE',  ( 0.000000000000000000, 0.000000000000000000, 0.000000000000000000 ) ) ;
#55052 = CARTESIAN_POINT ( 'NONE',  ( -7.670864526094549163, -97.73662565058241114, -5.500000000000000000 ) ) ;
#55053 = DIRECTION ( 'NONE',  ( 0.7585478161175706058, 0.6516173805718080692, -0.000000000000000000 ) ) ;
#55054 = VECTOR ( 'NONE', #27803, 1000.000000000000000 ) ;
#55055 = ORIENTED_EDGE ( 'NONE', *, *, #65911, .T. ) ;
#55056 = CARTESIAN_POINT ( 'NONE',  ( -97.30629616937501680, 88.66845928578038638, 80.80572916753382628 ) ) ;
#55057 = ADVANCED_FACE ( 'NONE', ( #27661 ), #73512, .T. ) ;
#55058 = CARTESIAN_POINT ( 'NONE',  ( 94.99999999999998579, 86.94004357329502852, 82.61812500173428475 ) ) ;
#55059 = FACE_OUTER_BOUND ( 'NONE', #30131, .T. ) ;
#55060 = DIRECTION ( 'NONE',  ( 0.000000000000000000, 0.1564344650402242354, 0.9876883405951387696 ) ) ;
#55061 = CARTESIAN_POINT ( 'NONE',  ( 0.000000000000000000, 59.03961581697465277, -46.53671651293886669 ) ) ;
#55062 = PLANE ( 'NONE',  #8877 ) ;
#55063 = FACE_OUTER_BOUND ( 'NONE', #15081, .T. ) ;
#55064 = EDGE_CURVE ( 'NONE', #20436, #69158, #57894, .T. ) ;
#55065 = LINE ( 'NONE', #31015, #8553 ) ;
#55066 = CARTESIAN_POINT ( 'NONE',  ( 97.64999999999999147, -209.9999999999999716, 90.00000000000000000 ) ) ;
#55067 = EDGE_CURVE ( 'NONE', #23136, #33855, #53117, .T. ) ;
#55068 = CARTESIAN_POINT ( 'NONE',  ( 92.69370383062498320, 90.00000000000002842, 79.64156250086715261 ) ) ;
#55069 = VECTOR ( 'NONE', #53501, 1000.000000000000000 ) ;
#55070 = AXIS2_PLACEMENT_3D ( 'NONE', #29267, #22919, #40559 ) ;
#55071 = EDGE_CURVE ( 'NONE', #6768, #42522, #7690, .T. ) ;
#55072 = CARTESIAN_POINT ( 'NONE',  ( -96.15314808468747287, -208.0026889286704943, 82.71072916753381321 ) ) ;
#55073 = FACE_OUTER_BOUND ( 'NONE', #17833, .T. ) ;
#55074 = ORIENTED_EDGE ( 'NONE', *, *, #8906, .F. ) ;
#55075 = DIRECTION ( 'NONE',  ( -0.000000000000000000, 0.000000000000000000, 1.000000000000000000 ) ) ;
#55076 = CARTESIAN_POINT ( 'NONE',  ( -94.99999999999997158, -206.9400435732949575, 79.04625000000000057 ) ) ;
#55077 = CARTESIAN_POINT ( 'NONE',  ( 7.893099573151324044, -11.68370571044642503, -1.199999999999999956 ) ) ;
#55078 = AXIS2_PLACEMENT_3D ( 'NONE', #15478, #38421, #60974 ) ;
#55079 = CARTESIAN_POINT ( 'NONE',  ( 95.00000000000000000, -212.6630814284392557, 84.08656250086713158 ) ) ;
#55080 = ORIENTED_EDGE ( 'NONE', *, *, #36414, .T. ) ;
#55081 = DIRECTION ( 'NONE',  ( 0.000000000000000000, 0.000000000000000000, -1.000000000000000000 ) ) ;
#55082 = EDGE_LOOP ( 'NONE', ( #54317, #73326, #4996, #23335 ) ) ;
#55083 = ADVANCED_FACE ( 'NONE', ( #35883, #40807 ), #53186, .F. ) ;
#55084 = CARTESIAN_POINT ( 'NONE',  ( -94.99999999999997158, -206.9400435732949575, 75.95062500173428077 ) ) ;
#55085 = VERTEX_POINT ( 'NONE', #42290 ) ;
#55086 = AXIS2_PLACEMENT_3D ( 'NONE', #71956, #20471, #43427 ) ;
#55087 = CIRCLE ( 'NONE', #69526, 77.49899999999999523 ) ;
#55088 = FACE_OUTER_BOUND ( 'NONE', #9892, .T. ) ;
#55089 = VECTOR ( 'NONE', #39944, 1000.000000000000000 ) ;
#55090 = AXIS2_PLACEMENT_3D ( 'NONE', #60639, #54974, #56845 ) ;
#55091 = CARTESIAN_POINT ( 'NONE',  ( 97.30629616937498838, -209.9999999999999716, 78.05406250086716113 ) ) ;
#55092 = ADVANCED_FACE ( 'NONE', ( #23880 ), #23506, .T. ) ;
#55093 = DIRECTION ( 'NONE',  ( -1.000000000000000000, -0.000000000000000000, -0.000000000000000000 ) ) ;
#55094 = EDGE_CURVE ( 'NONE', #719, #24118, #64109, .T. ) ;
#55095 = DIRECTION ( 'NONE',  ( 0.000000000000000000, 0.000000000000000000, 1.000000000000000000 ) ) ;
#55096 = CIRCLE ( 'NONE', #35887, 2.649999999999985700 ) ;
#55097 = CARTESIAN_POINT ( 'NONE',  ( 97.64999999999989200, -211.5299782133525071, 80.73958333333335702 ) ) ;
#55098 = CARTESIAN_POINT ( 'NONE',  ( 93.84685191531248449, 88.00268892867053694, 85.46239583420047836 ) ) ;
#55099 = ADVANCED_FACE ( 'NONE', ( #11836 ), #27880, .T. ) ;
#55100 = CARTESIAN_POINT ( 'NONE',  ( 0.000000000000000000, 0.000000000000000000, 0.000000000000000000 ) ) ;
#55101 = CARTESIAN_POINT ( 'NONE',  ( 95.00000000000000000, -206.9400435732949575, 82.22124999999999773 ) ) ;
#55102 = ORIENTED_EDGE ( 'NONE', *, *, #6167, .T. ) ;
#55103 = VERTEX_POINT ( 'NONE', #12588 ) ;
#55104 = ORIENTED_EDGE ( 'NONE', *, *, #54355, .F. ) ;
#55105 = ORIENTED_EDGE ( 'NONE', *, *, #16225, .F. ) ;
#55106 = DIRECTION ( 'NONE',  ( 1.000000000000000000, 0.000000000000000000, -0.000000000000000000 ) ) ;
#55107 = SURFACE_STYLE_USAGE ( .BOTH. , #47999 ) ;
#55108 = CARTESIAN_POINT ( 'NONE',  ( -97.30629616937501680, 90.00000000000004263, 85.35656250086715602 ) ) ;
#55109 = CARTESIAN_POINT ( 'NONE',  ( 92.35000752690139336, 88.47001744098895415, 88.22729196900363036 ) ) ;
#55110 = DIRECTION ( 'NONE',  ( 1.000000000000000000, 0.000000000000000000, 0.000000000000000000 ) ) ;
#55111 = CARTESIAN_POINT ( 'NONE',  ( 93.67499999999999716, 87.70503267997126784, 76.13583333333333769 ) ) ;
#55112 = CARTESIAN_POINT ( 'NONE',  ( 10.00000000000000000, 0.8828120875905820508, -37.48860685352290290 ) ) ;
#55113 = ORIENTED_EDGE ( 'NONE', *, *, #59094, .T. ) ;
#55114 = CIRCLE ( 'NONE', #67139, 82.00000000000000000 ) ;
#55115 = CARTESIAN_POINT ( 'NONE',  ( -97.64999999999994884, -208.4700217866474645, 85.58145833506763722 ) ) ;
#55116 = VERTEX_POINT ( 'NONE', #1722 ) ;
#55117 = LINE ( 'NONE', #61511, #19393 ) ;
#55118 = ORIENTED_EDGE ( 'NONE', *, *, #45618, .T. ) ;
#55119 = CARTESIAN_POINT ( 'NONE',  ( -92.35000000000003695, 90.00000000000004263, 83.41187500173430180 ) ) ;
#55120 = CIRCLE ( 'NONE', #32302, 2.499999999999999556 ) ;
#55121 = VERTEX_POINT ( 'NONE', #12945 ) ;
#55122 = CARTESIAN_POINT ( 'NONE',  ( 96.15314808468748708, 88.00268892867053694, 88.10822916753382117 ) ) ;
#55123 = DIRECTION ( 'NONE',  ( 0.7273375899149802093, -0.6862798483830544471, 0.000000000000000000 ) ) ;
#55124 = VECTOR ( 'NONE', #42264, 1000.000000000000000 ) ;
#55125 = FACE_OUTER_BOUND ( 'NONE', #71673, .T. ) ;
#55126 = CARTESIAN_POINT ( 'NONE',  ( 10.00000000000000000, -59.46389618801928378, -49.70050353004953791 ) ) ;
#55127 = LINE ( 'NONE', #49116, #11416 ) ;
#55128 = VECTOR ( 'NONE', #23605, 1000.000000000000000 ) ;
#55129 = FACE_OUTER_BOUND ( 'NONE', #28557, .T. ) ;
#55130 = VERTEX_POINT ( 'NONE', #2092 ) ;
#55131 = DIRECTION ( 'NONE',  ( -1.000000000000000000, 0.000000000000000000, -0.000000000000000000 ) ) ;
#55132 = LINE ( 'NONE', #9645, #26323 ) ;
#55133 = ORIENTED_EDGE ( 'NONE', *, *, #58401, .F. ) ;
#55134 = CIRCLE ( 'NONE', #47944, 32.00000000000000000 ) ;
#55135 = ORIENTED_EDGE ( 'NONE', *, *, #5294, .F. ) ;
#55136 = AXIS2_PLACEMENT_3D ( 'NONE', #66467, #49164, #37527 ) ;
#55137 = LINE ( 'NONE', #5048, #27782 ) ;
#55138 = DIRECTION ( 'NONE',  ( -1.000000000000000000, 0.000000000000000000, -0.000000000000000000 ) ) ;
#55139 = CARTESIAN_POINT ( 'NONE',  ( 15.00000000000000000, 5.835314593368470248, -22.81335362449854642 ) ) ;
#55140 = CARTESIAN_POINT ( 'NONE',  ( -92.69370383062498320, -208.6684592857803011, 84.45697916753383083 ) ) ;
#55141 = ORIENTED_EDGE ( 'NONE', *, *, #15688, .T. ) ;
#55142 = CARTESIAN_POINT ( 'NONE',  ( 0.000000000000000000, 0.000000000000000000, 0.000000000000000000 ) ) ;
#55143 = VERTEX_POINT ( 'NONE', #24610 ) ;
#55144 = CIRCLE ( 'NONE', #15535, 37.49900000000000944 ) ;
#55145 = FACE_OUTER_BOUND ( 'NONE', #73398, .T. ) ;
#55146 = VECTOR ( 'NONE', #37504, 1000.000000000000227 ) ;
#55147 = VECTOR ( 'NONE', #5211, 1000.000000000000000 ) ;
#55148 = CARTESIAN_POINT ( 'NONE',  ( 92.34999999999999432, 88.47002178664752137, 81.87729166840097150 ) ) ;
#55149 = CARTESIAN_POINT ( 'NONE',  ( 97.65000000000000568, -208.4700217866474645, 82.82979166840095786 ) ) ;
#55150 = CARTESIAN_POINT ( 'NONE',  ( 92.69370383062498320, 88.66845928578035796, 77.63072916753380071 ) ) ;
#55151 = CARTESIAN_POINT ( 'NONE',  ( 97.65000000000000568, -209.9999999999999716, 75.00000000000000000 ) ) ;
#55152 = CYLINDRICAL_SURFACE ( 'NONE', #67267, 31.99999999999998579 ) ;
#55153 = EDGE_CURVE ( 'NONE', #36890, #70455, #52433, .T. ) ;
#55154 = CARTESIAN_POINT ( 'NONE',  ( 10.00000000000000000, 0.000000000000000000, 0.000000000000000000 ) ) ;
#55155 = CIRCLE ( 'NONE', #59952, 31.99999999999999289 ) ;
#55156 = FACE_OUTER_BOUND ( 'NONE', #61018, .T. ) ;
#55157 = AXIS2_PLACEMENT_3D ( 'NONE', #16522, #46216, #44741 ) ;
#55158 = FACE_OUTER_BOUND ( 'NONE', #56533, .T. ) ;
#55159 = EDGE_CURVE ( 'NONE', #9042, #5291, #70451, .T. ) ;
#55160 = CARTESIAN_POINT ( 'NONE',  ( -11.59999999999999787, 0.000000000000000000, -44.99999999999998579 ) ) ;
#55161 =( BOUNDED_CURVE ( )  B_SPLINE_CURVE ( 2, ( #64945, #25077, #30704, #13783, #13422, #25447, #53650, #42377, #53282 ),
 .UNSPECIFIED., .F., .F. ) 
 B_SPLINE_CURVE_WITH_KNOTS ( ( 3, 2, 2, 2, 3 ),
 ( 0.7196881748069930973, 0.7267438507144522442, 0.7337996162553684920, 0.7408553817962847399, 0.7408554641904511184 ),
 .UNSPECIFIED. ) 
 CURVE ( )  GEOMETRIC_REPRESENTATION_ITEM ( )  RATIONAL_B_SPLINE_CURVE ( ( 0.9999965961301877648, 0.8660271057409657525, 1.000000000000000000, 0.8660254037844387076, 1.000000000000000000, 0.8660254037844387076, 1.000000000000000000, 0.9999984355028379568, 0.9999968710422149076 ) ) 
 REPRESENTATION_ITEM ( '' )  );
#55162 = CARTESIAN_POINT ( 'NONE',  ( 1.560000000000000053, 0.8660254037844389297, 1.500000000000000000 ) ) ;
#55163 = EDGE_CURVE ( 'NONE', #65045, #18300, #18959, .T. ) ;
#55164 = PLANE ( 'NONE',  #54145 ) ;
#55165 = VERTEX_POINT ( 'NONE', #29870 ) ;
#55166 = EDGE_CURVE ( 'NONE', #69920, #3672, #18594, .T. ) ;
#55167 = CARTESIAN_POINT ( 'NONE',  ( -93.84685191531252713, 88.00268892867056536, 81.59947916753381492 ) ) ;
#55168 = DIRECTION ( 'NONE',  ( 0.000000000000000000, 0.000000000000000000, 1.000000000000000000 ) ) ;
#55169 = DIRECTION ( 'NONE',  ( 0.000000000000000000, 0.000000000000000000, 1.000000000000000000 ) ) ;
#55170 = EDGE_LOOP ( 'NONE', ( #10665, #65328, #64739, #50040 ) ) ;
#55172 = PLANE ( 'NONE',  #13845 ) ;
#55171 = CIRCLE ( 'NONE', #4814, 31.99999999999998579 ) ;
#55173 = DIRECTION ( 'NONE',  ( -1.000000000000000000, -0.000000000000000000, -0.000000000000000000 ) ) ;
#55174 = EDGE_CURVE ( 'NONE', #70250, #65477, #52821, .T. ) ;
#55175 = CARTESIAN_POINT ( 'NONE',  ( 10.00000000000000000, 0.000000000000000000, 0.000000000000000000 ) ) ;
#55176 = AXIS2_PLACEMENT_3D ( 'NONE', #45854, #48416, #59708 ) ;
#55177 = AXIS2_PLACEMENT_3D ( 'NONE', #1283, #48573, #58748 ) ;
#55178 = DIRECTION ( 'NONE',  ( 1.000000000000000000, 0.000000000000000000, 0.000000000000000000 ) ) ;
#55179 = CARTESIAN_POINT ( 'NONE',  ( 95.00000000000000000, -207.3369185715606307, 77.57781250086715374 ) ) ;
#55180 = CIRCLE ( 'NONE', #25195, 5.315148208181396328 ) ;
#55181 = EDGE_LOOP ( 'NONE', ( #33029, #55836 ) ) ;
#55182 = ORIENTED_EDGE ( 'NONE', *, *, #57321, .T. ) ;
#55183 = EDGE_CURVE ( 'NONE', #27537, #74050, #61488, .T. ) ;
#55184 = EDGE_CURVE ( 'NONE', #71222, #67983, #8674, .T. ) ;
#55185 = CARTESIAN_POINT ( 'NONE',  ( -0.0004442498507136653329, 0.001194404164628348752, -70.59999999999999432 ) ) ;
#55186 = ADVANCED_FACE ( 'NONE', ( #69364 ), #1364, .F. ) ;
#55187 = PLANE ( 'NONE',  #14950 ) ;
#55188 = LINE ( 'NONE', #54091, #13573 ) ;
#55189 = DIRECTION ( 'NONE',  ( -1.000000000000000000, -0.000000000000000000, 0.000000000000000000 ) ) ;
#55190 = CARTESIAN_POINT ( 'NONE',  ( 95.00000000000000000, -207.3369185715606307, 76.30781250086715772 ) ) ;
#55191 = CIRCLE ( 'NONE', #56451, 11.59999999999999787 ) ;
#55192 = ORIENTED_EDGE ( 'NONE', *, *, #8831, .F. ) ;
#55193 = CARTESIAN_POINT ( 'NONE',  ( -94.99999999999997158, -206.9400435732949575, 87.93624999999998693 ) ) ;
#55194 = VERTEX_POINT ( 'NONE', #987 ) ;
#55195 = ORIENTED_EDGE ( 'NONE', *, *, #32216, .T. ) ;
#55196 = DIRECTION ( 'NONE',  ( -0.000000000000000000, -0.000000000000000000, -1.000000000000000000 ) ) ;
#55197 = VECTOR ( 'NONE', #10360, 1000.000000000000000 ) ;
#55198 = AXIS2_PLACEMENT_3D ( 'NONE', #12232, #35533, #64484 ) ;
#55199 = LINE ( 'NONE', #66491, #66516 ) ;
#55200 = CIRCLE ( 'NONE', #17969, 16.00000000000000000 ) ;
#55201 = VERTEX_POINT ( 'NONE', #35155 ) ;
#55202 = CARTESIAN_POINT ( 'NONE',  ( 10.00000000000000000, 29.81001611431009479, 22.74946021919143391 ) ) ;
#55203 = CARTESIAN_POINT ( 'NONE',  ( 97.64999999999999147, -209.9999999999999716, 80.23687500173429044 ) ) ;
#55205 = AXIS2_PLACEMENT_3D ( 'NONE', #68034, #40569, #63515 ) ;
#55204 = CARTESIAN_POINT ( 'NONE',  ( 93.67499999999999716, 87.70503267997126784, 85.66083333333332916 ) ) ;
#55206 = ORIENTED_EDGE ( 'NONE', *, *, #41692, .F. ) ;
#55207 = CYLINDRICAL_SURFACE ( 'NONE', #71879, 37.49900000000000233 ) ;
#55208 = FACE_OUTER_BOUND ( 'NONE', #60045, .T. ) ;
#55209 = ORIENTED_EDGE ( 'NONE', *, *, #62701, .T. ) ;
#55210 = DIRECTION ( 'NONE',  ( -1.000000000000000000, 0.000000000000000000, 0.000000000000000000 ) ) ;
#55211 = CARTESIAN_POINT ( 'NONE',  ( -93.84685191531254134, 91.99731107132950569, 84.50989583420049200 ) ) ;
#55212 = CARTESIAN_POINT ( 'NONE',  ( 97.30629616937498838, 88.66845928578037217, 81.65239583420049030 ) ) ;
#55213 = VERTEX_POINT ( 'NONE', #24255 ) ;
#55214 = FACE_OUTER_BOUND ( 'NONE', #43650, .T. ) ;
#55215 = ORIENTED_EDGE ( 'NONE', *, *, #25748, .F. ) ;
#55216 = FACE_OUTER_BOUND ( 'NONE', #33019, .T. ) ;
#55217 = ORIENTED_EDGE ( 'NONE', *, *, #26784, .T. ) ;
#55218 = ORIENTED_EDGE ( 'NONE', *, *, #15449, .F. ) ;
#55219 = DIRECTION ( 'NONE',  ( -1.000000000000000000, -0.000000000000000000, -0.000000000000000000 ) ) ;
#55220 = ORIENTED_EDGE ( 'NONE', *, *, #41522, .F. ) ;
#55221 = CARTESIAN_POINT ( 'NONE',  ( 5.000000000000000000, -51.29473840253270112, 63.97538442413407012 ) ) ;
#55222 = EDGE_CURVE ( 'NONE', #63128, #24873, #43528, .T. ) ;
#55223 = CARTESIAN_POINT ( 'NONE',  ( 93.67499999999998295, 92.29496732002878900, 88.70354166840097321 ) ) ;
#55224 = EDGE_LOOP ( 'NONE', ( #21343, #23504, #40122, #786 ) ) ;
#55225 = CARTESIAN_POINT ( 'NONE',  ( -2.500000000000000000, 16.00000000000000000, -19.01812422950394676 ) ) ;
#55226 = CARTESIAN_POINT ( 'NONE',  ( -97.30629616937497417, -211.3315407142195852, 79.53572916753380184 ) ) ;
#55227 = ORIENTED_EDGE ( 'NONE', *, *, #57457, .T. ) ;
#55228 = AXIS2_PLACEMENT_3D ( 'NONE', #28300, #10647, #39603 ) ;
#55229 = DIRECTION ( 'NONE',  ( 0.000000000000000000, -0.1564344650402170744, -0.9876883405951398798 ) ) ;
#55230 = CARTESIAN_POINT ( 'NONE',  ( -5.420674214417706693, -142.8662697233533265, -2.500000000000000000 ) ) ;
#55231 = DIRECTION ( 'NONE',  ( 0.000000000000000000, 0.7071067811865436870, 0.7071067811865512365 ) ) ;
#55232 = PLANE ( 'NONE',  #63894 ) ;
#55233 = EDGE_CURVE ( 'NONE', #1704, #6231, #58831, .T. ) ;
#55234 = AXIS2_PLACEMENT_3D ( 'NONE', #39260, #33601, #3949 ) ;
#55235 = ADVANCED_BREP_SHAPE_REPRESENTATION ( '', ( #63624, #43395 ), #59100 ) ;
#55236 = DIRECTION ( 'NONE',  ( -1.000000000000000000, 0.000000000000000000, 0.000000000000000000 ) ) ;
#55237 = EDGE_CURVE ( 'NONE', #72968, #19406, #17057, .T. ) ;
#55238 = DIRECTION ( 'NONE',  ( -0.000000000000000000, -0.000000000000000000, 1.000000000000000000 ) ) ;
#55240 = CARTESIAN_POINT ( 'NONE',  ( 97.30629616937498838, 91.33154071421968467, 86.83822916753381094 ) ) ;
#55239 = AXIS2_PLACEMENT_3D ( 'NONE', #73241, #22500, #5224 ) ;
#55241 = CARTESIAN_POINT ( 'NONE',  ( 11.99999999999999822, 0.000000000000000000, 0.000000000000000000 ) ) ;
#55242 = CARTESIAN_POINT ( 'NONE',  ( 0.000000000000000000, 8.966570791700698706, 81.50828551894228724 ) ) ;
#55243 = EDGE_CURVE ( 'NONE', #3072, #68962, #18281, .T. ) ;
#55244 = CARTESIAN_POINT ( 'NONE',  ( -97.64999999999997726, 88.47002178664752137, 86.87791666666664980 ) ) ;
#55245 = DIRECTION ( 'NONE',  ( -1.000000000000000000, 0.000000000000000000, 0.000000000000000000 ) ) ;
#55246 = DIRECTION ( 'NONE',  ( 0.000000000000000000, -0.7431448254773862505, 0.6691306063588671194 ) ) ;
#55247 = CARTESIAN_POINT ( 'NONE',  ( 97.64999999999999147, 90.00000000000002842, 77.61749999999999261 ) ) ;
#55248 = CARTESIAN_POINT ( 'NONE',  ( 95.00000000000000000, -206.9400435732949575, 75.23624999999998408 ) ) ;
#55249 = DIRECTION ( 'NONE',  ( -1.000000000000000000, 0.000000000000000000, 0.000000000000000000 ) ) ;
#55250 = CIRCLE ( 'NONE', #4895, 16.00000000000000000 ) ;
#55251 = ADVANCED_FACE ( 'NONE', ( #66332 ), #38109, .T. ) ;
#55252 = VECTOR ( 'NONE', #19826, 1000.000000000000000 ) ;
#55253 = CARTESIAN_POINT ( 'NONE',  ( 15.00000000000000000, -20.55727247249748402, -16.78983467731284307 ) ) ;
#55254 = CIRCLE ( 'NONE', #73218, 0.2000000000000000944 ) ;
#55255 = AXIS2_PLACEMENT_3D ( 'NONE', #43039, #66702, #15189 ) ;
#55256 = CYLINDRICAL_SURFACE ( 'NONE', #3523, 16.00000000000000000 ) ;
#55257 = CARTESIAN_POINT ( 'NONE',  ( 0.3000000000000016542, 0.000000000000000000, 0.000000000000000000 ) ) ;
#55258 = CARTESIAN_POINT ( 'NONE',  ( -92.34999999999999432, -208.4700217866474645, 89.73541666666666572 ) ) ;
#55259 = CIRCLE ( 'NONE', #20430, 37.49900000000000233 ) ;
#55260 = AXIS2_PLACEMENT_3D ( 'NONE', #52125, #14022, #59914 ) ;
#55261 = DIRECTION ( 'NONE',  ( -1.000000000000000000, 0.000000000000000000, 0.000000000000000000 ) ) ;
#55262 = EDGE_CURVE ( 'NONE', #50397, #54327, #72310, .T. ) ;
#55263 = CARTESIAN_POINT ( 'NONE',  ( 15.00000000000000000, 20.85821328998756385, 10.92862929874494249 ) ) ;
#55264 = EDGE_CURVE ( 'NONE', #45393, #12388, #48276, .T. ) ;
#55265 = PLANE ( 'NONE',  #45494 ) ;
#55266 = DIRECTION ( 'NONE',  ( 0.000000000000000000, 0.000000000000000000, 1.000000000000000000 ) ) ;
#55267 = LINE ( 'NONE', #62033, #59428 ) ;
#55268 = AXIS2_PLACEMENT_3D ( 'NONE', #25123, #41305, #54072 ) ;
#55269 = ADVANCED_FACE ( 'NONE', ( #19700 ), #47245, .F. ) ;
#55270 = EDGE_LOOP ( 'NONE', ( #65597, #59724, #50038, #63271 ) ) ;
#55271 = ORIENTED_EDGE ( 'NONE', *, *, #16402, .F. ) ;
#55272 = CARTESIAN_POINT ( 'NONE',  ( 11.99999999999999822, 65.64334221924964652, -41.19522573413665611 ) ) ;
#55273 = EDGE_CURVE ( 'NONE', #1863, #60548, #45887, .T. ) ;
#55274 = DIRECTION ( 'NONE',  ( -1.000000000000000000, 0.000000000000000000, -0.000000000000000000 ) ) ;
#55275 = ORIENTED_EDGE ( 'NONE', *, *, #16916, .T. ) ;
#55276 = CARTESIAN_POINT ( 'NONE',  ( 92.69370383062501162, -209.9999999999999716, 82.65781250086713783 ) ) ;
#55277 = CARTESIAN_POINT ( 'NONE',  ( 97.30629616937498838, -209.9999999999999716, 84.40406250086715545 ) ) ;
#55278 = ORIENTED_EDGE ( 'NONE', *, *, #58382, .T. ) ;
#55279 = CARTESIAN_POINT ( 'NONE',  ( 95.00000000000000000, -212.6630814284392557, 85.51531250086713953 ) ) ;
#55280 = EDGE_CURVE ( 'NONE', #35608, #60230, #53487, .T. ) ;
#55281 = CIRCLE ( 'NONE', #19275, 32.50000000000000000 ) ;
#55282 = ORIENTED_EDGE ( 'NONE', *, *, #62672, .F. ) ;
#55283 = CARTESIAN_POINT ( 'NONE',  ( 5.000000000000000000, -74.74816331893404708, -33.71516098798818462 ) ) ;
#55284 = ORIENTED_EDGE ( 'NONE', *, *, #544, .T. ) ;
#55285 = AXIS2_PLACEMENT_3D ( 'NONE', #34824, #28430, #6265 ) ;
#55286 = CARTESIAN_POINT ( 'NONE',  ( -97.30629616937501680, 91.33154071421968467, 78.95364583420048632 ) ) ;
#55287 = ORIENTED_EDGE ( 'NONE', *, *, #38007, .T. ) ;
#55288 = ORIENTED_EDGE ( 'NONE', *, *, #33327, .F. ) ;
#55289 = VECTOR ( 'NONE', #17224, 1000.000000000000000 ) ;
#55290 = DIRECTION ( 'NONE',  ( 0.000000000000000000, 0.5877852522924742473, -0.8090169943749466741 ) ) ;
#55291 = VERTEX_POINT ( 'NONE', #48218 ) ;
#55292 = CARTESIAN_POINT ( 'NONE',  ( 11.99999999999999822, 27.74655509720670210, 77.16300072079670258 ) ) ;
#55293 = CARTESIAN_POINT ( 'NONE',  ( 95.00000000000000000, -206.9400435732949575, 89.28562500173430294 ) ) ;
#55294 = ORIENTED_EDGE ( 'NONE', *, *, #48701, .F. ) ;
#55295 = CARTESIAN_POINT ( 'NONE',  ( -7.500000000000016875, -80.00000000000001421, -269.9999999999999432 ) ) ;
#55296 = ORIENTED_EDGE ( 'NONE', *, *, #62659, .F. ) ;
#55297 = LINE ( 'NONE', #15437, #9648 ) ;
#55298 = EDGE_LOOP ( 'NONE', ( #54234, #51888, #880, #2699 ) ) ;
#55299 = STYLED_ITEM ( 'NONE', ( #31556 ), #11785 ) ;
#55300 = EDGE_LOOP ( 'NONE', ( #51691, #69911, #46329, #5007 ) ) ;
#55301 = ORIENTED_EDGE ( 'NONE', *, *, #38622, .F. ) ;
#55302 = CARTESIAN_POINT ( 'NONE',  ( 95.00000000000000000, -212.6630814284392557, 75.19656250086714522 ) ) ;
#55303 = AXIS2_PLACEMENT_3D ( 'NONE', #34978, #45903, #12037 ) ;
#55304 = CONTEXT_DEPENDENT_SHAPE_REPRESENTATION ( #58502, #18851 ) ;
#55305 = FACE_BOUND ( 'NONE', #45577, .T. ) ;
#55306 = EDGE_LOOP ( 'NONE', ( #20752, #58818, #50383, #6343, #49899 ) ) ;
#55307 = CIRCLE ( 'NONE', #22920, 37.49900000000000233 ) ;
#55308 = EDGE_LOOP ( 'NONE', ( #28042, #66956, #28177, #44010 ) ) ;
#55309 = EDGE_LOOP ( 'NONE', ( #33135, #39011, #35335, #60483 ) ) ;
#55310 = DIRECTION ( 'NONE',  ( -1.000000000000000000, 0.000000000000000000, -0.000000000000000000 ) ) ;
#55311 = FACE_OUTER_BOUND ( 'NONE', #74326, .T. ) ;
#55312 = CARTESIAN_POINT ( 'NONE',  ( -92.69370383062504004, 90.00000000000004263, 76.14906250086716000 ) ) ;
#55313 = VERTEX_POINT ( 'NONE', #2023 ) ;
#55314 = CARTESIAN_POINT ( 'NONE',  ( 93.84685191531248449, 88.00268892867053694, 76.41364583420048007 ) ) ;
#55315 = EDGE_LOOP ( 'NONE', ( #10997, #8700, #52776, #7206 ) ) ;
#55316 = DIRECTION ( 'NONE',  ( -1.000000000000000000, 0.000000000000000000, -0.000000000000000000 ) ) ;
#55317 = CARTESIAN_POINT ( 'NONE',  ( -92.69370383062498320, -208.6684592857803011, 88.10822916753380696 ) ) ;
#55318 = FACE_OUTER_BOUND ( 'NONE', #28949, .T. ) ;
#55319 = DIRECTION ( 'NONE',  ( -1.000000000000000000, 0.000000000000000000, 0.000000000000000000 ) ) ;
#55320 = CYLINDRICAL_SURFACE ( 'NONE', #26098, 82.00000000000000000 ) ;
#55321 = CARTESIAN_POINT ( 'NONE',  ( -97.30629616937495996, -209.9999999999999716, 80.75281250086715090 ) ) ;
#55322 = EDGE_CURVE ( 'NONE', #11947, #9134, #47119, .T. ) ;
#55323 = DIRECTION ( 'NONE',  ( 0.000000000000000000, 0.000000000000000000, -1.000000000000000000 ) ) ;
#55324 = CARTESIAN_POINT ( 'NONE',  ( -18.12185313557660038, -104.9634299478706794, -5.500000000000000000 ) ) ;
#55325 = DIRECTION ( 'NONE',  ( -0.000000000000000000, -0.000000000000000000, -1.000000000000000000 ) ) ;
#55326 = VERTEX_POINT ( 'NONE', #18523 ) ;
#55327 = EDGE_CURVE ( 'NONE', #19604, #58617, #8736, .T. ) ;
#55328 = ORIENTED_EDGE ( 'NONE', *, *, #72883, .F. ) ;
#55329 = DIRECTION ( 'NONE',  ( 1.000000000000000000, 0.000000000000000000, 0.000000000000000000 ) ) ;
#55330 = EDGE_CURVE ( 'NONE', #70942, #33637, #13258, .T. ) ;
#55331 = CARTESIAN_POINT ( 'NONE',  ( -15.44521549751111422, -137.7748507232956001, -5.500000000000000000 ) ) ;
#55332 = FACE_OUTER_BOUND ( 'NONE', #45499, .T. ) ;
#55333 = CARTESIAN_POINT ( 'NONE',  ( -92.69370383062504004, 90.00000000000004263, 82.97531250086714749 ) ) ;
#55334 = DIRECTION ( 'NONE',  ( -1.000000000000000000, -0.000000000000000000, -0.000000000000000000 ) ) ;
#55335 = DIRECTION ( 'NONE',  ( 1.000000000000000000, -0.000000000000000000, -0.000000000000000000 ) ) ;
#55336 = ORIENTED_EDGE ( 'NONE', *, *, #45923, .F. ) ;
#55337 = DIRECTION ( 'NONE',  ( 0.000000000000000000, -0.5000000000000012212, -0.8660254037844380415 ) ) ;
#55338 = AXIS2_PLACEMENT_3D ( 'NONE', #56661, #69042, #68677 ) ;
#55339 = AXIS2_PLACEMENT_3D ( 'NONE', #59204, #71201, #55036 ) ;
#55340 = AXIS2_PLACEMENT_3D ( 'NONE', #43796, #37416, #37028 ) ;
#55341 = LINE ( 'NONE', #21117, #31621 ) ;
#55342 = LINE ( 'NONE', #3863, #15321 ) ;
#55343 = DIRECTION ( 'NONE',  ( 1.000000000000000000, 0.000000000000000000, 0.000000000000000000 ) ) ;
#55344 = DIRECTION ( 'NONE',  ( -1.000000000000000000, -0.000000000000000000, 0.000000000000000000 ) ) ;
#55345 = CARTESIAN_POINT ( 'NONE',  ( -97.30629616937495996, -209.9999999999999716, 82.81656250086714977 ) ) ;
#55346 = EDGE_CURVE ( 'NONE', #47641, #65045, #36249, .T. ) ;
#55347 = CARTESIAN_POINT ( 'NONE',  ( -2.977765906491215642, 0.000000000000000000, 0.000000000000000000 ) ) ;
#55348 = EDGE_LOOP ( 'NONE', ( #64643, #46046, #37444, #33579 ) ) ;
#55349 = DIRECTION ( 'NONE',  ( 0.000000000000000000, 0.000000000000000000, 1.000000000000000000 ) ) ;
#55350 = CARTESIAN_POINT ( 'NONE',  ( 10.00000000000000000, 44.99326035066052754, 68.55367621811160461 ) ) ;
#55351 = CARTESIAN_POINT ( 'NONE',  ( 6.000000000000000000, -44.99326035066007279, -68.55367621811190304 ) ) ;
#55352 = CONICAL_SURFACE ( 'NONE', #22961, 2.649999999999999467, 1.029744258676654312 ) ;
#55353 = ORIENTED_EDGE ( 'NONE', *, *, #19699, .T. ) ;
#55354 = CARTESIAN_POINT ( 'NONE',  ( -0.7195005275814509993, -118.6838241033926948, -2.500000000000000000 ) ) ;
#55355 = DIRECTION ( 'NONE',  ( 0.000000000000000000, 0.000000000000000000, 1.000000000000000000 ) ) ;
#55356 = CARTESIAN_POINT ( 'NONE',  ( 10.00000000000000000, -30.41916302227060598, -71.27951684758059514 ) ) ;
#55357 = AXIS2_PLACEMENT_3D ( 'NONE', #34056, #66148, #5508 ) ;
#55358 = EDGE_CURVE ( 'NONE', #16056, #7244, #19632, .T. ) ;
#55359 = EDGE_CURVE ( 'NONE', #12142, #38305, #7261, .T. ) ;
#55360 = AXIS2_PLACEMENT_3D ( 'NONE', #37116, #19436, #19804 ) ;
#55361 = VECTOR ( 'NONE', #749, 999.9999999999998863 ) ;
#55362 = DIRECTION ( 'NONE',  ( 1.000000000000000000, 0.000000000000000000, 0.000000000000000000 ) ) ;
#55363 = ORIENTED_EDGE ( 'NONE', *, *, #55018, .F. ) ;
#55364 = DIRECTION ( 'NONE',  ( 0.000000000000000000, 0.000000000000000000, 1.000000000000000000 ) ) ;
#55365 = EDGE_CURVE ( 'NONE', #17447, #60516, #3864, .T. ) ;
#55366 = LINE ( 'NONE', #31319, #18710 ) ;
#55367 = ORIENTED_EDGE ( 'NONE', *, *, #24044, .T. ) ;
#55368 =( BOUNDED_CURVE ( )  B_SPLINE_CURVE ( 2, ( #52519, #12300, #7777, #13775, #18674, #35239, #18313 ),
 .UNSPECIFIED., .F., .F. ) 
 B_SPLINE_CURVE_WITH_KNOTS ( ( 3, 2, 2, 3 ),
 ( 0.6666666666666667407, 0.6736111111111112715, 0.6805555555555555802, 0.6875000000000000000 ),
 .UNSPECIFIED. ) 
 CURVE ( )  GEOMETRIC_REPRESENTATION_ITEM ( )  RATIONAL_B_SPLINE_CURVE ( ( 0.9999999999999978906, 0.8660254037844408170, 1.000000000000000000, 0.8660254037844387076, 1.000000000000000000, 0.8660254037844387076, 1.000000000000000000 ) ) 
 REPRESENTATION_ITEM ( '' )  );
#55369 = FACE_OUTER_BOUND ( 'NONE', #4528, .T. ) ;
#55370 = DIRECTION ( 'NONE',  ( -1.000000000000000000, 0.000000000000000000, 0.000000000000000000 ) ) ;
#55371 = ORIENTED_EDGE ( 'NONE', *, *, #2343, .F. ) ;
#55372 = FACE_OUTER_BOUND ( 'NONE', #65469, .T. ) ;
#55373 = ORIENTED_EDGE ( 'NONE', *, *, #31378, .T. ) ;
#55374 = CARTESIAN_POINT ( 'NONE',  ( 0.000000000000000000, 0.000000000000000000, 0.000000000000000000 ) ) ;
#55375 = VERTEX_POINT ( 'NONE', #36928 ) ;
#55376 = ORIENTED_EDGE ( 'NONE', *, *, #537, .F. ) ;
#55377 = VERTEX_POINT ( 'NONE', #70383 ) ;
#55378 = ORIENTED_EDGE ( 'NONE', *, *, #49814, .T. ) ;
#55379 = DIRECTION ( 'NONE',  ( 0.4279312458752976833, 0.9038112904824853189, -0.000000000000000000 ) ) ;
#55380 = ORIENTED_EDGE ( 'NONE', *, *, #56302, .F. ) ;
#55381 = PRODUCT ( 'torque nut 03_iso_ISO 7042-M6-N', 'torque nut 03_iso_ISO 7042-M6-N', '', ( #67038 ) ) ;
#55382 = EDGE_LOOP ( 'NONE', ( #70943, #42914, #10512, #48634 ) ) ;
#55383 = CARTESIAN_POINT ( 'NONE',  ( 92.69370383062498320, 88.66845928578037217, 77.78947916753381264 ) ) ;
#55384 = DIRECTION ( 'NONE',  ( -0.000000000000000000, -0.000000000000000000, 1.000000000000000000 ) ) ;
#55385 = FACE_OUTER_BOUND ( 'NONE', #65574, .T. ) ;
#55386 = ORIENTED_EDGE ( 'NONE', *, *, #25137, .T. ) ;
#55387 = EDGE_LOOP ( 'NONE', ( #16631, #9736, #55418, #9726 ) ) ;
#55388 = AXIS2_PLACEMENT_3D ( 'NONE', #14475, #3961, #49428 ) ;
#55389 = VECTOR ( 'NONE', #57270, 1000.000000000000000 ) ;
#55390 = VERTEX_POINT ( 'NONE', #42218 ) ;
#55391 = CARTESIAN_POINT ( 'NONE',  ( 93.84685191531248449, 91.99731107132950569, 89.53697916753381492 ) ) ;
#55392 = ORIENTED_EDGE ( 'NONE', *, *, #16187, .F. ) ;
#55393 = CARTESIAN_POINT ( 'NONE',  ( 97.30629616937498838, -208.6684592857803011, 86.83822916753381094 ) ) ;
#55394 = CARTESIAN_POINT ( 'NONE',  ( 0.000000000000000000, 0.000000000000000000, 0.000000000000000000 ) ) ;
#55396 = FACE_OUTER_BOUND ( 'NONE', #38400, .T. ) ;
#55395 = CIRCLE ( 'NONE', #37384, 31.99999999999999645 ) ;
#55397 = CARTESIAN_POINT ( 'NONE',  ( -5.000000000000000000, 0.000000000000000000, -6.000000000000000000 ) ) ;
#55398 = CARTESIAN_POINT ( 'NONE',  ( -0.0004442498525516064278, 0.001194404164626844313, -85.60000000000000853 ) ) ;
#55399 = CARTESIAN_POINT ( 'NONE',  ( 0.000000000000000000, 0.000000000000000000, -5.974599999999999689 ) ) ;
#55400 = DIRECTION ( 'NONE',  ( -1.000000000000000000, 0.000000000000000000, -0.000000000000000000 ) ) ;
#55401 = CARTESIAN_POINT ( 'NONE',  ( -96.32499999999996021, -212.2949673200287179, 74.94520833506761903 ) ) ;
#55402 = DIRECTION ( 'NONE',  ( 0.000000000000000000, 0.000000000000000000, 1.000000000000000000 ) ) ;
#55403 = AXIS2_PLACEMENT_3D ( 'NONE', #5872, #11846, #18967 ) ;
#55404 = ORIENTED_EDGE ( 'NONE', *, *, #65130, .T. ) ;
#55406 = CARTESIAN_POINT ( 'NONE',  ( -92.35000000000003695, 88.93103996628917685, 74.48490336299447279 ) ) ;
#55405 = CARTESIAN_POINT ( 'NONE',  ( 92.69370383062498320, 88.66845928578037217, 87.79072916753381151 ) ) ;
#55407 = ORIENTED_EDGE ( 'NONE', *, *, #14358, .F. ) ;
#55408 = DIRECTION ( 'NONE',  ( -0.000000000000000000, 0.000000000000000000, -1.000000000000000000 ) ) ;
#55409 = FACE_OUTER_BOUND ( 'NONE', #51859, .T. ) ;
#55410 = FACE_OUTER_BOUND ( 'NONE', #62340, .T. ) ;
#55411 = CARTESIAN_POINT ( 'NONE',  ( 10.00000000000000000, 0.000000000000000000, 0.000000000000000000 ) ) ;
#55412 = DIRECTION ( 'NONE',  ( -1.000000000000000000, 0.000000000000000000, 0.000000000000000000 ) ) ;
#55413 = DIRECTION ( 'NONE',  ( -1.000000000000000000, 0.000000000000000000, 0.000000000000000000 ) ) ;
#55414 = EDGE_CURVE ( 'NONE', #15281, #44177, #11243, .T. ) ;
#55415 = LINE ( 'NONE', #35802, #1418 ) ;
#55416 = CIRCLE ( 'NONE', #28954, 2.699999999999999734 ) ;
#55417 = DIRECTION ( 'NONE',  ( -1.000000000000000000, 0.000000000000000000, 0.000000000000000000 ) ) ;
#55418 = ORIENTED_EDGE ( 'NONE', *, *, #36078, .F. ) ;
#55419 = VECTOR ( 'NONE', #17214, 1000.000000000000000 ) ;
#55420 = ADVANCED_FACE ( 'NONE', ( #38418 ), #71869, .T. ) ;
#55421 = ORIENTED_EDGE ( 'NONE', *, *, #70798, .T. ) ;
#55422 = VECTOR ( 'NONE', #35195, 1000.000000000000114 ) ;
#55423 = EDGE_CURVE ( 'NONE', #26982, #61409, #54352, .T. ) ;
#55424 = CARTESIAN_POINT ( 'NONE',  ( -96.32500000000001705, 92.29496732002878900, 79.73416666666666686 ) ) ;
#55425 = CARTESIAN_POINT ( 'NONE',  ( 0.000000000000000000, 25.88420570971400991, 27.13269053701105449 ) ) ;
#55426 = LINE ( 'NONE', #22329, #50176 ) ;
#55427 = CARTESIAN_POINT ( 'NONE',  ( 0.000000000000000000, 30.41916302227114599, 71.27951684758035356 ) ) ;
#55428 = CARTESIAN_POINT ( 'NONE',  ( 10.00000000000000000, -6.555932627142676772, 37.01155633439056203 ) ) ;
#55429 = CARTESIAN_POINT ( 'NONE',  ( 0.000000000000000000, 55.16347631943042984, 60.67117009219156643 ) ) ;
#55430 = CARTESIAN_POINT ( 'NONE',  ( -93.84685191531247028, -211.9973110713294489, 75.40822916753381833 ) ) ;
#55431 = EDGE_CURVE ( 'NONE', #27292, #50748, #14733, .T. ) ;
#55432 = EDGE_LOOP ( 'NONE', ( #29821, #70681, #6745, #54261 ) ) ;
#55433 = CARTESIAN_POINT ( 'NONE',  ( -95.00000000000002842, 87.33691857156074434, 83.45156250086714067 ) ) ;
#55434 = DIRECTION ( 'NONE',  ( -1.000000000000000000, 7.955419762439749020E-15, 2.563413034563919251E-14 ) ) ;
#55435 = ADVANCED_FACE ( 'NONE', ( #43697 ), #48938, .T. ) ;
#55436 = CARTESIAN_POINT ( 'NONE',  ( -93.67500000000003979, 87.70503267997129626, 85.76666666666665151 ) ) ;
#55437 = CARTESIAN_POINT ( 'NONE',  ( -95.00000000002611955, 90.00000000000007105, -65.00000000000000000 ) ) ;
#55438 = DIRECTION ( 'NONE',  ( 1.000000000000000000, -0.000000000000000000, -0.000000000000000000 ) ) ;
#55439 = CYLINDRICAL_SURFACE ( 'NONE', #4131, 32.00000000000000000 ) ;
#55440 = CARTESIAN_POINT ( 'NONE',  ( 92.35001798596596245, -208.4700114024452375, 80.50145761676020584 ) ) ;
#55441 = CARTESIAN_POINT ( 'NONE',  ( 10.00000000000000000, 73.95703589264006439, -23.16143007188350822 ) ) ;
#55442 = DIRECTION ( 'NONE',  ( 7.616308197390131428E-15, -1.000000000000000000, 2.546204323184492723E-14 ) ) ;
#55443 = EDGE_CURVE ( 'NONE', #67492, #31113, #24348, .T. ) ;
#55444 = EDGE_CURVE ( 'NONE', #59943, #63855, #6332, .T. ) ;
#55445 = CARTESIAN_POINT ( 'NONE',  ( 93.84685191531248449, 88.00268892867053694, 81.01739583420049939 ) ) ;
#55446 = CARTESIAN_POINT ( 'NONE',  ( -92.69370383062498320, -209.9999999999999716, 82.49906250086715431 ) ) ;
#55447 = DIRECTION ( 'NONE',  ( -1.000000000000000000, 0.000000000000000000, 0.000000000000000000 ) ) ;
#55448 = ORIENTED_EDGE ( 'NONE', *, *, #7966, .F. ) ;
#55449 = PRESENTATION_LAYER_ASSIGNMENT (  '', '', ( #2685 ) ) ;
#55450 = DIRECTION ( 'NONE',  ( 0.000000000000000000, 0.000000000000000000, -1.000000000000000000 ) ) ;
#55451 = CIRCLE ( 'NONE', #56692, 16.00000000000000000 ) ;
#55452 = CARTESIAN_POINT ( 'NONE',  ( -93.67499999999998295, -212.2949673200287179, 76.24166666666666003 ) ) ;
#55453 = CARTESIAN_POINT ( 'NONE',  ( 0.000000000000000000, 0.000000000000000000, 0.000000000000000000 ) ) ;
#55454 = EDGE_CURVE ( 'NONE', #44110, #62228, #27931, .T. ) ;
#55455 = ADVANCED_FACE ( 'NONE', ( #20747 ), #67352, .T. ) ;
#55456 = CIRCLE ( 'NONE', #32624, 82.00000000000000000 ) ;
#55457 = CARTESIAN_POINT ( 'NONE',  ( -92.69370383062505425, 91.33154071421968467, 78.74197916753381321 ) ) ;
#55458 = CARTESIAN_POINT ( 'NONE',  ( 93.84685191531251292, -211.9973110713294489, 82.12864583420046927 ) ) ;
#55459 = ORIENTED_EDGE ( 'NONE', *, *, #58037, .T. ) ;
#55460 = AXIS2_PLACEMENT_3D ( 'NONE', #6242, #64479, #52441 ) ;
#55461 = DIRECTION ( 'NONE',  ( -1.000000000000000000, 0.000000000000000000, 0.000000000000000000 ) ) ;
#55462 = VERTEX_POINT ( 'NONE', #32754 ) ;
#55463 = AXIS2_PLACEMENT_3D ( 'NONE', #44208, #60764, #37470 ) ;
#55464 = CARTESIAN_POINT ( 'NONE',  ( 97.64999999981932888, 89.99996905681224746, 78.33187387208513996 ) ) ;
#55465 = ORIENTED_EDGE ( 'NONE', *, *, #69750, .T. ) ;
#55466 = AXIS2_PLACEMENT_3D ( 'NONE', #47832, #70377, #36544 ) ;
#55467 = CARTESIAN_POINT ( 'NONE',  ( 93.67500000000001137, -207.7050326799711968, 84.17916666666666003 ) ) ;
#55468 = VECTOR ( 'NONE', #64405, 1000.000000000000000 ) ;
#55469 = VERTEX_POINT ( 'NONE', #55331 ) ;
#55470 = ORIENTED_EDGE ( 'NONE', *, *, #29854, .F. ) ;
#55471 = AXIS2_PLACEMENT_3D ( 'NONE', #52390, #47138, #64064 ) ;
#55472 = CARTESIAN_POINT ( 'NONE',  ( 10.00000000000000000, -30.80686688396994910, -21.53537804866113703 ) ) ;
#55473 = CARTESIAN_POINT ( 'NONE',  ( 11.99999999999999822, 0.000000000000000000, 77.49899999999999523 ) ) ;
#55474 = DIRECTION ( 'NONE',  ( -1.000000000000000000, -0.000000000000000000, -0.000000000000000000 ) ) ;
#55475 = DIRECTION ( 'NONE',  ( 0.000000000000000000, -0.4067366430757908269, 0.9135454576426049744 ) ) ;
#55476 = CARTESIAN_POINT ( 'NONE',  ( 92.69370383062498320, 91.33154071421968467, 87.84364583420048689 ) ) ;
#55477 = CARTESIAN_POINT ( 'NONE',  ( -92.35000000000003695, 90.00000000000004263, 83.41187500173430180 ) ) ;
#55478 = CARTESIAN_POINT ( 'NONE',  ( 92.35000000000000853, -209.9999999999999716, 81.10999999999999943 ) ) ;
#55479 = ORIENTED_EDGE ( 'NONE', *, *, #67553, .F. ) ;
#55480 = ORIENTED_EDGE ( 'NONE', *, *, #66105, .F. ) ;
#55481 = ORIENTED_EDGE ( 'NONE', *, *, #63694, .F. ) ;
#55482 = ORIENTED_EDGE ( 'NONE', *, *, #11865, .F. ) ;
#55483 = DIRECTION ( 'NONE',  ( 0.000000000000000000, 1.078060571631605808E-14, 1.000000000000000000 ) ) ;
#55484 = SURFACE_SIDE_STYLE ('',( #39690 ) ) ;
#55485 = CARTESIAN_POINT ( 'NONE',  ( 15.00000000000000000, -18.13022148937263012, -15.02647892043543898 ) ) ;
#55486 = CARTESIAN_POINT ( 'NONE',  ( -96.32499999999996021, -207.7050326799711968, 77.19416666666666060 ) ) ;
#55487 = EDGE_CURVE ( 'NONE', #35405, #7122, #48334, .T. ) ;
#55488 = DIRECTION ( 'NONE',  ( -1.000000000000000000, 0.000000000000000000, 0.000000000000000000 ) ) ;
#55489 = DIRECTION ( 'NONE',  ( -1.000000000000000000, 0.000000000000000000, 0.000000000000000000 ) ) ;
#55490 = DIRECTION ( 'NONE',  ( 0.000000000000000000, 0.000000000000000000, 1.000000000000000000 ) ) ;
#55491 = EDGE_CURVE ( 'NONE', #66220, #42336, #51923, .T. ) ;
#55492 = ORIENTED_EDGE ( 'NONE', *, *, #8737, .F. ) ;
#55493 = CARTESIAN_POINT ( 'NONE',  ( -96.32499999999996021, -212.2949673200287179, 86.37520833506764006 ) ) ;
#55494 = ORIENTED_EDGE ( 'NONE', *, *, #5789, .F. ) ;
#55495 = DIRECTION ( 'NONE',  ( 1.000000000000000000, 0.000000000000000000, 0.000000000000000000 ) ) ;
#55497 = ORIENTED_EDGE ( 'NONE', *, *, #50860, .T. ) ;
#55496 = EDGE_CURVE ( 'NONE', #58494, #15358, #66379, .T. ) ;
#55498 = CARTESIAN_POINT ( 'NONE',  ( -96.32500000000001705, 92.29496732002878900, 84.25854166840096582 ) ) ;
#55499 = ORIENTED_EDGE ( 'NONE', *, *, #61567, .T. ) ;
#55500 = CARTESIAN_POINT ( 'NONE',  ( 92.69370383062498320, 90.00000000000002842, 84.72156250086715090 ) ) ;
#55501 = CARTESIAN_POINT ( 'NONE',  ( 10.00000000000000000, 0.000000000000000000, 0.000000000000000000 ) ) ;
#55502 = CARTESIAN_POINT ( 'NONE',  ( 6.000000000000000000, 81.50828551894227303, 8.966570791700986476 ) ) ;
#55503 = EDGE_CURVE ( 'NONE', #10929, #48479, #39564, .T. ) ;
#55504 = DIRECTION ( 'NONE',  ( 0.000000000000000000, 0.9238795325112878487, -0.3826834323650874503 ) ) ;
#55505 = DIRECTION ( 'NONE',  ( 0.000000000000000000, 0.000000000000000000, 1.000000000000000000 ) ) ;
#55506 = MECHANICAL_DESIGN_GEOMETRIC_PRESENTATION_REPRESENTATION (  '', ( #39902 ), #60293 ) ;
#55507 = AXIS2_PLACEMENT_3D ( 'NONE', #71961, #54321, #65983 ) ;
#55508 = FACE_OUTER_BOUND ( 'NONE', #5461, .T. ) ;
#55509 = VERTEX_POINT ( 'NONE', #44804 ) ;
#55510 = DIRECTION ( 'NONE',  ( 1.000000000000000000, 0.000000000000000000, 0.000000000000000000 ) ) ;
#55511 = CARTESIAN_POINT ( 'NONE',  ( 15.00000000000000000, -25.60904388321925040, -6.976881207771165272 ) ) ;
#55512 = ORIENTED_EDGE ( 'NONE', *, *, #33329, .F. ) ;
#55513 = ADVANCED_FACE ( 'NONE', ( #62094 ), #66973, .F. ) ;
#55514 = VERTEX_POINT ( 'NONE', #37683 ) ;
#55515 = B_SPLINE_CURVE_WITH_KNOTS ( 'NONE', 3,
 ( #64308, #51155, #52644, #28973, #46639, #57926, #58287, #57186, #62849, #22603, #29329, #1195, #90, #45548, #16961, #448, #45913, #29695 ),
 .UNSPECIFIED., .F., .F.,
 ( 4, 2, 2, 2, 2, 2, 2, 2, 4 ),
 ( -0.004093595874563301339, -0.003575961937392278713, -0.003058328000221256088, -0.002540694063050233029, -0.002023060125879210403, -0.001505426188708187778, -0.0009877922515371647186, -0.0004701583143661420931, 4.747562280488053232E-05 ),
 .UNSPECIFIED. ) ;
#55516 = DIRECTION ( 'NONE',  ( -1.000000000000000000, -0.000000000000000000, 0.000000000000000000 ) ) ;
#55517 = CARTESIAN_POINT ( 'NONE',  ( -95.00000000000002842, 86.94004357329504273, 80.07812500173429271 ) ) ;
#55518 = LINE ( 'NONE', #43141, #53337 ) ;
#55519 = AXIS2_PLACEMENT_3D ( 'NONE', #29145, #62655, #73899 ) ;
#55520 = CARTESIAN_POINT ( 'NONE',  ( -92.69370383062498320, -211.3315407142195852, 85.62114583420047609 ) ) ;
#55521 = VERTEX_POINT ( 'NONE', #60617 ) ;
#55522 = EDGE_CURVE ( 'NONE', #73479, #38213, #49506, .T. ) ;
#55523 = CARTESIAN_POINT ( 'NONE',  ( 10.00000000000000000, -21.53537804866103045, 30.80686688397002371 ) ) ;
#55524 = VERTEX_POINT ( 'NONE', #52283 ) ;
#55525 = CYLINDRICAL_SURFACE ( 'NONE', #31888, 82.00000000000000000 ) ;
#55526 = CIRCLE ( 'NONE', #21868, 82.00000000000000000 ) ;
#55527 = CIRCLE ( 'NONE', #23123, 31.99999999999998579 ) ;
#55528 = FACE_BOUND ( 'NONE', #46589, .T. ) ;
#55529 = DIRECTION ( 'NONE',  ( 0.000000000000000000, 0.8090169943749445647, 0.5877852522924770229 ) ) ;
#55530 = CARTESIAN_POINT ( 'NONE',  ( 97.30629616937498838, 88.66845928578035796, 79.74739583420047495 ) ) ;
#55531 = CYLINDRICAL_SURFACE ( 'NONE', #47255, 77.49899999999999523 ) ;
#55532 = CARTESIAN_POINT ( 'NONE',  ( 11.99999999999999822, 76.41127070299290835, -12.93880638057234123 ) ) ;
#55533 = DIRECTION ( 'NONE',  ( -1.000000000000000000, 0.000000000000000000, 0.000000000000000000 ) ) ;
#55534 = CARTESIAN_POINT ( 'NONE',  ( 96.58546442478332494, 91.70561969393826018, 74.79912739178801928 ) ) ;
#55535 = CARTESIAN_POINT ( 'NONE',  ( 6.000000000000000000, 34.94270380257741238, -74.18225833017852722 ) ) ;
#55536 = EDGE_CURVE ( 'NONE', #64729, #70242, #45922, .T. ) ;
#55537 = CYLINDRICAL_SURFACE ( 'NONE', #43009, 16.00000000000000000 ) ;
#55538 = EDGE_CURVE ( 'NONE', #14968, #16250, #39909, .T. ) ;
#55539 = DIRECTION ( 'NONE',  ( 0.000000000000000000, 0.000000000000000000, 1.000000000000000000 ) ) ;
#55540 = DIRECTION ( 'NONE',  ( 1.000000000000000000, 6.951859121168206841E-17, -0.000000000000000000 ) ) ;
#55541 = FACE_OUTER_BOUND ( 'NONE', #39882, .T. ) ;
#55542 = EDGE_LOOP ( 'NONE', ( #17735, #60223, #4578, #21887 ) ) ;
#55543 = CARTESIAN_POINT ( 'NONE',  ( -97.30629616937501680, 90.00000000000004263, 84.56281250086713897 ) ) ;
#55544 = LINE ( 'NONE', #44649, #8328 ) ;
#55545 = DIRECTION ( 'NONE',  ( 0.000000000000000000, 0.000000000000000000, 1.000000000000000000 ) ) ;
#55546 = VERTEX_POINT ( 'NONE', #45176 ) ;
#55547 = LINE ( 'NONE', #43176, #30655 ) ;
#55548 = LINE ( 'NONE', #54801, #6021 ) ;
#55549 = DIRECTION ( 'NONE',  ( -1.000000000000000000, 0.000000000000000000, -0.000000000000000000 ) ) ;
#55550 = CARTESIAN_POINT ( 'NONE',  ( 11.99999999999999822, -70.53064760720336324, 26.01480285779810231 ) ) ;
#55551 = CARTESIAN_POINT ( 'NONE',  ( 93.84685191531249870, -208.0026889286704943, 77.63072916753381492 ) ) ;
#55552 = CIRCLE ( 'NONE', #43554, 3.299999999999997158 ) ;
#55553 = EDGE_LOOP ( 'NONE', ( #43043, #24484, #14535 ) ) ;
#55554 = EDGE_LOOP ( 'NONE', ( #19467, #72191, #40233, #33169 ) ) ;
#55555 = EDGE_CURVE ( 'NONE', #30315, #30862, #5701, .T. ) ;
#55556 = CARTESIAN_POINT ( 'NONE',  ( -97.64999999993850111, -209.9999881787635729, 81.82400613094797848 ) ) ;
#55557 = DIRECTION ( 'NONE',  ( -1.000000000000000000, 0.000000000000000000, 0.000000000000000000 ) ) ;
#55558 = AXIS2_PLACEMENT_3D ( 'NONE', #50978, #5136, #57004 ) ;
#55559 = LINE ( 'NONE', #5191, #43609 ) ;
#55560 = DIRECTION ( 'NONE',  ( -2.603472992746261562E-14, -2.546204323184492723E-14, 1.000000000000000000 ) ) ;
#55561 = FILL_AREA_STYLE_COLOUR ( '', #27291 ) ;
#55562 = CARTESIAN_POINT ( 'NONE',  ( 97.30629616937498838, -211.3315407142195852, 77.36614583420048064 ) ) ;
#55563 = ORIENTED_EDGE ( 'NONE', *, *, #22162, .F. ) ;
#55564 = PLANE ( 'NONE',  #46743 ) ;
#55565 = VERTEX_POINT ( 'NONE', #63215 ) ;
#55566 = AXIS2_PLACEMENT_3D ( 'NONE', #55428, #5061, #67823 ) ;
#55567 = ORIENTED_EDGE ( 'NONE', *, *, #16014, .F. ) ;
#55568 = CARTESIAN_POINT ( 'NONE',  ( 6.000000000000000000, -68.55367621811173251, 44.99326035066031437 ) ) ;
#55569 = CIRCLE ( 'NONE', #17205, 37.49900000000000233 ) ;
#55570 = DIRECTION ( 'NONE',  ( -1.000000000000000000, -0.000000000000000000, 0.000000000000000000 ) ) ;
#55571 = ADVANCED_FACE ( 'NONE', ( #62857 ), #23713, .T. ) ;
#55572 = ORIENTED_EDGE ( 'NONE', *, *, #63488, .T. ) ;
#55573 = CARTESIAN_POINT ( 'NONE',  ( 3.000000000000000000, 3.673940397442059868E-16, -5.974599999999999689 ) ) ;
#55574 = CARTESIAN_POINT ( 'NONE',  ( 96.32499999999998863, -207.7050326799711968, 79.70770833506762187 ) ) ;
#55575 = CARTESIAN_POINT ( 'NONE',  ( 93.67499999999998295, 92.29496732002878900, 80.36916666666665776 ) ) ;
#55576 = EDGE_CURVE ( 'NONE', #66054, #69389, #11149, .T. ) ;
#55577 = ORIENTED_EDGE ( 'NONE', *, *, #42010, .F. ) ;
#55578 = DIRECTION ( 'NONE',  ( 1.000000000000000000, 0.000000000000000000, 0.000000000000000000 ) ) ;
#55579 = VERTEX_POINT ( 'NONE', #56829 ) ;
#55580 = LINE ( 'NONE', #66133, #3339 ) ;
#55581 = ORIENTED_EDGE ( 'NONE', *, *, #27463, .T. ) ;
#55582 = DIRECTION ( 'NONE',  ( 0.000000000000000000, 0.7071067811865487940, -0.7071067811865462405 ) ) ;
#55583 = CARTESIAN_POINT ( 'NONE',  ( -95.00000000000002842, 87.33691857156074434, 83.61031250086715261 ) ) ;
#55584 = CARTESIAN_POINT ( 'NONE',  ( 97.30629616937498838, 88.66845928578037217, 79.74739583420047495 ) ) ;
#55585 = EDGE_LOOP ( 'NONE', ( #9350, #46229, #37717, #52271, #38354, #21834 ) ) ;
#55586 = EDGE_CURVE ( 'NONE', #1365, #41638, #67547, .T. ) ;
#55587 = FACE_OUTER_BOUND ( 'NONE', #71269, .T. ) ;
#55588 = EDGE_CURVE ( 'NONE', #70424, #21232, #51544, .T. ) ;
#55589 = DIRECTION ( 'NONE',  ( -1.000000000000000000, -0.000000000000000000, -0.000000000000000000 ) ) ;
#55590 = ORIENTED_EDGE ( 'NONE', *, *, #46457, .F. ) ;
#55591 = CARTESIAN_POINT ( 'NONE',  ( -0.8815729230226007074, -93.47222532549339746, -2.500000000000000000 ) ) ;
#55592 = CARTESIAN_POINT ( 'NONE',  ( -96.15314808468747287, -208.0026889286704943, 79.37697916753380412 ) ) ;
#55593 = ORIENTED_EDGE ( 'NONE', *, *, #57404, .F. ) ;
#55594 = ORIENTED_EDGE ( 'NONE', *, *, #18350, .T. ) ;
#55595 = DIRECTION ( 'NONE',  ( -1.000000000000000000, 0.000000000000000000, -0.000000000000000000 ) ) ;
#55596 = ORIENTED_EDGE ( 'NONE', *, *, #12246, .T. ) ;
#55597 = DIRECTION ( 'NONE',  ( -1.000000000000000000, 0.000000000000000000, 0.000000000000000000 ) ) ;
#55598 = DIRECTION ( 'NONE',  ( 0.000000000000000000, 0.4539904997395414754, 0.8910065241883706744 ) ) ;
#55599 = ORIENTED_EDGE ( 'NONE', *, *, #60017, .T. ) ;
#55600 =( BOUNDED_CURVE ( )  B_SPLINE_CURVE ( 2, ( #22299, #10272, #4286, #38482, #45243, #15166, #61420 ),
 .UNSPECIFIED., .F., .F. ) 
 B_SPLINE_CURVE_WITH_KNOTS ( ( 3, 2, 2, 3 ),
 ( 0.6250000000000003331, 0.6319444444444446418, 0.6388888888888890616, 0.6458333333333334814 ),
 .UNSPECIFIED. ) 
 CURVE ( )  GEOMETRIC_REPRESENTATION_ITEM ( )  RATIONAL_B_SPLINE_CURVE ( ( 0.9999999999999935607, 0.8660254037844451469, 1.000000000000000000, 0.8660254037844387076, 1.000000000000000000, 0.8660254037844365982, 1.000000000000002220 ) ) 
 REPRESENTATION_ITEM ( '' )  );
#55601 = DIRECTION ( 'NONE',  ( 0.000000000000000000, -0.9876883405951394357, 0.1564344650402205716 ) ) ;
#55602 = CARTESIAN_POINT ( 'NONE',  ( -96.15314808468745866, -211.9973110713294489, 79.58864583420047722 ) ) ;
#55603 = ORIENTED_EDGE ( 'NONE', *, *, #24228, .T. ) ;
#55605 = EDGE_CURVE ( 'NONE', #42829, #12604, #68098, .T. ) ;
#55604 = CARTESIAN_POINT ( 'NONE',  ( 10.00000000000000000, -30.41916302227164337, 71.27951684758015460 ) ) ;
#55606 = DIRECTION ( 'NONE',  ( -1.000000000000000000, 0.000000000000000000, 0.000000000000000000 ) ) ;
#55607 = DIRECTION ( 'NONE',  ( 0.3311129884571304971, 0.9435911131814395114, -0.000000000000000000 ) ) ;
#55608 = DIRECTION ( 'NONE',  ( 0.000000000000000000, 0.1564344650402311743, -0.9876883405951376593 ) ) ;
#55609 = AXIS2_PLACEMENT_3D ( 'NONE', #7682, #31345, #30598 ) ;
#55610 = DIRECTION ( 'NONE',  ( 0.000000000000000000, 0.000000000000000000, 1.000000000000000000 ) ) ;
#55611 = CARTESIAN_POINT ( 'NONE',  ( 92.35003714631601213, -208.4700003402118966, 82.40645685155124056 ) ) ;
#55612 = CARTESIAN_POINT ( 'NONE',  ( 94.99999999999998579, 87.33691857156068750, 88.53156250086716739 ) ) ;
#55613 = CARTESIAN_POINT ( 'NONE',  ( 5.000000000000002665, 21.60688246758586217, 79.10210256391376049 ) ) ;
#55614 = PLANE ( 'NONE',  #44568 ) ;
#55615 = DIRECTION ( 'NONE',  ( 1.000000000000000000, 0.000000000000000000, -0.000000000000000000 ) ) ;
#55616 = LINE ( 'NONE', #67644, #10431 ) ;
#55617 = EDGE_CURVE ( 'NONE', #29007, #68795, #28979, .T. ) ;
#55618 = DIRECTION ( 'NONE',  ( -1.000000000000000000, 0.000000000000000000, 0.000000000000000000 ) ) ;
#55619 = DIRECTION ( 'NONE',  ( 0.000000000000000000, 0.000000000000000000, 1.000000000000000000 ) ) ;
#55620 = AXIS2_PLACEMENT_3D ( 'NONE', #62234, #67120, #4355 ) ;
#55621 = DIRECTION ( 'NONE',  ( -1.000000000000000000, -1.427937372958388501E-15, 7.962523111839142123E-16 ) ) ;
#55622 = EDGE_CURVE ( 'NONE', #47166, #52810, #56926, .T. ) ;
#55623 = CIRCLE ( 'NONE', #20782, 82.00000000000000000 ) ;
#55624 = FACE_OUTER_BOUND ( 'NONE', #6657, .T. ) ;
#55625 = AXIS2_PLACEMENT_3D ( 'NONE', #11107, #28384, #38940 ) ;
#55626 = AXIS2_PLACEMENT_3D ( 'NONE', #20661, #33040, #45468 ) ;
#55627 = CYLINDRICAL_SURFACE ( 'NONE', #26955, 2.649999999999999467 ) ;
#55628 = AXIS2_PLACEMENT_3D ( 'NONE', #49321, #60262, #14739 ) ;
#55629 = CIRCLE ( 'NONE', #28040, 15.99999999999999822 ) ;
#55630 = LINE ( 'NONE', #22539, #31074 ) ;
#55631 = CARTESIAN_POINT ( 'NONE',  ( -96.32499999999996021, -212.2949673200287179, 86.29583333333333428 ) ) ;
#55632 = LINE ( 'NONE', #9388, #39829 ) ;
#55633 = CARTESIAN_POINT ( 'NONE',  ( 10.00000000000000000, 4.992566952384984269, 37.16516213103279398 ) ) ;
#55634 = CARTESIAN_POINT ( 'NONE',  ( 11.99999999999999822, -74.65491531819111515, -8.830959090343204920 ) ) ;
#55635 = DIRECTION ( 'NONE',  ( 0.6575728627325957421, -0.7533909544171993877, -1.230411769795008318E-16 ) ) ;
#55636 = DIRECTION ( 'NONE',  ( -1.000000000000000000, 0.000000000000000000, 0.000000000000000000 ) ) ;
#55637 = CARTESIAN_POINT ( 'NONE',  ( 92.69370383062501162, -209.9999999999999716, 89.80156250086714920 ) ) ;
#55638 = ORIENTED_EDGE ( 'NONE', *, *, #50818, .F. ) ;
#55639 = VERTEX_POINT ( 'NONE', #28600 ) ;
#55640 = DIRECTION ( 'NONE',  ( -0.000000000000000000, -0.000000000000000000, 1.000000000000000000 ) ) ;
#55641 = CARTESIAN_POINT ( 'NONE',  ( 10.00000000000000000, 6.736453364084091788, -36.88895765772625879 ) ) ;
#55642 = VERTEX_POINT ( 'NONE', #17701 ) ;
#55643 = CIRCLE ( 'NONE', #22063, 82.00000000000000000 ) ;
#55644 = CARTESIAN_POINT ( 'NONE',  ( 96.15314808468748708, -208.0026889286704943, 78.00114583420048575 ) ) ;
#55645 = CARTESIAN_POINT ( 'NONE',  ( 93.84685191531249870, -208.0026889286704943, 86.52072916753382970 ) ) ;
#55646 = ORIENTED_EDGE ( 'NONE', *, *, #33201, .F. ) ;
#55647 = CARTESIAN_POINT ( 'NONE',  ( 93.84685191531251292, -211.9973110713294489, 85.46239583420047836 ) ) ;
#55648 = CARTESIAN_POINT ( 'NONE',  ( 93.67500000000001137, -212.2949673200287179, 78.12020833506763040 ) ) ;
#55649 = ADVANCED_FACE ( 'NONE', ( #22988 ), #22235, .T. ) ;
#55650 = ORIENTED_EDGE ( 'NONE', *, *, #63876, .F. ) ;
#55651 = CARTESIAN_POINT ( 'NONE',  ( -92.34999999999999432, -209.9999999999999716, 78.25249999999999773 ) ) ;
#55652 = VERTEX_POINT ( 'NONE', #40267 ) ;
#55653 = CARTESIAN_POINT ( 'NONE',  ( -92.69370383062502583, 89.06967028092473981, 74.84209033237942776 ) ) ;
#55654 = VECTOR ( 'NONE', #37073, 999.9999999999998863 ) ;
#55655 = ORIENTED_EDGE ( 'NONE', *, *, #70177, .T. ) ;
#55656 = ORIENTED_EDGE ( 'NONE', *, *, #63705, .F. ) ;
#55657 = CARTESIAN_POINT ( 'NONE',  ( -92.35000000035638834, 89.99995654222792041, 89.12687334326074051 ) ) ;
#55658 = EDGE_CURVE ( 'NONE', #66947, #60556, #61545, .T. ) ;
#55659 = ORIENTED_EDGE ( 'NONE', *, *, #10251, .F. ) ;
#55660 = CARTESIAN_POINT ( 'NONE',  ( 0.000000000000000000, -81.34940948281344220, 10.30890764327356557 ) ) ;
#55661 = CARTESIAN_POINT ( 'NONE',  ( 0.000000000000000000, 0.000000000000000000, 0.000000000000000000 ) ) ;
#55662 = EDGE_CURVE ( 'NONE', #38385, #48805, #73543, .T. ) ;
#55663 = VERTEX_POINT ( 'NONE', #41017 ) ;
#55664 = DIRECTION ( 'NONE',  ( 1.000000000000000000, 0.000000000000000000, 0.000000000000000000 ) ) ;
#55665 = AXIS2_PLACEMENT_3D ( 'NONE', #44385, #49273, #55290 ) ;
#55666 = VERTEX_POINT ( 'NONE', #62480 ) ;
#55667 = DIRECTION ( 'NONE',  ( -1.000000000000000000, 0.000000000000000000, 0.000000000000000000 ) ) ;
#55668 = AXIS2_PLACEMENT_3D ( 'NONE', #30290, #52117, #52480 ) ;
#55669 = ORIENTED_EDGE ( 'NONE', *, *, #44199, .F. ) ;
#55670 = EDGE_CURVE ( 'NONE', #66304, #41093, #30344, .T. ) ;
#55671 = ORIENTED_EDGE ( 'NONE', *, *, #4103, .T. ) ;
#55672 = VECTOR ( 'NONE', #73920, 1000.000000000000000 ) ;
#55673 = ORIENTED_EDGE ( 'NONE', *, *, #23587, .T. ) ;
#55674 = CARTESIAN_POINT ( 'NONE',  ( 92.69370383062501162, -211.3315407142195852, 75.72572916753381378 ) ) ;
#55675 = AXIS2_PLACEMENT_3D ( 'NONE', #21031, #10498, #72164 ) ;
#55676 = ITEM_DEFINED_TRANSFORMATION ( 'NONE', 'NONE', #29183,  #43395 ) ;
#55677 = DIRECTION ( 'NONE',  ( -1.000000000000000000, 0.000000000000000000, 0.000000000000000000 ) ) ;
#55678 = ORIENTED_EDGE ( 'NONE', *, *, #50656, .T. ) ;
#55679 = EDGE_LOOP ( 'NONE', ( #24861, #12013, #38662, #71355 ) ) ;
#55680 = ORIENTED_EDGE ( 'NONE', *, *, #65869, .T. ) ;
#55681 = DIRECTION ( 'NONE',  ( -0.9966891607226786576, -0.08130631524009861166, 0.000000000000000000 ) ) ;
#55682 = DIRECTION ( 'NONE',  ( 0.000000000000000000, 0.000000000000000000, 1.000000000000000000 ) ) ;
#55683 = CARTESIAN_POINT ( 'NONE',  ( -97.65000000000001990, 90.00000000000004263, 90.00000000000000000 ) ) ;
#55684 = VERTEX_POINT ( 'NONE', #22609 ) ;
#55685 = EDGE_CURVE ( 'NONE', #69332, #56782, #68482, .T. ) ;
#55686 = CARTESIAN_POINT ( 'NONE',  ( 97.30629616937498838, 91.33154071421968467, 76.67822916753378593 ) ) ;
#55687 = ORIENTED_EDGE ( 'NONE', *, *, #23458, .T. ) ;
#55688 = CARTESIAN_POINT ( 'NONE',  ( 97.65000000000000568, 89.99998452726534026, 78.33187446658581621 ) ) ;
#55689 = CARTESIAN_POINT ( 'NONE',  ( -97.30629616937495996, -209.9999999999999716, 89.00781250086714635 ) ) ;
#55690 = EDGE_LOOP ( 'NONE', ( #43485, #12685, #57229, #13290 ) ) ;
#55692 = EDGE_CURVE ( 'NONE', #37007, #73707, #39965, .T. ) ;
#55691 = CARTESIAN_POINT ( 'NONE',  ( 1.898848305348270982, -4.677202111653177674, -0.6020238742160556322 ) ) ;
#55693 = DIRECTION ( 'NONE',  ( -1.000000000000000000, 0.000000000000000000, -0.000000000000000000 ) ) ;
#55694 = CARTESIAN_POINT ( 'NONE',  ( 0.000000000000000000, -10.45096189432314837, -21.10159698893440350 ) ) ;
#55695 = CARTESIAN_POINT ( 'NONE',  ( -96.15314808468747287, -208.0026889286704943, 78.74197916753381321 ) ) ;
#55696 = AXIS2_PLACEMENT_3D ( 'NONE', #63467, #46911, #70181 ) ;
#55697 = DIRECTION ( 'NONE',  ( 0.4279312458752991266, 0.9038112904824847638, 0.000000000000000000 ) ) ;
#55698 = LINE ( 'NONE', #55324, #36684 ) ;
#55699 = ADVANCED_FACE ( 'NONE', ( #71407 ), #59047, .T. ) ;
#55700 = DIRECTION ( 'NONE',  ( 1.000000000000000000, -3.974818696583893186E-13, -2.612289469705706870E-14 ) ) ;
#55701 = VERTEX_POINT ( 'NONE', #41379 ) ;
#55702 = ORIENTED_EDGE ( 'NONE', *, *, #6720, .F. ) ;
#55703 = LINE ( 'NONE', #15853, #34858 ) ;
#55704 = DIRECTION ( 'NONE',  ( 0.000000000000000000, 0.000000000000000000, 1.000000000000000000 ) ) ;
#55705 = CARTESIAN_POINT ( 'NONE',  ( 94.21072067537654959, -207.7213858236421231, 74.85481846778738202 ) ) ;
#55706 = EDGE_CURVE ( 'NONE', #70972, #22766, #21778, .T. ) ;
#55707 = CARTESIAN_POINT ( 'NONE',  ( -95.00000000000002842, 87.33691857156074434, 82.81656250086713555 ) ) ;
#55708 = DIRECTION ( 'NONE',  ( -0.000000000000000000, -0.000000000000000000, 1.000000000000000000 ) ) ;
#55709 = DIRECTION ( 'NONE',  ( 0.000000000000000000, 0.9238795325112851842, 0.3826834323650937786 ) ) ;
#55710 = VERTEX_POINT ( 'NONE', #65790 ) ;
#55711 = DIRECTION ( 'NONE',  ( 0.000000000000000000, 0.000000000000000000, -1.000000000000000000 ) ) ;
#55712 = DIRECTION ( 'NONE',  ( 2.603472992746261562E-14, 2.546204323184492723E-14, -1.000000000000000000 ) ) ;
#55713 = DIRECTION ( 'NONE',  ( -1.000000000000000000, -0.000000000000000000, 0.000000000000000000 ) ) ;
#55714 = AXIS2_PLACEMENT_3D ( 'NONE', #51503, #59, #34579 ) ;
#55715 = CARTESIAN_POINT ( 'NONE',  ( -92.35000000000003695, 90.00000000000004263, 89.68250000000000455 ) ) ;
#55716 = CARTESIAN_POINT ( 'NONE',  ( 92.35000000045006630, -210.0000310946952595, 88.81037122969986797 ) ) ;
#55717 = CARTESIAN_POINT ( 'NONE',  ( -92.69370383062498320, -208.6684592857803011, 80.64697916753382856 ) ) ;
#55718 = CARTESIAN_POINT ( 'NONE',  ( -92.34999999999999432, -209.9999753241900748, 87.22187585518541653 ) ) ;
#55719 = AXIS2_PLACEMENT_3D ( 'NONE', #67967, #39025, #73964 ) ;
#55720 = ORIENTED_EDGE ( 'NONE', *, *, #72797, .T. ) ;
#55721 = AXIS2_PLACEMENT_3D ( 'NONE', #48611, #66644, #36214 ) ;
#55722 = CARTESIAN_POINT ( 'NONE',  ( 1.560000000000000053, 0.000000000000000000, 0.000000000000000000 ) ) ;
#55723 = DIRECTION ( 'NONE',  ( 0.000000000000000000, -0.8910065241883626808, -0.4539904997395570740 ) ) ;
#55724 = DIRECTION ( 'NONE',  ( -1.000000000000000000, -0.000000000000000000, -0.000000000000000000 ) ) ;
#55725 = ORIENTED_EDGE ( 'NONE', *, *, #59268, .T. ) ;
#55726 = FACE_OUTER_BOUND ( 'NONE', #67, .T. ) ;
#55727 = CARTESIAN_POINT ( 'NONE',  ( 0.000000000000000000, -26.01480285779785362, -70.53064760720343429 ) ) ;
#55728 = AXIS2_PLACEMENT_3D ( 'NONE', #25009, #47950, #26115 ) ;
#55729 = CIRCLE ( 'NONE', #54544, 16.00000000000000000 ) ;
#55730 = UNCERTAINTY_MEASURE_WITH_UNIT (LENGTH_MEASURE( 1.000000000000000082E-05 ), #19864, 'distance_accuracy_value', 'NONE');
#55731 = CARTESIAN_POINT ( 'NONE',  ( 5.000000000000000000, 32.34446384429971744, 26.79245525562726016 ) ) ;
#55732 = ORIENTED_EDGE ( 'NONE', *, *, #40981, .T. ) ;
#55733 = DIRECTION ( 'NONE',  ( 1.000000000000000000, 0.000000000000000000, 0.000000000000000000 ) ) ;
#55734 = CARTESIAN_POINT ( 'NONE',  ( 12.13205353604972814, -140.1820037904669789, -2.500000000000000000 ) ) ;
#55735 = ORIENTED_EDGE ( 'NONE', *, *, #16538, .T. ) ;
#55736 = VECTOR ( 'NONE', #14066, 1000.000000000000000 ) ;
#55737 = DIRECTION ( 'NONE',  ( -1.000000000000000000, -0.000000000000000000, -0.000000000000000000 ) ) ;
#55738 = CARTESIAN_POINT ( 'NONE',  ( 92.34999999999999432, 90.00000000000002842, 84.92000000000000171 ) ) ;
#55739 = ORIENTED_EDGE ( 'NONE', *, *, #55365, .T. ) ;
#55740 = AXIS2_PLACEMENT_3D ( 'NONE', #23778, #64748, #46718 ) ;
#55741 = EDGE_CURVE ( 'NONE', #71076, #48732, #53761, .T. ) ;
#55742 = DIRECTION ( 'NONE',  ( 0.000000000000000000, 0.000000000000000000, 1.000000000000000000 ) ) ;
#55743 = VERTEX_POINT ( 'NONE', #13895 ) ;
#55744 = DIRECTION ( 'NONE',  ( -0.000000000000000000, -0.000000000000000000, -1.000000000000000000 ) ) ;
#55745 = LINE ( 'NONE', #4262, #61255 ) ;
#55746 = EDGE_CURVE ( 'NONE', #5309, #65173, #59132, .T. ) ;
#55747 = VERTEX_POINT ( 'NONE', #65063 ) ;
#55748 = VERTEX_POINT ( 'NONE', #36836 ) ;
#55749 = EDGE_CURVE ( 'NONE', #62067, #57334, #18329, .T. ) ;
#55750 = EDGE_CURVE ( 'NONE', #19617, #67442, #24454, .T. ) ;
#55751 = ORIENTED_EDGE ( 'NONE', *, *, #64317, .F. ) ;
#55752 = CARTESIAN_POINT ( 'NONE',  ( 10.00000000000000000, -33.17418723428319538, 17.67226234102814431 ) ) ;
#55753 = ORIENTED_EDGE ( 'NONE', *, *, #7656, .F. ) ;
#55754 = AXIS2_PLACEMENT_3D ( 'NONE', #11140, #45744, #50987 ) ;
#55756 = EDGE_CURVE ( 'NONE', #62740, #185, #59411, .T. ) ;
#55755 = VERTEX_POINT ( 'NONE', #36464 ) ;
#55757 = CARTESIAN_POINT ( 'NONE',  ( 97.30629616937498838, 88.66845928578037217, 76.73114583420048973 ) ) ;
#55758 = DIRECTION ( 'NONE',  ( -1.000000000000000000, 0.000000000000000000, 0.000000000000000000 ) ) ;
#55759 = DIRECTION ( 'NONE',  ( 0.000000000000000000, 0.000000000000000000, 1.000000000000000000 ) ) ;
#55760 = EDGE_LOOP ( 'NONE', ( #15331, #21646, #49359, #59742 ) ) ;
#55761 = VERTEX_POINT ( 'NONE', #64680 ) ;
#55762 = EDGE_CURVE ( 'NONE', #61705, #20201, #6792, .T. ) ;
#55763 = VERTEX_POINT ( 'NONE', #31194 ) ;
#55764 = CARTESIAN_POINT ( 'NONE',  ( 92.69370383062498320, 90.00000000000002842, 87.10281250086714522 ) ) ;
#55765 = EDGE_LOOP ( 'NONE', ( #68189, #30269, #34068, #28051 ) ) ;
#55766 = CARTESIAN_POINT ( 'NONE',  ( 93.84685191531251292, -211.9973110713294489, 84.66864583420047552 ) ) ;
#55767 = AXIS2_PLACEMENT_3D ( 'NONE', #9328, #38282, #25515 ) ;
#55768 = DIRECTION ( 'NONE',  ( -5.551115123125782702E-17, 0.000000000000000000, -1.000000000000000000 ) ) ;
#55769 = FACE_OUTER_BOUND ( 'NONE', #54707, .T. ) ;
#55770 = CARTESIAN_POINT ( 'NONE',  ( 11.99999999999999822, 11.30684508768339569, 76.66974797899841576 ) ) ;
#55771 = DIRECTION ( 'NONE',  ( 0.000000000000000000, -0.9781476007338067991, -0.2079116908177533196 ) ) ;
#55772 = DIRECTION ( 'NONE',  ( 0.000000000000000000, -0.3090169943749549453, 0.9510565162951511997 ) ) ;
#55773 = CARTESIAN_POINT ( 'NONE',  ( 10.00000000000000000, 37.16516213103285082, -4.992566952384588141 ) ) ;
#55774 = CARTESIAN_POINT ( 'NONE',  ( 97.64999999999990621, 90.00000071509185773, 85.31687502647973531 ) ) ;
#55775 = CARTESIAN_POINT ( 'NONE',  ( -93.84685191531248449, -208.0026889286704943, 86.89114583420047211 ) ) ;
#55776 = CARTESIAN_POINT ( 'NONE',  ( -92.69370383062502583, 88.66845928578038638, 84.35114583420049428 ) ) ;
#55777 = ORIENTED_EDGE ( 'NONE', *, *, #37770, .T. ) ;
#55779 = CARTESIAN_POINT ( 'NONE',  ( -97.30629616937501680, 90.00000000000004263, 87.73781250086713612 ) ) ;
#55778 = CARTESIAN_POINT ( 'NONE',  ( 92.69370383062498320, 91.33154071421968467, 88.31989583420046586 ) ) ;
#55780 = ORIENTED_EDGE ( 'NONE', *, *, #73732, .F. ) ;
#55781 = AXIS2_PLACEMENT_3D ( 'NONE', #33906, #56849, #38808 ) ;
#55783 = EDGE_CURVE ( 'NONE', #52606, #63903, #30450, .T. ) ;
#55782 = DIRECTION ( 'NONE',  ( -1.000000000000000000, -0.000000000000000000, -0.000000000000000000 ) ) ;
#55784 = VECTOR ( 'NONE', #64746, 1000.000000000000000 ) ;
#55785 = CARTESIAN_POINT ( 'NONE',  ( -7.500000000000014211, -69.70000000000001705, -204.9999999999999716 ) ) ;
#55786 = LINE ( 'NONE', #9553, #4818 ) ;
#55787 = CARTESIAN_POINT ( 'NONE',  ( -93.84685191531247028, -211.9973110713294489, 89.21947916753380525 ) ) ;
#55788 = CYLINDRICAL_SURFACE ( 'NONE', #13712, 2.649999999999985700 ) ;
#55789 = FACE_OUTER_BOUND ( 'NONE', #72802, .T. ) ;
#55790 = EDGE_CURVE ( 'NONE', #57242, #51571, #55527, .T. ) ;
#55791 = ADVANCED_FACE ( 'NONE', ( #48495 ), #64315, .F. ) ;
#55792 = CARTESIAN_POINT ( 'NONE',  ( -0.0004442498512760095037, 0.001194404164628348752, -49.00000000000000000 ) ) ;
#55793 = ORIENTED_EDGE ( 'NONE', *, *, #31039, .T. ) ;
#55794 = ORIENTED_EDGE ( 'NONE', *, *, #41363, .F. ) ;
#55795 = VECTOR ( 'NONE', #53405, 1000.000000000000000 ) ;
#55796 = CARTESIAN_POINT ( 'NONE',  ( -96.32500000000001705, 87.70503267997129626, 80.58083333333331666 ) ) ;
#55797 = DIRECTION ( 'NONE',  ( 0.000000000000000000, 0.000000000000000000, 1.000000000000000000 ) ) ;
#55798 = EDGE_CURVE ( 'NONE', #68814, #27944, #12318, .T. ) ;
#55799 = DIRECTION ( 'NONE',  ( -1.000000000000000000, 0.000000000000000000, -0.000000000000000000 ) ) ;
#55800 = DIRECTION ( 'NONE',  ( -0.000000000000000000, -0.000000000000000000, 1.000000000000000000 ) ) ;
#55801 = AXIS2_PLACEMENT_3D ( 'NONE', #14963, #37538, #54445 ) ;
#55802 = CARTESIAN_POINT ( 'NONE',  ( 96.92442009029373651, 88.17815826261617929, 75.00000000000000000 ) ) ;
#55803 = DIRECTION ( 'NONE',  ( -1.000000000000000000, 0.000000000000000000, 0.000000000000000000 ) ) ;
#55804 = CARTESIAN_POINT ( 'NONE',  ( -96.32499999999996021, -207.7050326799711968, 79.73416666666666686 ) ) ;
#55805 = EDGE_LOOP ( 'NONE', ( #41354, #2842 ) ) ;
#55806 = CARTESIAN_POINT ( 'NONE',  ( -95.00000000000002842, 87.33691857156074434, 82.18156250086714465 ) ) ;
#55807 = VECTOR ( 'NONE', #33381, 1000.000000000000114 ) ;
#55808 = CARTESIAN_POINT ( 'NONE',  ( 10.00000000000000000, -37.48860685352290290, -0.8828120875904512665 ) ) ;
#55809 = CARTESIAN_POINT ( 'NONE',  ( -13.05994868825747446, -139.5943292883446532, 5.500000000000000000 ) ) ;
#55810 = FACE_OUTER_BOUND ( 'NONE', #47846, .T. ) ;
#55811 = DIRECTION ( 'NONE',  ( -1.000000000000000000, -0.000000000000000000, -0.000000000000000000 ) ) ;
#55812 = DIRECTION ( 'NONE',  ( -1.000000000000000000, 0.000000000000000000, 0.000000000000000000 ) ) ;
#55813 = CARTESIAN_POINT ( 'NONE',  ( 11.99999999999999822, -46.53671651293991118, 59.03961581697383565 ) ) ;
#55814 = SURFACE_SIDE_STYLE ('',( #5444 ) ) ;
#55815 = CARTESIAN_POINT ( 'NONE',  ( 92.35000000021534561, -209.9999789922616458, 79.91868729553134187 ) ) ;
#55816 =( BOUNDED_CURVE ( )  B_SPLINE_CURVE ( 2, ( #61071, #16319, #55802 ),
 .UNSPECIFIED., .F., .T. ) 
 B_SPLINE_CURVE_WITH_KNOTS ( ( 3, 3 ),
 ( 0.9791666666666669627, 0.9841647806526081510 ),
 .UNSPECIFIED. ) 
 CURVE ( )  GEOMETRIC_REPRESENTATION_ITEM ( )  RATIONAL_B_SPLINE_CURVE ( ( 0.9999999999999935607, 0.9035746763527595649, 0.9459494432169361922 ) ) 
 REPRESENTATION_ITEM ( '' )  );
#55817 = CARTESIAN_POINT ( 'NONE',  ( 94.99999999999998579, 92.66308142843932671, 80.11781250086714579 ) ) ;
#55818 = CARTESIAN_POINT ( 'NONE',  ( -92.69370383062498320, -208.6684592857803295, 83.82197916753382572 ) ) ;
#55819 = CARTESIAN_POINT ( 'NONE',  ( 5.000000000000000000, 36.13751322684419165, 21.40280677340384585 ) ) ;
#55820 = ORIENTED_EDGE ( 'NONE', *, *, #15452, .T. ) ;
#55821 = CARTESIAN_POINT ( 'NONE',  ( -97.65000000000001990, 90.00000000000004263, 83.09437500173430635 ) ) ;
#55822 = CARTESIAN_POINT ( 'NONE',  ( -92.34999999999999432, -208.4700217866474645, 77.67041666666665378 ) ) ;
#55823 = CARTESIAN_POINT ( 'NONE',  ( -97.64999999999996305, -209.9999999999999716, 90.00000000000000000 ) ) ;
#55824 = CIRCLE ( 'NONE', #11377, 0.9999999999999991118 ) ;
#55825 = CARTESIAN_POINT ( 'NONE',  ( -93.84685191531252713, 88.00268892867056536, 79.21822916753382060 ) ) ;
#55826 = CARTESIAN_POINT ( 'NONE',  ( 92.69370383062501162, -208.6684592857803011, 80.69989583420048973 ) ) ;
#55827 = ORIENTED_EDGE ( 'NONE', *, *, #32981, .T. ) ;
#55828 = CARTESIAN_POINT ( 'NONE',  ( -26.53422223201112828, -120.6595836127786043, -5.500000000000000000 ) ) ;
#55829 = VERTEX_POINT ( 'NONE', #24099 ) ;
#55830 = DIRECTION ( 'NONE',  ( 1.000000000000000000, -0.000000000000000000, -0.000000000000000000 ) ) ;
#55831 = VECTOR ( 'NONE', #32556, 1000.000000000000000 ) ;
#55832 = ORIENTED_EDGE ( 'NONE', *, *, #55019, .T. ) ;
#55833 = CARTESIAN_POINT ( 'NONE',  ( -92.34999999999999432, -209.9999999999999716, 83.33250000000001023 ) ) ;
#55834 = CIRCLE ( 'NONE', #20999, 31.99999999999998224 ) ;
#55835 = EDGE_CURVE ( 'NONE', #57645, #19199, #32691, .T. ) ;
#55836 = ORIENTED_EDGE ( 'NONE', *, *, #15121, .F. ) ;
#55837 = VERTEX_POINT ( 'NONE', #32295 ) ;
#55838 = AXIS2_PLACEMENT_3D ( 'NONE', #65783, #43608, #14641 ) ;
#55840 = EDGE_CURVE ( 'NONE', #51073, #57704, #18908, .T. ) ;
#55839 = VERTEX_POINT ( 'NONE', #38326 ) ;
#55841 = EDGE_CURVE ( 'NONE', #7754, #56288, #68792, .T. ) ;
#55842 = CARTESIAN_POINT ( 'NONE',  ( 97.64999999999999147, -209.9999999999999716, 90.00000000000000000 ) ) ;
#55843 = CYLINDRICAL_SURFACE ( 'NONE', #72891, 16.00000000000000000 ) ;
#55844 = DIRECTION ( 'NONE',  ( -0.8660254037844380415, 0.5000000000000008882, 0.000000000000000000 ) ) ;
#55845 = DIRECTION ( 'NONE',  ( 0.000000000000000000, 0.4539904997395478037, -0.8910065241883673437 ) ) ;
#55846 = CARTESIAN_POINT ( 'NONE',  ( 92.69370383062498320, 88.66845928578037217, 86.67947916753382742 ) ) ;
#55847 = DIRECTION ( 'NONE',  ( -0.000000000000000000, -0.000000000000000000, -1.000000000000000000 ) ) ;
#55848 = CARTESIAN_POINT ( 'NONE',  ( 96.32499999999998863, -212.2949673200287179, 78.14666666666667538 ) ) ;
#55849 = VECTOR ( 'NONE', #44976, 1000.000000000000000 ) ;
#55850 = VERTEX_POINT ( 'NONE', #9376 ) ;
#55851 = ORIENTED_EDGE ( 'NONE', *, *, #126, .T. ) ;
#55852 = ORIENTED_EDGE ( 'NONE', *, *, #62151, .T. ) ;
#55853 = ORIENTED_EDGE ( 'NONE', *, *, #67467, .F. ) ;
#55854 = CARTESIAN_POINT ( 'NONE',  ( -0.0004442498525516064278, 0.001194404164626844313, -64.00000000000000000 ) ) ;
#55855 = DIRECTION ( 'NONE',  ( -0.000000000000000000, -0.000000000000000000, 1.000000000000000000 ) ) ;
#55856 = CIRCLE ( 'NONE', #23455, 31.99999999999999289 ) ;
#55857 = DIRECTION ( 'NONE',  ( 0.000000000000000000, 0.000000000000000000, 1.000000000000000000 ) ) ;
#55858 = DIRECTION ( 'NONE',  ( -1.000000000000000000, -0.000000000000000000, -0.000000000000000000 ) ) ;
#55859 = CARTESIAN_POINT ( 'NONE',  ( 10.00000000000000000, 16.65560815589411092, 38.55633173627015964 ) ) ;
#55860 = EDGE_CURVE ( 'NONE', #46998, #45794, #29443, .T. ) ;
#55861 = LINE ( 'NONE', #61507, #7964 ) ;
#55862 = VERTEX_POINT ( 'NONE', #66892 ) ;
#55863 = CARTESIAN_POINT ( 'NONE',  ( -93.67499999999998295, -212.2949673200287179, 81.40104166840096411 ) ) ;
#55864 = EDGE_LOOP ( 'NONE', ( #69339, #4040, #25347, #47013 ) ) ;
#55865 = FACE_OUTER_BOUND ( 'NONE', #2208, .T. ) ;
#55866 = EDGE_LOOP ( 'NONE', ( #16989, #46876, #27014, #35958 ) ) ;
#55868 = CARTESIAN_POINT ( 'NONE',  ( -97.65000000000001990, 88.47002178664754979, 81.87729166840097150 ) ) ;
#55867 = CARTESIAN_POINT ( 'NONE',  ( 94.99999999999998579, 93.05995642670504253, 82.93562500173429441 ) ) ;
#55869 = ORIENTED_EDGE ( 'NONE', *, *, #47196, .F. ) ;
#55870 = CARTESIAN_POINT ( 'NONE',  ( 96.15314808468748708, 88.00268892867053694, 81.75822916753382685 ) ) ;
#55871 = CARTESIAN_POINT ( 'NONE',  ( -97.64999999999996305, -209.9999999999999716, 86.82500000000000284 ) ) ;
#55872 = DIRECTION ( 'NONE',  ( -1.000000000000000000, 0.000000000000000000, -0.000000000000000000 ) ) ;
#55873 = FACE_OUTER_BOUND ( 'NONE', #13054, .T. ) ;
#55874 = DIRECTION ( 'NONE',  ( 1.000000000000000000, 0.000000000000000000, 0.000000000000000000 ) ) ;
#55875 = CARTESIAN_POINT ( 'NONE',  ( 97.64999999999999147, 90.00000000000002842, 87.77749999999998920 ) ) ;
#55876 = VERTEX_POINT ( 'NONE', #66173 ) ;
#55877 = CARTESIAN_POINT ( 'NONE',  ( -3.000000000000000000, -1.278221433540502217, 26.51162292216071847 ) ) ;
#55878 = CARTESIAN_POINT ( 'NONE',  ( 0.000000000000000000, 76.69515212746016175, 29.01471420065591289 ) ) ;
#55879 = EDGE_CURVE ( 'NONE', #68271, #44941, #9755, .T. ) ;
#55880 = EDGE_CURVE ( 'NONE', #63637, #73028, #67643, .T. ) ;
#55881 = CARTESIAN_POINT ( 'NONE',  ( 97.64999999999821512, -209.9999969335172807, 75.79187510780352000 ) ) ;
#55882 = AXIS2_PLACEMENT_3D ( 'NONE', #40801, #57721, #70085 ) ;
#55883 = EDGE_LOOP ( 'NONE', ( #14218, #42479, #26690, #7020 ) ) ;
#55884 = ORIENTED_EDGE ( 'NONE', *, *, #46000, .T. ) ;
#55885 = DIRECTION ( 'NONE',  ( 1.000000000000000000, 0.000000000000000000, 0.000000000000000000 ) ) ;
#55886 = DIRECTION ( 'NONE',  ( 1.000000000000000000, -0.000000000000000000, -0.000000000000000000 ) ) ;
#55887 = LINE ( 'NONE', #61907, #6505 ) ;
#55888 = CARTESIAN_POINT ( 'NONE',  ( -97.30629616937497417, -211.3315407142195852, 79.69447916753381378 ) ) ;
#55889 = VERTEX_POINT ( 'NONE', #44341 ) ;
#55890 = CIRCLE ( 'NONE', #28237, 1.000000000000000888 ) ;
#55891 = FACE_OUTER_BOUND ( 'NONE', #23589, .T. ) ;
#55892 = CIRCLE ( 'NONE', #7845, 15.99999999999999822 ) ;
#55893 = VERTEX_POINT ( 'NONE', #54505 ) ;
#55894 = PLANE ( 'NONE',  #47520 ) ;
#55895 = DIRECTION ( 'NONE',  ( 0.000000000000000000, 0.000000000000000000, -1.000000000000000000 ) ) ;
#55896 = CARTESIAN_POINT ( 'NONE',  ( 10.00000000000000000, 72.35432306680455383, 20.40083707023012494 ) ) ;
#55897 = CARTESIAN_POINT ( 'NONE',  ( 97.30629616937498838, 91.33154071421968467, 78.58322916753381548 ) ) ;
#55898 = CARTESIAN_POINT ( 'NONE',  ( 0.000000000000000000, 27.75498641678742473, 31.52238457039609187 ) ) ;
#55899 = DIRECTION ( 'NONE',  ( 1.000000000000000000, 0.000000000000000000, 0.000000000000000000 ) ) ;
#55900 = AXIS2_PLACEMENT_3D ( 'NONE', #28053, #21675, #72429 ) ;
#55901 = DIRECTION ( 'NONE',  ( 0.000000000000000000, 0.000000000000000000, -1.000000000000000000 ) ) ;
#55902 = CARTESIAN_POINT ( 'NONE',  ( 95.77009744696134419, 92.23316662872740324, 74.81945665767625542 ) ) ;
#55903 = CARTESIAN_POINT ( 'NONE',  ( 11.99999999999999822, -26.01480285779885904, 70.53064760720306481 ) ) ;
#55904 = DIRECTION ( 'NONE',  ( 1.000000000000000000, 0.000000000000000000, 0.000000000000000000 ) ) ;
#55905 = AXIS2_PLACEMENT_3D ( 'NONE', #58011, #17780, #24536 ) ;
#55906 = DIRECTION ( 'NONE',  ( -1.000000000000000000, 0.000000000000000000, 0.000000000000000000 ) ) ;
#55907 = DIRECTION ( 'NONE',  ( 0.9781476007338069101, 0.000000000000000000, -0.2079116908177528755 ) ) ;
#55908 = CARTESIAN_POINT ( 'NONE',  ( -94.99999999999997158, -213.0599564267049857, 75.63312500173429953 ) ) ;
#55909 = ORIENTED_EDGE ( 'NONE', *, *, #70927, .F. ) ;
#55910 = CARTESIAN_POINT ( 'NONE',  ( -96.15314808468752972, 91.99731107132950569, 83.82197916753381151 ) ) ;
#55911 = DIRECTION ( 'NONE',  ( 1.000000000000000000, -0.000000000000000000, -0.000000000000000000 ) ) ;
#55912 = AXIS2_PLACEMENT_3D ( 'NONE', #60650, #32051, #72275 ) ;
#55913 = CYLINDRICAL_SURFACE ( 'NONE', #22217, 82.00000000000000000 ) ;
#55914 = ORIENTED_EDGE ( 'NONE', *, *, #14241, .T. ) ;
#55915 = FACE_OUTER_BOUND ( 'NONE', #45447, .T. ) ;
#55916 = DIRECTION ( 'NONE',  ( -0.000000000000000000, -0.000000000000000000, -1.000000000000000000 ) ) ;
#55917 = CARTESIAN_POINT ( 'NONE',  ( 10.00000000000000000, 0.000000000000000000, 0.000000000000000000 ) ) ;
#55918 = PRODUCT_RELATED_PRODUCT_CATEGORY ( 'part', '', ( #37971 ) ) ;
#55919 = EDGE_CURVE ( 'NONE', #64962, #7487, #20663, .T. ) ;
#55920 = CARTESIAN_POINT ( 'NONE',  ( 0.000000000000000000, -1.467624384280027838, 2.542000000000001592 ) ) ;
#55921 = CARTESIAN_POINT ( 'NONE',  ( 92.69370383062501162, -209.9999999999999716, 80.27656250086714351 ) ) ;
#55922 = ADVANCED_FACE ( 'NONE', ( #31933 ), #32670, .T. ) ;
#55923 = ORIENTED_EDGE ( 'NONE', *, *, #31391, .F. ) ;
#55924 = EDGE_LOOP ( 'NONE', ( #33937, #49132, #39350, #55055 ) ) ;
#55925 = EDGE_CURVE ( 'NONE', #40890, #51530, #4505, .T. ) ;
#55926 = CARTESIAN_POINT ( 'NONE',  ( 15.00000000000000000, 8.688484142253932063, -21.88630264137371029 ) ) ;
#55927 = DIRECTION ( 'NONE',  ( -1.000000000000000000, -0.000000000000000000, 0.000000000000000000 ) ) ;
#55928 = CARTESIAN_POINT ( 'NONE',  ( -97.64999999999996305, -208.4700217866474645, 85.58145833506763722 ) ) ;
#55929 = CARTESIAN_POINT ( 'NONE',  ( 11.99999999999999822, -59.03961581697432592, 46.53671651293927880 ) ) ;
#55930 = EDGE_CURVE ( 'NONE', #48180, #13600, #4136, .T. ) ;
#55931 = CIRCLE ( 'NONE', #1984, 31.99999999999999645 ) ;
#55932 = DIRECTION ( 'NONE',  ( 0.000000000000000000, 0.000000000000000000, 1.000000000000000000 ) ) ;
#55933 = CARTESIAN_POINT ( 'NONE',  ( 92.35000000000002274, -208.4700217866474645, 87.40708333333333258 ) ) ;
#55934 = ORIENTED_EDGE ( 'NONE', *, *, #71433, .T. ) ;
#55935 = CARTESIAN_POINT ( 'NONE',  ( 0.000000000000000000, -78.73519480814938731, -22.90783923731713045 ) ) ;
#55936 = ORIENTED_EDGE ( 'NONE', *, *, #9099, .F. ) ;
#55937 = VERTEX_POINT ( 'NONE', #21774 ) ;
#55938 = PLANE ( 'NONE',  #63409 ) ;
#55939 = AXIS2_PLACEMENT_3D ( 'NONE', #44275, #8949, #12815 ) ;
#55940 = CARTESIAN_POINT ( 'NONE',  ( -92.35000000000005116, 91.52997821335253548, 89.17979166840096639 ) ) ;
#55941 = CIRCLE ( 'NONE', #24757, 15.99999999999999822 ) ;
#55942 = ORIENTED_EDGE ( 'NONE', *, *, #64245, .F. ) ;
#55943 = CARTESIAN_POINT ( 'NONE',  ( 97.64999999999999147, -209.9999999999999716, 80.87187500173430976 ) ) ;
#55944 = CARTESIAN_POINT ( 'NONE',  ( 92.34999999999999432, 91.52997821335252127, 81.69208333333332916 ) ) ;
#55945 = EDGE_CURVE ( 'NONE', #49062, #40306, #20281, .T. ) ;
#55946 = ORIENTED_EDGE ( 'NONE', *, *, #73560, .T. ) ;
#55947 = CARTESIAN_POINT ( 'NONE',  ( -19.90058851926621841, -132.5883508287165853, -2.500000000000000000 ) ) ;
#55948 = ORIENTED_EDGE ( 'NONE', *, *, #73085, .T. ) ;
#55949 = EDGE_CURVE ( 'NONE', #36342, #58159, #55984, .T. ) ;
#55950 = FACE_OUTER_BOUND ( 'NONE', #24742, .T. ) ;
#55951 = CIRCLE ( 'NONE', #42755, 31.99999999999999289 ) ;
#55952 = VERTEX_POINT ( 'NONE', #37593 ) ;
#55953 = CIRCLE ( 'NONE', #53593, 42.00000000000000000 ) ;
#55954 = DIRECTION ( 'NONE',  ( 0.000000000000000000, 0.000000000000000000, 1.000000000000000000 ) ) ;
#55955 = CARTESIAN_POINT ( 'NONE',  ( -96.15314808468751551, 88.00268892867056536, 83.55739583420049144 ) ) ;
#55956 = CARTESIAN_POINT ( 'NONE',  ( 97.30629616937498838, 91.33154071421968467, 77.94822916753381037 ) ) ;
#55957 = ORIENTED_EDGE ( 'NONE', *, *, #33078, .F. ) ;
#55958 = CYLINDRICAL_SURFACE ( 'NONE', #36470, 42.00000000000000000 ) ;
#55959 = CARTESIAN_POINT ( 'NONE',  ( -97.65000000000001990, 90.00000000000004263, 80.47499999999999432 ) ) ;
#55960 = DIRECTION ( 'NONE',  ( -1.000000000000000000, 0.000000000000000000, 0.000000000000000000 ) ) ;
#55961 = EDGE_LOOP ( 'NONE', ( #73684, #69554, #6758, #10202 ) ) ;
#55962 = CARTESIAN_POINT ( 'NONE',  ( 0.000000000000000000, -36.13751322684404244, -21.40280677340410165 ) ) ;
#55963 = CARTESIAN_POINT ( 'NONE',  ( -97.30629616937497417, -208.6684592857803011, 81.96989583420048575 ) ) ;
#55964 = VERTEX_POINT ( 'NONE', #54872 ) ;
#55965 = CIRCLE ( 'NONE', #59565, 16.00000000000000000 ) ;
#55966 = ORIENTED_EDGE ( 'NONE', *, *, #5384, .F. ) ;
#55967 = CARTESIAN_POINT ( 'NONE',  ( -3.000000000000002665, 2.527670993440137339E-15, -20.64000000000000057 ) ) ;
#55968 = EDGE_LOOP ( 'NONE', ( #55118, #62035, #45518, #20986 ) ) ;
#55969 = DIRECTION ( 'NONE',  ( 1.000000000000000000, 0.000000000000000000, 0.000000000000000000 ) ) ;
#55970 = CARTESIAN_POINT ( 'NONE',  ( 10.00000000000000000, -35.95386929396248377, -10.96151621346525751 ) ) ;
#55971 = ORIENTED_EDGE ( 'NONE', *, *, #56467, .F. ) ;
#55972 = CARTESIAN_POINT ( 'NONE',  ( -93.84685191531248449, -208.0026889286704943, 74.82614583420047438 ) ) ;
#55973 = ORIENTED_EDGE ( 'NONE', *, *, #45950, .T. ) ;
#55974 = CARTESIAN_POINT ( 'NONE',  ( 25.38712131070745315, -112.4010479962415872, 2.500000000000000000 ) ) ;
#55975 = DIRECTION ( 'NONE',  ( 0.000000000000000000, 0.000000000000000000, -1.000000000000000000 ) ) ;
#55976 = DIRECTION ( 'NONE',  ( -0.000000000000000000, -0.3090169943749448977, -0.9510565162951543083 ) ) ;
#55977 = CARTESIAN_POINT ( 'NONE',  ( -2.500000000000015543, -73.00000000000001421, -208.2999999999999545 ) ) ;
#55978 = LINE ( 'NONE', #45463, #53422 ) ;
#55979 = LINE ( 'NONE', #62006, #21701 ) ;
#55980 = CARTESIAN_POINT ( 'NONE',  ( 97.30629616937498838, 90.00000000000002842, 88.69031250086715090 ) ) ;
#55981 = CYLINDRICAL_SURFACE ( 'NONE', #7592, 16.00000000000000000 ) ;
#55982 = CARTESIAN_POINT ( 'NONE',  ( -7.499999999999969802, 73.00000000000001421, -255.0000000000000000 ) ) ;
#55983 = FACE_OUTER_BOUND ( 'NONE', #28036, .T. ) ;
#55984 = LINE ( 'NONE', #44723, #72417 ) ;
#55985 = LINE ( 'NONE', #16508, #21211 ) ;
#55986 = LINE ( 'NONE', #33413, #22739 ) ;
#55987 = CARTESIAN_POINT ( 'NONE',  ( -95.00000000000002842, 86.94004357329504273, 87.69812500173429726 ) ) ;
#55988 = CARTESIAN_POINT ( 'NONE',  ( -95.00000000000002842, 93.05995642670504253, 75.87125000000000341 ) ) ;
#55989 = AXIS2_PLACEMENT_3D ( 'NONE', #39898, #74088, #6429 ) ;
#55990 = FACE_OUTER_BOUND ( 'NONE', #16351, .T. ) ;
#55991 = EDGE_CURVE ( 'NONE', #30067, #62636, #510, .T. ) ;
#55992 = CYLINDRICAL_SURFACE ( 'NONE', #58918, 31.99999999999998579 ) ;
#55993 = FACE_OUTER_BOUND ( 'NONE', #48437, .T. ) ;
#55994 = LINE ( 'NONE', #49970, #46708 ) ;
#55995 = AXIS2_PLACEMENT_3D ( 'NONE', #55398, #62544, #43765 ) ;
#55996 = CARTESIAN_POINT ( 'NONE',  ( -92.34999999999999432, -208.4700217866474645, 85.29041666666665833 ) ) ;
#55997 = EDGE_CURVE ( 'NONE', #41513, #45152, #65192, .T. ) ;
#55998 = AXIS2_PLACEMENT_3D ( 'NONE', #56754, #16512, #45477 ) ;
#55999 = ADVANCED_FACE ( 'NONE', ( #34533 ), #69137, .F. ) ;
#56000 = DIRECTION ( 'NONE',  ( 1.000000000000000000, 0.000000000000000000, 0.000000000000000000 ) ) ;
#56001 = CIRCLE ( 'NONE', #51172, 82.00000000000000000 ) ;
#56002 = AXIS2_PLACEMENT_3D ( 'NONE', #57846, #3676, #59687 ) ;
#56003 = CARTESIAN_POINT ( 'NONE',  ( 10.00000000000000000, -73.44644590900078640, 24.73286445877676343 ) ) ;
#56004 = DIRECTION ( 'NONE',  ( 1.000000000000000000, 0.000000000000000000, 0.000000000000000000 ) ) ;
#56005 = DIRECTION ( 'NONE',  ( -1.000000000000000000, -0.000000000000000000, 0.000000000000000000 ) ) ;
#56006 = EDGE_CURVE ( 'NONE', #19127, #16009, #32751, .T. ) ;
#56007 = PLANE ( 'NONE',  #25774 ) ;
#56008 = CARTESIAN_POINT ( 'NONE',  ( 95.00000000000000000, -212.6630814284392557, 88.05531250086716000 ) ) ;
#56009 = CIRCLE ( 'NONE', #15165, 32.00000000000000000 ) ;
#56010 = VERTEX_POINT ( 'NONE', #34916 ) ;
#56011 = VERTEX_POINT ( 'NONE', #56371 ) ;
#56012 = DIRECTION ( 'NONE',  ( 1.000000000000000000, 0.000000000000000000, 0.000000000000000000 ) ) ;
#56013 = CYLINDRICAL_SURFACE ( 'NONE', #19994, 31.99999999999999289 ) ;
#56014 = ORIENTED_EDGE ( 'NONE', *, *, #57295, .F. ) ;
#56015 = DIRECTION ( 'NONE',  ( 1.000000000000000000, -7.571544473058805744E-15, -2.612289469705706870E-14 ) ) ;
#56016 = CARTESIAN_POINT ( 'NONE',  ( 92.69370383062501162, -208.6684592857803295, 79.42989583420047950 ) ) ;
#56017 = EDGE_CURVE ( 'NONE', #40400, #13774, #23767, .T. ) ;
#56018 = ORIENTED_EDGE ( 'NONE', *, *, #57221, .T. ) ;
#56019 = CARTESIAN_POINT ( 'NONE',  ( 92.69370383062501162, -208.6684592857803011, 85.30364583420048064 ) ) ;
#56020 = ORIENTED_EDGE ( 'NONE', *, *, #19501, .F. ) ;
#56021 = DIRECTION ( 'NONE',  ( 0.000000000000000000, 0.5877852522924742473, -0.8090169943749466741 ) ) ;
#56022 = ORIENTED_EDGE ( 'NONE', *, *, #58979, .T. ) ;
#56023 = CYLINDRICAL_SURFACE ( 'NONE', #70503, 16.00000000000000000 ) ;
#56024 = CIRCLE ( 'NONE', #23381, 31.99999999999999289 ) ;
#56025 = VERTEX_POINT ( 'NONE', #17620 ) ;
#56026 = DIRECTION ( 'NONE',  ( -0.6516173805718079581, 0.7585478161175704948, 0.000000000000000000 ) ) ;
#56027 = ORIENTED_EDGE ( 'NONE', *, *, #49134, .T. ) ;
#56028 = CARTESIAN_POINT ( 'NONE',  ( -97.65000000000006253, 88.47002178664756400, 77.35291666666665833 ) ) ;
#56029 = CARTESIAN_POINT ( 'NONE',  ( 92.35000000000002274, -208.4700217866474645, 88.75645833506762017 ) ) ;
#56030 = ADVANCED_FACE ( 'NONE', ( #40190 ), #5252, .T. ) ;
#56031 = ORIENTED_EDGE ( 'NONE', *, *, #11280, .F. ) ;
#56032 = DIRECTION ( 'NONE',  ( -1.000000000000000000, -0.000000000000000000, -0.000000000000000000 ) ) ;
#56033 = EDGE_CURVE ( 'NONE', #54897, #35415, #14777, .T. ) ;
#56034 = ORIENTED_EDGE ( 'NONE', *, *, #20866, .T. ) ;
#56035 =( BOUNDED_CURVE ( )  B_SPLINE_CURVE ( 2, ( #64492, #58474, #64133, #6254, #2118, #70857, #12607 ),
 .UNSPECIFIED., .F., .F. ) 
 B_SPLINE_CURVE_WITH_KNOTS ( ( 3, 2, 2, 3 ),
 ( 0.9166666666666662966, 0.9236111111111108274, 0.9305555555555551361, 0.9374999999999995559 ),
 .UNSPECIFIED. ) 
 CURVE ( )  GEOMETRIC_REPRESENTATION_ITEM ( )  RATIONAL_B_SPLINE_CURVE ( ( 1.000000000000006439, 0.8660254037844322683, 1.000000000000000000, 0.8660254037844387076, 1.000000000000000000, 0.8660254037844472563, 0.9999999999999914513 ) ) 
 REPRESENTATION_ITEM ( '' )  );
#56036 = CARTESIAN_POINT ( 'NONE',  ( 0.000000000000000000, 0.000000000000000000, -1.466666666666671670 ) ) ;
#56037 = EDGE_CURVE ( 'NONE', #19406, #588, #40024, .T. ) ;
#56038 = AXIS2_PLACEMENT_3D ( 'NONE', #33397, #49216, #72145 ) ;
#56039 = ORIENTED_EDGE ( 'NONE', *, *, #25412, .T. ) ;
#56040 = AXIS2_PLACEMENT_3D ( 'NONE', #22196, #31976, #27448 ) ;
#56041 = ORIENTED_EDGE ( 'NONE', *, *, #13521, .T. ) ;
#56042 = VERTEX_POINT ( 'NONE', #16889 ) ;
#56043 = CARTESIAN_POINT ( 'NONE',  ( 95.00000000000000000, -212.6630814284392557, 76.46656250086712703 ) ) ;
#56044 = CONTEXT_DEPENDENT_SHAPE_REPRESENTATION ( #46987, #63882 ) ;
#56045 = PLANE ( 'NONE',  #72606 ) ;
#56046 = VERTEX_POINT ( 'NONE', #74013 ) ;
#56047 = ORIENTED_EDGE ( 'NONE', *, *, #32420, .F. ) ;
#56048 = AXIS2_PLACEMENT_3D ( 'NONE', #30163, #64764, #30527 ) ;
#56049 = ORIENTED_EDGE ( 'NONE', *, *, #53498, .F. ) ;
#56050 = VECTOR ( 'NONE', #6617, 1000.000000000000000 ) ;
#56051 = CARTESIAN_POINT ( 'NONE',  ( 10.00000000000000000, 12.42422080174639021, 35.38097989696516521 ) ) ;
#56052 = B_SPLINE_CURVE_WITH_KNOTS ( 'NONE', 1,
 ( #45366, #61165 ),
 .UNSPECIFIED., .F., .F.,
 ( 2, 2 ),
 ( 0.000000000000000000, 1.000000000000000000 ),
 .UNSPECIFIED. ) ;
#56053 = CARTESIAN_POINT ( 'NONE',  ( -97.64999999999996305, -209.9999999999999716, 88.73000000000000398 ) ) ;
#56054 = CARTESIAN_POINT ( 'NONE',  ( -95.00000000000002842, 87.33691857156074434, 75.35531250086715715 ) ) ;
#56055 = ORIENTED_EDGE ( 'NONE', *, *, #7216, .T. ) ;
#56056 = CIRCLE ( 'NONE', #18804, 31.99999999999999289 ) ;
#56057 = CARTESIAN_POINT ( 'NONE',  ( 96.15314808468748708, 91.99731107132950569, 76.73114583420047552 ) ) ;
#56058 = ORIENTED_EDGE ( 'NONE', *, *, #24124, .F. ) ;
#56059 = LINE ( 'NONE', #44791, #5932 ) ;
#56060 = CARTESIAN_POINT ( 'NONE',  ( -93.84685191531248449, -208.0026889286704943, 89.43114583420047836 ) ) ;
#56061 = ORIENTED_EDGE ( 'NONE', *, *, #16385, .F. ) ;
#56062 = CARTESIAN_POINT ( 'NONE',  ( 2.991272306860053298, -4.046490820311139380, -0.5592653008974324269 ) ) ;
#56064 = VECTOR ( 'NONE', #47678, 1000.000000000000000 ) ;
#56063 = DIRECTION ( 'NONE',  ( -0.000000000000000000, -0.000000000000000000, 1.000000000000000000 ) ) ;
#56065 = DIRECTION ( 'NONE',  ( 2.603472992746261562E-14, 2.546204323184492723E-14, -1.000000000000000000 ) ) ;
#56066 = CARTESIAN_POINT ( 'NONE',  ( -92.69370383062498320, -211.3315407142195852, 81.01739583420048518 ) ) ;
#56067 = LINE ( 'NONE', #67722, #17054 ) ;
#56068 = DIRECTION ( 'NONE',  ( 1.000000000000000000, 0.000000000000000000, 0.000000000000000000 ) ) ;
#56069 = CARTESIAN_POINT ( 'NONE',  ( -94.99999999999997158, -206.9400435732949575, 84.12624999999999886 ) ) ;
#56070 = ORIENTED_EDGE ( 'NONE', *, *, #56373, .T. ) ;
#56071 = AXIS2_PLACEMENT_3D ( 'NONE', #39764, #68707, #47242 ) ;
#56072 = ORIENTED_EDGE ( 'NONE', *, *, #70260, .T. ) ;
#56073 = DIRECTION ( 'NONE',  ( 0.000000000000000000, 0.000000000000000000, -1.000000000000000000 ) ) ;
#56074 = CARTESIAN_POINT ( 'NONE',  ( 10.00000000000000000, 0.000000000000000000, 0.000000000000000000 ) ) ;
#56075 = AXIS2_PLACEMENT_3D ( 'NONE', #24594, #23132, #69716 ) ;
#56076 = LINE ( 'NONE', #33498, #45181 ) ;
#56077 = CARTESIAN_POINT ( 'NONE',  ( -95.00000000000002842, 92.66308142843932671, 81.22906250086715829 ) ) ;
#56078 = DIRECTION ( 'NONE',  ( 0.000000000000000000, 0.000000000000000000, 1.000000000000000000 ) ) ;
#56079 = DIRECTION ( 'NONE',  ( -0.3311129884571281101, -0.9435911131814402886, 0.000000000000000000 ) ) ;
#56080 = ORIENTED_EDGE ( 'NONE', *, *, #73676, .T. ) ;
#56081 = CARTESIAN_POINT ( 'NONE',  ( -7.499999999999969802, 73.00000000000001421, -204.9999999999999716 ) ) ;
#56082 = EDGE_CURVE ( 'NONE', #14793, #14764, #45472, .T. ) ;
#56083 = CARTESIAN_POINT ( 'NONE',  ( 10.00000000000000000, -26.02418014898260878, -70.52718814184285634 ) ) ;
#56084 = LINE ( 'NONE', #9475, #10553 ) ;
#56085 = CYLINDRICAL_SURFACE ( 'NONE', #7040, 32.00000000000000000 ) ;
#56086 = LINE ( 'NONE', #21873, #54973 ) ;
#56087 = DIRECTION ( 'NONE',  ( 0.000000000000000000, 0.000000000000000000, 1.000000000000000000 ) ) ;
#56088 = CARTESIAN_POINT ( 'NONE',  ( -97.30629616937497417, -208.6684592857803011, 78.31864583420050963 ) ) ;
#56089 = EDGE_CURVE ( 'NONE', #13197, #49491, #37608, .T. ) ;
#56090 = EDGE_CURVE ( 'NONE', #11281, #64952, #11192, .T. ) ;
#56091 = CYLINDRICAL_SURFACE ( 'NONE', #66505, 42.00000000000000000 ) ;
#56092 = APPLICATION_CONTEXT ( 'automotive_design' ) ;
#56093 = VERTEX_POINT ( 'NONE', #17254 ) ;
#56094 =( GEOMETRIC_REPRESENTATION_CONTEXT ( 3 ) GLOBAL_UNCERTAINTY_ASSIGNED_CONTEXT ( ( #2309 ) ) GLOBAL_UNIT_ASSIGNED_CONTEXT ( ( #36000, #7059, #65329 ) ) REPRESENTATION_CONTEXT ( 'NONE', 'WORKASPACE' ) );
#56095 = LINE ( 'NONE', #72992, #41905 ) ;
#56096 = CARTESIAN_POINT ( 'NONE',  ( -3.000000000000000000, -22.32062822937489344, 14.36278369418800160 ) ) ;
#56097 = CARTESIAN_POINT ( 'NONE',  ( 0.000000000000000000, 70.52718814184260054, 26.02418014898334420 ) ) ;
#56098 = CIRCLE ( 'NONE', #12888, 77.49899999999999523 ) ;
#56099 = ORIENTED_EDGE ( 'NONE', *, *, #6385, .T. ) ;
#56100 = EDGE_CURVE ( 'NONE', #59929, #9910, #8776, .T. ) ;
#56101 = CARTESIAN_POINT ( 'NONE',  ( -6.509281303079589520, -14.89695620656361008, 0.000000000000000000 ) ) ;
#56102 = CARTESIAN_POINT ( 'NONE',  ( -16.06301359042743115, -102.7814171781257357, -2.500000000000000000 ) ) ;
#56103 = AXIS2_PLACEMENT_3D ( 'NONE', #57187, #35364, #69203 ) ;
#56104 = VECTOR ( 'NONE', #15209, 1000.000000000000000 ) ;
#56105 = DIRECTION ( 'NONE',  ( 0.000000000000000000, 0.000000000000000000, -1.000000000000000000 ) ) ;
#56106 = ORIENTED_EDGE ( 'NONE', *, *, #16842, .T. ) ;
#56107 = CARTESIAN_POINT ( 'NONE',  ( 93.67499999999998295, 92.29496732002878900, 78.46416666666667084 ) ) ;
#56108 = CARTESIAN_POINT ( 'NONE',  ( -94.99999999999997158, -209.9999999999999716, 90.00000000000000000 ) ) ;
#56109 = ORIENTED_EDGE ( 'NONE', *, *, #63876, .T. ) ;
#56110 = CARTESIAN_POINT ( 'NONE',  ( 96.15314808468748708, -208.0026889286704943, 88.16114583420046813 ) ) ;
#56111 = CARTESIAN_POINT ( 'NONE',  ( 97.64999999999999147, -209.9999999999999716, 85.87249999999998806 ) ) ;
#56112 = EDGE_CURVE ( 'NONE', #10248, #52143, #64011, .T. ) ;
#56113 = ORIENTED_EDGE ( 'NONE', *, *, #16528, .T. ) ;
#56114 = CARTESIAN_POINT ( 'NONE',  ( 23.41451323550360186, -132.5004227906269989, 5.500000000000000000 ) ) ;
#56115 = EDGE_LOOP ( 'NONE', ( #58246, #54549, #4732, #49349 ) ) ;
#56116 = LINE ( 'NONE', #27536, #24996 ) ;
#56117 = VERTEX_POINT ( 'NONE', #40550 ) ;
#56118 = CARTESIAN_POINT ( 'NONE',  ( 0.000000000000000000, 30.84782396557217865, 21.32104025579125306 ) ) ;
#56119 = CIRCLE ( 'NONE', #60946, 37.49900000000000233 ) ;
#56120 = ORIENTED_EDGE ( 'NONE', *, *, #22848, .T. ) ;
#56121 = ORIENTED_EDGE ( 'NONE', *, *, #68432, .F. ) ;
#56122 = EDGE_LOOP ( 'NONE', ( #21135, #36700, #71027, #45353 ) ) ;
#56123 = PLANE ( 'NONE',  #37156 ) ;
#56124 = ADVANCED_FACE ( 'NONE', ( #63499 ), #50713, .F. ) ;
#56125 = EDGE_LOOP ( 'NONE', ( #52328, #8959, #6319, #17012, #10180, #3875, #18857, #17241, #47085, #31150, #26099, #46464, #26058, #46071, #34363, #20227, #72035, #13716, #37800, #73725, #14127, #7799, #25421, #23321, #24506, #6757, #10107, #42919, #70425, #67410, #27355, #12192, #67453, #35422, #36605, #29853, #7134, #65970, #69896, #39773, #39414, #71109, #66596, #50473, #73970, #34146, #24896, #62353, #3831, #39751, #18331, #6391, #12921, #19390, #17275, #2972, #34571, #29960, #47183, #2255, #23786, #40063, #1446, #14988, #30775, #73883, #68168, #36510, #2713, #31535, #2254, #15307, #28364, #57729, #8975, #39212, #37856, #64899, #2876, #12470, #8198, #43830, #73529, #19975, #63060, #11296, #63635, #28984, #65833, #70058, #27838, #43306, #14863, #66243, #61607, #53892, #61482, #34028, #24320, #42518, #39194, #42551, #5940, #51574, #68719, #32772, #69717, #14778, #33480, #11334, #46972, #33633, #17113, #60392, #69474, #39100, #57141, #49310, #47777, #52533, #40316, #8070, #35535, #3719, #52549, #32808, #41720, #40353, #4955, #48100, #16735, #59474, #7106, #70438, #25054, #2109, #53430, #26783, #71393, #6824, #53372, #5556, #39620, #69115, #15830, #69700, #55220, #23987, #44834, #71298, #6827, #57332, #10995, #54739, #43510, #39433, #28784, #40294, #69708, #4031, #65828, #31138, #43925, #29957, #39744, #25248, #4712, #59575, #43671, #52978, #7383, #29392, #5022, #59833, #32634, #13585, #29964, #55480, #34206, #154, #1531, #10626, #35309, #25514, #58947, #49478, #41857, #39052, #36453, #56943, #40983, #8482, #2846, #12577, #10280, #10163, #73514, #20791, #31092, #69709, #74291, #32487, #66111, #34901, #45317, #36712, #15040, #35154, #46555, #51255, #24297, #11185, #54201, #67694, #48310, #42216, #60298, #70814, #66474, #38752, #69544, #60224, #21527, #28457, #9439, #17825, #58282, #65195, #61594, #26556, #33924, #42530, #19389, #31623, #57962, #173, #54996, #1545, #70613, #18933, #52253, #1641, #71948, #58448, #38640, #39141, #69885, #45738, #73694, #15612, #39572, #35403, #13789, #21989, #31532, #54358, #69112, #17940, #65186, #63445, #44583, #39320, #18673, #17421, #36066, #9416, #7380, #42560, #48971, #43733, #69157, #15836, #62811, #59296, #72832, #71646, #68074, #3208, #48979, #47508, #68383, #8140, #45401, #22854, #35534, #21608, #29686, #36816, #66869, #13304, #8994, #38364, #66349, #1511, #53787, #71238, #22370, #52231, #25253, #27690, #50939, #4276, #30871, #16400, #57880, #13257, #60670, #63893, #28752, #4993, #998, #36366, #32565, #35361, #59941, #33933, #19419, #417, #31546, #44571, #47699, #43185, #59176, #46302, #47157 ) ) ;
#56126 = EDGE_CURVE ( 'NONE', #68048, #44533, #68014, .T. ) ;
#56127 = ORIENTED_EDGE ( 'NONE', *, *, #60928, .F. ) ;
#56128 = CARTESIAN_POINT ( 'NONE',  ( 96.15314808468748708, 91.99731107132950569, 78.15989583420049769 ) ) ;
#56129 = DIRECTION ( 'NONE',  ( -0.000000000000000000, -0.000000000000000000, 1.000000000000000000 ) ) ;
#56130 = CYLINDRICAL_SURFACE ( 'NONE', #14095, 82.00000000000000000 ) ;
#56131 = ORIENTED_EDGE ( 'NONE', *, *, #24802, .T. ) ;
#56132 = ORIENTED_EDGE ( 'NONE', *, *, #1342, .T. ) ;
#56133 = ORIENTED_EDGE ( 'NONE', *, *, #28608, .F. ) ;
#56134 = CARTESIAN_POINT ( 'NONE',  ( 97.30629616937498838, 88.66845928578037217, 87.36739583420047950 ) ) ;
#56135 = ORIENTED_EDGE ( 'NONE', *, *, #9693, .T. ) ;
#56136 = CARTESIAN_POINT ( 'NONE',  ( 96.15314808468748708, -208.0026889286704943, 86.25614583420048120 ) ) ;
#56137 = PRODUCT_CONTEXT ( 'NONE', #43597, 'mechanical' ) ;
#56138 = CARTESIAN_POINT ( 'NONE',  ( 10.00000000000000000, -28.89263327155693517, -71.91182617369219088 ) ) ;
#56139 = CARTESIAN_POINT ( 'NONE',  ( -95.00000000000002842, 93.05995642670504253, 77.22062500173429100 ) ) ;
#56140 = DIRECTION ( 'NONE',  ( -0.000000000000000000, -0.000000000000000000, -1.000000000000000000 ) ) ;
#56141 = DIRECTION ( 'NONE',  ( 0.000000000000000000, 0.000000000000000000, 1.000000000000000000 ) ) ;
#56142 = DIRECTION ( 'NONE',  ( -0.000000000000000000, -0.000000000000000000, 1.000000000000000000 ) ) ;
#56143 = LINE ( 'NONE', #67797, #19047 ) ;
#56144 = CARTESIAN_POINT ( 'NONE',  ( -97.30629616937497417, -208.6684592857803011, 87.68489583420047495 ) ) ;
#56145 = CARTESIAN_POINT ( 'NONE',  ( -92.69370383062502583, 91.33154071421968467, 86.36197916753383197 ) ) ;
#56146 = ORIENTED_EDGE ( 'NONE', *, *, #2355, .T. ) ;
#56148 = CARTESIAN_POINT ( 'NONE',  ( -92.69370383062504004, 90.00000000000004263, 88.05531250086713158 ) ) ;
#56147 = CARTESIAN_POINT ( 'NONE',  ( 94.99999999999998579, 87.33691857156068750, 87.89656250086713385 ) ) ;
#56149 = ORIENTED_EDGE ( 'NONE', *, *, #46944, .T. ) ;
#56150 = DIRECTION ( 'NONE',  ( -1.000000000000000000, 0.000000000000000000, 0.000000000000000000 ) ) ;
#56151 = AXIS2_PLACEMENT_3D ( 'NONE', #7115, #60842, #9324 ) ;
#56152 = CARTESIAN_POINT ( 'NONE',  ( -3.000000000000000000, 0.000000000000000000, 0.000000000000000000 ) ) ;
#56153 = CARTESIAN_POINT ( 'NONE',  ( 10.00000000000000000, 26.01480285779933510, -70.53064760720289428 ) ) ;
#56154 = DIRECTION ( 'NONE',  ( 0.000000000000000000, 0.000000000000000000, 1.000000000000000000 ) ) ;
#56155 = CARTESIAN_POINT ( 'NONE',  ( -97.30629616937497417, -208.6684592857803295, 88.95489583420048518 ) ) ;
#56156 = AXIS2_PLACEMENT_3D ( 'NONE', #38230, #71687, #32582 ) ;
#56157 = DIRECTION ( 'NONE',  ( 0.6516173805718079581, -0.7585478161175704948, 0.000000000000000000 ) ) ;
#56158 = DIRECTION ( 'NONE',  ( 0.000000000000000000, -0.07845909572785224328, 0.9969173337331274087 ) ) ;
#56159 = CARTESIAN_POINT ( 'NONE',  ( 11.99999999999999822, -0.8261519478436571973, 77.49459641780886443 ) ) ;
#56160 = ORIENTED_EDGE ( 'NONE', *, *, #73405, .T. ) ;
#56161 = ORIENTED_EDGE ( 'NONE', *, *, #21748, .F. ) ;
#56162 = AXIS2_PLACEMENT_3D ( 'NONE', #60631, #3133, #14744 ) ;
#56163 = CARTESIAN_POINT ( 'NONE',  ( -97.65000000000001990, 88.47002178664754979, 82.43291666666665662 ) ) ;
#56164 = CARTESIAN_POINT ( 'NONE',  ( 0.000000000000000000, 0.000000000000000000, 0.000000000000000000 ) ) ;
#56165 = CARTESIAN_POINT ( 'NONE',  ( 97.64999999999999147, -209.9999999999999716, 75.71250000000000568 ) ) ;
#56166 = DIRECTION ( 'NONE',  ( -0.000000000000000000, -0.000000000000000000, 1.000000000000000000 ) ) ;
#56167 = CYLINDRICAL_SURFACE ( 'NONE', #41139, 77.49899999999999523 ) ;
#56168 = FACE_OUTER_BOUND ( 'NONE', #53737, .T. ) ;
#56169 = EDGE_CURVE ( 'NONE', #63446, #6569, #55569, .T. ) ;
#56170 = CARTESIAN_POINT ( 'NONE',  ( -97.64999999980591383, 89.99998015720542810, 86.27002759516649633 ) ) ;
#56171 = CARTESIAN_POINT ( 'NONE',  ( 0.000000000000000000, 0.000000000000000000, 125.0000000000000000 ) ) ;
#56172 = ORIENTED_EDGE ( 'NONE', *, *, #72023, .F. ) ;
#56173 = CARTESIAN_POINT ( 'NONE',  ( -97.30629616937501680, 91.33154071421968467, 80.69989583420048973 ) ) ;
#56174 = ADVANCED_FACE ( 'NONE', ( #64975 ), #52942, .T. ) ;
#56175 = CARTESIAN_POINT ( 'NONE',  ( 97.64999322989690711, 88.47001787792670768, 82.72395806468932733 ) ) ;
#56176 = CARTESIAN_POINT ( 'NONE',  ( 5.000000000000000000, 63.97538442413498672, -51.29473840253155714 ) ) ;
#56177 = EDGE_CURVE ( 'NONE', #50675, #37724, #53676, .T. ) ;
#56178 = AXIS2_PLACEMENT_3D ( 'NONE', #63812, #6654, #64540 ) ;
#56179 = CARTESIAN_POINT ( 'NONE',  ( 0.000000000000000000, 0.000000000000000000, 0.000000000000000000 ) ) ;
#56180 = LINE ( 'NONE', #44541, #4501 ) ;
#56181 = DIRECTION ( 'NONE',  ( -1.000000000000000000, 0.000000000000000000, 0.000000000000000000 ) ) ;
#56182 = CARTESIAN_POINT ( 'NONE',  ( 2.500000000000000000, 16.00000000000000000, 0.000000000000000000 ) ) ;
#56183 =( NAMED_UNIT ( * ) SI_UNIT ( $, .STERADIAN. ) SOLID_ANGLE_UNIT ( ) );
#56184 = ADVANCED_FACE ( 'NONE', ( #35633 ), #65340, .T. ) ;
#56185 = CIRCLE ( 'NONE', #20151, 31.99999999999999289 ) ;
#56186 = VECTOR ( 'NONE', #71878, 1000.000000000000000 ) ;
#56187 = AXIS2_PLACEMENT_3D ( 'NONE', #72993, #44455, #57596 ) ;
#56188 = CARTESIAN_POINT ( 'NONE',  ( 97.30629616937498838, 88.66845928578035796, 81.81114583420048803 ) ) ;
#56189 = CARTESIAN_POINT ( 'NONE',  ( -94.99999999999997158, -207.3369185715606307, 78.84781250086714977 ) ) ;
#56190 = DIRECTION ( 'NONE',  ( 0.000000000000000000, 0.000000000000000000, -1.000000000000000000 ) ) ;
#56191 = ORIENTED_EDGE ( 'NONE', *, *, #72700, .F. ) ;
#56192 = EDGE_CURVE ( 'NONE', #27433, #68051, #58208, .T. ) ;
#56193 = CARTESIAN_POINT ( 'NONE',  ( 95.00000000000000000, -206.9400435732949575, 81.03062500173430749 ) ) ;
#56194 = DIRECTION ( 'NONE',  ( -1.000000000000000000, 0.000000000000000000, 0.000000000000000000 ) ) ;
#56195 = CARTESIAN_POINT ( 'NONE',  ( 92.35000000049295465, 89.99996796756887818, 85.63541623677173220 ) ) ;
#56196 = CARTESIAN_POINT ( 'NONE',  ( -96.15314808468751551, 88.00268892867056536, 79.74739583420048916 ) ) ;
#56197 = CARTESIAN_POINT ( 'NONE',  ( 95.00000000000000000, -207.3369185715606307, 81.22906250086715829 ) ) ;
#56198 = VERTEX_POINT ( 'NONE', #58961 ) ;
#56199 = CARTESIAN_POINT ( 'NONE',  ( 97.24889018994932144, 89.40965860031440116, 74.79348190356850523 ) ) ;
#56200 = ADVANCED_FACE ( 'NONE', ( #2217 ), #7450, .F. ) ;
#56201 = VERTEX_POINT ( 'NONE', #30365 ) ;
#56202 =( GEOMETRIC_REPRESENTATION_CONTEXT ( 3 ) GLOBAL_UNCERTAINTY_ASSIGNED_CONTEXT ( ( #71413 ) ) GLOBAL_UNIT_ASSIGNED_CONTEXT ( ( #30320, #34484, #23225 ) ) REPRESENTATION_CONTEXT ( 'NONE', 'WORKASPACE' ) );
#56203 = DIRECTION ( 'NONE',  ( 0.000000000000000000, 0.000000000000000000, 1.000000000000000000 ) ) ;
#56204 = EDGE_CURVE ( 'NONE', #39671, #44028, #59228, .T. ) ;
#56205 = ADVANCED_FACE ( 'NONE', ( #18348 ), #42401, .F. ) ;
#56206 = ORIENTED_EDGE ( 'NONE', *, *, #38301, .F. ) ;
#56207 = AXIS2_PLACEMENT_3D ( 'NONE', #9669, #32953, #31483 ) ;
#56208 = EDGE_CURVE ( 'NONE', #60292, #55893, #23175, .T. ) ;
#56209 = EDGE_CURVE ( 'NONE', #38913, #8717, #53310, .T. ) ;
#56210 = AXIS2_PLACEMENT_3D ( 'NONE', #61446, #32848, #72689 ) ;
#56211 = ORIENTED_EDGE ( 'NONE', *, *, #43558, .T. ) ;
#56212 = ORIENTED_EDGE ( 'NONE', *, *, #37252, .T. ) ;
#56213 = VECTOR ( 'NONE', #3873, 1000.000000000000000 ) ;
#56214 = ORIENTED_EDGE ( 'NONE', *, *, #47858, .F. ) ;
#56215 = CARTESIAN_POINT ( 'NONE',  ( 97.64999999999999147, -209.9999999999999716, 75.71250000000000568 ) ) ;
#56216 = ADVANCED_FACE ( 'NONE', ( #70573 ), #31106, .T. ) ;
#56217 = EDGE_LOOP ( 'NONE', ( #14164, #36489 ) ) ;
#56218 = CARTESIAN_POINT ( 'NONE',  ( -2.410829926157000802E-12, -120.0000000000000000, 127.5000000000000000 ) ) ;
#56219 = CYLINDRICAL_SURFACE ( 'NONE', #32842, 31.99999999999999289 ) ;
#56220 = CARTESIAN_POINT ( 'NONE',  ( 93.84685191531248449, 88.00268892867053694, 87.36739583420049371 ) ) ;
#56221 = CARTESIAN_POINT ( 'NONE',  ( 97.64999999999999147, 89.99999997928482287, 80.87187500099604165 ) ) ;
#56222 = CARTESIAN_POINT ( 'NONE',  ( 93.67500000000001137, -212.2949673200287179, 78.04083333333333883 ) ) ;
#56223 = ORIENTED_EDGE ( 'NONE', *, *, #35648, .F. ) ;
#56224 = EDGE_CURVE ( 'NONE', #74280, #16188, #7815, .T. ) ;
#56225 = ORIENTED_EDGE ( 'NONE', *, *, #51618, .T. ) ;
#56226 = ORIENTED_EDGE ( 'NONE', *, *, #17389, .T. ) ;
#56227 = ORIENTED_EDGE ( 'NONE', *, *, #32810, .T. ) ;
#56228 = CARTESIAN_POINT ( 'NONE',  ( 97.64999999999999147, -209.9999999999999716, 89.04749999999999943 ) ) ;
#56229 = DIRECTION ( 'NONE',  ( 0.000000000000000000, 0.1564344650402311743, -0.9876883405951376593 ) ) ;
#56230 = LINE ( 'NONE', #24604, #62687 ) ;
#56231 = CIRCLE ( 'NONE', #65835, 31.99999999999998934 ) ;
#56232 = FACE_OUTER_BOUND ( 'NONE', #45159, .T. ) ;
#56233 = DIRECTION ( 'NONE',  ( 0.000000000000000000, 0.000000000000000000, 1.000000000000000000 ) ) ;
#56234 = CIRCLE ( 'NONE', #9375, 31.99999999999999289 ) ;
#56235 = DIRECTION ( 'NONE',  ( 0.000000000000000000, -0.000000000000000000, -1.000000000000000000 ) ) ;
#56236 = VECTOR ( 'NONE', #46292, 1000.000000000000000 ) ;
#56237 = VERTEX_POINT ( 'NONE', #70954 ) ;
#56238 = CARTESIAN_POINT ( 'NONE',  ( -92.34999999999999432, -208.4700217866474645, 81.55979166840097605 ) ) ;
#56239 = ORIENTED_EDGE ( 'NONE', *, *, #21732, .T. ) ;
#56240 = DIRECTION ( 'NONE',  ( 0.000000000000000000, 0.000000000000000000, 1.000000000000000000 ) ) ;
#56241 = ORIENTED_EDGE ( 'NONE', *, *, #39247, .T. ) ;
#56243 = CARTESIAN_POINT ( 'NONE',  ( -92.35000000000003695, 90.00000000000004263, 82.77687500173431090 ) ) ;
#56242 = CARTESIAN_POINT ( 'NONE',  ( 93.67499999999999716, 87.70503267997126784, 81.29520833506762756 ) ) ;
#56244 = STYLED_ITEM ( 'NONE', ( #20309 ), #36766 ) ;
#56245 = ORIENTED_EDGE ( 'NONE', *, *, #37157, .T. ) ;
#56246 = CARTESIAN_POINT ( 'NONE',  ( 94.99999999999998579, 92.66308142843935514, 83.92781250086716227 ) ) ;
#56247 = LINE ( 'NONE', #51333, #40617 ) ;
#56248 = DIRECTION ( 'NONE',  ( -1.000000000000000000, 0.000000000000000000, 0.000000000000000000 ) ) ;
#56249 = CARTESIAN_POINT ( 'NONE',  ( 11.99999999999999822, 0.000000000000000000, 0.000000000000000000 ) ) ;
#56250 = DIRECTION ( 'NONE',  ( 0.000000000000000000, 0.9238795325112877377, -0.3826834323650873948 ) ) ;
#56251 = DIRECTION ( 'NONE',  ( 0.000000000000000000, 0.000000000000000000, 1.000000000000000000 ) ) ;
#56252 = ORIENTED_EDGE ( 'NONE', *, *, #64698, .F. ) ;
#56253 = CARTESIAN_POINT ( 'NONE',  ( 96.32499999999998863, -207.7050326799711968, 77.72333333333332916 ) ) ;
#56254 = CARTESIAN_POINT ( 'NONE',  ( -23.42219527698293646, -121.9106984081423803, 2.500000000000000000 ) ) ;
#56255 = DIRECTION ( 'NONE',  ( 0.000000000000000000, 0.3090169943749482839, -0.9510565162951533091 ) ) ;
#56256 = VERTEX_POINT ( 'NONE', #70210 ) ;
#56257 = ORIENTED_EDGE ( 'NONE', *, *, #38136, .T. ) ;
#56258 = DIRECTION ( 'NONE',  ( 0.000000000000000000, 0.9969173337331282969, -0.07845909572784179331 ) ) ;
#56259 = CARTESIAN_POINT ( 'NONE',  ( 2.949999999999999734, 0.000000000000000000, 0.000000000000000000 ) ) ;
#56260 = DIRECTION ( 'NONE',  ( -1.000000000000000000, -0.000000000000000000, -0.000000000000000000 ) ) ;
#56261 =( BOUNDED_CURVE ( )  B_SPLINE_CURVE ( 2, ( #64017, #63653, #35064, #23418, #33950, #69643, #165 ),
 .UNSPECIFIED., .F., .F. ) 
 B_SPLINE_CURVE_WITH_KNOTS ( ( 3, 2, 2, 3 ),
 ( 0.6875000000000000000, 0.6944444444444443088, 0.7013888888888887285, 0.7083333333333331483 ),
 .UNSPECIFIED. ) 
 CURVE ( )  GEOMETRIC_REPRESENTATION_ITEM ( )  RATIONAL_B_SPLINE_CURVE ( ( 1.000000000000000000, 0.8660254037844387076, 1.000000000000000000, 0.8660254037844387076, 1.000000000000000000, 0.8660254037844430375, 0.9999999999999956701 ) ) 
 REPRESENTATION_ITEM ( '' )  );
#56262 = CARTESIAN_POINT ( 'NONE',  ( -96.15314808468747287, -208.0026889286704943, 82.71072916753381321 ) ) ;
#56263 = EDGE_LOOP ( 'NONE', ( #7941, #49207, #5748, #53724 ) ) ;
#56264 = DIRECTION ( 'NONE',  ( 0.000000000000000000, 0.000000000000000000, 1.000000000000000000 ) ) ;
#56265 = ORIENTED_EDGE ( 'NONE', *, *, #14582, .T. ) ;
#56266 = VECTOR ( 'NONE', #1306, 1000.000000000000000 ) ;
#56267 = AXIS2_PLACEMENT_3D ( 'NONE', #51179, #68110, #67741 ) ;
#56268 = EDGE_CURVE ( 'NONE', #40273, #8991, #46937, .T. ) ;
#56269 = CARTESIAN_POINT ( 'NONE',  ( -7.469491406282094736, 4.756046723998911929, 42.00000000000001421 ) ) ;
#56270 = CARTESIAN_POINT ( 'NONE',  ( 92.34999999999999432, 90.00000000000002842, 90.00000000000000000 ) ) ;
#56271 = AXIS2_PLACEMENT_3D ( 'NONE', #11321, #34252, #17705 ) ;
#56272 = ADVANCED_FACE ( 'NONE', ( #36752 ), #35281, .T. ) ;
#56273 = DIRECTION ( 'NONE',  ( -0.8571673007021122226, 1.049727191138618572E-16, 0.5150380749100542666 ) ) ;
#56274 = CARTESIAN_POINT ( 'NONE',  ( -11.99999999999999645, 1.702802944658382841E-15, 13.90444123027096879 ) ) ;
#56275 = CIRCLE ( 'NONE', #27429, 15.80000000000028315 ) ;
#56276 = FACE_OUTER_BOUND ( 'NONE', #13647, .T. ) ;
#56277 = CARTESIAN_POINT ( 'NONE',  ( 0.000000000000000000, 0.000000000000000000, -1.466666666666671670 ) ) ;
#56278 = DIRECTION ( 'NONE',  ( 1.000000000000000000, 0.000000000000000000, 0.000000000000000000 ) ) ;
#56279 = CYLINDRICAL_SURFACE ( 'NONE', #59278, 23.50000000000000355 ) ;
#56280 = ADVANCED_FACE ( 'NONE', ( #12705 ), #18716, .T. ) ;
#56282 = EDGE_CURVE ( 'NONE', #19205, #3369, #38782, .T. ) ;
#56281 = CARTESIAN_POINT ( 'NONE',  ( 10.00000000000000000, 6.736453364084091788, -36.88895765772625879 ) ) ;
#56283 = DIRECTION ( 'NONE',  ( 0.000000000000000000, 0.6691306063588579045, -0.7431448254773945772 ) ) ;
#56284 = CARTESIAN_POINT ( 'NONE',  ( 97.65000000000009095, -211.5299782133523649, 83.27958333333332064 ) ) ;
#56285 = DIRECTION ( 'NONE',  ( -1.000000000000000000, 0.000000000000000000, -0.000000000000000000 ) ) ;
#56286 = DIRECTION ( 'NONE',  ( 0.000000000000000000, 0.000000000000000000, 1.000000000000000000 ) ) ;
#56287 = AXIS2_PLACEMENT_3D ( 'NONE', #62596, #11076, #33998 ) ;
#56288 = VERTEX_POINT ( 'NONE', #4415 ) ;
#56289 = CARTESIAN_POINT ( 'NONE',  ( -96.15314808468752972, 91.99731107132950569, 80.01197916753380923 ) ) ;
#56290 = AXIS2_PLACEMENT_3D ( 'NONE', #30044, #6756, #46985 ) ;
#56291 = AXIS2_PLACEMENT_3D ( 'NONE', #37990, #32703, #15052 ) ;
#56292 = EDGE_CURVE ( 'NONE', #18301, #16255, #67595, .T. ) ;
#56293 = CIRCLE ( 'NONE', #2284, 77.49899999999999523 ) ;
#56294 = CARTESIAN_POINT ( 'NONE',  ( 92.69370383062501162, -209.9999999999999716, 89.64281250086713726 ) ) ;
#56295 = ORIENTED_EDGE ( 'NONE', *, *, #7290, .F. ) ;
#56296 = VECTOR ( 'NONE', #15611, 1000.000000000000000 ) ;
#56297 = LINE ( 'NONE', #27715, #47474 ) ;
#56298 = DIRECTION ( 'NONE',  ( 0.000000000000000000, -0.6691306063588579045, 0.7431448254773945772 ) ) ;
#56299 = CARTESIAN_POINT ( 'NONE',  ( 11.99999999999999822, 0.000000000000000000, 0.000000000000000000 ) ) ;
#56300 = CARTESIAN_POINT ( 'NONE',  ( -92.35000000000003695, 90.00000000000004263, 90.00000000000000000 ) ) ;
#56301 = EDGE_CURVE ( 'NONE', #45965, #39865, #43501, .T. ) ;
#56302 = EDGE_CURVE ( 'NONE', #49934, #16205, #73590, .T. ) ;
#56303 = CARTESIAN_POINT ( 'NONE',  ( 97.30629616937498838, -208.6684592857803011, 76.20197916753382117 ) ) ;
#56304 = ORIENTED_EDGE ( 'NONE', *, *, #33689, .T. ) ;
#56305 = EDGE_LOOP ( 'NONE', ( #16763, #32325, #8107, #39327 ) ) ;
#56306 = VECTOR ( 'NONE', #38763, 1000.000000000000000 ) ;
#56307 = FACE_OUTER_BOUND ( 'NONE', #56408, .T. ) ;
#56308 = DIRECTION ( 'NONE',  ( -1.000000000000000000, 0.000000000000000000, 0.000000000000000000 ) ) ;
#56309 = LINE ( 'NONE', #15710, #66458 ) ;
#56310 = DIRECTION ( 'NONE',  ( -1.000000000000000000, 0.000000000000000000, 0.000000000000000000 ) ) ;
#56311 = VECTOR ( 'NONE', #12201, 1000.000000000000000 ) ;
#56312 = DIRECTION ( 'NONE',  ( -0.000000000000000000, -0.000000000000000000, -1.000000000000000000 ) ) ;
#56313 = CARTESIAN_POINT ( 'NONE',  ( 97.64999999999997726, -208.4700217866474645, 88.46541666666665549 ) ) ;
#56314 = AXIS2_PLACEMENT_3D ( 'NONE', #24587, #17834, #24233 ) ;
#56315 = AXIS2_PLACEMENT_3D ( 'NONE', #8661, #37609, #42141 ) ;
#56316 = EDGE_LOOP ( 'NONE', ( #8783, #31338, #13040, #59456 ) ) ;
#56317 = CARTESIAN_POINT ( 'NONE',  ( -92.34999999999996589, -208.4700217866474645, 87.83041666666669300 ) ) ;
#56318 = VERTEX_POINT ( 'NONE', #20939 ) ;
#56319 = ORIENTED_EDGE ( 'NONE', *, *, #41866, .T. ) ;
#56320 = DIRECTION ( 'NONE',  ( 1.000000000000000000, 0.000000000000000000, -0.000000000000000000 ) ) ;
#56321 = CIRCLE ( 'NONE', #13100, 37.49900000000000233 ) ;
#56322 = DIRECTION ( 'NONE',  ( -1.000000000000000000, 0.000000000000000000, 0.000000000000000000 ) ) ;
#56323 = CIRCLE ( 'NONE', #51543, 42.00000000000000000 ) ;
#56324 = ORIENTED_EDGE ( 'NONE', *, *, #62784, .F. ) ;
#56325 = CARTESIAN_POINT ( 'NONE',  ( 97.64999999999997726, 88.47002178664752137, 87.72458333333332803 ) ) ;
#56326 = CARTESIAN_POINT ( 'NONE',  ( 93.67500000000001137, -207.7050326799711968, 79.17854166840096752 ) ) ;
#56327 = CARTESIAN_POINT ( 'NONE',  ( 96.32499999999997442, 92.29496732002878900, 81.53333333333333144 ) ) ;
#56328 = VERTEX_POINT ( 'NONE', #54417 ) ;
#56329 = CARTESIAN_POINT ( 'NONE',  ( 5.999999999999999112, 51.29473840253223216, 63.97538442413444670 ) ) ;
#56330 = ORIENTED_EDGE ( 'NONE', *, *, #11315, .F. ) ;
#56331 = DIRECTION ( 'NONE',  ( 1.000000000000000000, 0.000000000000000000, -0.000000000000000000 ) ) ;
#56332 = ORIENTED_EDGE ( 'NONE', *, *, #45150, .T. ) ;
#56333 = DIRECTION ( 'NONE',  ( -1.000000000000000000, -0.000000000000000000, 0.000000000000000000 ) ) ;
#56334 = CARTESIAN_POINT ( 'NONE',  ( -95.00000000000002842, 92.66308142843932671, 83.29281250086715715 ) ) ;
#56335 = CARTESIAN_POINT ( 'NONE',  ( 94.99999999999998579, 92.66308142843935514, 79.95906250086713385 ) ) ;
#56336 = ORIENTED_EDGE ( 'NONE', *, *, #44243, .F. ) ;
#56337 = CARTESIAN_POINT ( 'NONE',  ( 10.00000000000000000, 46.21855187248719687, -62.20884554313968806 ) ) ;
#56338 = CIRCLE ( 'NONE', #52737, 77.49900000000002365 ) ;
#56339 = DIRECTION ( 'NONE',  ( 1.000000000000000000, 0.000000000000000000, 0.000000000000000000 ) ) ;
#56340 = AXIS2_PLACEMENT_3D ( 'NONE', #53382, #7883, #1919 ) ;
#56341 = CARTESIAN_POINT ( 'NONE',  ( 97.64999999964362587, 89.99995654222556141, 89.12687334326064104 ) ) ;
#56342 = DIRECTION ( 'NONE',  ( 0.000000000000000000, 0.000000000000000000, 1.000000000000000000 ) ) ;
#56343 = VERTEX_POINT ( 'NONE', #43893 ) ;
#56344 = CARTESIAN_POINT ( 'NONE',  ( -96.32499999999996021, -212.2949673200287179, 86.29583333333333428 ) ) ;
#56345 = AXIS2_PLACEMENT_3D ( 'NONE', #25957, #15795, #60912 ) ;
#56347 = CARTESIAN_POINT ( 'NONE',  ( -94.99999999999997158, -207.3369185715606307, 77.41906250086714181 ) ) ;
#56346 = AXIS2_PLACEMENT_3D ( 'NONE', #14911, #60423, #3293 ) ;
#56348 = VERTEX_POINT ( 'NONE', #15299 ) ;
#56349 = EDGE_LOOP ( 'NONE', ( #58804, #27553, #42611, #61615 ) ) ;
#56350 = CARTESIAN_POINT ( 'NONE',  ( 0.000000000000000000, 0.000000000000000000, 0.000000000000000000 ) ) ;
#56351 = VECTOR ( 'NONE', #30399, 1000.000000000000000 ) ;
#56352 = CIRCLE ( 'NONE', #19139, 82.00000000000000000 ) ;
#56353 = ORIENTED_EDGE ( 'NONE', *, *, #58583, .F. ) ;
#56354 = CYLINDRICAL_SURFACE ( 'NONE', #34758, 15.99999999999999645 ) ;
#56355 = AXIS2_PLACEMENT_3D ( 'NONE', #63801, #13007, #53606 ) ;
#56356 = CARTESIAN_POINT ( 'NONE',  ( 0.000000000000000000, 0.000000000000000000, 0.000000000000000000 ) ) ;
#56357 = VERTEX_POINT ( 'NONE', #8926 ) ;
#56358 = CARTESIAN_POINT ( 'NONE',  ( -97.30629616937495996, -209.9999999999999716, 75.03781250086713328 ) ) ;
#56359 = ORIENTED_EDGE ( 'NONE', *, *, #54807, .T. ) ;
#56360 = CARTESIAN_POINT ( 'NONE',  ( 93.67499999999998295, 92.29496732002878900, 88.70354166840097321 ) ) ;
#56361 = DIRECTION ( 'NONE',  ( -1.000000000000000000, -0.000000000000000000, -0.000000000000000000 ) ) ;
#56362 = PLANE ( 'NONE',  #69353 ) ;
#56363 = CARTESIAN_POINT ( 'NONE',  ( -8.000000000000007105, -1.142349898368590025E-14, -6.370018489464426943E-15 ) ) ;
#56364 = EDGE_CURVE ( 'NONE', #26612, #1727, #455, .T. ) ;
#56365 = FACE_OUTER_BOUND ( 'NONE', #14584, .T. ) ;
#56366 = EDGE_CURVE ( 'NONE', #40438, #18610, #49710, .T. ) ;
#56367 = CARTESIAN_POINT ( 'NONE',  ( -3.000000000000000000, 24.81905959214261514, 9.408202855044825341 ) ) ;
#56368 = CARTESIAN_POINT ( 'NONE',  ( 94.99999999999998579, 87.33691857156068750, 84.08656250086714579 ) ) ;
#56369 = FACE_OUTER_BOUND ( 'NONE', #42161, .T. ) ;
#56370 = CARTESIAN_POINT ( 'NONE',  ( -1.029419772574582836, -121.0910063848724718, -2.500000000000000000 ) ) ;
#56371 = CARTESIAN_POINT ( 'NONE',  ( -7.468086116107294004, -12.33868914344945189, 0.000000000000000000 ) ) ;
#56373 = EDGE_CURVE ( 'NONE', #52503, #13202, #55629, .T. ) ;
#56372 = CARTESIAN_POINT ( 'NONE',  ( 0.000000000000000000, -59.03961581697432592, 46.53671651293927880 ) ) ;
#56374 = DIRECTION ( 'NONE',  ( 0.000000000000000000, 0.000000000000000000, -1.000000000000000000 ) ) ;
#56375 = CARTESIAN_POINT ( 'NONE',  ( -97.64999999969894873, 90.00002455906438570, 87.53856274002211535 ) ) ;
#56376 = CARTESIAN_POINT ( 'NONE',  ( 2.459674775249762302, -2.093084008641303565E-13, -20.20000000000035456 ) ) ;
#56377 = EDGE_CURVE ( 'NONE', #33442, #71294, #56871, .T. ) ;
#56378 = AXIS2_PLACEMENT_3D ( 'NONE', #40717, #57269, #23789 ) ;
#56379 = CARTESIAN_POINT ( 'NONE',  ( 93.67499999999999716, 87.70503267997126784, 78.67583333333332973 ) ) ;
#56380 = VECTOR ( 'NONE', #49722, 1000.000000000000000 ) ;
#56381 = VECTOR ( 'NONE', #43420, 1000.000000000000000 ) ;
#56382 = DIRECTION ( 'NONE',  ( -1.000000000000000000, -0.000000000000000000, 0.000000000000000000 ) ) ;
#56383 = CIRCLE ( 'NONE', #64807, 82.00000000000000000 ) ;
#56384 = CYLINDRICAL_SURFACE ( 'NONE', #55675, 2.649999999999999467 ) ;
#56385 = DIRECTION ( 'NONE',  ( -0.000000000000000000, -0.000000000000000000, -1.000000000000000000 ) ) ;
#56386 = CARTESIAN_POINT ( 'NONE',  ( -96.32499999999996021, -207.7050326799711968, 83.54416666666666913 ) ) ;
#56387 = ADVANCED_FACE ( 'NONE', ( #14560 ), #38236, .T. ) ;
#56388 = DIRECTION ( 'NONE',  ( -1.000000000000000000, -0.000000000000000000, -0.000000000000000000 ) ) ;
#56389 = ADVANCED_FACE ( 'NONE', ( #55156 ), #61552, .F. ) ;
#56390 = FACE_OUTER_BOUND ( 'NONE', #24893, .T. ) ;
#56391 = DIRECTION ( 'NONE',  ( -1.000000000000000000, -0.000000000000000000, -0.000000000000000000 ) ) ;
#56392 = SURFACE_SIDE_STYLE ('',( #21789 ) ) ;
#56393 = CARTESIAN_POINT ( 'NONE',  ( 10.00000000000000000, 12.93880638057314059, 76.41127070299278046 ) ) ;
#56394 = VECTOR ( 'NONE', #62758, 1000.000000000000000 ) ;
#56395 = CIRCLE ( 'NONE', #15541, 31.99999999999998224 ) ;
#56396 = EDGE_CURVE ( 'NONE', #8203, #29480, #68889, .T. ) ;
#56397 = ADVANCED_FACE ( 'NONE', ( #16422 ), #22436, .F. ) ;
#56398 = AXIS2_PLACEMENT_3D ( 'NONE', #35170, #41186, #64127 ) ;
#56399 = CARTESIAN_POINT ( 'NONE',  ( 95.00000000000000000, -212.6630814284392557, 87.42031250086715488 ) ) ;
#56400 = ORIENTED_EDGE ( 'NONE', *, *, #67826, .F. ) ;
#56401 = VECTOR ( 'NONE', #43753, 1000.000000000000000 ) ;
#56402 = ORIENTED_EDGE ( 'NONE', *, *, #72110, .F. ) ;
#56403 = AXIS2_PLACEMENT_3D ( 'NONE', #5177, #46128, #17182 ) ;
#56404 = SURFACE_STYLE_FILL_AREA ( #57509 ) ;
#56405 = ORIENTED_EDGE ( 'NONE', *, *, #53911, .F. ) ;
#56406 = DIRECTION ( 'NONE',  ( 0.000000000000000000, 0.000000000000000000, 1.000000000000000000 ) ) ;
#56407 = CARTESIAN_POINT ( 'NONE',  ( 95.00000000000000000, -207.3369185715606307, 76.78406250086712248 ) ) ;
#56408 = EDGE_LOOP ( 'NONE', ( #46510, #23837, #21633, #8632 ) ) ;
#56409 = CARTESIAN_POINT ( 'NONE',  ( 92.69370383062501162, -209.9999999999999716, 82.81656250086714977 ) ) ;
#56410 = ORIENTED_EDGE ( 'NONE', *, *, #23770, .T. ) ;
#56411 = CARTESIAN_POINT ( 'NONE',  ( 1.692257445284848207E-12, 0.000000000000000000, -65.00000000000000000 ) ) ;
#56412 = ORIENTED_EDGE ( 'NONE', *, *, #34555, .T. ) ;
#56413 = CARTESIAN_POINT ( 'NONE',  ( -93.33922900947484891, 88.39973697852397549, 74.80065534806809069 ) ) ;
#56414 = CARTESIAN_POINT ( 'NONE',  ( 15.00000000000000000, 23.49999999999999645, -1.500000000000003997 ) ) ;
#56415 = ORIENTED_EDGE ( 'NONE', *, *, #16144, .T. ) ;
#56416 = CARTESIAN_POINT ( 'NONE',  ( 96.32499999999998863, -212.2949673200287179, 76.95604166840095672 ) ) ;
#56417 = CARTESIAN_POINT ( 'NONE',  ( 10.00000000000000000, -63.97538442413389248, -51.29473840253292138 ) ) ;
#56418 = ORIENTED_EDGE ( 'NONE', *, *, #45856, .F. ) ;
#56419 = DIRECTION ( 'NONE',  ( -1.000000000000000000, -0.000000000000000000, -0.000000000000000000 ) ) ;
#56420 = EDGE_LOOP ( 'NONE', ( #31706, #24995, #41892 ) ) ;
#56421 = DIRECTION ( 'NONE',  ( 1.000000000000000000, 0.000000000000000000, -0.000000000000000000 ) ) ;
#56422 = AXIS2_PLACEMENT_3D ( 'NONE', #54489, #60153, #2292 ) ;
#56423 = VERTEX_POINT ( 'NONE', #40459 ) ;
#56424 = VECTOR ( 'NONE', #3510, 1000.000000000000000 ) ;
#56425 = ORIENTED_EDGE ( 'NONE', *, *, #23878, .T. ) ;
#56426 = ORIENTED_EDGE ( 'NONE', *, *, #9485, .F. ) ;
#56427 = CARTESIAN_POINT ( 'NONE',  ( 97.30629616937498838, -209.9999999999999716, 75.99031250086714806 ) ) ;
#56428 = DIRECTION ( 'NONE',  ( 0.000000000000000000, 0.4999999999999920064, 0.8660254037844432595 ) ) ;
#56429 = ORIENTED_EDGE ( 'NONE', *, *, #40841, .F. ) ;
#56430 = ORIENTED_EDGE ( 'NONE', *, *, #18608, .F. ) ;
#56431 = CIRCLE ( 'NONE', #24021, 0.2500000000000002220 ) ;
#56433 = EDGE_CURVE ( 'NONE', #12910, #7033, #16023, .T. ) ;
#56432 = ORIENTED_EDGE ( 'NONE', *, *, #39737, .T. ) ;
#56434 = CARTESIAN_POINT ( 'NONE',  ( 95.00000000000000000, -209.9999999999999716, 90.00000000000000000 ) ) ;
#56435 = DIRECTION ( 'NONE',  ( -1.000000000000000000, 0.000000000000000000, -0.000000000000000000 ) ) ;
#56436 = EDGE_CURVE ( 'NONE', #44823, #20714, #39358, .T. ) ;
#56437 = CARTESIAN_POINT ( 'NONE',  ( -95.00000000000002842, 92.66308142843932671, 76.30781250086715772 ) ) ;
#56438 = VERTEX_POINT ( 'NONE', #45003 ) ;
#56439 = CARTESIAN_POINT ( 'NONE',  ( 15.00000000000000000, 0.000000000000000000, 0.000000000000000000 ) ) ;
#56440 = ADVANCED_FACE ( 'NONE', ( #16799 ), #11876, .F. ) ;
#56441 = ORIENTED_EDGE ( 'NONE', *, *, #53883, .T. ) ;
#56442 = CARTESIAN_POINT ( 'NONE',  ( 11.99999999999999822, -60.67117009219096957, -55.16347631943106933 ) ) ;
#56443 = CARTESIAN_POINT ( 'NONE',  ( -93.84685191531247028, -211.9973110713294489, 86.04447916753380809 ) ) ;
#56444 = ORIENTED_EDGE ( 'NONE', *, *, #457, .T. ) ;
#56445 = CARTESIAN_POINT ( 'NONE',  ( 96.92442009029420547, -211.8218417373832096, 75.00000000000001421 ) ) ;
#56446 = AXIS2_PLACEMENT_3D ( 'NONE', #5173, #51017, #34456 ) ;
#56447 = CARTESIAN_POINT ( 'NONE',  ( 6.000000000000000000, 76.69515212746057387, -29.01471420065479379 ) ) ;
#56448 = DIRECTION ( 'NONE',  ( 0.000000000000000000, 0.7071067811865487940, -0.7071067811865463515 ) ) ;
#56449 = CARTESIAN_POINT ( 'NONE',  ( -97.30629616937497417, -211.3315407142195852, 79.53572916753380184 ) ) ;
#56450 = ADVANCED_FACE ( 'NONE', ( #34827 ), #4028, .F. ) ;
#56451 = AXIS2_PLACEMENT_3D ( 'NONE', #41277, #19069, #70193 ) ;
#56452 = CARTESIAN_POINT ( 'NONE',  ( 11.99999999999999822, 0.000000000000000000, 0.000000000000000000 ) ) ;
#56453 = DIRECTION ( 'NONE',  ( 1.000000000000000000, 0.000000000000000000, -0.000000000000000000 ) ) ;
#56454 = VECTOR ( 'NONE', #25844, 1000.000000000000000 ) ;
#56455 = CARTESIAN_POINT ( 'NONE',  ( 11.99999999999999822, 0.000000000000000000, 0.000000000000000000 ) ) ;
#56456 = AXIS2_PLACEMENT_3D ( 'NONE', #5766, #34318, #28672 ) ;
#56457 = AXIS2_PLACEMENT_3D ( 'NONE', #27952, #68568, #16683 ) ;
#56459 = ORIENTED_EDGE ( 'NONE', *, *, #70774, .T. ) ;
#56458 = EDGE_CURVE ( 'NONE', #46172, #19845, #62296, .T. ) ;
#56460 = CARTESIAN_POINT ( 'NONE',  ( 0.000000000000000000, 0.000000000000000000, 125.0000000000000000 ) ) ;
#56461 = AXIS2_PLACEMENT_3D ( 'NONE', #69263, #64736, #59098 ) ;
#56462 = CARTESIAN_POINT ( 'NONE',  ( 10.00000000000000000, 0.000000000000000000, 0.000000000000000000 ) ) ;
#56463 = DIRECTION ( 'NONE',  ( -0.000000000000000000, 0.7431448254773946882, -0.6691306063588577935 ) ) ;
#56464 = CARTESIAN_POINT ( 'NONE',  ( -95.00000000000002842, 92.66308142843932671, 80.59406250086715318 ) ) ;
#56465 = CARTESIAN_POINT ( 'NONE',  ( 0.000000000000000000, 0.000000000000000000, 0.000000000000000000 ) ) ;
#56466 = CARTESIAN_POINT ( 'NONE',  ( 5.000000000000000000, -39.04073710021332744, -15.48615015657624205 ) ) ;
#56467 = EDGE_CURVE ( 'NONE', #65091, #16429, #5999, .T. ) ;
#56468 = VERTEX_POINT ( 'NONE', #51363 ) ;
#56469 = CARTESIAN_POINT ( 'NONE',  ( -0.0004442498525516064278, 0.001194404164626844313, -64.00000000000000000 ) ) ;
#56470 = AXIS2_PLACEMENT_3D ( 'NONE', #53323, #47320, #70590 ) ;
#56471 = CARTESIAN_POINT ( 'NONE',  ( -97.30629616937495996, -209.9999999999999716, 89.64281250086713726 ) ) ;
#56472 = DIRECTION ( 'NONE',  ( 0.000000000000000000, 0.000000000000000000, 1.000000000000000000 ) ) ;
#56473 = DIRECTION ( 'NONE',  ( -1.000000000000000000, 0.000000000000000000, -0.000000000000000000 ) ) ;
#56474 = CARTESIAN_POINT ( 'NONE',  ( -0.9154378789997292820, 5.244974386029388036, -1.156968425231163167 ) ) ;
#56475 = CARTESIAN_POINT ( 'NONE',  ( 92.35000000000002274, -210.0000343786552719, 88.80937619077336365 ) ) ;
#56476 = CARTESIAN_POINT ( 'NONE',  ( -94.99999999999997158, -212.6630814284392557, 78.53031250086715431 ) ) ;
#56477 = EDGE_CURVE ( 'NONE', #38312, #70074, #41247, .T. ) ;
#56478 = LINE ( 'NONE', #68497, #41667 ) ;
#56479 = EDGE_CURVE ( 'NONE', #45901, #43278, #34077, .T. ) ;
#56480 = ORIENTED_EDGE ( 'NONE', *, *, #30466, .T. ) ;
#56481 = DIRECTION ( 'NONE',  ( 0.000000000000000000, 0.000000000000000000, 1.000000000000000000 ) ) ;
#56482 = CARTESIAN_POINT ( 'NONE',  ( -93.67500000000003979, 92.29496732002878900, 88.51833333333333087 ) ) ;
#56483 = PLANE ( 'NONE',  #47754 ) ;
#56484 = ORIENTED_EDGE ( 'NONE', *, *, #59234, .F. ) ;
#56485 = AXIS2_PLACEMENT_3D ( 'NONE', #56749, #68397, #39823 ) ;
#56486 = DIRECTION ( 'NONE',  ( 0.000000000000000000, 0.6494480483301793283, 0.7604059656000345946 ) ) ;
#56487 = VECTOR ( 'NONE', #27308, 1000.000000000000000 ) ;
#56488 = AXIS2_PLACEMENT_3D ( 'NONE', #33680, #39710, #61897 ) ;
#56489 = DIRECTION ( 'NONE',  ( 1.000000000000000000, 0.000000000000000000, 0.000000000000000000 ) ) ;
#56490 = ORIENTED_EDGE ( 'NONE', *, *, #47032, .F. ) ;
#56491 = CARTESIAN_POINT ( 'NONE',  ( 10.00000000000000000, 30.41916302227216562, -71.27951684757994144 ) ) ;
#56492 = DIRECTION ( 'NONE',  ( -1.000000000000000000, 0.000000000000000000, -0.000000000000000000 ) ) ;
#56493 = VERTEX_POINT ( 'NONE', #38987 ) ;
#56494 =( BOUNDED_CURVE ( )  B_SPLINE_CURVE ( 2, ( #70066, #6209, #6567, #28746, #57703, #35498, #63718 ),
 .UNSPECIFIED., .F., .F. ) 
 B_SPLINE_CURVE_WITH_KNOTS ( ( 3, 2, 2, 3 ),
 ( 0.6350190250571088324, 0.6420746642202954657, 0.6491304297611778518, 0.6561861948910820974 ),
 .UNSPECIFIED. ) 
 CURVE ( )  GEOMETRIC_REPRESENTATION_ITEM ( )  RATIONAL_B_SPLINE_CURVE ( ( 0.9999952007766141904, 0.8660278034391124535, 1.000000000000000000, 0.8660254037844387076, 1.000000000000000000, 0.8660254037844387076, 1.000000000000000000 ) ) 
 REPRESENTATION_ITEM ( '' )  );
#56495 = DIRECTION ( 'NONE',  ( 0.000000000000000000, -0.4999999999999912847, -0.8660254037844435926 ) ) ;
#56496 = DIRECTION ( 'NONE',  ( 0.000000000000000000, -0.9969173337331271867, -0.07845909572785568498 ) ) ;
#56497 = ORIENTED_EDGE ( 'NONE', *, *, #37440, .F. ) ;
#56498 = CARTESIAN_POINT ( 'NONE',  ( -2.499999999999970690, 73.00000000000001421, -204.9999999999999716 ) ) ;
#56499 = VECTOR ( 'NONE', #63391, 1000.000000000000000 ) ;
#56500 = VERTEX_POINT ( 'NONE', #63405 ) ;
#56501 = CARTESIAN_POINT ( 'NONE',  ( 0.000000000000000000, 30.41916302227113178, 71.27951684758036777 ) ) ;
#56502 = VERTEX_POINT ( 'NONE', #45756 ) ;
#56503 = AXIS2_PLACEMENT_3D ( 'NONE', #47454, #36165, #47817 ) ;
#56504 = FACE_OUTER_BOUND ( 'NONE', #1910, .T. ) ;
#56505 = ORIENTED_EDGE ( 'NONE', *, *, #17315, .T. ) ;
#56506 = VERTEX_POINT ( 'NONE', #57762 ) ;
#56507 = AXIS2_PLACEMENT_3D ( 'NONE', #59161, #65180, #7652 ) ;
#56508 = ORIENTED_EDGE ( 'NONE', *, *, #45338, .T. ) ;
#56509 = DIRECTION ( 'NONE',  ( 0.000000000000000000, 0.3090169943749411230, 0.9510565162951555296 ) ) ;
#56510 = ADVANCED_FACE ( 'NONE', ( #63052 ), #56279, .F. ) ;
#56511 = ORIENTED_EDGE ( 'NONE', *, *, #17925, .T. ) ;
#56512 = EDGE_LOOP ( 'NONE', ( #25532, #24416, #48414, #68658 ) ) ;
#56513 = CARTESIAN_POINT ( 'NONE',  ( 93.67499999999999716, 87.70503267997126784, 87.56583333333333030 ) ) ;
#56514 = DIRECTION ( 'NONE',  ( 0.000000000000000000, 0.000000000000000000, 1.000000000000000000 ) ) ;
#56515 = DIRECTION ( 'NONE',  ( -1.000000000000000000, 0.000000000000000000, 0.000000000000000000 ) ) ;
#56516 = VERTEX_POINT ( 'NONE', #56662 ) ;
#56517 = ORIENTED_EDGE ( 'NONE', *, *, #69987, .T. ) ;
#56518 = VERTEX_POINT ( 'NONE', #69043 ) ;
#56519 = CARTESIAN_POINT ( 'NONE',  ( 92.69370383062498320, 90.00000000000002842, 88.37281250086715545 ) ) ;
#56520 = EDGE_LOOP ( 'NONE', ( #48984, #35129, #25546, #58850 ) ) ;
#56521 = CARTESIAN_POINT ( 'NONE',  ( 95.00000000000000000, -207.3369185715606307, 83.76906250086713612 ) ) ;
#56522 = SHAPE_DEFINITION_REPRESENTATION ( #36733, #15311 ) ;
#56523 = DIRECTION ( 'NONE',  ( 0.000000000000000000, 0.000000000000000000, 1.000000000000000000 ) ) ;
#56524 = CYLINDRICAL_SURFACE ( 'NONE', #614, 42.00000000000000000 ) ;
#56525 = DIRECTION ( 'NONE',  ( -1.000000000000000000, -0.000000000000000000, 0.000000000000000000 ) ) ;
#56526 = CARTESIAN_POINT ( 'NONE',  ( 10.00000000000000000, -37.22597642581153821, 10.79786254984320415 ) ) ;
#56527 = EDGE_CURVE ( 'NONE', #28695, #22274, #17528, .T. ) ;
#56528 = DIRECTION ( 'NONE',  ( -0.3420201433256714330, 0.000000000000000000, -0.9396926207859073177 ) ) ;
#56529 = LINE ( 'NONE', #38852, #13199 ) ;
#56530 = CARTESIAN_POINT ( 'NONE',  ( -94.99999999999997158, -212.6630814284392557, 88.53156250086713897 ) ) ;
#56531 = ADVANCED_FACE ( 'NONE', ( #51743 ), #50246, .T. ) ;
#56532 = CARTESIAN_POINT ( 'NONE',  ( -97.30629616937501680, 91.33154071421968467, 84.66864583420047552 ) ) ;
#56533 = EDGE_LOOP ( 'NONE', ( #48761, #17201, #62645, #72296, #60458, #39208, #66837, #939 ) ) ;
#56535 = CARTESIAN_POINT ( 'NONE',  ( -96.15314808468752972, 91.99731107132950569, 86.36197916753381776 ) ) ;
#56534 = CARTESIAN_POINT ( 'NONE',  ( 97.30629616937498838, 91.33154071421968467, 87.47322916753381605 ) ) ;
#56536 = ORIENTED_EDGE ( 'NONE', *, *, #23006, .F. ) ;
#56537 = LINE ( 'NONE', #15927, #4704 ) ;
#56538 = CARTESIAN_POINT ( 'NONE',  ( 11.99999999999999822, -26.02418014898260878, -70.52718814184285634 ) ) ;
#56539 = DIRECTION ( 'NONE',  ( 1.000000000000000000, -3.061616997868382648E-16, -0.000000000000000000 ) ) ;
#56540 = CARTESIAN_POINT ( 'NONE',  ( 97.64999999999324132, 90.00000598221777182, 82.14187520865721126 ) ) ;
#56541 = CARTESIAN_POINT ( 'NONE',  ( -97.65000000000001990, 90.00000000000004263, 86.82500000000000284 ) ) ;
#56542 = LINE ( 'NONE', #73805, #13864 ) ;
#56543 = EDGE_CURVE ( 'NONE', #44032, #39761, #52028, .T. ) ;
#56544 = EDGE_CURVE ( 'NONE', #47972, #47168, #51002, .T. ) ;
#56545 = VECTOR ( 'NONE', #7728, 1000.000000000000000 ) ;
#56546 = DIRECTION ( 'NONE',  ( -1.000000000000000000, -0.000000000000000000, -0.000000000000000000 ) ) ;
#56547 = DIRECTION ( 'NONE',  ( -0.7950889364178796992, 0.6064928550163510845, 0.000000000000000000 ) ) ;
#56548 = VECTOR ( 'NONE', #13714, 1000.000000000000114 ) ;
#56549 = CARTESIAN_POINT ( 'NONE',  ( -26.53422223201112828, -120.6595836127786043, -5.500000000000000000 ) ) ;
#56550 = ORIENTED_EDGE ( 'NONE', *, *, #8000, .F. ) ;
#56551 = ORIENTED_EDGE ( 'NONE', *, *, #73309, .F. ) ;
#56552 = CARTESIAN_POINT ( 'NONE',  ( -93.67500000000003979, 92.29496732002878900, 80.26333333333332121 ) ) ;
#56553 = DIRECTION ( 'NONE',  ( -1.000000000000000000, 0.000000000000000000, -0.000000000000000000 ) ) ;
#56554 = CARTESIAN_POINT ( 'NONE',  ( 92.34999999999995168, -208.4700217866474929, 75.97708333333333997 ) ) ;
#56555 = CARTESIAN_POINT ( 'NONE',  ( -6.782329983125267248, 10.49999999999999645, -104.9999999999999858 ) ) ;
#56556 = CARTESIAN_POINT ( 'NONE',  ( -16.06301359042743115, -102.7814171781257357, 5.500000000000000000 ) ) ;
#56557 = APPLICATION_CONTEXT ( 'automotive_design' ) ;
#56558 = CARTESIAN_POINT ( 'NONE',  ( 10.00000000000000000, -23.16143007188376757, -73.95703589263997912 ) ) ;
#56559 = PLANE ( 'NONE',  #30106 ) ;
#56560 = DIRECTION ( 'NONE',  ( 1.000000000000000000, 0.000000000000000000, 0.000000000000000000 ) ) ;
#56561 = EDGE_CURVE ( 'NONE', #34086, #7754, #47259, .T. ) ;
#56562 = ORIENTED_EDGE ( 'NONE', *, *, #61728, .F. ) ;
#56563 = CARTESIAN_POINT ( 'NONE',  ( -92.69370383062502583, 91.33154071421968467, 79.21822916753380639 ) ) ;
#56564 = AXIS2_PLACEMENT_3D ( 'NONE', #37223, #35716, #36101 ) ;
#56565 = DIRECTION ( 'NONE',  ( 0.9435911131814395114, -0.3311129884571304971, 0.000000000000000000 ) ) ;
#56566 = VECTOR ( 'NONE', #10381, 999.9999999999998863 ) ;
#56567 = DIRECTION ( 'NONE',  ( 0.000000000000000000, 0.9510565162951523099, 0.3090169943749517811 ) ) ;
#56568 = CIRCLE ( 'NONE', #18121, 16.00000000000000000 ) ;
#56569 = DIRECTION ( 'NONE',  ( 0.000000000000000000, 0.9876883405951381034, -0.1564344650402276216 ) ) ;
#56570 = CARTESIAN_POINT ( 'NONE',  ( 0.000000000000000000, 0.000000000000000000, 0.000000000000000000 ) ) ;
#56571 = CARTESIAN_POINT ( 'NONE',  ( -97.65000000000001990, 90.00000000000004263, 89.44437500173430067 ) ) ;
#56572 = CARTESIAN_POINT ( 'NONE',  ( -94.99999999999997158, -207.3369185715606307, 89.64281250086715147 ) ) ;
#56573 = CIRCLE ( 'NONE', #68592, 31.99999999999999289 ) ;
#56574 = ADVANCED_FACE ( 'NONE', ( #6980 ), #47216, .F. ) ;
#56575 = ADVANCED_FACE ( 'NONE', ( #58872 ), #6621, .F. ) ;
#56576 = CARTESIAN_POINT ( 'NONE',  ( 97.30629616937498838, 88.66845928578035796, 79.90614583420048689 ) ) ;
#56577 = CARTESIAN_POINT ( 'NONE',  ( -97.30629616937495996, -209.9999999999999716, 79.64156250086715261 ) ) ;
#56578 = DIRECTION ( 'NONE',  ( -1.000000000000000000, 0.000000000000000000, 0.000000000000000000 ) ) ;
#56579 = ORIENTED_EDGE ( 'NONE', *, *, #10954, .T. ) ;
#56580 = CARTESIAN_POINT ( 'NONE',  ( -97.65000000000001990, 88.47002178664754979, 86.95729166840096980 ) ) ;
#56581 = CARTESIAN_POINT ( 'NONE',  ( -94.99999999999997158, -213.0599564267049857, 75.55375000000000796 ) ) ;
#56582 = DIRECTION ( 'NONE',  ( -1.000000000000000000, 0.000000000000000000, 0.000000000000000000 ) ) ;
#56583 = CARTESIAN_POINT ( 'NONE',  ( -97.30629616937501680, 91.33154071421968467, 78.95364583420045790 ) ) ;
#56584 = CARTESIAN_POINT ( 'NONE',  ( 96.15314808468748708, -208.0026889286704943, 79.27114583420046756 ) ) ;
#56585 = ORIENTED_EDGE ( 'NONE', *, *, #27333, .T. ) ;
#56586 = DIRECTION ( 'NONE',  ( 1.000000000000000000, 1.427937372958405461E-15, 7.962523111839130290E-16 ) ) ;
#56587 = ORIENTED_EDGE ( 'NONE', *, *, #64946, .T. ) ;
#56588 = CARTESIAN_POINT ( 'NONE',  ( -3.000000000000000000, -10.45096189432344147, 21.10159698893426494 ) ) ;
#56589 = ORIENTED_EDGE ( 'NONE', *, *, #57672, .F. ) ;
#56590 = CIRCLE ( 'NONE', #48208, 31.99999999999999289 ) ;
#56591 = CIRCLE ( 'NONE', #20513, 37.49900000000001654 ) ;
#56593 = AXIS2_PLACEMENT_3D ( 'NONE', #7266, #47484, #12149 ) ;
#56592 = CARTESIAN_POINT ( 'NONE',  ( -92.35000000002618492, -210.0000000000000853, -64.99999999999342037 ) ) ;
#56594 = CIRCLE ( 'NONE', #17147, 77.49899999999999523 ) ;
#56595 = ORIENTED_EDGE ( 'NONE', *, *, #6083, .F. ) ;
#56596 = ORIENTED_EDGE ( 'NONE', *, *, #32088, .T. ) ;
#56597 = ORIENTED_EDGE ( 'NONE', *, *, #12038, .T. ) ;
#56598 = CARTESIAN_POINT ( 'NONE',  ( 96.15314808468748708, -208.0026889286704943, 74.98489583420048632 ) ) ;
#56599 = EDGE_LOOP ( 'NONE', ( #28554, #55936, #774, #52923 ) ) ;
#56600 = PLANE ( 'NONE',  #62841 ) ;
#56601 = EDGE_CURVE ( 'NONE', #27271, #44954, #44393, .T. ) ;
#56602 = CARTESIAN_POINT ( 'NONE',  ( 96.15314808468748708, 91.99731107132950569, 86.41489583420049314 ) ) ;
#56603 = DIRECTION ( 'NONE',  ( -0.9997280174009349762, 0.02332147558787823691, 0.000000000000000000 ) ) ;
#56604 = CARTESIAN_POINT ( 'NONE',  ( 93.67500000000001137, -212.2949673200287179, 79.31083333333333485 ) ) ;
#56605 = ORIENTED_EDGE ( 'NONE', *, *, #35391, .F. ) ;
#56606 = ORIENTED_EDGE ( 'NONE', *, *, #24694, .F. ) ;
#56607 = ORIENTED_EDGE ( 'NONE', *, *, #71806, .F. ) ;
#56608 = ORIENTED_EDGE ( 'NONE', *, *, #28508, .F. ) ;
#56609 = LINE ( 'NONE', #73875, #14213 ) ;
#56610 = AXIS2_PLACEMENT_3D ( 'NONE', #69292, #29415, #52363 ) ;
#56611 = ADVANCED_FACE ( 'NONE', ( #29166 ), #69767, .T. ) ;
#56612 = AXIS2_PLACEMENT_3D ( 'NONE', #50884, #22701, #57276 ) ;
#56613 = DIRECTION ( 'NONE',  ( -1.000000000000000000, 0.000000000000000000, 0.000000000000000000 ) ) ;
#56614 = CARTESIAN_POINT ( 'NONE',  ( 5.000000000000000000, 35.47612816024556537, -22.48208911017461631 ) ) ;
#56615 = CIRCLE ( 'NONE', #15764, 82.00000000000000000 ) ;
#56616 = DIRECTION ( 'NONE',  ( 0.000000000000000000, 0.000000000000000000, 1.000000000000000000 ) ) ;
#56617 = ADVANCED_FACE ( 'NONE', ( #69396 ), #1760, .T. ) ;
#56618 = DIRECTION ( 'NONE',  ( -0.000000000000000000, -0.000000000000000000, 1.000000000000000000 ) ) ;
#56619 = CARTESIAN_POINT ( 'NONE',  ( -97.64995850092280705, -211.5300021728558022, 83.78229332575403987 ) ) ;
#56620 = ORIENTED_EDGE ( 'NONE', *, *, #48873, .F. ) ;
#56621 = CARTESIAN_POINT ( 'NONE',  ( -97.64999999999994884, -208.4700217866474645, 81.77145833506763495 ) ) ;
#56622 = ORIENTED_EDGE ( 'NONE', *, *, #12537, .F. ) ;
#56623 = CARTESIAN_POINT ( 'NONE',  ( 94.99999999999998579, 90.00000000000002842, 75.00000000000000000 ) ) ;
#56624 = ORIENTED_EDGE ( 'NONE', *, *, #18297, .F. ) ;
#56626 = CARTESIAN_POINT ( 'NONE',  ( -96.32500000000001705, 92.29496732002878900, 79.17854166840096752 ) ) ;
#56625 = CARTESIAN_POINT ( 'NONE',  ( 94.99999999999998579, 86.94004357329500010, 83.25312500173430408 ) ) ;
#56627 = VECTOR ( 'NONE', #31578, 1000.000000000000000 ) ;
#56628 = ORIENTED_EDGE ( 'NONE', *, *, #36471, .F. ) ;
#56629 = CARTESIAN_POINT ( 'NONE',  ( 94.99999999999998579, 92.66308142843935514, 82.65781250086715204 ) ) ;
#56630 = CARTESIAN_POINT ( 'NONE',  ( -97.64999999999999147, -208.4700217866475498, 86.77208333333334167 ) ) ;
#56631 = CYLINDRICAL_SURFACE ( 'NONE', #72654, 37.49900000000000233 ) ;
#56632 = CARTESIAN_POINT ( 'NONE',  ( -3.000000000000000000, 0.000000000000000000, 0.000000000000000000 ) ) ;
#56633 = DIRECTION ( 'NONE',  ( -1.000000000000000000, -0.000000000000000000, 0.000000000000000000 ) ) ;
#56634 = ADVANCED_FACE ( 'NONE', ( #12618 ), #17896, .T. ) ;
#56635 = DIRECTION ( 'NONE',  ( -0.000000000000000000, -0.000000000000000000, 1.000000000000000000 ) ) ;
#56636 = ORIENTED_EDGE ( 'NONE', *, *, #25460, .T. ) ;
#56637 = DIRECTION ( 'NONE',  ( 1.000000000000000000, 0.000000000000000000, 0.000000000000000000 ) ) ;
#56638 = CARTESIAN_POINT ( 'NONE',  ( 92.35000000009274856, -209.9999861897330788, 80.55392363656960697 ) ) ;
#56639 = DIRECTION ( 'NONE',  ( 1.000000000000000000, 0.000000000000000000, 0.000000000000000000 ) ) ;
#56640 = ORIENTED_EDGE ( 'NONE', *, *, #565, .F. ) ;
#56641 = ORIENTED_EDGE ( 'NONE', *, *, #68620, .T. ) ;
#56642 = PRODUCT_DEFINITION_SHAPE ( 'NONE', 'NONE',  #29261 ) ;
#56643 = DIRECTION ( 'NONE',  ( -1.000000000000000000, 5.236901059551556403E-15, 2.618450529775778123E-14 ) ) ;
#56644 = EDGE_CURVE ( 'NONE', #71305, #32419, #29207, .T. ) ;
#56645 = CARTESIAN_POINT ( 'NONE',  ( 0.000000000000000000, -27.13269053701114331, 25.88420570971391754 ) ) ;
#56646 = LINE ( 'NONE', #62279, #36535 ) ;
#56647 = CARTESIAN_POINT ( 'NONE',  ( -94.99999999999997158, -212.6630814284392557, 80.43531250086715545 ) ) ;
#56648 = VERTEX_POINT ( 'NONE', #41948 ) ;
#56649 = FACE_OUTER_BOUND ( 'NONE', #22007, .T. ) ;
#56650 = EDGE_CURVE ( 'NONE', #53734, #12406, #71226, .T. ) ;
#56651 = ORIENTED_EDGE ( 'NONE', *, *, #71115, .T. ) ;
#56652 =( GEOMETRIC_REPRESENTATION_CONTEXT ( 3 ) GLOBAL_UNCERTAINTY_ASSIGNED_CONTEXT ( ( #10600 ) ) GLOBAL_UNIT_ASSIGNED_CONTEXT ( ( #795, #36071, #40988 ) ) REPRESENTATION_CONTEXT ( 'NONE', 'WORKASPACE' ) );
#56653 = DIRECTION ( 'NONE',  ( 0.000000000000000000, 0.000000000000000000, 1.000000000000000000 ) ) ;
#56654 = EDGE_CURVE ( 'NONE', #57624, #47069, #66268, .T. ) ;
#56655 = CARTESIAN_POINT ( 'NONE',  ( 92.34999999999999432, 90.00000000000002842, 81.82437500173429612 ) ) ;
#56656 = AXIS2_PLACEMENT_3D ( 'NONE', #22993, #40642, #40271 ) ;
#56657 = CARTESIAN_POINT ( 'NONE',  ( 12.00000000000000000, 24.81905959214260804, -9.408202855044828894 ) ) ;
#56658 = CYLINDRICAL_SURFACE ( 'NONE', #46455, 2.649999999999985700 ) ;
#56659 = FACE_OUTER_BOUND ( 'NONE', #44420, .T. ) ;
#56660 = DIRECTION ( 'NONE',  ( 1.000000000000000000, -0.000000000000000000, -0.000000000000000000 ) ) ;
#56661 = CARTESIAN_POINT ( 'NONE',  ( 10.00000000000000000, -73.73191006444561424, -14.66109333815538918 ) ) ;
#56662 = CARTESIAN_POINT ( 'NONE',  ( 0.000000000000000000, 22.90783923731740401, -78.73519480814930205 ) ) ;
#56663 = DIRECTION ( 'NONE',  ( -1.000000000000000000, -0.000000000000000000, -0.000000000000000000 ) ) ;
#56664 = CARTESIAN_POINT ( 'NONE',  ( 10.00000000000000000, -65.58780272294048075, -36.73666225445966660 ) ) ;
#56665 = EDGE_CURVE ( 'NONE', #18290, #58390, #747, .T. ) ;
#56666 = CARTESIAN_POINT ( 'NONE',  ( -11.59517495878806947, -96.12423995607481686, 5.500000000000000000 ) ) ;
#56667 = DIRECTION ( 'NONE',  ( 0.8541291221503261033, -0.5200609990133016058, 0.000000000000000000 ) ) ;
#56668 = DIRECTION ( 'NONE',  ( -1.000000000000000000, -0.000000000000000000, -0.000000000000000000 ) ) ;
#56669 = DIRECTION ( 'NONE',  ( -1.000000000000000000, -0.000000000000000000, 0.000000000000000000 ) ) ;
#56670 = ORIENTED_EDGE ( 'NONE', *, *, #9347, .T. ) ;
#56671 = DIRECTION ( 'NONE',  ( 1.000000000000000000, 0.000000000000000000, 0.000000000000000000 ) ) ;
#56672 = CARTESIAN_POINT ( 'NONE',  ( -93.84685191531252713, 88.00268892867056536, 80.96447916753380980 ) ) ;
#56673 = VECTOR ( 'NONE', #30899, 1000.000000000000000 ) ;
#56674 = CONICAL_SURFACE ( 'NONE', #36203, 15.39727592589476579, 0.2094395102393128150 ) ;
#56675 = LINE ( 'NONE', #57399, #33865 ) ;
#56676 = EDGE_LOOP ( 'NONE', ( #12107, #41894, #19135, #19654 ) ) ;
#56677 = CARTESIAN_POINT ( 'NONE',  ( 95.00000000000000000, -213.0599564267049857, 80.07812500173429271 ) ) ;
#56678 = LINE ( 'NONE', #33336, #60005 ) ;
#56679 = CYLINDRICAL_SURFACE ( 'NONE', #8396, 16.00000000000000000 ) ;
#56680 = DIRECTION ( 'NONE',  ( -0.2306669878475637314, -0.9730327541852493711, 0.000000000000000000 ) ) ;
#56681 = CARTESIAN_POINT ( 'NONE',  ( 97.30629616937498838, -211.3315407142195852, 76.09614583420048461 ) ) ;
#56682 = VERTEX_POINT ( 'NONE', #20395 ) ;
#56683 = VERTEX_POINT ( 'NONE', #58122 ) ;
#56684 = DIRECTION ( 'NONE',  ( -1.000000000000000000, -0.000000000000000000, -0.000000000000000000 ) ) ;
#56685 = CARTESIAN_POINT ( 'NONE',  ( -3.000000000000000000, 0.000000000000000000, 0.000000000000000000 ) ) ;
#56686 = LINE ( 'NONE', #33741, #24427 ) ;
#56687 = CYLINDRICAL_SURFACE ( 'NONE', #54293, 82.00000000000000000 ) ;
#56688 = CARTESIAN_POINT ( 'NONE',  ( 6.782329983125270800, 10.49999999999999467, 20.00000000000000000 ) ) ;
#56689 = CARTESIAN_POINT ( 'NONE',  ( 93.67500000000001137, -212.2949673200287179, 87.56583333333333030 ) ) ;
#56690 = EDGE_CURVE ( 'NONE', #6124, #56906, #25619, .T. ) ;
#56691 = PRESENTATION_LAYER_ASSIGNMENT (  '', '', ( #21897 ) ) ;
#56692 = AXIS2_PLACEMENT_3D ( 'NONE', #19165, #54494, #2295 ) ;
#56693 = VERTEX_POINT ( 'NONE', #16598 ) ;
#56694 = EDGE_CURVE ( 'NONE', #39132, #55889, #4974, .T. ) ;
#56695 = DIRECTION ( 'NONE',  ( 0.000000000000000000, 0.000000000000000000, 1.000000000000000000 ) ) ;
#56696 = ORIENTED_EDGE ( 'NONE', *, *, #34235, .T. ) ;
#56697 = ORIENTED_EDGE ( 'NONE', *, *, #8397, .T. ) ;
#56698 = FACE_OUTER_BOUND ( 'NONE', #19263, .T. ) ;
#56699 = ADVANCED_FACE ( 'NONE', ( #45188 ), #44812, .T. ) ;
#56700 = VECTOR ( 'NONE', #5255, 1000.000000000000000 ) ;
#56701 = PRESENTATION_STYLE_ASSIGNMENT (( #45042 ) ) ;
#56702 = DIRECTION ( 'NONE',  ( 0.000000000000000000, 0.000000000000000000, 1.000000000000000000 ) ) ;
#56703 = VERTEX_POINT ( 'NONE', #68108 ) ;
#56704 = CARTESIAN_POINT ( 'NONE',  ( 50.00005079999999680, 0.000000000000000000, 0.000000000000000000 ) ) ;
#56705 = CARTESIAN_POINT ( 'NONE',  ( 97.64999999999997726, -211.5299782133524502, 75.10395833506764518 ) ) ;
#56706 = EDGE_CURVE ( 'NONE', #54282, #73989, #38829, .T. ) ;
#56707 = CARTESIAN_POINT ( 'NONE',  ( 92.34999999999999432, 88.47002178664753558, 83.06791666666664753 ) ) ;
#56708 = ORIENTED_EDGE ( 'NONE', *, *, #58886, .F. ) ;
#56709 = FACE_OUTER_BOUND ( 'NONE', #2264, .T. ) ;
#56710 = CIRCLE ( 'NONE', #21861, 31.99999999999999289 ) ;
#56711 = EDGE_LOOP ( 'NONE', ( #35497, #5317, #31321, #32104 ) ) ;
#56712 = CARTESIAN_POINT ( 'NONE',  ( 0.000000000000000000, 71.27951684758068041, -30.41916302227035018 ) ) ;
#56713 = ORIENTED_EDGE ( 'NONE', *, *, #40653, .F. ) ;
#56714 = CARTESIAN_POINT ( 'NONE',  ( 97.65000000000000568, 88.47002178664752137, 84.62895833506763665 ) ) ;
#56715 = VECTOR ( 'NONE', #12316, 1000.000000000000000 ) ;
#56716 = EDGE_CURVE ( 'NONE', #46506, #58494, #73361, .T. ) ;
#56717 =( BOUNDED_CURVE ( )  B_SPLINE_CURVE ( 2, ( #53954, #32110, #65984, #7711, #71214, #48304, #26480 ),
 .UNSPECIFIED., .F., .T. ) 
 B_SPLINE_CURVE_WITH_KNOTS ( ( 3, 2, 2, 3 ),
 ( 0.4583333333333335924, 0.4652777777777780122, 0.4722222222222224319, 0.4791666666666668517 ),
 .UNSPECIFIED. ) 
 CURVE ( )  GEOMETRIC_REPRESENTATION_ITEM ( )  RATIONAL_B_SPLINE_CURVE ( ( 0.9999999999999946709, 0.8660254037844440367, 1.000000000000000000, 0.8660254037844387076, 1.000000000000000000, 0.8660254037844354880, 1.000000000000003109 ) ) 
 REPRESENTATION_ITEM ( '' )  );
#56718 = CARTESIAN_POINT ( 'NONE',  ( -95.00000000000002842, 87.33691857156074434, 82.97531250086714749 ) ) ;
#56719 = CARTESIAN_POINT ( 'NONE',  ( 93.84685191531248449, 91.99731107132950569, 77.47197916753380298 ) ) ;
#56720 = ORIENTED_EDGE ( 'NONE', *, *, #31137, .T. ) ;
#56721 = DIRECTION ( 'NONE',  ( 0.000000000000000000, 0.1564344650402311743, -0.9876883405951377704 ) ) ;
#56722 = CARTESIAN_POINT ( 'NONE',  ( -95.00000000000002842, 90.00000000000004263, 90.00000000000000000 ) ) ;
#56723 = DIRECTION ( 'NONE',  ( -1.000000000000000000, 0.000000000000000000, 0.000000000000000000 ) ) ;
#56724 = CARTESIAN_POINT ( 'NONE',  ( 0.000000000000000000, 0.000000000000000000, 0.000000000000000000 ) ) ;
#56725 = ORIENTED_EDGE ( 'NONE', *, *, #38096, .F. ) ;
#56726 = DIRECTION ( 'NONE',  ( 1.000000000000000000, -0.000000000000000000, -0.000000000000000000 ) ) ;
#56727 = AXIS2_PLACEMENT_3D ( 'NONE', #60389, #25427, #48349 ) ;
#56728 = AXIS2_PLACEMENT_3D ( 'NONE', #58090, #46817, #29496 ) ;
#56729 = CARTESIAN_POINT ( 'NONE',  ( -93.84685191531248449, -208.0026889286704943, 76.73114583420047552 ) ) ;
#56730 = ORIENTED_EDGE ( 'NONE', *, *, #44025, .T. ) ;
#56731 = ORIENTED_EDGE ( 'NONE', *, *, #58716, .F. ) ;
#56732 = DIRECTION ( 'NONE',  ( 0.000000000000000000, 0.000000000000000000, 1.000000000000000000 ) ) ;
#56733 = ORIENTED_EDGE ( 'NONE', *, *, #22929, .T. ) ;
#56734 = CARTESIAN_POINT ( 'NONE',  ( 97.64999999999999147, 90.00000000000002842, 78.25249999999999773 ) ) ;
#56735 = CARTESIAN_POINT ( 'NONE',  ( -11.63999999999999702, 0.000000000000000000, 0.000000000000000000 ) ) ;
#56736 = ORIENTED_EDGE ( 'NONE', *, *, #42466, .T. ) ;
#56737 = CARTESIAN_POINT ( 'NONE',  ( -97.30629616937497417, -208.6684592857803011, 74.98489583420048632 ) ) ;
#56738 = ORIENTED_EDGE ( 'NONE', *, *, #68358, .T. ) ;
#56739 = DIRECTION ( 'NONE',  ( -0.000000000000000000, -0.000000000000000000, -1.000000000000000000 ) ) ;
#56740 = CYLINDRICAL_SURFACE ( 'NONE', #32034, 16.00000000000000000 ) ;
#56741 = CARTESIAN_POINT ( 'NONE',  ( 4.250000000000000000, -13.95926121303099343, 0.000000000000000000 ) ) ;
#56742 = DIRECTION ( 'NONE',  ( 0.000000000000000000, 0.000000000000000000, 1.000000000000000000 ) ) ;
#56743 = CARTESIAN_POINT ( 'NONE',  ( -10.00000000000000000, 0.000000000000000000, 0.000000000000000000 ) ) ;
#56744 = EDGE_CURVE ( 'NONE', #22108, #63004, #21869, .T. ) ;
#56745 = EDGE_CURVE ( 'NONE', #53342, #18595, #27878, .T. ) ;
#56746 = CARTESIAN_POINT ( 'NONE',  ( 94.99999999999998579, 87.33691857156068750, 84.72156250086713669 ) ) ;
#56747 = DIRECTION ( 'NONE',  ( -0.9038112904824853189, 0.4279312458752976833, 0.000000000000000000 ) ) ;
#56748 = CARTESIAN_POINT ( 'NONE',  ( 10.00000000000000000, 31.47745569255237896, -68.26794271651228030 ) ) ;
#56749 = CARTESIAN_POINT ( 'NONE',  ( 0.000000000000000000, 0.000000000000000000, 0.000000000000000000 ) ) ;
#56750 = DIRECTION ( 'NONE',  ( 0.1736481776669309418, 0.9848077530122080203, -0.000000000000000000 ) ) ;
#56751 = DIRECTION ( 'NONE',  ( 0.000000000000000000, -0.1564344650402381687, 0.9876883405951365491 ) ) ;
#56752 = CARTESIAN_POINT ( 'NONE',  ( 92.35000000000002274, -209.9999719686936430, 87.53937403222813884 ) ) ;
#56753 = EDGE_CURVE ( 'NONE', #5465, #38312, #32397, .T. ) ;
#56754 = CARTESIAN_POINT ( 'NONE',  ( 10.00000000000000000, 0.000000000000000000, 0.000000000000000000 ) ) ;
#56755 = CARTESIAN_POINT ( 'NONE',  ( 92.34999999999999432, 90.00000000000002842, 78.57000000000000739 ) ) ;
#56756 =( GEOMETRIC_REPRESENTATION_CONTEXT ( 3 ) GLOBAL_UNCERTAINTY_ASSIGNED_CONTEXT ( ( #2508 ) ) GLOBAL_UNIT_ASSIGNED_CONTEXT ( ( #45710, #63008, #26900 ) ) REPRESENTATION_CONTEXT ( 'NONE', 'WORKASPACE' ) );
#56757 = DIRECTION ( 'NONE',  ( -1.000000000000000000, 0.000000000000000000, 0.000000000000000000 ) ) ;
#56758 = CARTESIAN_POINT ( 'NONE',  ( -99.99999999999997158, -204.9999999999999716, 90.00000000000000000 ) ) ;
#56759 = DIRECTION ( 'NONE',  ( -1.000000000000000000, -0.000000000000000000, 0.000000000000000000 ) ) ;
#56760 = AXIS2_PLACEMENT_3D ( 'NONE', #31347, #49005, #19326 ) ;
#56761 = CARTESIAN_POINT ( 'NONE',  ( -94.99999999999997158, -213.0599564267049857, 83.80875000000000341 ) ) ;
#56762 = VECTOR ( 'NONE', #37777, 1000.000000000000227 ) ;
#56763 = DIRECTION ( 'NONE',  ( 0.000000000000000000, 0.000000000000000000, 1.000000000000000000 ) ) ;
#56764 = AXIS2_PLACEMENT_3D ( 'NONE', #50275, #23212, #51392 ) ;
#56765 = FACE_OUTER_BOUND ( 'NONE', #48581, .T. ) ;
#56766 = DIRECTION ( 'NONE',  ( -0.000000000000000000, -0.000000000000000000, 1.000000000000000000 ) ) ;
#56767 = CYLINDRICAL_SURFACE ( 'NONE', #7800, 82.00000000000000000 ) ;
#56768 = VECTOR ( 'NONE', #26482, 1000.000000000000000 ) ;
#56769 = AXIS2_PLACEMENT_3D ( 'NONE', #44058, #10204, #9464 ) ;
#56770 = CARTESIAN_POINT ( 'NONE',  ( 95.00000000000000000, -212.6630814284392557, 86.78531250086716398 ) ) ;
#56771 = ORIENTED_EDGE ( 'NONE', *, *, #59924, .F. ) ;
#56772 = ORIENTED_EDGE ( 'NONE', *, *, #21288, .T. ) ;
#56773 = PLANE ( 'NONE',  #43998 ) ;
#56774 = VERTEX_POINT ( 'NONE', #61364 ) ;
#56775 = DIRECTION ( 'NONE',  ( 2.603472992746261562E-14, 2.546204323184492723E-14, -1.000000000000000000 ) ) ;
#56776 = CARTESIAN_POINT ( 'NONE',  ( 96.15314808468750130, -211.9973110713294489, 79.69447916753379957 ) ) ;
#56777 = EDGE_LOOP ( 'NONE', ( #59528, #20795, #31290, #6217 ) ) ;
#56778 = CARTESIAN_POINT ( 'NONE',  ( 96.15314808468750130, -211.9973110713294489, 84.29822916753381890 ) ) ;
#56779 = VERTEX_POINT ( 'NONE', #62101 ) ;
#56780 = LINE ( 'NONE', #72190, #44267 ) ;
#56781 = ORIENTED_EDGE ( 'NONE', *, *, #60522, .T. ) ;
#56782 = VERTEX_POINT ( 'NONE', #60981 ) ;
#56783 = SURFACE_SIDE_STYLE ('',( #51127 ) ) ;
#56784 = EDGE_CURVE ( 'NONE', #65045, #27851, #7651, .T. ) ;
#56785 = DIRECTION ( 'NONE',  ( 0.000000000000000000, 0.000000000000000000, 1.000000000000000000 ) ) ;
#56786 = VERTEX_POINT ( 'NONE', #32027 ) ;
#56787 = DIRECTION ( 'NONE',  ( 0.000000000000000000, 0.000000000000000000, 1.000000000000000000 ) ) ;
#56788 = CARTESIAN_POINT ( 'NONE',  ( 95.00000000000000000, -206.9400435732949575, 85.47562500173431488 ) ) ;
#56789 = EDGE_CURVE ( 'NONE', #60775, #17276, #55341, .T. ) ;
#56790 = ORIENTED_EDGE ( 'NONE', *, *, #46094, .T. ) ;
#56791 = CARTESIAN_POINT ( 'NONE',  ( 11.34017801569539685, -96.04900080221412395, 2.500000000000000000 ) ) ;
#56792 = VERTEX_POINT ( 'NONE', #54966 ) ;
#56793 = DIRECTION ( 'NONE',  ( 0.000000000000000000, 0.000000000000000000, 1.000000000000000000 ) ) ;
#56794 = EDGE_CURVE ( 'NONE', #46417, #44028, #15484, .T. ) ;
#56795 = EDGE_LOOP ( 'NONE', ( #63631, #56790, #36339, #3337 ) ) ;
#56796 = AXIS2_PLACEMENT_3D ( 'NONE', #41161, #19691, #26075 ) ;
#56797 = EDGE_LOOP ( 'NONE', ( #45961, #41771 ) ) ;
#56798 = ORIENTED_EDGE ( 'NONE', *, *, #68598, .T. ) ;
#56799 = CARTESIAN_POINT ( 'NONE',  ( 92.69370383062501162, -211.3315407142195852, 75.09072916753382287 ) ) ;
#56800 = CARTESIAN_POINT ( 'NONE',  ( 0.000000000000000000, 0.000000000000000000, 0.000000000000000000 ) ) ;
#56801 = ORIENTED_EDGE ( 'NONE', *, *, #5064, .T. ) ;
#56802 = CIRCLE ( 'NONE', #33985, 77.49900000000000944 ) ;
#56803 = EDGE_LOOP ( 'NONE', ( #48700, #24065, #64629, #7297 ) ) ;
#56804 = ORIENTED_EDGE ( 'NONE', *, *, #21105, .F. ) ;
#56805 = DIRECTION ( 'NONE',  ( -4.476705744456277943E-17, 1.000000000000000000, -0.000000000000000000 ) ) ;
#56806 = CARTESIAN_POINT ( 'NONE',  ( -7.500000000000015099, -73.00000000000001421, -255.0000000000000000 ) ) ;
#56807 = EDGE_CURVE ( 'NONE', #48269, #21245, #71145, .T. ) ;
#56808 = CARTESIAN_POINT ( 'NONE',  ( -92.69370383062502583, 88.66845928578038638, 76.09614583420048461 ) ) ;
#56809 = EDGE_CURVE ( 'NONE', #19812, #3451, #50438, .T. ) ;
#56810 = VERTEX_POINT ( 'NONE', #72981 ) ;
#56811 = LINE ( 'NONE', #809, #47898 ) ;
#56812 = AXIS2_PLACEMENT_3D ( 'NONE', #3985, #73865, #27251 ) ;
#56813 = ORIENTED_EDGE ( 'NONE', *, *, #34273, .F. ) ;
#56814 = DIRECTION ( 'NONE',  ( 0.000000000000000000, 0.000000000000000000, 1.000000000000000000 ) ) ;
#56815 = CARTESIAN_POINT ( 'NONE',  ( -94.99999999999997158, -207.3369185715606307, 86.30906250086715659 ) ) ;
#56816 = ORIENTED_EDGE ( 'NONE', *, *, #38783, .T. ) ;
#56817 = VECTOR ( 'NONE', #12161, 1000.000000000000000 ) ;
#56818 = CARTESIAN_POINT ( 'NONE',  ( 96.74471819418084806, -211.6811075874703931, 74.86350982016034550 ) ) ;
#56819 = DIRECTION ( 'NONE',  ( 0.000000000000000000, 0.000000000000000000, -1.000000000000000000 ) ) ;
#56820 = LINE ( 'NONE', #33874, #40483 ) ;
#56821 = CARTESIAN_POINT ( 'NONE',  ( -96.15314808468747287, -208.0026889286704943, 74.93197916753379673 ) ) ;
#56822 = DIRECTION ( 'NONE',  ( -1.000000000000000000, -0.000000000000000000, -0.000000000000000000 ) ) ;
#56823 = CARTESIAN_POINT ( 'NONE',  ( 0.000000000000000000, -63.97538442413463855, 51.29473840253199057 ) ) ;
#56824 = AXIS2_PLACEMENT_3D ( 'NONE', #69486, #17984, #63866 ) ;
#56825 = EDGE_CURVE ( 'NONE', #39476, #28106, #22246, .T. ) ;
#56827 = EDGE_CURVE ( 'NONE', #70501, #62894, #25679, .T. ) ;
#56826 = AXIS2_PLACEMENT_3D ( 'NONE', #27788, #28900, #51833 ) ;
#56828 = DIRECTION ( 'NONE',  ( 0.000000000000000000, 0.000000000000000000, 1.000000000000000000 ) ) ;
#56829 = CARTESIAN_POINT ( 'NONE',  ( 10.00000000000000000, -41.81611651403859042, -3.925862922256606602 ) ) ;
#56830 = CARTESIAN_POINT ( 'NONE',  ( -92.34999999999999432, -209.9999999999999716, 90.00000000000000000 ) ) ;
#56831 = CARTESIAN_POINT ( 'NONE',  ( -93.84685191531252713, 88.00268892867056536, 82.86947916753379673 ) ) ;
#56832 = CARTESIAN_POINT ( 'NONE',  ( 11.99999999999999822, 0.000000000000000000, 0.000000000000000000 ) ) ;
#56833 = CARTESIAN_POINT ( 'NONE',  ( 0.000000000000000000, 39.04073710021366139, -15.48615015657542315 ) ) ;
#56834 = ORIENTED_EDGE ( 'NONE', *, *, #60522, .F. ) ;
#56835 = CARTESIAN_POINT ( 'NONE',  ( 11.99999999999999822, -49.70050353004932475, 59.46389618801947563 ) ) ;
#56836 = CARTESIAN_POINT ( 'NONE',  ( 0.000000000000000000, 58.39081064771751528, 50.95692526931350841 ) ) ;
#56837 = DIRECTION ( 'NONE',  ( 0.000000000000000000, 0.000000000000000000, 1.000000000000000000 ) ) ;
#56838 = PLANE ( 'NONE',  #62286 ) ;
#56839 = DIRECTION ( 'NONE',  ( 0.000000000000000000, 0.000000000000000000, 1.000000000000000000 ) ) ;
#56840 = DIRECTION ( 'NONE',  ( -0.000000000000000000, -0.000000000000000000, -1.000000000000000000 ) ) ;
#56841 = CARTESIAN_POINT ( 'NONE',  ( -97.30629616937495996, -209.9999999999999716, 79.64156250086715261 ) ) ;
#56842 = CYLINDRICAL_SURFACE ( 'NONE', #30868, 2.649999999999985700 ) ;
#56843 = AXIS2_PLACEMENT_3D ( 'NONE', #22060, #4050, #49875 ) ;
#56844 = ORIENTED_EDGE ( 'NONE', *, *, #53204, .F. ) ;
#56845 = DIRECTION ( 'NONE',  ( 0.000000000000000000, 0.000000000000000000, 1.000000000000000000 ) ) ;
#56846 = CARTESIAN_POINT ( 'NONE',  ( 0.000000000000000000, -67.80270845531855173, -46.11716303203261447 ) ) ;
#56847 = FACE_OUTER_BOUND ( 'NONE', #73144, .T. ) ;
#56848 = PLANE ( 'NONE',  #7740 ) ;
#56849 = DIRECTION ( 'NONE',  ( 1.000000000000000000, 0.000000000000000000, 0.000000000000000000 ) ) ;
#56850 = DIRECTION ( 'NONE',  ( 1.000000000000000000, 0.000000000000000000, 0.000000000000000000 ) ) ;
#56851 = VECTOR ( 'NONE', #39015, 1000.000000000000000 ) ;
#56852 = CARTESIAN_POINT ( 'NONE',  ( 12.49999999999999645, 1.530808498934191127E-15, -56.19999999999998863 ) ) ;
#56853 = VERTEX_POINT ( 'NONE', #61732 ) ;
#56854 = FACE_OUTER_BOUND ( 'NONE', #68904, .T. ) ;
#56855 = CARTESIAN_POINT ( 'NONE',  ( 97.64999999999999147, -209.9999999999999716, 90.00000000000000000 ) ) ;
#56856 = EDGE_LOOP ( 'NONE', ( #27143, #66403 ) ) ;
#56857 = EDGE_CURVE ( 'NONE', #60516, #57603, #16072, .T. ) ;
#56858 = CIRCLE ( 'NONE', #36448, 31.99999999999997868 ) ;
#56859 = FACE_OUTER_BOUND ( 'NONE', #10993, .T. ) ;
#56860 = LINE ( 'NONE', #45591, #63465 ) ;
#56861 = VECTOR ( 'NONE', #70307, 1000.000000000000000 ) ;
#56862 = EDGE_LOOP ( 'NONE', ( #5220, #42178, #10041, #66615 ) ) ;
#56863 = PRODUCT_DEFINITION ( 'UNKNOWN', '', #12394, #70960 ) ;
#56864 = ADVANCED_FACE ( 'NONE', ( #15864 ), #9849, .F. ) ;
#56865 = FACE_OUTER_BOUND ( 'NONE', #39960, .T. ) ;
#56866 = ORIENTED_EDGE ( 'NONE', *, *, #6461, .T. ) ;
#56867 = CIRCLE ( 'NONE', #41243, 31.99999999999998934 ) ;
#56868 = CARTESIAN_POINT ( 'NONE',  ( -97.64999999996706492, -209.9999916046304520, 84.99910573338409847 ) ) ;
#56869 = ORIENTED_EDGE ( 'NONE', *, *, #16274, .T. ) ;
#56870 = AXIS2_PLACEMENT_3D ( 'NONE', #64323, #25205, #71047 ) ;
#56871 = CIRCLE ( 'NONE', #48427, 77.49900000000000944 ) ;
#56872 = ORIENTED_EDGE ( 'NONE', *, *, #27689, .F. ) ;
#56873 = EDGE_CURVE ( 'NONE', #73588, #21230, #27121, .T. ) ;
#56874 = ORIENTED_EDGE ( 'NONE', *, *, #4066, .F. ) ;
#56875 = ORIENTED_EDGE ( 'NONE', *, *, #2540, .F. ) ;
#56876 = CARTESIAN_POINT ( 'NONE',  ( 0.000000000000000000, 51.02545421589402252, -55.20638768913705263 ) ) ;
#56877 = ADVANCED_FACE ( 'NONE', ( #33137 ), #11684, .F. ) ;
#56878 = VERTEX_POINT ( 'NONE', #63597 ) ;
#56879 = ORIENTED_EDGE ( 'NONE', *, *, #16519, .F. ) ;
#56880 = CARTESIAN_POINT ( 'NONE',  ( 97.64999999999997726, 88.47002178664753558, 89.62958333333332916 ) ) ;
#56881 = DIRECTION ( 'NONE',  ( 1.000000000000000000, -0.000000000000000000, -0.000000000000000000 ) ) ;
#56882 = EDGE_CURVE ( 'NONE', #61291, #66432, #38890, .T. ) ;
#56883 = CARTESIAN_POINT ( 'NONE',  ( 0.000000000000000000, -81.34940948281328588, -10.30890764327469711 ) ) ;
#56884 = VERTEX_POINT ( 'NONE', #57943 ) ;
#56885 = AXIS2_PLACEMENT_3D ( 'NONE', #63111, #4475, #28871 ) ;
#56886 = VERTEX_POINT ( 'NONE', #12071 ) ;
#56887 = EDGE_LOOP ( 'NONE', ( #254, #50646, #72129, #61891 ) ) ;
#56888 = CARTESIAN_POINT ( 'NONE',  ( 92.69370383062498320, 90.00000000000002842, 84.56281250086713897 ) ) ;
#56889 = ORIENTED_EDGE ( 'NONE', *, *, #7331, .T. ) ;
#56890 = CARTESIAN_POINT ( 'NONE',  ( 95.00000000000000000, -207.3369185715606307, 85.67406250086715147 ) ) ;
#56891 = SHAPE_DEFINITION_REPRESENTATION ( #21154, #23457 ) ;
#56892 = DIRECTION ( 'NONE',  ( 1.000000000000000000, 0.000000000000000000, 0.000000000000000000 ) ) ;
#56893 = CARTESIAN_POINT ( 'NONE',  ( 92.34999999999999432, 90.00000000000002842, 75.39499999999999602 ) ) ;
#56894 = CARTESIAN_POINT ( 'NONE',  ( -97.65000000000001990, 91.52997821335253548, 77.96145833506763267 ) ) ;
#56895 = PLANE ( 'NONE',  #46396 ) ;
#56896 = DIRECTION ( 'NONE',  ( -1.000000000000000000, -0.000000000000000000, -0.000000000000000000 ) ) ;
#56897 = DIRECTION ( 'NONE',  ( 0.000000000000000000, 0.000000000000000000, 1.000000000000000000 ) ) ;
#56898 = CARTESIAN_POINT ( 'NONE',  ( -92.69370383062498320, -208.6684592857803011, 86.20322916753382003 ) ) ;
#56899 = EDGE_CURVE ( 'NONE', #36914, #3905, #2904, .T. ) ;
#56900 = CARTESIAN_POINT ( 'NONE',  ( -92.69370383062502583, 88.66845928578038638, 86.25614583420048120 ) ) ;
#56901 = EDGE_CURVE ( 'NONE', #20649, #16746, #1739, .T. ) ;
#56902 = ORIENTED_EDGE ( 'NONE', *, *, #70230, .F. ) ;
#56903 = AXIS2_PLACEMENT_3D ( 'NONE', #58731, #54565, #2732 ) ;
#56905 = CARTESIAN_POINT ( 'NONE',  ( -96.15314808468751551, 88.00268892867056536, 84.03364583420047040 ) ) ;
#56904 = CARTESIAN_POINT ( 'NONE',  ( 96.15314808468748708, 88.00268892867053694, 82.86947916753379673 ) ) ;
#56906 = VERTEX_POINT ( 'NONE', #52293 ) ;
#56907 = CARTESIAN_POINT ( 'NONE',  ( 11.99999999999999822, -76.69515212746036070, 29.01471420065536932 ) ) ;
#56908 = CARTESIAN_POINT ( 'NONE',  ( -97.64999999999996305, -209.9999844236418198, 80.55437446300184945 ) ) ;
#56909 = CARTESIAN_POINT ( 'NONE',  ( 11.99999999999999822, 62.50329211542435104, 41.76937507738811917 ) ) ;
#56910 = CARTESIAN_POINT ( 'NONE',  ( -20.63749999999999574, -2.946905753440916183E-14, -1.643265707205091412E-14 ) ) ;
#56911 = CARTESIAN_POINT ( 'NONE',  ( -92.69370383062498320, -211.3315407142195852, 89.27239583420048064 ) ) ;
#56912 = CARTESIAN_POINT ( 'NONE',  ( -97.64999999999992042, -211.5299782133524218, 81.79791666666665151 ) ) ;
#56913 = DIRECTION ( 'NONE',  ( 0.000000000000000000, 0.000000000000000000, -1.000000000000000000 ) ) ;
#56914 = FACE_OUTER_BOUND ( 'NONE', #29894, .T. ) ;
#56915 = CARTESIAN_POINT ( 'NONE',  ( 92.35000000000003695, 88.47002178664747873, 89.41791666666667027 ) ) ;
#56916 = VERTEX_POINT ( 'NONE', #56836 ) ;
#56917 = AXIS2_PLACEMENT_3D ( 'NONE', #6395, #36057, #57898 ) ;
#56918 = ORIENTED_EDGE ( 'NONE', *, *, #47630, .F. ) ;
#56919 = CARTESIAN_POINT ( 'NONE',  ( -97.65000000000001990, 90.00000000000004263, 79.20499999999999829 ) ) ;
#56920 = CYLINDRICAL_SURFACE ( 'NONE', #69160, 2.649999999999985700 ) ;
#56921 = CARTESIAN_POINT ( 'NONE',  ( 1.250000000000000444, -16.78109714094927085, -1.199999999999999956 ) ) ;
#56922 = CARTESIAN_POINT ( 'NONE',  ( 0.000000000000000000, 2.663952781846728790, -41.91543099594814947 ) ) ;
#56923 = CARTESIAN_POINT ( 'NONE',  ( -97.64999999999996305, -209.9999999999999716, 90.00000000000000000 ) ) ;
#56924 = DIRECTION ( 'NONE',  ( -0.000000000000000000, -0.000000000000000000, 1.000000000000000000 ) ) ;
#56925 = AXIS2_PLACEMENT_3D ( 'NONE', #34956, #34210, #6393 ) ;
#56926 =( BOUNDED_CURVE ( )  B_SPLINE_CURVE ( 2, ( #5334, #28232, #6077, #50794, #57569, #18080, #51167 ),
 .UNSPECIFIED., .F., .F. ) 
 B_SPLINE_CURVE_WITH_KNOTS ( ( 3, 2, 2, 3 ),
 ( 0.8749999999999997780, 0.8819444444444441977, 0.8888888888888886175, 0.8958333333333331483 ),
 .UNSPECIFIED. ) 
 CURVE ( )  GEOMETRIC_REPRESENTATION_ITEM ( )  RATIONAL_B_SPLINE_CURVE ( ( 1.000000000000004219, 0.8660254037844343777, 1.000000000000000000, 0.8660254037844387076, 1.000000000000000000, 0.8660254037844430375, 0.9999999999999956701 ) ) 
 REPRESENTATION_ITEM ( '' )  );
#56927 = CARTESIAN_POINT ( 'NONE',  ( 11.99999999999999822, 0.000000000000000000, 0.000000000000000000 ) ) ;
#56928 = AXIS2_PLACEMENT_3D ( 'NONE', #50917, #67471, #74218 ) ;
#56929 = VERTEX_POINT ( 'NONE', #52662 ) ;
#56930 = CARTESIAN_POINT ( 'NONE',  ( -93.84685191531252713, 88.00268892867056536, 79.05947916753380866 ) ) ;
#56931 = CARTESIAN_POINT ( 'NONE',  ( -100.0000000000260485, 95.00000000000001421, 75.00000000000001421 ) ) ;
#56932 = CIRCLE ( 'NONE', #24491, 16.00000000000000000 ) ;
#56933 = AXIS2_PLACEMENT_3D ( 'NONE', #15111, #38050, #3861 ) ;
#56934 = DIRECTION ( 'NONE',  ( 0.000000000000000000, 0.000000000000000000, 1.000000000000000000 ) ) ;
#56935 = DIRECTION ( 'NONE',  ( -1.000000000000000000, 0.000000000000000000, -0.000000000000000000 ) ) ;
#56936 = CARTESIAN_POINT ( 'NONE',  ( 11.99999999999999822, -2.956366410620109519, -75.11725578898472122 ) ) ;
#56937 = FACE_OUTER_BOUND ( 'NONE', #69718, .T. ) ;
#56938 = DIRECTION ( 'NONE',  ( 1.000000000000000000, 0.000000000000000000, 0.000000000000000000 ) ) ;
#56939 = CARTESIAN_POINT ( 'NONE',  ( 94.99999999999998579, 92.66308142843932671, 78.21281250086717307 ) ) ;
#56940 = EDGE_CURVE ( 'NONE', #3129, #28069, #43727, .T. ) ;
#56941 = CARTESIAN_POINT ( 'NONE',  ( -93.84685191531247028, -211.9973110713294489, 78.58322916753382970 ) ) ;
#56942 = CARTESIAN_POINT ( 'NONE',  ( 16.30584220631899228, -140.9432449716519784, 5.500000000000000000 ) ) ;
#56943 = ORIENTED_EDGE ( 'NONE', *, *, #42262, .F. ) ;
#56944 = CARTESIAN_POINT ( 'NONE',  ( 0.000000000000000000, 41.76106447765580043, -62.50884508063379741 ) ) ;
#56945 = CARTESIAN_POINT ( 'NONE',  ( -93.67499999999998295, -212.2949673200287179, 75.60666666666665492 ) ) ;
#56946 = DIRECTION ( 'NONE',  ( -0.000000000000000000, -0.000000000000000000, -1.000000000000000000 ) ) ;
#56947 = EDGE_CURVE ( 'NONE', #68345, #65774, #50526, .T. ) ;
#56948 = CARTESIAN_POINT ( 'NONE',  ( -92.69370383062504004, 90.00000000000004263, 77.41906250086715602 ) ) ;
#56949 = CARTESIAN_POINT ( 'NONE',  ( 92.69370383062501162, -208.6684592857803011, 79.42989583420046529 ) ) ;
#56950 = VERTEX_POINT ( 'NONE', #58307 ) ;
#56951 = EDGE_CURVE ( 'NONE', #70850, #29463, #71273, .T. ) ;
#56952 = VECTOR ( 'NONE', #16407, 1000.000000000000000 ) ;
#56953 = DIRECTION ( 'NONE',  ( -1.000000000000000000, -0.000000000000000000, 0.000000000000000000 ) ) ;
#56954 = EDGE_LOOP ( 'NONE', ( #10020, #18651, #49444, #11885 ) ) ;
#56955 = CARTESIAN_POINT ( 'NONE',  ( -97.64999999999996305, -209.9999999999999716, 88.17437500173430465 ) ) ;
#56956 = EDGE_LOOP ( 'NONE', ( #67296, #67628, #14101, #32885 ) ) ;
#56957 = AXIS2_PLACEMENT_3D ( 'NONE', #53872, #25308, #2041 ) ;
#56958 = EDGE_CURVE ( 'NONE', #22660, #48200, #5343, .T. ) ;
#56959 = CARTESIAN_POINT ( 'NONE',  ( 97.64999999999999147, 89.99999989488613039, 86.58687499784845443 ) ) ;
#56960 = AXIS2_PLACEMENT_3D ( 'NONE', #53268, #47623, #35596 ) ;
#56961 = VERTEX_POINT ( 'NONE', #35010 ) ;
#56962 = ORIENTED_EDGE ( 'NONE', *, *, #26389, .T. ) ;
#56963 = ORIENTED_EDGE ( 'NONE', *, *, #37207, .F. ) ;
#56964 = CARTESIAN_POINT ( 'NONE',  ( 95.00000000000000000, -207.3369185715606307, 75.03781250086714749 ) ) ;
#56965 = ORIENTED_EDGE ( 'NONE', *, *, #1428, .F. ) ;
#56966 = LINE ( 'NONE', #73492, #23213 ) ;
#56967 = CARTESIAN_POINT ( 'NONE',  ( 0.000000000000000000, 16.00000000000000000, 2.500000000000000000 ) ) ;
#56968 = CARTESIAN_POINT ( 'NONE',  ( 94.99999999999998579, 87.33691857156068750, 82.97531250086716170 ) ) ;
#56969 = AXIS2_PLACEMENT_3D ( 'NONE', #36581, #19655, #59529 ) ;
#56970 = ADVANCED_FACE ( 'NONE', ( #51921 ), #17342, .F. ) ;
#56971 = CARTESIAN_POINT ( 'NONE',  ( 96.32499999999998863, -207.7050326799711968, 78.35833333333333428 ) ) ;
#56972 = ORIENTED_EDGE ( 'NONE', *, *, #1312, .F. ) ;
#56973 = ORIENTED_EDGE ( 'NONE', *, *, #18562, .F. ) ;
#56974 = ORIENTED_EDGE ( 'NONE', *, *, #61650, .T. ) ;
#56975 = AXIS2_PLACEMENT_3D ( 'NONE', #71514, #53867, #37332 ) ;
#56976 = VERTEX_POINT ( 'NONE', #34258 ) ;
#56977 = CARTESIAN_POINT ( 'NONE',  ( -11.59517495878806947, -96.12423995607481686, 5.500000000000000000 ) ) ;
#56978 = AXIS2_PLACEMENT_3D ( 'NONE', #23926, #7375, #9592 ) ;
#56979 = CARTESIAN_POINT ( 'NONE',  ( 10.00000000000000000, 67.80270845531889279, 46.11716303203210998 ) ) ;
#56980 = CARTESIAN_POINT ( 'NONE',  ( -20.63750000000001350, -2.447635064697195611E-13, -20.20000000000038298 ) ) ;
#56981 = DIRECTION ( 'NONE',  ( 0.000000000000000000, 0.07845909572783793529, 0.9969173337331285190 ) ) ;
#56982 = VECTOR ( 'NONE', #67738, 1000.000000000000000 ) ;
#56983 = CARTESIAN_POINT ( 'NONE',  ( 10.00000000000000000, 27.05870788708267582, -26.08949754952995903 ) ) ;
#56984 = CARTESIAN_POINT ( 'NONE',  ( 93.67499999999999716, 87.70503267997126784, 83.83520833506763381 ) ) ;
#56985 = ORIENTED_EDGE ( 'NONE', *, *, #63237, .F. ) ;
#56986 = CARTESIAN_POINT ( 'NONE',  ( -94.99999999999997158, -213.0599564267049857, 83.88812500173429498 ) ) ;
#56988 = ORIENTED_EDGE ( 'NONE', *, *, #71030, .F. ) ;
#56987 = EDGE_CURVE ( 'NONE', #2356, #67569, #42417, .T. ) ;
#56989 = CARTESIAN_POINT ( 'NONE',  ( 11.99999999999999822, 41.76937507738875155, -62.50329211542393892 ) ) ;
#56990 = EDGE_CURVE ( 'NONE', #19782, #54634, #40277, .T. ) ;
#56991 = ORIENTED_EDGE ( 'NONE', *, *, #10429, .T. ) ;
#56993 = CARTESIAN_POINT ( 'NONE',  ( -92.35000000000005116, 91.52997821335253548, 79.01979166840095559 ) ) ;
#56992 = CARTESIAN_POINT ( 'NONE',  ( 96.32499999999997442, 92.29496732002878900, 80.34270833506762699 ) ) ;
#56995 = ADVANCED_FACE ( 'NONE', ( #45565 ), #57580, .T. ) ;
#56994 = ORIENTED_EDGE ( 'NONE', *, *, #3592, .T. ) ;
#56996 = CARTESIAN_POINT ( 'NONE',  ( 93.84685191531248449, 88.00268892867053694, 84.82739583420048746 ) ) ;
#56997 = CARTESIAN_POINT ( 'NONE',  ( 0.000000000000000000, 0.000000000000000000, -1.199999999999999956 ) ) ;
#56998 = CARTESIAN_POINT ( 'NONE',  ( 0.000000000000000000, 0.000000000000000000, 0.000000000000000000 ) ) ;
#56999 = AXIS2_PLACEMENT_3D ( 'NONE', #36721, #70182, #2567 ) ;
#57000 = DIRECTION ( 'NONE',  ( -1.000000000000000000, 0.000000000000000000, 0.000000000000000000 ) ) ;
#57001 = CARTESIAN_POINT ( 'NONE',  ( 0.000000000000000000, -3.925862922255855647, -41.81611651403866858 ) ) ;
#57002 = CARTESIAN_POINT ( 'NONE',  ( 10.00000000000000000, -5.202137450156129717, -37.22597642581163768 ) ) ;
#57003 = ORIENTED_EDGE ( 'NONE', *, *, #21732, .F. ) ;
#57004 = DIRECTION ( 'NONE',  ( -8.332732854036912157E-16, -1.065814103640131031E-14, -1.000000000000000000 ) ) ;
#57005 = CARTESIAN_POINT ( 'NONE',  ( 10.00000000000000000, 5.256550761632864166, 77.32052557432842832 ) ) ;
#57006 = DIRECTION ( 'NONE',  ( 0.000000000000000000, 0.000000000000000000, 1.000000000000000000 ) ) ;
#57007 = ORIENTED_EDGE ( 'NONE', *, *, #28444, .F. ) ;
#57008 = EDGE_LOOP ( 'NONE', ( #17838, #3252, #3506, #42604, #5341 ) ) ;
#57009 = CYLINDRICAL_SURFACE ( 'NONE', #27597, 16.00000000000000000 ) ;
#57010 = DIRECTION ( 'NONE',  ( -0.000000000000000000, -0.000000000000000000, 1.000000000000000000 ) ) ;
#57011 = CARTESIAN_POINT ( 'NONE',  ( 23.49916127795269460, -121.5130826919798039, 2.500000000000000000 ) ) ;
#57012 = CARTESIAN_POINT ( 'NONE',  ( -97.30629616937495996, -209.9999999999999716, 81.54656250086715374 ) ) ;
#57013 = ORIENTED_EDGE ( 'NONE', *, *, #59794, .T. ) ;
#57014 = ORIENTED_EDGE ( 'NONE', *, *, #42369, .T. ) ;
#57015 = DIRECTION ( 'NONE',  ( -0.000000000000000000, -0.000000000000000000, 1.000000000000000000 ) ) ;
#57016 = AXIS2_PLACEMENT_3D ( 'NONE', #29212, #13407, #29952 ) ;
#57017 = CARTESIAN_POINT ( 'NONE',  ( -95.12556226663647863, -212.6467947905573510, 74.99648857272255498 ) ) ;
#57018 = FILL_AREA_STYLE_COLOUR ( '', #42964 ) ;
#57019 = CARTESIAN_POINT ( 'NONE',  ( 10.00000000000000000, 22.90783923731741112, -78.73519480814930205 ) ) ;
#57020 = CARTESIAN_POINT ( 'NONE',  ( 92.35000000000000853, -209.9999999999999716, 83.01499999999998636 ) ) ;
#57021 = DIRECTION ( 'NONE',  ( -0.000000000000000000, -0.000000000000000000, -1.000000000000000000 ) ) ;
#57022 = DIRECTION ( 'NONE',  ( -0.9580045777625452175, -0.2867529058022035837, 0.000000000000000000 ) ) ;
#57023 = DIRECTION ( 'NONE',  ( 0.8541291221503275466, -0.5200609990132993854, 0.000000000000000000 ) ) ;
#57024 = DIRECTION ( 'NONE',  ( 0.000000000000000000, 0.000000000000000000, 1.000000000000000000 ) ) ;
#57025 = DIRECTION ( 'NONE',  ( 0.000000000000000000, 0.000000000000000000, 1.000000000000000000 ) ) ;
#57026 = AXIS2_PLACEMENT_3D ( 'NONE', #15036, #72900, #21790 ) ;
#57027 = AXIS2_PLACEMENT_3D ( 'NONE', #58733, #47812, #53091 ) ;
#57028 = CARTESIAN_POINT ( 'NONE',  ( 93.84685191531248449, 88.00268892867053694, 86.73239583420048859 ) ) ;
#57029 = CARTESIAN_POINT ( 'NONE',  ( -97.30629616937497417, -211.3315407142195852, 89.21947916753381946 ) ) ;
#57030 = LINE ( 'NONE', #28439, #18181 ) ;
#57032 = ADVANCED_FACE ( 'NONE', ( #62866 ), #63224, .T. ) ;
#57031 = ORIENTED_EDGE ( 'NONE', *, *, #74193, .T. ) ;
#57033 = DIRECTION ( 'NONE',  ( 1.000000000000000000, -0.000000000000000000, 0.000000000000000000 ) ) ;
#57034 = CARTESIAN_POINT ( 'NONE',  ( -96.15314808468751551, 88.00268892867056536, 78.31864583420048120 ) ) ;
#57035 = VECTOR ( 'NONE', #4618, 1000.000000000000000 ) ;
#57036 = EDGE_CURVE ( 'NONE', #2268, #15264, #69222, .T. ) ;
#57037 = CARTESIAN_POINT ( 'NONE',  ( 95.00000000000000000, -212.6630814284392557, 89.16656250086712987 ) ) ;
#57038 = ADVANCED_FACE ( 'NONE', ( #41385 ), #19187, .T. ) ;
#57039 = ORIENTED_EDGE ( 'NONE', *, *, #16116, .T. ) ;
#57040 = CARTESIAN_POINT ( 'NONE',  ( 15.00000000000000000, 9.615535125378766423, -24.73947219025917121 ) ) ;
#57041 = DIRECTION ( 'NONE',  ( -0.000000000000000000, 0.7431448254773945772, 0.6691306063588579045 ) ) ;
#57042 = DIRECTION ( 'NONE',  ( -1.000000000000000000, 0.000000000000000000, 0.000000000000000000 ) ) ;
#57043 = CIRCLE ( 'NONE', #72621, 31.99999999999998579 ) ;
#57044 = EDGE_CURVE ( 'NONE', #54476, #40343, #30458, .T. ) ;
#57045 = DIRECTION ( 'NONE',  ( -1.000000000000000000, -0.000000000000000000, 0.000000000000000000 ) ) ;
#57046 = DIRECTION ( 'NONE',  ( -1.000000000000000000, 0.000000000000000000, 0.000000000000000000 ) ) ;
#57047 = VECTOR ( 'NONE', #28334, 1000.000000000000000 ) ;
#57048 = VERTEX_POINT ( 'NONE', #30827 ) ;
#57050 = ORIENTED_EDGE ( 'NONE', *, *, #68771, .T. ) ;
#57049 =( BOUNDED_CURVE ( )  B_SPLINE_CURVE ( 2, ( #33039, #48852, #72152, #15011, #67270, #10116, #32667, #25924, #4134, #49589, #73265, #3035, #61630, #60528, #43247, #72517, #37952, #10486, #55980, #44720, #9006, #55612, #27397, #4499, #21378, #31930, #21769, #16134, #54869, #27025, #15379, #66531, #72877, #43611, #44338, #49224, #67638, #38323, #33403, #39071, #71772, #38698, #20279, #3762, #9371, #32292, #66170, #15762, #14643, #60889, #37590, #3389, #26289, #55240, #26660, #66888, #21017, #43970, #17983, #39819, #69133, #33795, #57475, #68762, #45466, #5989, #22523, #28896, #28148, #738, #17250, #40929, #52191, #57849, #11233, #17616, #73632, #57111, #62770, #34167, #63493, #34912, #63137, #39444, #45090, #46559, #68394, #16885, #10, #40545, #62388, #40186, #10871, #56746, #6350, #69485, #11588, #11969, #5614, #28513, #29250, #23628, #4884, #63865, #12337, #56368, #5248, #51450, #34527, #22904, #27784, #16502, #51085, #23266, #46197, #50709, #51828, #22148, #45840, #74009, #68010, #373, #35277, #24367, #19084, #35629, #2213, #7070, #13448, #64587, #54052, #25101, #70950, #2589, #25474, #29992, #53672, #65336, #6706, #41646, #52938, #24004, #41290, #31101, #24732, #19818, #52558, #1478, #70206, #70568, #47302, #18712, #48400, #18344, #42034, #1112, #42768, #8174, #7810, #64971, #30727, #13071, #48035, #42398, #36371, #58204, #59316, #7446, #71313, #29612, #19455, #64229, #46932, #30360, #36009, #58957, #13804, #58570, #36748, #53306, #65702, #69847, #1843, #47660, #59690, #12701, #15295, #55530, #31840, #21292, #26199, #4046, #60079, #9284, #66086, #25836, #43531, #10027, #49141, #38611, #26941, #49510, #49869, #72067, #20578, #72790, #26576, #8557, #61548, #55897, #37134, #32947, #14928, #32583, #43888, #44249, #43154, #48768, #31475, #66809, #4411, #9661, #67178, #66444, #14556, #15678, #32204, #55150, #54784, #27306, #50241, #73177, #21678, #3679, #38231, #44632, #37872, #54413, #60804, #72432, #20935, #14181, #2946, #71688, #61176, #60439, #20189, #37506, #8922, #3308, #62678, #68299, #51739, #17523, #40455, #34822, #44999, #67550, #5895, #57758, #11871, #645, #63400, #40093, #74299, #63048, #67925, #28428, #38983, #16795, #16041, #29162, #52103, #28056, #34074, #6263, #62291, #68674, #284, #22432, #28807, #46105, #23536 ),
 .UNSPECIFIED., .F., .F. ) 
 B_SPLINE_CURVE_WITH_KNOTS ( ( 3, 2, 2, 2, 2, 2, 2, 2, 2, 2, 2, 2, 2, 2, 2, 2, 2, 2, 2, 2, 2, 2, 2, 2, 2, 2, 2, 2, 2, 2, 2, 2, 2, 2, 2, 2, 2, 2, 2, 2, 2, 2, 2, 2, 2, 2, 2, 2, 2, 2, 2, 2, 2, 2, 2, 2, 2, 2, 2, 2, 2, 2, 2, 2, 2, 2, 2, 2, 2, 2, 2, 2, 2, 2, 2, 2, 2, 2, 2, 2, 2, 2, 2, 2, 2, 2, 2, 2, 2, 2, 2, 2, 2, 2, 2, 2, 2, 2, 2, 2, 2, 2, 2, 2, 2, 2, 2, 2, 2, 2, 2, 2, 2, 2, 2, 2, 2, 2, 2, 2, 2, 2, 2, 2, 2, 2, 2, 2, 2, 2, 2, 2, 2, 2, 2, 2, 2, 2, 2, 2, 2, 3 ),
 ( 0.000000000000000000, 0.007055765384978172905, 0.01411153076995634581, 0.02116729615493451871, 0.02822306153991269162, 0.03527882692489087146, 0.04233459230986903743, 0.04939035769484721727, 0.05644612307982538324, 0.06350188846480356308, 0.07055765384978174293, 0.07761341923475992277, 0.08466918461973807486, 0.09172495000471625470, 0.09878071538969443455, 0.1058364807746726005, 0.1128922461596507665, 0.1199480115446289463, 0.1270037769296071262, 0.1340595423145853060, 0.1411153076995634859, 0.1481710730845416657, 0.1552268384695198455, 0.1622826038544979699, 0.1693383692394761497, 0.1763941346244543296, 0.1834499000094325094, 0.1905056653944106893, 0.1975614307793888691, 0.2046171961643670212, 0.2116729615493452010, 0.2187287269343233809, 0.2257844923193015330, 0.2328402577042797128, 0.2398960230892578926, 0.2469517884742360447, 0.2540075538592142523, 0.2610633192441924044, 0.2681190846291706120, 0.2751748500141487086, 0.2822306153991269717, 0.2892863807841050683, 0.2963421461690833314, 0.3033979115540614280, 0.3104536769390396911, 0.3175094423240177877, 0.3245652077089959398, 0.3316209730939741473, 0.3386767384789522994, 0.3457325038639305070, 0.3527882692489086591, 0.3598440346338868112, 0.3668998000188650188, 0.3739555654038431709, 0.3810113307888213785, 0.3880670961737994751, 0.3951228615587777382, 0.4021786269437558348, 0.4092343923287340424, 0.4162901577137121945, 0.4233459230986904021, 0.4304016884836685541, 0.4374574538686467617, 0.4445132192536248583, 0.4515689846386030659, 0.4586247500235812180, 0.4656805154085594256, 0.4727362807935375777, 0.4797920461785157853, 0.4868478115634939374, 0.4939035769484720895, 0.5009593423334502971, 0.5080151077184285047, 0.5150708731034066012, 0.5221266384883848088, 0.5291824038733630164, 0.5362381692583412240, 0.5432939346433193206, 0.5503497000282974172, 0.5574054654132757358, 0.5644612307982539434, 0.5715169961832320400, 0.5785727615682101366, 0.5856285269531882332, 0.5926842923381666628, 0.5997400577231447594, 0.6067958231081228559, 0.6138515884931009525, 0.6209073538780793822, 0.6279631192630574787, 0.6350188846480355753, 0.6420746500330136719, 0.6491304154179918795, 0.6561861808029701981, 0.6632419461879482947, 0.6702977115729263913, 0.6773534769579045989, 0.6844092423428828065, 0.6914650077278610141, 0.6985207731128391107, 0.7055765384978173183, 0.7126323038827954148, 0.7196880692677736224, 0.7267438346527518300, 0.7337996000377300376, 0.7408553654227081342, 0.7479111308076863418, 0.7549668961926644384, 0.7620226615776427570, 0.7690784269626208536, 0.7761341923475989502, 0.7831899577325772688, 0.7902457231175554764, 0.7973014885025335730, 0.8043572538875116695, 0.8114130192724899882, 0.8184687846574680847, 0.8255245500424462923, 0.8325803154274243889, 0.8396360808124025965, 0.8466918461973808041, 0.8537476115823589007, 0.8608033769673371083, 0.8678591423523153159, 0.8749149077372935235, 0.8819706731222716201, 0.8890264385072497166, 0.8960822038922280353, 0.9031379692772061318, 0.9101937346621843394, 0.9172495000471624360, 0.9243052654321407546, 0.9313610308171188512, 0.9384167962020970588, 0.9454725615870751554, 0.9525283269720533630, 0.9595840923570315706, 0.9666398577420096672, 0.9736956231269878748, 0.9807513885119660824, 0.9878071538969441789, 0.9900635123082152100 ),
 .UNSPECIFIED. ) 
 CURVE ( )  GEOMETRIC_REPRESENTATION_ITEM ( )  RATIONAL_B_SPLINE_CURVE ( ( 1.000000000000000000, 0.8660254037844387076, 1.000000000000000000, 0.8660254037844387076, 1.000000000000000000, 0.8660254037844387076, 1.000000000000000000, 0.8660254037844387076, 1.000000000000000000, 0.8660254037844387076, 1.000000000000000000, 0.8660254037844387076, 1.000000000000000000, 0.8660254037844387076, 1.000000000000000000, 0.8660254037844387076, 1.000000000000000000, 0.8660254037844387076, 1.000000000000000000, 0.8660254037844387076, 1.000000000000000000, 0.8660254037844387076, 1.000000000000000000, 0.8660254037844387076, 1.000000000000000000, 0.8660254037844387076, 1.000000000000000000, 0.8660254037844387076, 1.000000000000000000, 0.8660254037844387076, 1.000000000000000000, 0.8660254037844387076, 1.000000000000000000, 0.8660254037844387076, 1.000000000000000000, 0.8660254037844387076, 1.000000000000000000, 0.8660254037844387076, 1.000000000000000000, 0.8660254037844387076, 1.000000000000000000, 0.8660254037844387076, 1.000000000000000000, 0.8660254037844387076, 1.000000000000000000, 0.8660254037844387076, 1.000000000000000000, 0.8660254037844387076, 1.000000000000000000, 0.8660254037844387076, 1.000000000000000000, 0.8660254037844387076, 1.000000000000000000, 0.8660254037844387076, 1.000000000000000000, 0.8660254037844387076, 1.000000000000000000, 0.8660254037844387076, 1.000000000000000000, 0.8660254037844387076, 1.000000000000000000, 0.8660254037844387076, 1.000000000000000000, 0.8660254037844387076, 1.000000000000000000, 0.8660254037844387076, 1.000000000000000000, 0.8660254037844387076, 1.000000000000000000, 0.8660254037844387076, 1.000000000000000000, 0.8660254037844387076, 1.000000000000000000, 0.8660254037844387076, 1.000000000000000000, 0.8660254037844387076, 1.000000000000000000, 0.8660254037844387076, 1.000000000000000000, 0.8660254037844387076, 1.000000000000000000, 0.8660254037844387076, 1.000000000000000000, 0.8660254037844387076, 1.000000000000000000, 0.8660254037844387076, 1.000000000000000000, 0.8660254037844387076, 1.000000000000000000, 0.8660254037844387076, 1.000000000000000000, 0.8660254037844387076, 1.000000000000000000, 0.8660254037844387076, 1.000000000000000000, 0.8660254037844387076, 1.000000000000000000, 0.8660254037844387076, 1.000000000000000000, 0.8660254037844387076, 1.000000000000000000, 0.8660254037844387076, 1.000000000000000000, 0.8660254037844387076, 1.000000000000000000, 0.8660254037844387076, 1.000000000000000000, 0.8660254037844387076, 1.000000000000000000, 0.8660254037844387076, 1.000000000000000000, 0.8660254037844387076, 1.000000000000000000, 0.8660254037844387076, 1.000000000000000000, 0.8660254037844387076, 1.000000000000000000, 0.8660254037844387076, 1.000000000000000000, 0.8660254037844387076, 1.000000000000000000, 0.8660254037844387076, 1.000000000000000000, 0.8660254037844387076, 1.000000000000000000, 0.8660254037844387076, 1.000000000000000000, 0.8660254037844387076, 1.000000000000000000, 0.8660254037844387076, 1.000000000000000000, 0.8660254037844387076, 1.000000000000000000, 0.8660254037844387076, 1.000000000000000000, 0.8660254037844387076, 1.000000000000000000, 0.8660254037844387076, 1.000000000000000000, 0.8660254037844387076, 1.000000000000000000, 0.8660254037844387076, 1.000000000000000000, 0.8660254037844387076, 1.000000000000000000, 0.8660254037844387076, 1.000000000000000000, 0.8660254037844387076, 1.000000000000000000, 0.8660254037844387076, 1.000000000000000000, 0.8660254037844387076, 1.000000000000000000, 0.8660254037844387076, 1.000000000000000000, 0.8660254037844387076, 1.000000000000000000, 0.8660254037844387076, 1.000000000000000000, 0.8660254037844387076, 1.000000000000000000, 0.8660254037844387076, 1.000000000000000000, 0.8660254037844387076, 1.000000000000000000, 0.8660254037844387076, 1.000000000000000000, 0.8660254037844387076, 1.000000000000000000, 0.8660254037844387076, 1.000000000000000000, 0.8660254037844387076, 1.000000000000000000, 0.8660254037844387076, 1.000000000000000000, 0.8660254037844387076, 1.000000000000000000, 0.8660254037844387076, 1.000000000000000000, 0.8660254037844387076, 1.000000000000000000, 0.8660254037844387076, 1.000000000000000000, 0.8660254037844387076, 1.000000000000000000, 0.8660254037844387076, 1.000000000000000000, 0.8660254037844387076, 1.000000000000000000, 0.8660254037844387076, 1.000000000000000000, 0.8660254037844387076, 1.000000000000000000, 0.8660254037844387076, 1.000000000000000000, 0.8660254037844387076, 1.000000000000000000, 0.8660254037844387076, 1.000000000000000000, 0.8660254037844387076, 1.000000000000000000, 0.8660254037844387076, 1.000000000000000000, 0.8660254037844387076, 1.000000000000000000, 0.8660254037844387076, 1.000000000000000000, 0.8660254037844387076, 1.000000000000000000, 0.8660254037844387076, 1.000000000000000000, 0.8660254037844387076, 1.000000000000000000, 0.8660254037844387076, 1.000000000000000000, 0.8660254037844387076, 1.000000000000000000, 0.8660254037844387076, 1.000000000000000000, 0.8660254037844387076, 1.000000000000000000, 0.8660254037844387076, 1.000000000000000000, 0.8660254037844387076, 1.000000000000000000, 0.8660254037844387076, 1.000000000000000000, 0.8660254037844387076, 1.000000000000000000, 0.8660254037844387076, 1.000000000000000000, 0.8660254037844387076, 1.000000000000000000, 0.8660254037844387076, 1.000000000000000000, 0.8660254037844387076, 1.000000000000000000, 0.8660254037844387076, 1.000000000000000000, 0.8660254037844387076, 1.000000000000000000, 0.8660254037844387076, 1.000000000000000000, 0.8660254037844387076, 1.000000000000000000, 0.8660254037844387076, 1.000000000000000000, 0.8660254037844387076, 1.000000000000000000, 0.8660254037844387076, 1.000000000000000000, 0.8660254037844387076, 1.000000000000000000, 0.8660254037844387076, 1.000000000000000000, 0.8660254037844387076, 1.000000000000000000, 0.8660254037844387076, 1.000000000000000000, 0.8660254037844387076, 1.000000000000000000, 0.8660254037844387076, 1.000000000000000000, 0.8660254037844387076, 1.000000000000000000, 0.8660254037844387076, 1.000000000000000000, 0.8660254037844387076, 1.000000000000000000, 0.8660254037844387076, 1.000000000000000000, 0.8660254037844387076, 1.000000000000000000, 0.8660254037844387076, 1.000000000000000000, 0.8660254037844387076, 1.000000000000000000, 0.8660254037844387076, 1.000000000000000000, 0.8660254037844387076, 1.000000000000000000, 0.9571563550410552290, 0.9417145902178747363 ) ) 
 REPRESENTATION_ITEM ( '' )  );
#57051 = CARTESIAN_POINT ( 'NONE',  ( 96.15314808468750130, -211.9973110713294489, 86.20322916753382003 ) ) ;
#57052 = CARTESIAN_POINT ( 'NONE',  ( 0.000000000000000000, 26.79245525562762253, -32.34446384429942611 ) ) ;
#57053 = ADVANCED_FACE ( 'NONE', ( #59796 ), #24829, .T. ) ;
#57054 = LINE ( 'NONE', #38645, #71162 ) ;
#57055 = DIRECTION ( 'NONE',  ( 3.061616997868383141E-16, 1.000000000000000000, -0.000000000000000000 ) ) ;
#57056 = CARTESIAN_POINT ( 'NONE',  ( 96.32499999999998863, -212.2949673200287179, 76.87666666666666515 ) ) ;
#57057 = EDGE_CURVE ( 'NONE', #55291, #50178, #7705, .T. ) ;
#57058 = LINE ( 'NONE', #29561, #36960 ) ;
#57059 = CARTESIAN_POINT ( 'NONE',  ( 92.35000000000002274, -208.4700217866474645, 88.67708333333332860 ) ) ;
#57060 = ORIENTED_EDGE ( 'NONE', *, *, #27160, .T. ) ;
#57061 = ORIENTED_EDGE ( 'NONE', *, *, #30308, .T. ) ;
#57062 = CARTESIAN_POINT ( 'NONE',  ( 12.50000000000000000, -132.5000000000000000, 2.500000000000000000 ) ) ;
#57063 = EDGE_LOOP ( 'NONE', ( #9047, #8986, #54650, #58931 ) ) ;
#57064 = VERTEX_POINT ( 'NONE', #31571 ) ;
#57065 = FACE_OUTER_BOUND ( 'NONE', #9965, .T. ) ;
#57066 = CIRCLE ( 'NONE', #45041, 31.99999999999999289 ) ;
#57067 = FILL_AREA_STYLE_COLOUR ( '', #25493 ) ;
#57068 = DIRECTION ( 'NONE',  ( -1.000000000000000000, -0.000000000000000000, 0.000000000000000000 ) ) ;
#57069 = DIRECTION ( 'NONE',  ( -1.000000000000000000, 0.000000000000000000, 0.000000000000000000 ) ) ;
#57070 = CARTESIAN_POINT ( 'NONE',  ( 93.67500000000001137, -212.2949673200287179, 77.48520833506763950 ) ) ;
#57071 = CARTESIAN_POINT ( 'NONE',  ( 93.67499999999999716, 87.70503267997126784, 80.58083333333331666 ) ) ;
#57072 = ORIENTED_EDGE ( 'NONE', *, *, #2745, .T. ) ;
#57073 = CYLINDRICAL_SURFACE ( 'NONE', #28740, 31.99999999999998579 ) ;
#57074 = ORIENTED_EDGE ( 'NONE', *, *, #33861, .T. ) ;
#57075 = EDGE_CURVE ( 'NONE', #21495, #72597, #49702, .T. ) ;
#57076 = CARTESIAN_POINT ( 'NONE',  ( 0.000000000000000000, 37.22597642581158084, 10.79786254984347593 ) ) ;
#57077 = EDGE_CURVE ( 'NONE', #20209, #14859, #71415, .T. ) ;
#57078 = ORIENTED_EDGE ( 'NONE', *, *, #18926, .T. ) ;
#57079 = CARTESIAN_POINT ( 'NONE',  ( -1.250000000000002442, -12.36245420541525242, 0.000000000000000000 ) ) ;
#57080 = CARTESIAN_POINT ( 'NONE',  ( -97.30629616937501680, 88.66845928578038638, 80.96447916753382401 ) ) ;
#57081 = CARTESIAN_POINT ( 'NONE',  ( 94.99999999999998579, 92.66308142843935514, 76.78406250086712248 ) ) ;
#57082 = VECTOR ( 'NONE', #11650, 1000.000000000000000 ) ;
#57083 = ORIENTED_EDGE ( 'NONE', *, *, #20042, .T. ) ;
#57084 = DIRECTION ( 'NONE',  ( -1.000000000000000000, 0.000000000000000000, 0.000000000000000000 ) ) ;
#57085 = DIRECTION ( 'NONE',  ( -1.000000000000000000, -0.000000000000000000, -0.000000000000000000 ) ) ;
#57086 = CARTESIAN_POINT ( 'NONE',  ( 92.35000000045006630, 89.99996890530464100, 88.81037122970248276 ) ) ;
#57087 = CARTESIAN_POINT ( 'NONE',  ( -93.67499999999998295, -207.7050326799711968, 77.72333333333332916 ) ) ;
#57088 = ORIENTED_EDGE ( 'NONE', *, *, #32652, .T. ) ;
#57089 = DIRECTION ( 'NONE',  ( -1.000000000000000000, 0.000000000000000000, -0.000000000000000000 ) ) ;
#57090 = AXIS2_PLACEMENT_3D ( 'NONE', #21697, #8945, #61937 ) ;
#57091 = CARTESIAN_POINT ( 'NONE',  ( -94.99999999999997158, -212.6630814284392557, 76.46656250086712703 ) ) ;
#57092 = ORIENTED_EDGE ( 'NONE', *, *, #27075, .F. ) ;
#57093 = VERTEX_POINT ( 'NONE', #25568 ) ;
#57095 = DIRECTION ( 'NONE',  ( -1.000000000000000000, -0.000000000000000000, -0.000000000000000000 ) ) ;
#57094 = AXIS2_PLACEMENT_3D ( 'NONE', #35544, #58116, #74294 ) ;
#57096 = ORIENTED_EDGE ( 'NONE', *, *, #57302, .F. ) ;
#57097 = CARTESIAN_POINT ( 'NONE',  ( 97.65000000000009095, 88.47002178664759242, 78.19958333333332234 ) ) ;
#57098 = APPLICATION_CONTEXT ( 'automotive_design' ) ;
#57099 = DIRECTION ( 'NONE',  ( -1.000000000000000000, -0.000000000000000000, -0.000000000000000000 ) ) ;
#57100 = VERTEX_POINT ( 'NONE', #54516 ) ;
#57101 = CARTESIAN_POINT ( 'NONE',  ( -94.99999999999997158, -207.3369185715606307, 75.51406250086714067 ) ) ;
#57102 = VERTEX_POINT ( 'NONE', #7177 ) ;
#57103 = CARTESIAN_POINT ( 'NONE',  ( -93.67499999999998295, -207.7050326799711968, 81.53333333333333144 ) ) ;
#57104 = DIRECTION ( 'NONE',  ( -1.000000000000000000, 0.000000000000000000, 0.000000000000000000 ) ) ;
#57105 = LINE ( 'NONE', #35902, #21308 ) ;
#57106 = DIRECTION ( 'NONE',  ( 0.000000000000000000, 0.000000000000000000, 1.000000000000000000 ) ) ;
#57107 = CIRCLE ( 'NONE', #69126, 16.00000000000000000 ) ;
#57108 = DIRECTION ( 'NONE',  ( -1.000000000000000000, 0.000000000000000000, 0.000000000000000000 ) ) ;
#57109 = CIRCLE ( 'NONE', #19886, 16.00000000000000000 ) ;
#57110 = CYLINDRICAL_SURFACE ( 'NONE', #60160, 37.49900000000000233 ) ;
#57111 = CARTESIAN_POINT ( 'NONE',  ( 97.30629616937498838, 91.33154071421968467, 85.56822916753380071 ) ) ;
#57112 = DIRECTION ( 'NONE',  ( -1.000000000000000000, 0.000000000000000000, 0.000000000000000000 ) ) ;
#57113 = CYLINDRICAL_SURFACE ( 'NONE', #70990, 31.99999999999999289 ) ;
#57114 = LINE ( 'NONE', #58574, #63686 ) ;
#57115 = DIRECTION ( 'NONE',  ( 0.000000000000000000, 0.000000000000000000, 1.000000000000000000 ) ) ;
#57116 = PLANE ( 'NONE',  #64437 ) ;
#57117 = CARTESIAN_POINT ( 'NONE',  ( -97.65000000000001990, 89.99997747860815878, 84.36437578067155130 ) ) ;
#57118 = CARTESIAN_POINT ( 'NONE',  ( -10.00000000000000000, 0.000000000000000000, 0.000000000000000000 ) ) ;
#57119 = DIRECTION ( 'NONE',  ( -1.000000000000000000, 0.000000000000000000, 0.000000000000000000 ) ) ;
#57120 = EDGE_CURVE ( 'NONE', #55748, #23136, #64125, .T. ) ;
#57121 = CYLINDRICAL_SURFACE ( 'NONE', #64989, 82.00000000000000000 ) ;
#57122 = CYLINDRICAL_SURFACE ( 'NONE', #18537, 82.00000000000000000 ) ;
#57123 = CARTESIAN_POINT ( 'NONE',  ( 10.00000000000000000, -34.94270380257586339, -74.18225833017926618 ) ) ;
#57124 = ADVANCED_FACE ( 'NONE', ( #53040 ), #2687, .T. ) ;
#57125 = CARTESIAN_POINT ( 'NONE',  ( -94.99999999999997158, -206.9400435732949575, 86.03125000000000000 ) ) ;
#57126 = EDGE_CURVE ( 'NONE', #8233, #69330, #41538, .T. ) ;
#57127 = CARTESIAN_POINT ( 'NONE',  ( 22.30499999999999972, 0.000000000000000000, 2.500000000000000444 ) ) ;
#57128 = ORIENTED_EDGE ( 'NONE', *, *, #7966, .T. ) ;
#57129 = DIRECTION ( 'NONE',  ( -1.000000000000000000, 0.000000000000000000, 0.000000000000000000 ) ) ;
#57130 = VECTOR ( 'NONE', #66696, 1000.000000000000000 ) ;
#57131 = CARTESIAN_POINT ( 'NONE',  ( 10.00000000000000000, 38.55633173627034438, -16.65560815589369881 ) ) ;
#57132 = LINE ( 'NONE', #45112, #16625 ) ;
#57133 = DIRECTION ( 'NONE',  ( 0.000000000000000000, -1.000000000000000000, -1.040834085586084257E-14 ) ) ;
#57134 = EDGE_CURVE ( 'NONE', #45883, #719, #17307, .T. ) ;
#57135 = VECTOR ( 'NONE', #39225, 1000.000000000000000 ) ;
#57136 = CARTESIAN_POINT ( 'NONE',  ( 95.00000000000000000, -207.3369185715606307, 87.10281250086715943 ) ) ;
#57137 = AXIS2_PLACEMENT_3D ( 'NONE', #57599, #74128, #63615 ) ;
#57138 = ORIENTED_EDGE ( 'NONE', *, *, #66560, .F. ) ;
#57139 = ORIENTED_EDGE ( 'NONE', *, *, #52186, .T. ) ;
#57140 = CARTESIAN_POINT ( 'NONE',  ( 10.00000000000000000, -74.65491531819124305, 8.830959090342128448 ) ) ;
#57141 = ORIENTED_EDGE ( 'NONE', *, *, #28336, .F. ) ;
#57142 = AXIS2_PLACEMENT_3D ( 'NONE', #3944, #31740, #2847 ) ;
#57143 = ADVANCED_FACE ( 'NONE', ( #25935 ), #19552, .F. ) ;
#57144 = LINE ( 'NONE', #22181, #42704 ) ;
#57145 = VECTOR ( 'NONE', #52364, 1000.000000000000000 ) ;
#57146 =( BOUNDED_CURVE ( )  B_SPLINE_CURVE ( 2, ( #19003, #65629, #25401, #48328, #24296, #71237, #14100 ),
 .UNSPECIFIED., .F., .F. ) 
 B_SPLINE_CURVE_WITH_KNOTS ( ( 3, 2, 2, 3 ),
 ( 0.3598440426530883918, 0.3668998081258832422, 0.3739555736667655728, 0.3810111478265176821 ),
 .UNSPECIFIED. ) 
 CURVE ( )  GEOMETRIC_REPRESENTATION_ITEM ( )  RATIONAL_B_SPLINE_CURVE ( ( 1.000000000000000000, 0.8660254037844387076, 1.000000000000000000, 0.8660254037844387076, 1.000000000000000000, 0.8660290377217475521, 0.9999927323225166198 ) ) 
 REPRESENTATION_ITEM ( '' )  );
#57147 = CARTESIAN_POINT ( 'NONE',  ( 97.30629616937498838, -208.6684592857803295, 79.85322916753379729 ) ) ;
#57149 = ORIENTED_EDGE ( 'NONE', *, *, #71955, .T. ) ;
#57148 = EDGE_CURVE ( 'NONE', #15614, #9567, #26899, .T. ) ;
#57150 = CARTESIAN_POINT ( 'NONE',  ( 95.00000000000000000, -207.3369185715606307, 82.02281250086714692 ) ) ;
#57151 = VERTEX_POINT ( 'NONE', #64690 ) ;
#57152 = CARTESIAN_POINT ( 'NONE',  ( 92.35001798596591982, 91.52998859755481931, 80.50145761676020584 ) ) ;
#57153 = ORIENTED_EDGE ( 'NONE', *, *, #7060, .F. ) ;
#57154 = ADVANCED_FACE ( 'NONE', ( #36111 ), #7546, .F. ) ;
#57155 = EDGE_CURVE ( 'NONE', #63633, #8129, #13544, .T. ) ;
#57156 = EDGE_LOOP ( 'NONE', ( #70280, #59536, #35945, #20324 ) ) ;
#57157 = CIRCLE ( 'NONE', #24730, 3.299999999999969624 ) ;
#57158 = CARTESIAN_POINT ( 'NONE',  ( 0.000000000000000000, -120.0000000000000000, 2.500000000000000000 ) ) ;
#57159 = ORIENTED_EDGE ( 'NONE', *, *, #1906, .T. ) ;
#57160 = DIRECTION ( 'NONE',  ( 0.000000000000000000, 0.8526401643540936215, -0.5224985647159469115 ) ) ;
#57161 = CARTESIAN_POINT ( 'NONE',  ( 97.64999999999999147, -209.9999999999999716, 87.85687500173429498 ) ) ;
#57162 = ORIENTED_EDGE ( 'NONE', *, *, #29262, .T. ) ;
#57163 = CARTESIAN_POINT ( 'NONE',  ( -7.572224309238338336, -145.4393675041377492, 5.500000000000000000 ) ) ;
#57164 = EDGE_CURVE ( 'NONE', #32709, #57704, #20296, .T. ) ;
#57165 = ORIENTED_EDGE ( 'NONE', *, *, #57673, .F. ) ;
#57166 = CARTESIAN_POINT ( 'NONE',  ( 5.000000000000000000, 44.99326035066149387, -68.55367621811095091 ) ) ;
#57167 = VERTEX_POINT ( 'NONE', #67654 ) ;
#57168 = ADVANCED_FACE ( 'NONE', ( #55993 ), #56384, .F. ) ;
#57169 = ORIENTED_EDGE ( 'NONE', *, *, #69406, .F. ) ;
#57170 = VERTEX_POINT ( 'NONE', #66901 ) ;
#57171 = DIRECTION ( 'NONE',  ( -1.000000000000000000, -0.000000000000000000, -0.000000000000000000 ) ) ;
#57172 = CARTESIAN_POINT ( 'NONE',  ( -5.000000000000000000, -1.472375319565265794, -0.9369361380397573935 ) ) ;
#57173 = ORIENTED_EDGE ( 'NONE', *, *, #38648, .T. ) ;
#57174 = ORIENTED_EDGE ( 'NONE', *, *, #23402, .F. ) ;
#57175 = ORIENTED_EDGE ( 'NONE', *, *, #13388, .F. ) ;
#57176 = CARTESIAN_POINT ( 'NONE',  ( 11.99999999999999822, 0.000000000000000000, 0.000000000000000000 ) ) ;
#57177 = CYLINDRICAL_SURFACE ( 'NONE', #40944, 16.00000000000000000 ) ;
#57178 = CARTESIAN_POINT ( 'NONE',  ( -96.32500000000001705, 92.29496732002878900, 87.98916666666666231 ) ) ;
#57179 = VERTEX_POINT ( 'NONE', #66545 ) ;
#57180 = CARTESIAN_POINT ( 'NONE',  ( 96.15314808468748708, 91.99731107132950569, 75.46114583420047950 ) ) ;
#57181 = EDGE_LOOP ( 'NONE', ( #62538, #2366, #42314, #21481 ) ) ;
#57182 = CARTESIAN_POINT ( 'NONE',  ( 0.000000000000000000, 33.79645857604513992, -16.45098606841138178 ) ) ;
#57183 = CARTESIAN_POINT ( 'NONE',  ( -92.69370383062498320, -208.6684592857803011, 87.47322916753381605 ) ) ;
#57184 = ORIENTED_EDGE ( 'NONE', *, *, #62568, .F. ) ;
#57185 = CARTESIAN_POINT ( 'NONE',  ( 0.000000000000000000, 0.000000000000000000, 0.000000000000000000 ) ) ;
#57186 = CARTESIAN_POINT ( 'NONE',  ( 92.98340954502104694, -211.6055158133078749, 74.95309847082319266 ) ) ;
#57187 = CARTESIAN_POINT ( 'NONE',  ( -10.00000000000000000, 0.000000000000000000, 0.000000000000000000 ) ) ;
#57188 = CARTESIAN_POINT ( 'NONE',  ( -96.15314808468747287, -208.0026889286704943, 76.83697916753381207 ) ) ;
#57189 = DIRECTION ( 'NONE',  ( 0.000000000000000000, 0.3090169943749572767, 0.9510565162951503115 ) ) ;
#57190 = DIRECTION ( 'NONE',  ( 0.000000000000000000, 0.8910065241883690090, -0.4539904997395446395 ) ) ;
#57191 = VECTOR ( 'NONE', #59476, 1000.000000000000000 ) ;
#57192 = CARTESIAN_POINT ( 'NONE',  ( -96.32500000000001705, 87.70503267997129626, 85.10520833506762983 ) ) ;
#57193 = AXIS2_PLACEMENT_3D ( 'NONE', #34725, #1304, #68948 ) ;
#57194 = DIRECTION ( 'NONE',  ( -1.000000000000000000, 0.000000000000000000, 0.000000000000000000 ) ) ;
#57195 = LINE ( 'NONE', #62859, #6797 ) ;
#57196 = CARTESIAN_POINT ( 'NONE',  ( -97.30629616937501680, 88.66845928578038638, 77.63072916753380071 ) ) ;
#57197 = CARTESIAN_POINT ( 'NONE',  ( 10.00000000000000000, 0.000000000000000000, 0.000000000000000000 ) ) ;
#57198 = LINE ( 'NONE', #52656, #41034 ) ;
#57199 = AXIS2_PLACEMENT_3D ( 'NONE', #18165, #41108, #51995 ) ;
#57200 = AXIS2_PLACEMENT_3D ( 'NONE', #48850, #19902, #42853 ) ;
#57201 = ORIENTED_EDGE ( 'NONE', *, *, #51193, .F. ) ;
#57202 = DIRECTION ( 'NONE',  ( -1.000000000000000000, -0.000000000000000000, -0.000000000000000000 ) ) ;
#57203 = ADVANCED_FACE ( 'NONE', ( #33050 ), #3774, .T. ) ;
#57204 = CARTESIAN_POINT ( 'NONE',  ( 92.35000000000000853, -208.4700217866474645, 89.39145833506763950 ) ) ;
#57205 = DIRECTION ( 'NONE',  ( 1.000000000000000000, -0.000000000000000000, -0.000000000000000000 ) ) ;
#57206 = CARTESIAN_POINT ( 'NONE',  ( 0.000000000000000000, 1.530808498934191521E-15, -12.50000000000000000 ) ) ;
#57207 = ADVANCED_FACE ( 'NONE', ( #27413 ), #3404, .F. ) ;
#57208 = DIRECTION ( 'NONE',  ( 0.000000000000000000, 0.000000000000000000, 1.000000000000000000 ) ) ;
#57209 = CIRCLE ( 'NONE', #4409, 31.99999999999998579 ) ;
#57210 = DIRECTION ( 'NONE',  ( -0.000000000000000000, -0.000000000000000000, 1.000000000000000000 ) ) ;
#57211 = CARTESIAN_POINT ( 'NONE',  ( -92.69370383062498320, -208.6684592857803011, 78.74197916753382742 ) ) ;
#57212 = EDGE_CURVE ( 'NONE', #6635, #67063, #27796, .T. ) ;
#57213 = EDGE_CURVE ( 'NONE', #46917, #11307, #71786, .T. ) ;
#57214 = CARTESIAN_POINT ( 'NONE',  ( 11.99999999999999822, 46.53671651293948486, 59.03961581697416250 ) ) ;
#57215 = ORIENTED_EDGE ( 'NONE', *, *, #40658, .T. ) ;
#57216 = CARTESIAN_POINT ( 'NONE',  ( 0.000000000000000000, 0.000000000000000000, 0.000000000000000000 ) ) ;
#57217 = CARTESIAN_POINT ( 'NONE',  ( 0.000000000000000000, 2.571758278209441661E-15, -21.00000000000000000 ) ) ;
#57218 = CARTESIAN_POINT ( 'NONE',  ( 10.00000000000000000, 2.663952781846149254, 41.91543099594818500 ) ) ;
#57219 = CARTESIAN_POINT ( 'NONE',  ( 5.999999999999999112, 50.23322058963348979, 64.81221759200361987 ) ) ;
#57220 = LINE ( 'NONE', #52310, #46344 ) ;
#57221 = EDGE_CURVE ( 'NONE', #51520, #10248, #31682, .T. ) ;
#57222 = VERTEX_POINT ( 'NONE', #43259 ) ;
#57223 = CARTESIAN_POINT ( 'NONE',  ( -0.4966694826856976608, -121.4153866697721611, 2.500000000000000000 ) ) ;
#57224 = CARTESIAN_POINT ( 'NONE',  ( 10.00000000000000000, -2.543863470248951320, 81.96053171279901051 ) ) ;
#57225 = VERTEX_POINT ( 'NONE', #32677 ) ;
#57226 = CARTESIAN_POINT ( 'NONE',  ( 92.69370383062501162, -209.9999999999999716, 88.37281250086715545 ) ) ;
#57227 = LINE ( 'NONE', #24132, #68295 ) ;
#57228 = AXIS2_PLACEMENT_3D ( 'NONE', #1557, #8640, #42848 ) ;
#57229 = ORIENTED_EDGE ( 'NONE', *, *, #69857, .F. ) ;
#57230 = FACE_OUTER_BOUND ( 'NONE', #57063, .T. ) ;
#57231 = CIRCLE ( 'NONE', #52442, 0.2000000000000000944 ) ;
#57232 = ORIENTED_EDGE ( 'NONE', *, *, #71609, .T. ) ;
#57233 = DIRECTION ( 'NONE',  ( 7.962523111839282146E-16, -1.065814103640130873E-14, -1.000000000000000000 ) ) ;
#57234 = EDGE_LOOP ( 'NONE', ( #36045, #68729, #60155, #50598 ) ) ;
#57235 = EDGE_CURVE ( 'NONE', #40253, #37974, #37715, .T. ) ;
#57236 = EDGE_CURVE ( 'NONE', #21580, #59943, #50902, .T. ) ;
#57237 = ORIENTED_EDGE ( 'NONE', *, *, #33189, .F. ) ;
#57238 = CIRCLE ( 'NONE', #68073, 77.49899999999999523 ) ;
#57239 = DIRECTION ( 'NONE',  ( -1.000000000000000000, 0.000000000000000000, -0.000000000000000000 ) ) ;
#57240 = ORIENTED_EDGE ( 'NONE', *, *, #16311, .F. ) ;
#57241 = CIRCLE ( 'NONE', #825, 0.5999999999999998668 ) ;
#57242 = VERTEX_POINT ( 'NONE', #66180 ) ;
#57243 = DIRECTION ( 'NONE',  ( 1.000000000000000000, -0.000000000000000000, -0.000000000000000000 ) ) ;
#57244 = ORIENTED_EDGE ( 'NONE', *, *, #65178, .T. ) ;
#57245 = PRODUCT_DEFINITION_SHAPE ( 'NONE', 'NONE',  #74351 ) ;
#57246 = CIRCLE ( 'NONE', #48797, 23.50000000000000355 ) ;
#57247 = ORIENTED_EDGE ( 'NONE', *, *, #58164, .T. ) ;
#57248 = DIRECTION ( 'NONE',  ( 0.000000000000000000, 0.9238795325112878487, -0.3826834323650874503 ) ) ;
#57249 = DIRECTION ( 'NONE',  ( 0.000000000000000000, 0.000000000000000000, 1.000000000000000000 ) ) ;
#57250 = VERTEX_POINT ( 'NONE', #14654 ) ;
#57251 = ORIENTED_EDGE ( 'NONE', *, *, #39885, .T. ) ;
#57252 = CARTESIAN_POINT ( 'NONE',  ( 94.99999999999998579, 87.33691857156068750, 85.99156250086714692 ) ) ;
#57253 = ORIENTED_EDGE ( 'NONE', *, *, #2321, .F. ) ;
#57254 = CARTESIAN_POINT ( 'NONE',  ( 97.30629616937498838, -208.6684592857803011, 81.12322916753382174 ) ) ;
#57255 = APPLICATION_PROTOCOL_DEFINITION ( 'draft international standard', 'automotive_design', 1998, #57098 ) ;
#57256 = CYLINDRICAL_SURFACE ( 'NONE', #60625, 42.00000000000000000 ) ;
#57257 = VECTOR ( 'NONE', #41595, 1000.000000000000000 ) ;
#57258 = CARTESIAN_POINT ( 'NONE',  ( 0.000000000000000000, 27.75498641678786527, -31.52238457039571173 ) ) ;
#57259 = DIRECTION ( 'NONE',  ( -1.000000000000000000, 0.000000000000000000, 0.000000000000000000 ) ) ;
#57260 = CARTESIAN_POINT ( 'NONE',  ( 12.50000000000000000, 0.000000000000000000, -4.400000000000001243 ) ) ;
#57261 = CARTESIAN_POINT ( 'NONE',  ( 10.00000000000000000, 0.000000000000000000, 0.000000000000000000 ) ) ;
#57262 = CARTESIAN_POINT ( 'NONE',  ( 15.00000000000000000, 23.59884966291521380, -12.14883922797262805 ) ) ;
#57263 = CARTESIAN_POINT ( 'NONE',  ( -96.15314808468745866, -211.9973110713294489, 87.20864583420046756 ) ) ;
#57264 = CARTESIAN_POINT ( 'NONE',  ( -93.84685191531252713, 88.00268892867056536, 87.47322916753381605 ) ) ;
#57265 = ORIENTED_EDGE ( 'NONE', *, *, #4169, .T. ) ;
#57267 = CARTESIAN_POINT ( 'NONE',  ( -92.69370383062502583, 88.66845928578038638, 83.55739583420047722 ) ) ;
#57266 = CARTESIAN_POINT ( 'NONE',  ( 97.30629616937498838, 88.66845928578037217, 86.09739583420048348 ) ) ;
#57268 = VERTEX_POINT ( 'NONE', #37606 ) ;
#57269 = DIRECTION ( 'NONE',  ( -1.427937372958396784E-15, 1.000000000000000000, -1.078060571631604545E-14 ) ) ;
#57270 = DIRECTION ( 'NONE',  ( 0.000000000000000000, 1.000000000000000000, 0.000000000000000000 ) ) ;
#57271 = DIRECTION ( 'NONE',  ( 0.000000000000000000, 0.000000000000000000, -1.000000000000000000 ) ) ;
#57272 = CARTESIAN_POINT ( 'NONE',  ( 5.000000000000002665, 80.28980883073781172, -16.65972982744850839 ) ) ;
#57273 = CARTESIAN_POINT ( 'NONE',  ( -93.84685191531247028, -211.9973110713294489, 87.31447916753380412 ) ) ;
#57274 = CARTESIAN_POINT ( 'NONE',  ( -96.32499999999996021, -212.2949673200287179, 81.85083333333332689 ) ) ;
#57275 = DIRECTION ( 'NONE',  ( 0.000000000000000000, 0.000000000000000000, 1.000000000000000000 ) ) ;
#57276 = DIRECTION ( 'NONE',  ( -7.728965982074743403E-16, -1.065814103640131188E-14, -1.000000000000000000 ) ) ;
#57277 = FACE_BOUND ( 'NONE', #8346, .T. ) ;
#57278 = EDGE_LOOP ( 'NONE', ( #60874, #71751, #48338, #56304 ) ) ;
#57279 = ORIENTED_EDGE ( 'NONE', *, *, #11347, .F. ) ;
#57280 = CARTESIAN_POINT ( 'NONE',  ( -93.67500000000003979, 92.29496732002878900, 76.45333333333333314 ) ) ;
#57281 = DIRECTION ( 'NONE',  ( -1.000000000000000000, 0.000000000000000000, 0.000000000000000000 ) ) ;
#57282 = CARTESIAN_POINT ( 'NONE',  ( -93.26027265873587169, -208.4859488783624215, 74.79348190356851944 ) ) ;
#57283 = FACE_OUTER_BOUND ( 'NONE', #19479, .T. ) ;
#57284 = CYLINDRICAL_SURFACE ( 'NONE', #20515, 31.99999999999999289 ) ;
#57285 = LINE ( 'NONE', #552, #6047 ) ;
#57286 = CIRCLE ( 'NONE', #29622, 82.00000000000000000 ) ;
#57287 = ORIENTED_EDGE ( 'NONE', *, *, #8125, .F. ) ;
#57288 = CARTESIAN_POINT ( 'NONE',  ( -92.69370383062502583, 91.33154071421968467, 77.31322916753380525 ) ) ;
#57289 = ADVANCED_FACE ( 'NONE', ( #60899 ), #55627, .F. ) ;
#57290 = CARTESIAN_POINT ( 'NONE',  ( 92.35000000046409241, 89.99996903277681781, 77.38038495127642591 ) ) ;
#57291 = ADVANCED_FACE ( 'NONE', ( #15022 ), #62020, .F. ) ;
#57292 = CARTESIAN_POINT ( 'NONE',  ( 11.99999999999999822, 65.59268652807263322, -36.72794159290169347 ) ) ;
#57293 = FACE_OUTER_BOUND ( 'NONE', #65771, .T. ) ;
#57294 = AXIS2_PLACEMENT_3D ( 'NONE', #37673, #60607, #9086 ) ;
#57295 = EDGE_CURVE ( 'NONE', #36593, #51805, #35345, .T. ) ;
#57296 = CARTESIAN_POINT ( 'NONE',  ( 11.99999999999999822, 41.76937507738875155, -62.50329211542393892 ) ) ;
#57297 = CARTESIAN_POINT ( 'NONE',  ( 0.000000000000000000, -68.67312586194971402, -35.91791733033549860 ) ) ;
#57298 = CARTESIAN_POINT ( 'NONE',  ( -97.30629616937497417, -211.3315407142195852, 89.21947916753381946 ) ) ;
#57299 = VECTOR ( 'NONE', #56235, 1000.000000000000000 ) ;
#57300 = SURFACE_STYLE_USAGE ( .BOTH. , #55814 ) ;
#57301 = ADVANCED_FACE ( 'NONE', ( #32308 ), #15393, .F. ) ;
#57302 = EDGE_CURVE ( 'NONE', #2654, #58705, #67280, .T. ) ;
#57303 = CARTESIAN_POINT ( 'NONE',  ( 93.84685191531248449, 88.00268892867053694, 77.84239583420048803 ) ) ;
#57304 = CARTESIAN_POINT ( 'NONE',  ( -97.30629616937497417, -208.6684592857803295, 78.31864583420050963 ) ) ;
#57305 = DIRECTION ( 'NONE',  ( 0.000000000000000000, 0.000000000000000000, 1.000000000000000000 ) ) ;
#57306 = VERTEX_POINT ( 'NONE', #10131 ) ;
#57307 = DIRECTION ( 'NONE',  ( -0.000000000000000000, -0.000000000000000000, -1.000000000000000000 ) ) ;
#57308 = CARTESIAN_POINT ( 'NONE',  ( -97.64999999999994884, -208.4700217866474645, 75.97708333333333997 ) ) ;
#57309 = LINE ( 'NONE', #5819, #13748 ) ;
#57310 = CARTESIAN_POINT ( 'NONE',  ( 0.000000000000000000, -46.11716303203233736, 67.80270845531873647 ) ) ;
#57312 = ADVANCED_FACE ( 'NONE', ( #23640 ), #57122, .T. ) ;
#57311 = CARTESIAN_POINT ( 'NONE',  ( 95.00000000000000000, -212.6630814284392557, 81.54656250086715374 ) ) ;
#57313 = ORIENTED_EDGE ( 'NONE', *, *, #51914, .T. ) ;
#57314 = VECTOR ( 'NONE', #48089, 1000.000000000000000 ) ;
#57315 = EDGE_CURVE ( 'NONE', #64608, #24000, #34165, .T. ) ;
#57316 = DIRECTION ( 'NONE',  ( -0.000000000000000000, -0.000000000000000000, -1.000000000000000000 ) ) ;
#57317 = ORIENTED_EDGE ( 'NONE', *, *, #49798, .F. ) ;
#57318 = DIRECTION ( 'NONE',  ( 0.000000000000000000, -0.000000000000000000, 1.000000000000000000 ) ) ;
#57319 = ORIENTED_EDGE ( 'NONE', *, *, #59234, .T. ) ;
#57320 = DIRECTION ( 'NONE',  ( -1.000000000000000000, 0.000000000000000000, -0.000000000000000000 ) ) ;
#57321 = EDGE_CURVE ( 'NONE', #38563, #40323, #28907, .T. ) ;
#57322 = EDGE_CURVE ( 'NONE', #19874, #60828, #72555, .T. ) ;
#57323 = ORIENTED_EDGE ( 'NONE', *, *, #55454, .F. ) ;
#57324 = VERTEX_POINT ( 'NONE', #34926 ) ;
#57325 = VERTEX_POINT ( 'NONE', #40199 ) ;
#57326 = CARTESIAN_POINT ( 'NONE',  ( -7.400000000000003908, -1.056673655988042765E-14, -5.892267102755452808E-15 ) ) ;
#57327 = ORIENTED_EDGE ( 'NONE', *, *, #45576, .F. ) ;
#57328 = ORIENTED_EDGE ( 'NONE', *, *, #39953, .T. ) ;
#57329 = CARTESIAN_POINT ( 'NONE',  ( 92.69370383062498320, 88.66845928578037217, 84.77447916753381207 ) ) ;
#57330 = VECTOR ( 'NONE', #71306, 1000.000000000000000 ) ;
#57331 = CARTESIAN_POINT ( 'NONE',  ( 93.67500000000001137, -207.7050326799711968, 77.82916666666665151 ) ) ;
#57332 = ORIENTED_EDGE ( 'NONE', *, *, #70345, .F. ) ;
#57333 = ORIENTED_EDGE ( 'NONE', *, *, #73727, .T. ) ;
#57334 = VERTEX_POINT ( 'NONE', #69144 ) ;
#57335 = EDGE_LOOP ( 'NONE', ( #70745, #69405, #6250, #65393 ) ) ;
#57336 = DIRECTION ( 'NONE',  ( 0.000000000000000000, 1.000000000000000000, -9.787530781167598712E-16 ) ) ;
#57337 =( LENGTH_UNIT ( ) NAMED_UNIT ( * ) SI_UNIT ( .MILLI., .METRE. ) );
#57338 = LINE ( 'NONE', #64464, #15094 ) ;
#57339 = AXIS2_PLACEMENT_3D ( 'NONE', #27019, #26656, #8641 ) ;
#57340 = DIRECTION ( 'NONE',  ( 0.000000000000000000, 0.000000000000000000, -1.000000000000000000 ) ) ;
#57341 = DIRECTION ( 'NONE',  ( 0.000000000000000000, 0.000000000000000000, 1.000000000000000000 ) ) ;
#57342 = AXIS2_PLACEMENT_3D ( 'NONE', #56570, #73830, #50905 ) ;
#57343 = CARTESIAN_POINT ( 'NONE',  ( 92.35000000000002274, -209.9999907117589260, 86.90437468048608594 ) ) ;
#57344 = DIRECTION ( 'NONE',  ( -0.4796670183876317051, 0.8774505977381972244, 0.000000000000000000 ) ) ;
#57345 = LINE ( 'NONE', #27657, #70409 ) ;
#57346 = ORIENTED_EDGE ( 'NONE', *, *, #42219, .F. ) ;
#57347 = CARTESIAN_POINT ( 'NONE',  ( -97.64999999999996305, -209.9999999999999716, 82.45937500173430124 ) ) ;
#57348 = ORIENTED_EDGE ( 'NONE', *, *, #68945, .F. ) ;
#57349 = CYLINDRICAL_SURFACE ( 'NONE', #20684, 37.49900000000000233 ) ;
#57350 = VERTEX_POINT ( 'NONE', #6360 ) ;
#57352 = CARTESIAN_POINT ( 'NONE',  ( -93.67500000000003979, 87.70503267997129626, 78.22604166840096696 ) ) ;
#57351 = CARTESIAN_POINT ( 'NONE',  ( 92.34999999999999432, 88.47002178664753558, 80.60729166840097548 ) ) ;
#57353 =( BOUNDED_CURVE ( )  B_SPLINE_CURVE ( 2, ( #66694, #9550, #72676, #67804, #67431, #44129, #21178 ),
 .UNSPECIFIED., .F., .F. ) 
 B_SPLINE_CURVE_WITH_KNOTS ( ( 3, 2, 2, 3 ),
 ( 0.3175094496506952191, 0.3245652148805888704, 0.3316209804214712564, 0.3386766260338262002 ),
 .UNSPECIFIED. ) 
 CURVE ( )  GEOMETRIC_REPRESENTATION_ITEM ( )  RATIONAL_B_SPLINE_CURVE ( ( 1.000000000000000000, 0.8660254037844387076, 1.000000000000000000, 0.8660254037844387076, 1.000000000000000000, 0.8660276809825602218, 0.9999954456811690484 ) ) 
 REPRESENTATION_ITEM ( '' )  );
#57354 = ORIENTED_EDGE ( 'NONE', *, *, #60928, .T. ) ;
#57355 = CARTESIAN_POINT ( 'NONE',  ( 97.30629616937498838, 91.33154071421968467, 78.74197916753382742 ) ) ;
#57356 = CARTESIAN_POINT ( 'NONE',  ( -96.32499999999996021, -207.7050326799711968, 82.27416666666665890 ) ) ;
#57358 = EDGE_CURVE ( 'NONE', #23124, #15280, #34542, .T. ) ;
#57357 = CARTESIAN_POINT ( 'NONE',  ( -0.9515373497862389396, -96.47140937769621871, 5.500000000000000000 ) ) ;
#57359 = DIRECTION ( 'NONE',  ( -1.000000000000000000, -0.000000000000000000, -0.000000000000000000 ) ) ;
#57360 = CARTESIAN_POINT ( 'NONE',  ( 10.00000000000000000, -20.40083707022935400, 72.35432306680478121 ) ) ;
#57361 = ORIENTED_EDGE ( 'NONE', *, *, #67234, .T. ) ;
#57362 = CARTESIAN_POINT ( 'NONE',  ( 97.64999999999999147, 90.00000000000002842, 90.00000000000000000 ) ) ;
#57363 = LINE ( 'NONE', #57741, #58969 ) ;
#57364 = DIRECTION ( 'NONE',  ( 0.000000000000000000, 0.000000000000000000, 1.000000000000000000 ) ) ;
#57365 = ORIENTED_EDGE ( 'NONE', *, *, #10343, .F. ) ;
#57366 = AXIS2_PLACEMENT_3D ( 'NONE', #17198, #57421, #73209 ) ;
#57367 = ORIENTED_EDGE ( 'NONE', *, *, #19229, .T. ) ;
#57368 = EDGE_CURVE ( 'NONE', #9077, #44189, #29265, .T. ) ;
#57370 = ADVANCED_FACE ( 'NONE', ( #62783 ), #52206, .F. ) ;
#57369 = VECTOR ( 'NONE', #38796, 1000.000000000000000 ) ;
#57371 = CARTESIAN_POINT ( 'NONE',  ( -0.9515373497862389396, -96.47140937769621871, 5.500000000000000000 ) ) ;
#57372 = ADVANCED_FACE ( 'NONE', ( #40558 ), #51098, .T. ) ;
#57373 = DIRECTION ( 'NONE',  ( 1.000000000000000000, -0.000000000000000000, 0.000000000000000000 ) ) ;
#57374 = CARTESIAN_POINT ( 'NONE',  ( 0.000000000000000000, 0.000000000000000000, 0.000000000000000000 ) ) ;
#57375 = CARTESIAN_POINT ( 'NONE',  ( -94.99999999999997158, -212.6630814284392557, 81.07031250086716057 ) ) ;
#57376 = CIRCLE ( 'NONE', #21326, 37.49900000000000944 ) ;
#57377 = ORIENTED_EDGE ( 'NONE', *, *, #40131, .F. ) ;
#57378 = EDGE_CURVE ( 'NONE', #55000, #47150, #13640, .T. ) ;
#57379 = DIRECTION ( 'NONE',  ( -1.000000000000000000, -0.000000000000000000, 0.000000000000000000 ) ) ;
#57380 = LINE ( 'NONE', #57756, #61107 ) ;
#57381 = DIRECTION ( 'NONE',  ( -1.000000000000000000, -0.000000000000000000, 0.000000000000000000 ) ) ;
#57382 = DIRECTION ( 'NONE',  ( 0.000000000000000000, 0.6494480483301793283, 0.7604059656000345946 ) ) ;
#57383 = DIRECTION ( 'NONE',  ( 1.000000000000000000, 0.000000000000000000, 0.000000000000000000 ) ) ;
#57384 = DIRECTION ( 'NONE',  ( -1.000000000000000000, -0.000000000000000000, -0.000000000000000000 ) ) ;
#57385 = LINE ( 'NONE', #22817, #61361 ) ;
#57386 = DIRECTION ( 'NONE',  ( -0.9435911131814398445, 0.3311129884571295534, 0.000000000000000000 ) ) ;
#57387 = DIRECTION ( 'NONE',  ( -0.000000000000000000, -0.000000000000000000, 1.000000000000000000 ) ) ;
#57388 = CARTESIAN_POINT ( 'NONE',  ( 11.99999999999999822, -55.19960302592029677, -51.03279382321147750 ) ) ;
#57389 = EDGE_CURVE ( 'NONE', #64823, #37625, #65352, .T. ) ;
#57390 = VECTOR ( 'NONE', #69170, 1000.000000000000000 ) ;
#57391 = CARTESIAN_POINT ( 'NONE',  ( 97.30629616937498838, 91.33154071421968467, 88.90197916753382401 ) ) ;
#57392 = DIRECTION ( 'NONE',  ( 0.000000000000000000, 0.000000000000000000, 1.000000000000000000 ) ) ;
#57393 = CARTESIAN_POINT ( 'NONE',  ( -2.499999999999970690, 73.00000000000001421, -258.2999999999999545 ) ) ;
#57394 = EDGE_LOOP ( 'NONE', ( #5652, #62123, #41690, #47045 ) ) ;
#57395 = CARTESIAN_POINT ( 'NONE',  ( 10.00000000000000000, 35.47612816024556537, -22.48208911017461631 ) ) ;
#57396 = CARTESIAN_POINT ( 'NONE',  ( -97.30629616937501680, 88.66845928578038638, 78.90072916753381094 ) ) ;
#57397 = CIRCLE ( 'NONE', #56210, 82.00000000000000000 ) ;
#57398 = AXIS2_PLACEMENT_3D ( 'NONE', #71881, #42968, #31297 ) ;
#57400 = ADVANCED_FACE ( 'NONE', ( #37439 ), #42695, .T. ) ;
#57399 = CARTESIAN_POINT ( 'NONE',  ( -3.000000000000000000, -18.13022148937243472, -15.02647892043568767 ) ) ;
#57401 = ADVANCED_FACE ( 'NONE', ( #15225 ), #31767, .F. ) ;
#57402 = ORIENTED_EDGE ( 'NONE', *, *, #17315, .F. ) ;
#57403 = LINE ( 'NONE', #307, #39050 ) ;
#57404 = EDGE_CURVE ( 'NONE', #37858, #71422, #11339, .T. ) ;
#57405 = DIRECTION ( 'NONE',  ( 0.000000000000000000, 0.8090169943749445647, 0.5877852522924770229 ) ) ;
#57406 = CARTESIAN_POINT ( 'NONE',  ( 0.000000000000000000, -10.74501242461307982, 35.92658777277507198 ) ) ;
#57407 = DIRECTION ( 'NONE',  ( 0.000000000000000000, -0.5877852522924625900, -0.8090169943749551118 ) ) ;
#57408 = DIRECTION ( 'NONE',  ( -0.000000000000000000, -0.000000000000000000, 1.000000000000000000 ) ) ;
#57409 = CIRCLE ( 'NONE', #2171, 31.99999999999998579 ) ;
#57410 = CIRCLE ( 'NONE', #33342, 2.541999999999999815 ) ;
#57411 = ORIENTED_EDGE ( 'NONE', *, *, #44071, .F. ) ;
#57412 = ORIENTED_EDGE ( 'NONE', *, *, #61272, .F. ) ;
#57413 = AXIS2_PLACEMENT_3D ( 'NONE', #57699, #30217, #52793 ) ;
#57414 = CIRCLE ( 'NONE', #63435, 82.00000000000000000 ) ;
#57415 = CARTESIAN_POINT ( 'NONE',  ( 92.69370383062501162, -209.9999999999999716, 85.99156250086716113 ) ) ;
#57416 = DIRECTION ( 'NONE',  ( 0.000000000000000000, 0.000000000000000000, 1.000000000000000000 ) ) ;
#57417 = CARTESIAN_POINT ( 'NONE',  ( 10.00000000000000000, 74.74816331893477184, -33.71516098798658589 ) ) ;
#57418 = VECTOR ( 'NONE', #43634, 1000.000000000000000 ) ;
#57419 = CARTESIAN_POINT ( 'NONE',  ( 94.99999999999998579, 93.05995642670504253, 82.85625000000000284 ) ) ;
#57420 = CARTESIAN_POINT ( 'NONE',  ( 15.00000000000000000, -0.9646360437375368635, -23.52805723605589705 ) ) ;
#57421 = DIRECTION ( 'NONE',  ( -1.000000000000000000, 0.000000000000000000, -0.000000000000000000 ) ) ;
#57422 = CARTESIAN_POINT ( 'NONE',  ( 96.32499999999998863, -207.7050326799711968, 88.51833333333333087 ) ) ;
#57423 = ORIENTED_EDGE ( 'NONE', *, *, #70241, .T. ) ;
#57424 = ORIENTED_EDGE ( 'NONE', *, *, #67399, .T. ) ;
#57425 = ORIENTED_EDGE ( 'NONE', *, *, #21668, .F. ) ;
#57426 = ORIENTED_EDGE ( 'NONE', *, *, #62508, .F. ) ;
#57427 = CARTESIAN_POINT ( 'NONE',  ( -42.50000000000000000, 0.000000000000000000, -13.90444123027096879 ) ) ;
#57428 =( NAMED_UNIT ( * ) SI_UNIT ( $, .STERADIAN. ) SOLID_ANGLE_UNIT ( ) );
#57429 = CARTESIAN_POINT ( 'NONE',  ( -96.15314808468752972, 91.99731107132950569, 88.42572916753381662 ) ) ;
#57430 = CYLINDRICAL_SURFACE ( 'NONE', #49691, 82.00000000000000000 ) ;
#57431 = CARTESIAN_POINT ( 'NONE',  ( 0.000000000000000000, 0.000000000000000000, 0.000000000000000000 ) ) ;
#57432 = CARTESIAN_POINT ( 'NONE',  ( 92.35000000000002274, -208.4700217866474645, 76.05645833506761733 ) ) ;
#57433 = CARTESIAN_POINT ( 'NONE',  ( 92.34999999999999432, 88.47002178664753558, 79.89291666666666458 ) ) ;
#57434 = EDGE_LOOP ( 'NONE', ( #35396, #35128, #12766, #34807 ) ) ;
#57435 = CARTESIAN_POINT ( 'NONE',  ( 12.00000000000000000, -11.95096189432345923, -23.69967320028757030 ) ) ;
#57436 = ADVANCED_FACE ( 'NONE', ( #67098 ), #72365, .F. ) ;
#57437 = VERTEX_POINT ( 'NONE', #14104 ) ;
#57438 = CARTESIAN_POINT ( 'NONE',  ( -97.64999999999996305, -210.0000348885099015, 83.09437620840745353 ) ) ;
#57439 = ORIENTED_EDGE ( 'NONE', *, *, #1576, .T. ) ;
#57440 = CARTESIAN_POINT ( 'NONE',  ( -95.00000000000002842, 93.05995642670501411, 89.28562500173430294 ) ) ;
#57441 = CARTESIAN_POINT ( 'NONE',  ( -92.69370383062505425, 91.33154071421968467, 82.55197916753380127 ) ) ;
#57442 = AXIS2_PLACEMENT_3D ( 'NONE', #70909, #43107, #14130 ) ;
#57443 = CARTESIAN_POINT ( 'NONE',  ( 93.84685191531248449, 91.99731107132950569, 76.20197916753380696 ) ) ;
#57444 = EDGE_LOOP ( 'NONE', ( #46727, #11681, #36683, #15556 ) ) ;
#57445 = CARTESIAN_POINT ( 'NONE',  ( 95.00000000000000000, -209.9999999999999716, 90.00000000000000000 ) ) ;
#57446 = CIRCLE ( 'NONE', #36984, 37.49900000000000233 ) ;
#57447 = AXIS2_PLACEMENT_3D ( 'NONE', #58124, #53972, #58488 ) ;
#57448 = DIRECTION ( 'NONE',  ( 1.000000000000000000, 0.000000000000000000, 0.000000000000000000 ) ) ;
#57449 = DIRECTION ( 'NONE',  ( 0.000000000000000000, 0.9876883405951371042, 0.1564344650402347547 ) ) ;
#57450 = CARTESIAN_POINT ( 'NONE',  ( 10.00000000000000000, 73.73191006444572793, -14.66109333815486515 ) ) ;
#57451 = ORIENTED_EDGE ( 'NONE', *, *, #47053, .T. ) ;
#57452 = LINE ( 'NONE', #5968, #61536 ) ;
#57453 = CARTESIAN_POINT ( 'NONE',  ( -93.84685191531247028, -211.9973110713294489, 79.05947916753380866 ) ) ;
#57454 = ORIENTED_EDGE ( 'NONE', *, *, #72291, .T. ) ;
#57455 = ORIENTED_EDGE ( 'NONE', *, *, #791, .T. ) ;
#57456 = AXIS2_PLACEMENT_3D ( 'NONE', #32036, #49696, #26408 ) ;
#57457 = EDGE_CURVE ( 'NONE', #24083, #61302, #13705, .T. ) ;
#57458 = FACE_BOUND ( 'NONE', #73138, .T. ) ;
#57459 = EDGE_CURVE ( 'NONE', #9432, #52406, #65633, .T. ) ;
#57460 = VERTEX_POINT ( 'NONE', #3239 ) ;
#57461 = DIRECTION ( 'NONE',  ( -1.000000000000000000, 0.000000000000000000, 0.000000000000000000 ) ) ;
#57462 = DIRECTION ( 'NONE',  ( 0.000000000000000000, 0.5224985647159441360, 0.8526401643540952868 ) ) ;
#57463 = EDGE_LOOP ( 'NONE', ( #41348, #24550, #52577, #47536 ) ) ;
#57464 = CARTESIAN_POINT ( 'NONE',  ( -93.84685191531248449, -208.0026889286704943, 76.09614583420047040 ) ) ;
#57465 = ORIENTED_EDGE ( 'NONE', *, *, #52417, .T. ) ;
#57466 = CARTESIAN_POINT ( 'NONE',  ( 5.000000000000002665, -81.50828551894220197, -8.966570791701590437 ) ) ;
#57467 = DIRECTION ( 'NONE',  ( -1.000000000000000000, -0.000000000000000000, -0.000000000000000000 ) ) ;
#57468 = CARTESIAN_POINT ( 'NONE',  ( 0.000000000000000000, 62.50329211542494789, -41.76937507738723099 ) ) ;
#57469 = ORIENTED_EDGE ( 'NONE', *, *, #215, .F. ) ;
#57470 = EDGE_CURVE ( 'NONE', #36758, #1076, #14944, .T. ) ;
#57471 = CIRCLE ( 'NONE', #25035, 12.49999999999999822 ) ;
#57472 = EDGE_CURVE ( 'NONE', #16471, #32358, #43785, .T. ) ;
#57473 = DIRECTION ( 'NONE',  ( 0.000000000000000000, 0.000000000000000000, -1.000000000000000000 ) ) ;
#57474 = CARTESIAN_POINT ( 'NONE',  ( 5.000000000000000000, 2.663952781846149254, 41.91543099594818500 ) ) ;
#57475 = CARTESIAN_POINT ( 'NONE',  ( 93.84685191531248449, 91.99731107132950569, 86.36197916753381776 ) ) ;
#57476 = CARTESIAN_POINT ( 'NONE',  ( -94.99999999999997158, -213.0599564267049857, 83.80875000000000341 ) ) ;
#57477 = CARTESIAN_POINT ( 'NONE',  ( -92.35000000000013642, 88.47002178664750716, 88.35958333333334735 ) ) ;
#57478 = CARTESIAN_POINT ( 'NONE',  ( 0.000000000000000000, -120.0000000000000000, -2.500000000000000000 ) ) ;
#57479 = CIRCLE ( 'NONE', #20260, 42.00000000000000000 ) ;
#57480 = CARTESIAN_POINT ( 'NONE',  ( -4.999999999999999112, 2.059541880721995177, -1.329159518034682685 ) ) ;
#57481 = CIRCLE ( 'NONE', #25043, 16.00000000000000000 ) ;
#57482 = CYLINDRICAL_SURFACE ( 'NONE', #51220, 31.99999999999999289 ) ;
#57483 = FACE_OUTER_BOUND ( 'NONE', #61162, .T. ) ;
#57484 = CIRCLE ( 'NONE', #31006, 77.49900000000000944 ) ;
#57485 = EDGE_CURVE ( 'NONE', #31772, #59828, #20863, .T. ) ;
#57486 = FACE_OUTER_BOUND ( 'NONE', #21063, .T. ) ;
#57487 = LINE ( 'NONE', #29625, #50538 ) ;
#57488 = CARTESIAN_POINT ( 'NONE',  ( -97.30629616937501680, 90.00000000000004263, 88.37281250086715545 ) ) ;
#57489 = LINE ( 'NONE', #6006, #68340 ) ;
#57490 = AXIS2_PLACEMENT_3D ( 'NONE', #67774, #33545, #33922 ) ;
#57492 = ADVANCED_FACE ( 'NONE', ( #72716 ), #3970, .T. ) ;
#57491 = LINE ( 'NONE', #29270, #41672 ) ;
#57493 = EDGE_CURVE ( 'NONE', #51207, #6061, #21313, .T. ) ;
#57494 = EDGE_CURVE ( 'NONE', #17127, #13140, #12527, .T. ) ;
#57495 = AXIS2_PLACEMENT_3D ( 'NONE', #42278, #14044, #65206 ) ;
#57496 = ADVANCED_FACE ( 'NONE', ( #48696 ), #71620, .T. ) ;
#57497 = CARTESIAN_POINT ( 'NONE',  ( 0.000000000000000000, 0.000000000000000000, 0.000000000000000000 ) ) ;
#57498 = DIRECTION ( 'NONE',  ( 0.000000000000000000, -0.9876883405951361050, -0.1564344650402419989 ) ) ;
#57499 =( LENGTH_UNIT ( ) NAMED_UNIT ( * ) SI_UNIT ( .MILLI., .METRE. ) );
#57500 = AXIS2_PLACEMENT_3D ( 'NONE', #18112, #69965, #34657 ) ;
#57501 = VECTOR ( 'NONE', #1946, 1000.000000000000000 ) ;
#57502 = DIRECTION ( 'NONE',  ( 0.000000000000000000, 0.000000000000000000, -1.000000000000000000 ) ) ;
#57503 = CARTESIAN_POINT ( 'NONE',  ( 10.00000000000000000, 0.000000000000000000, 0.000000000000000000 ) ) ;
#57504 = CARTESIAN_POINT ( 'NONE',  ( 92.69370383062501162, -208.6684592857803011, 86.57364583420047666 ) ) ;
#57505 = VECTOR ( 'NONE', #59698, 1000.000000000000000 ) ;
#57506 = AXIS2_PLACEMENT_3D ( 'NONE', #63610, #36485, #63973 ) ;
#57507 = EDGE_LOOP ( 'NONE', ( #39294, #29379, #18204, #47784 ) ) ;
#57508 = ORIENTED_EDGE ( 'NONE', *, *, #21136, .F. ) ;
#57509 = FILL_AREA_STYLE ('',( #10514 ) ) ;
#57510 = ORIENTED_EDGE ( 'NONE', *, *, #1398, .F. ) ;
#57511 = DIRECTION ( 'NONE',  ( 0.000000000000000000, 0.000000000000000000, 1.000000000000000000 ) ) ;
#57512 = CARTESIAN_POINT ( 'NONE',  ( 0.000000000000000000, 0.8261519478431083030, 77.49459641780886443 ) ) ;
#57513 = VERTEX_POINT ( 'NONE', #66010 ) ;
#57514 = CARTESIAN_POINT ( 'NONE',  ( 92.69370383062501162, -208.6684592857803011, 82.76364583420048859 ) ) ;
#57515 = AXIS2_PLACEMENT_3D ( 'NONE', #4044, #38981, #61917 ) ;
#57516 = EDGE_LOOP ( 'NONE', ( #48550, #41585 ) ) ;
#57517 = PLANE ( 'NONE',  #73112 ) ;
#57518 = VERTEX_POINT ( 'NONE', #14484 ) ;
#57519 = EDGE_LOOP ( 'NONE', ( #63764, #10151, #56027, #65088 ) ) ;
#57520 = DIRECTION ( 'NONE',  ( -0.000000000000000000, -0.000000000000000000, 1.000000000000000000 ) ) ;
#57521 = CIRCLE ( 'NONE', #22750, 77.49899999999999523 ) ;
#57522 = CIRCLE ( 'NONE', #19080, 31.99999999999999645 ) ;
#57523 = CARTESIAN_POINT ( 'NONE',  ( 11.99999999999999822, -18.89407956138310496, 75.16055320797023853 ) ) ;
#57524 = CIRCLE ( 'NONE', #40731, 31.99999999999998934 ) ;
#57525 = ORIENTED_EDGE ( 'NONE', *, *, #14946, .F. ) ;
#57526 = DIRECTION ( 'NONE',  ( -1.000000000000000000, 0.000000000000000000, 0.000000000000000000 ) ) ;
#57527 = CARTESIAN_POINT ( 'NONE',  ( 95.00000000000000000, -206.9400435732949575, 86.74562500173429669 ) ) ;
#57528 = AXIS2_PLACEMENT_3D ( 'NONE', #54615, #9484, #32408 ) ;
#57529 = ORIENTED_EDGE ( 'NONE', *, *, #27135, .T. ) ;
#57530 = DIRECTION ( 'NONE',  ( 0.000000000000000000, 0.000000000000000000, 1.000000000000000000 ) ) ;
#57531 = EDGE_CURVE ( 'NONE', #6316, #42183, #22145, .T. ) ;
#57532 = EDGE_LOOP ( 'NONE', ( #24166, #27905, #15934, #26727 ) ) ;
#57533 = AXIS2_PLACEMENT_3D ( 'NONE', #6555, #44933, #11083 ) ;
#57534 = CARTESIAN_POINT ( 'NONE',  ( 97.64999999999689351, 89.99999595380309358, 77.06187486178042434 ) ) ;
#57535 = ORIENTED_EDGE ( 'NONE', *, *, #19286, .F. ) ;
#57536 = EDGE_CURVE ( 'NONE', #45615, #1516, #9213, .T. ) ;
#57537 = ORIENTED_EDGE ( 'NONE', *, *, #64333, .T. ) ;
#57538 = EDGE_LOOP ( 'NONE', ( #48255, #43229, #14625, #59481 ) ) ;
#57539 = FACE_OUTER_BOUND ( 'NONE', #72221, .T. ) ;
#57540 = CARTESIAN_POINT ( 'NONE',  ( -5.000000000000000000, -0.1416384297035285789, -0.5080592402122394713 ) ) ;
#57542 = EDGE_CURVE ( 'NONE', #11201, #47808, #4173, .T. ) ;
#57541 = VERTEX_POINT ( 'NONE', #5083 ) ;
#57543 = ORIENTED_EDGE ( 'NONE', *, *, #34011, .T. ) ;
#57544 = VERTEX_POINT ( 'NONE', #33625 ) ;
#57545 = CARTESIAN_POINT ( 'NONE',  ( 97.65000000000000568, 91.52997821335252127, 79.65479166840096070 ) ) ;
#57546 = ADVANCED_FACE ( 'NONE', ( #22353 ), #10699, .F. ) ;
#57547 = CARTESIAN_POINT ( 'NONE',  ( 10.00000000000000000, 0.000000000000000000, 0.000000000000000000 ) ) ;
#57549 = CARTESIAN_POINT ( 'NONE',  ( -97.65000000000001990, 88.47002178664754979, 88.14791666666666003 ) ) ;
#57548 = AXIS2_PLACEMENT_3D ( 'NONE', #44785, #73329, #33474 ) ;
#57550 = ORIENTED_EDGE ( 'NONE', *, *, #27830, .F. ) ;
#57551 = PLANE ( 'NONE',  #33506 ) ;
#57552 = ORIENTED_EDGE ( 'NONE', *, *, #27041, .F. ) ;
#57553 = CARTESIAN_POINT ( 'NONE',  ( 92.34999999999999432, 90.00000000000002842, 90.00000000000000000 ) ) ;
#57554 = CARTESIAN_POINT ( 'NONE',  ( -92.69370383062498320, -208.6684592857803011, 85.56822916753380071 ) ) ;
#57555 = ORIENTED_EDGE ( 'NONE', *, *, #46120, .F. ) ;
#57556 = VECTOR ( 'NONE', #10944, 1000.000000000000000 ) ;
#57557 = FACE_OUTER_BOUND ( 'NONE', #37658, .T. ) ;
#57558 = CARTESIAN_POINT ( 'NONE',  ( 0.000000000000000000, 0.000000000000000000, 42.00000000000001421 ) ) ;
#57559 = DIRECTION ( 'NONE',  ( 0.000000000000000000, 0.000000000000000000, -1.000000000000000000 ) ) ;
#57560 = CARTESIAN_POINT ( 'NONE',  ( -92.69370383062498320, -208.6684592857803295, 76.67822916753378593 ) ) ;
#57561 = CIRCLE ( 'NONE', #16708, 77.49900000000000944 ) ;
#57562 = CIRCLE ( 'NONE', #10752, 16.00000000000000000 ) ;
#57563 = EDGE_CURVE ( 'NONE', #12963, #32707, #57309, .T. ) ;
#57564 = AXIS2_PLACEMENT_3D ( 'NONE', #37417, #59981, #49039 ) ;
#57565 = CARTESIAN_POINT ( 'NONE',  ( 94.99999999999998579, 90.00000000000002842, 90.00000000000000000 ) ) ;
#57566 = DIRECTION ( 'NONE',  ( -1.000000000000000000, -0.000000000000000000, -0.000000000000000000 ) ) ;
#57567 = CIRCLE ( 'NONE', #28728, 2.649999999999985700 ) ;
#57568 = CARTESIAN_POINT ( 'NONE',  ( 5.999999999999999112, -64.81221759200379040, 50.23322058963324110 ) ) ;
#57569 = CARTESIAN_POINT ( 'NONE',  ( -93.67500000000003979, 92.29496732002878900, 76.45333333333333314 ) ) ;
#57570 = CARTESIAN_POINT ( 'NONE',  ( 92.35000000021533140, 90.00002100773845370, 79.91868729553033290 ) ) ;
#57571 = CARTESIAN_POINT ( 'NONE',  ( -93.84685191531252713, 88.00268892867056536, 78.42447916753381776 ) ) ;
#57572 = CARTESIAN_POINT ( 'NONE',  ( 1.560000000000000053, 0.000000000000000000, 1.500000000000000000 ) ) ;
#57573 = CARTESIAN_POINT ( 'NONE',  ( 11.99999999999999822, -74.65491531819111515, -8.830959090343204920 ) ) ;
#57574 = EDGE_CURVE ( 'NONE', #13600, #11350, #55729, .T. ) ;
#57575 = ORIENTED_EDGE ( 'NONE', *, *, #17563, .T. ) ;
#57576 = EDGE_CURVE ( 'NONE', #62322, #6316, #28727, .T. ) ;
#57577 = CARTESIAN_POINT ( 'NONE',  ( 92.34999999999999432, 90.00001433786182758, 79.28437450583713542 ) ) ;
#57578 = AXIS2_PLACEMENT_3D ( 'NONE', #45453, #69116, #50697 ) ;
#57579 = EDGE_CURVE ( 'NONE', #44464, #35626, #51286, .T. ) ;
#57580 = CYLINDRICAL_SURFACE ( 'NONE', #44910, 82.00000000000000000 ) ;
#57582 = DIRECTION ( 'NONE',  ( -1.000000000000000000, -0.000000000000000000, -0.000000000000000000 ) ) ;
#57581 = AXIS2_PLACEMENT_3D ( 'NONE', #12212, #35878, #28764 ) ;
#57583 = VECTOR ( 'NONE', #69826, 1000.000000000000000 ) ;
#57584 = CARTESIAN_POINT ( 'NONE',  ( 11.99999999999999822, 0.000000000000000000, 0.000000000000000000 ) ) ;
#57585 = CARTESIAN_POINT ( 'NONE',  ( -10.00000000000000000, 0.000000000000000000, 0.000000000000000000 ) ) ;
#57586 = CARTESIAN_POINT ( 'NONE',  ( -92.35000000045957336, 90.00004935162611730, 87.22187670868784437 ) ) ;
#57587 = CARTESIAN_POINT ( 'NONE',  ( -92.69370383062498320, -209.9999999999999716, 77.41906250086715602 ) ) ;
#57588 = VECTOR ( 'NONE', #52413, 1000.000000000000227 ) ;
#57589 = AXIS2_PLACEMENT_3D ( 'NONE', #6369, #73284, #68415 ) ;
#57590 = CARTESIAN_POINT ( 'NONE',  ( 10.00000000000000000, 0.000000000000000000, 0.000000000000000000 ) ) ;
#57591 = EDGE_CURVE ( 'NONE', #59274, #41967, #38938, .T. ) ;
#57592 =( BOUNDED_CURVE ( )  B_SPLINE_CURVE ( 2, ( #1875, #52971, #34942, #1143, #23657, #7104, #30394 ),
 .UNSPECIFIED., .F., .F. ) 
 B_SPLINE_CURVE_WITH_KNOTS ( ( 3, 2, 2, 3 ),
 ( 0.08333333333333288462, 0.09027777777777759582, 0.09722222222222230703, 0.1041666666666670182 ),
 .UNSPECIFIED. ) 
 CURVE ( )  GEOMETRIC_REPRESENTATION_ITEM ( )  RATIONAL_B_SPLINE_CURVE ( ( 1.000000000000008660, 0.8660254037844301589, 1.000000000000000000, 0.8660254037844387076, 1.000000000000000000, 0.8660254037844320463, 1.000000000000006661 ) ) 
 REPRESENTATION_ITEM ( '' )  );
#57593 = ORIENTED_EDGE ( 'NONE', *, *, #15187, .F. ) ;
#57594 = CARTESIAN_POINT ( 'NONE',  ( 0.000000000000000000, 0.000000000000000000, 0.000000000000000000 ) ) ;
#57595 = CARTESIAN_POINT ( 'NONE',  ( -10.00000000000000000, 0.000000000000000000, 0.000000000000000000 ) ) ;
#57596 = DIRECTION ( 'NONE',  ( 0.000000000000000000, 0.000000000000000000, 1.000000000000000000 ) ) ;
#57597 = EDGE_CURVE ( 'NONE', #25432, #64863, #25734, .T. ) ;
#57598 = DIRECTION ( 'NONE',  ( -1.000000000000000000, 0.000000000000000000, 0.000000000000000000 ) ) ;
#57599 = CARTESIAN_POINT ( 'NONE',  ( 10.00000000000000000, -16.45098606841102651, -33.79645857604531045 ) ) ;
#57600 = ORIENTED_EDGE ( 'NONE', *, *, #12544, .T. ) ;
#57601 = DIRECTION ( 'NONE',  ( -1.000000000000000000, -0.000000000000000000, -0.000000000000000000 ) ) ;
#57602 = FACE_OUTER_BOUND ( 'NONE', #33927, .T. ) ;
#57603 = VERTEX_POINT ( 'NONE', #28350 ) ;
#57604 = AXIS2_PLACEMENT_3D ( 'NONE', #35705, #58652, #7153 ) ;
#57605 = CARTESIAN_POINT ( 'NONE',  ( 92.69370383062501162, -208.6684592857803295, 88.95489583420048518 ) ) ;
#57606 = CARTESIAN_POINT ( 'NONE',  ( 10.00000000000000000, 35.53030884539102630, -12.26510123303222599 ) ) ;
#57607 = EDGE_LOOP ( 'NONE', ( #2350, #54456, #67827, #53960 ) ) ;
#57608 = AXIS2_PLACEMENT_3D ( 'NONE', #43728, #56489, #66648 ) ;
#57609 = DIRECTION ( 'NONE',  ( -1.000000000000000000, 0.000000000000000000, 0.000000000000000000 ) ) ;
#57610 = AXIS2_PLACEMENT_3D ( 'NONE', #25278, #59484, #42940 ) ;
#57611 = ORIENTED_EDGE ( 'NONE', *, *, #25974, .T. ) ;
#57612 = LINE ( 'NONE', #6113, #71886 ) ;
#57613 = VERTEX_POINT ( 'NONE', #74220 ) ;
#57614 = CARTESIAN_POINT ( 'NONE',  ( 5.000000000000000000, -31.52238457039579345, -27.75498641678775158 ) ) ;
#57615 = ORIENTED_EDGE ( 'NONE', *, *, #51808, .F. ) ;
#57616 = CARTESIAN_POINT ( 'NONE',  ( 11.99999999999999822, -17.28742895386031719, -75.54627589209962935 ) ) ;
#57617 = ORIENTED_EDGE ( 'NONE', *, *, #12947, .F. ) ;
#57618 = VECTOR ( 'NONE', #27958, 1000.000000000000000 ) ;
#57619 = EDGE_LOOP ( 'NONE', ( #13464, #43204, #22734, #73393 ) ) ;
#57620 = DIRECTION ( 'NONE',  ( -1.000000000000000000, 0.000000000000000000, 0.000000000000000000 ) ) ;
#57621 = ORIENTED_EDGE ( 'NONE', *, *, #47480, .T. ) ;
#57622 = VERTEX_POINT ( 'NONE', #16339 ) ;
#57623 = CARTESIAN_POINT ( 'NONE',  ( 92.59666252161191835, 89.15460556225134781, 74.93511027845775629 ) ) ;
#57624 = VERTEX_POINT ( 'NONE', #62212 ) ;
#57625 = EDGE_CURVE ( 'NONE', #3632, #57151, #37767, .T. ) ;
#57626 = ORIENTED_EDGE ( 'NONE', *, *, #68184, .T. ) ;
#57627 = CARTESIAN_POINT ( 'NONE',  ( 92.69370383062498320, 91.33154071421968467, 85.14489583420048291 ) ) ;
#57628 = VERTEX_POINT ( 'NONE', #4715 ) ;
#57629 = VECTOR ( 'NONE', #60086, 1000.000000000000000 ) ;
#57630 = CARTESIAN_POINT ( 'NONE',  ( 95.00000000000000000, -212.6630814284392557, 80.27656250086714351 ) ) ;
#57631 = AXIS2_PLACEMENT_3D ( 'NONE', #48561, #30515, #53827 ) ;
#57632 = AXIS2_PLACEMENT_3D ( 'NONE', #65232, #41548, #24625 ) ;
#57633 = APPLICATION_PROTOCOL_DEFINITION ( 'draft international standard', 'automotive_design', 1998, #60386 ) ;
#57634 = CYLINDRICAL_SURFACE ( 'NONE', #73801, 31.99999999999998579 ) ;
#57635 = EDGE_CURVE ( 'NONE', #28632, #51981, #62597, .T. ) ;
#57636 = CARTESIAN_POINT ( 'NONE',  ( -94.95306897617061281, -212.6495843973424655, 75.00000002508416230 ) ) ;
#57637 = CARTESIAN_POINT ( 'NONE',  ( 10.00000000000000000, -51.03279382321125723, 55.19960302592048862 ) ) ;
#57638 = CARTESIAN_POINT ( 'NONE',  ( 94.99999999999998579, 90.00000000000002842, 90.00000000000000000 ) ) ;
#57639 = CYLINDRICAL_SURFACE ( 'NONE', #21602, 82.00000000000000000 ) ;
#57640 = ADVANCED_FACE ( 'NONE', ( #62976 ), #70146, .T. ) ;
#57641 = CARTESIAN_POINT ( 'NONE',  ( 8.700667342345820288, -98.11853780484867116, -2.500000000000000000 ) ) ;
#57642 = CONICAL_SURFACE ( 'NONE', #35994, 2.649999999999999467, 1.029744258676654312 ) ;
#57643 = CARTESIAN_POINT ( 'NONE',  ( -92.69370383062498320, -211.3315407142195852, 84.82739583420045903 ) ) ;
#57644 = CARTESIAN_POINT ( 'NONE',  ( -96.15314808468752972, 91.99731107132950569, 81.44072916753381719 ) ) ;
#57645 = VERTEX_POINT ( 'NONE', #51665 ) ;
#57647 = CARTESIAN_POINT ( 'NONE',  ( -93.84685191531254134, 91.99731107132950569, 84.98614583420047097 ) ) ;
#57646 = CARTESIAN_POINT ( 'NONE',  ( 94.99999999999998579, 87.33691857156068750, 83.45156250086714067 ) ) ;
#57648 = ORIENTED_EDGE ( 'NONE', *, *, #25956, .F. ) ;
#57649 = DIRECTION ( 'NONE',  ( 0.1736481776669309696, -0.9848077530122080203, 0.000000000000000000 ) ) ;
#57650 = CARTESIAN_POINT ( 'NONE',  ( 92.35000000000002274, -209.9999872707216468, 76.10937456147249236 ) ) ;
#57651 = CARTESIAN_POINT ( 'NONE',  ( -2.499999999999968914, 79.99999999999998579, -269.9999999999999432 ) ) ;
#57652 = CARTESIAN_POINT ( 'NONE',  ( -97.30629616937497417, -211.3315407142195852, 85.88572916753381037 ) ) ;
#57653 = DIRECTION ( 'NONE',  ( 1.000000000000000000, 0.000000000000000000, 0.000000000000000000 ) ) ;
#57654 = DIRECTION ( 'NONE',  ( 1.000000000000000000, 0.000000000000000000, 0.000000000000000000 ) ) ;
#57655 = FACE_OUTER_BOUND ( 'NONE', #58279, .T. ) ;
#57656 = CYLINDRICAL_SURFACE ( 'NONE', #37238, 2.649999999999999467 ) ;
#57657 = ORIENTED_EDGE ( 'NONE', *, *, #13428, .T. ) ;
#57658 = VERTEX_POINT ( 'NONE', #68601 ) ;
#57659 = CARTESIAN_POINT ( 'NONE',  ( -93.67500000000003979, 87.70503267997129626, 78.14666666666667538 ) ) ;
#57660 = CARTESIAN_POINT ( 'NONE',  ( 96.32499999999998863, -212.2949673200287179, 88.94166666666666288 ) ) ;
#57661 = DIRECTION ( 'NONE',  ( 1.000000000000000000, 0.000000000000000000, 0.000000000000000000 ) ) ;
#57662 = DIRECTION ( 'NONE',  ( -0.000000000000000000, -0.8660254037844427044, 0.4999999999999929501 ) ) ;
#57663 = CARTESIAN_POINT ( 'NONE',  ( -92.35000000000003695, 90.00000000000004263, 77.61749999999999261 ) ) ;
#57664 = CARTESIAN_POINT ( 'NONE',  ( 15.00000000000000000, 6.762365576493310826, -25.66652317338401090 ) ) ;
#57665 = DIRECTION ( 'NONE',  ( 0.000000000000000000, 0.000000000000000000, 1.000000000000000000 ) ) ;
#57666 = AXIS2_PLACEMENT_3D ( 'NONE', #1789, #32798, #24672 ) ;
#57667 = ORIENTED_EDGE ( 'NONE', *, *, #5936, .T. ) ;
#57668 = CARTESIAN_POINT ( 'NONE',  ( -97.30629616937501680, 90.00000000000004263, 78.21281250086714465 ) ) ;
#57670 = DIRECTION ( 'NONE',  ( 0.000000000000000000, 2.312964634635746211E-15, -1.000000000000000000 ) ) ;
#57669 = CIRCLE ( 'NONE', #45659, 77.49899999999999523 ) ;
#57671 = VECTOR ( 'NONE', #58120, 1000.000000000000227 ) ;
#57672 = EDGE_CURVE ( 'NONE', #73292, #58350, #8384, .T. ) ;
#57673 = EDGE_CURVE ( 'NONE', #13102, #35941, #19359, .T. ) ;
#57674 = DIRECTION ( 'NONE',  ( 1.000000000000000000, 0.000000000000000000, 0.000000000000000000 ) ) ;
#57675 = CARTESIAN_POINT ( 'NONE',  ( 10.00000000000000000, 6.736453364084091788, -36.88895765772625879 ) ) ;
#57676 = DIRECTION ( 'NONE',  ( -1.000000000000000000, 0.000000000000000000, 0.000000000000000000 ) ) ;
#57677 = CARTESIAN_POINT ( 'NONE',  ( 10.00000000000000000, 34.44570377933695227, -69.42325613327405165 ) ) ;
#57678 = CARTESIAN_POINT ( 'NONE',  ( -94.99999999999997158, -207.3369185715606307, 87.10281250086715943 ) ) ;
#57679 = SURFACE_STYLE_FILL_AREA ( #46387 ) ;
#57680 = EDGE_CURVE ( 'NONE', #63817, #22572, #24573, .T. ) ;
#57681 = CARTESIAN_POINT ( 'NONE',  ( 97.30629616937498838, 88.66845928578035796, 78.00114583420049996 ) ) ;
#57682 = CARTESIAN_POINT ( 'NONE',  ( -94.99999999999997158, -212.6630814284392557, 80.43531250086715545 ) ) ;
#57683 = LINE ( 'NONE', #10321, #47055 ) ;
#57684 = VECTOR ( 'NONE', #32753, 1000.000000000000000 ) ;
#57685 = ORIENTED_EDGE ( 'NONE', *, *, #26795, .F. ) ;
#57686 = CARTESIAN_POINT ( 'NONE',  ( 92.34999999999999432, 90.00000000000002842, 87.53937500173429953 ) ) ;
#57687 = CARTESIAN_POINT ( 'NONE',  ( -97.64999999999996305, -209.9999999999999716, 75.39499999999999602 ) ) ;
#57688 = DIRECTION ( 'NONE',  ( -1.000000000000000000, 0.000000000000000000, 0.000000000000000000 ) ) ;
#57689 = CIRCLE ( 'NONE', #64925, 31.99999999999999289 ) ;
#57690 = AXIS2_PLACEMENT_3D ( 'NONE', #11642, #51885, #69902 ) ;
#57691 = VECTOR ( 'NONE', #19665, 1000.000000000000000 ) ;
#57692 = CARTESIAN_POINT ( 'NONE',  ( -93.33921851433964889, 88.39974787049349914, 74.80065602173004891 ) ) ;
#57693 = CARTESIAN_POINT ( 'NONE',  ( 92.69370383062501162, -211.3315407142195852, 76.36072916753381890 ) ) ;
#57694 = EDGE_LOOP ( 'NONE', ( #35311, #29693, #1837, #45871 ) ) ;
#57695 = DIRECTION ( 'NONE',  ( 0.000000000000000000, 0.000000000000000000, 1.000000000000000000 ) ) ;
#57696 = EDGE_LOOP ( 'NONE', ( #17203, #55720, #41404, #68615 ) ) ;
#57697 = CARTESIAN_POINT ( 'NONE',  ( 12.75000000000024336, -120.0000000000000995, 127.4999999999996732 ) ) ;
#57698 = ORIENTED_EDGE ( 'NONE', *, *, #28477, .T. ) ;
#57699 = CARTESIAN_POINT ( 'NONE',  ( 11.99999999999999822, 0.000000000000000000, 0.000000000000000000 ) ) ;
#57700 = VERTEX_POINT ( 'NONE', #35479 ) ;
#57701 = ORIENTED_EDGE ( 'NONE', *, *, #11683, .T. ) ;
#57702 = ORIENTED_EDGE ( 'NONE', *, *, #47118, .F. ) ;
#57703 = CARTESIAN_POINT ( 'NONE',  ( 96.32499999999998863, -207.7050326799711968, 79.70770833506762187 ) ) ;
#57704 = VERTEX_POINT ( 'NONE', #7287 ) ;
#57705 = ORIENTED_EDGE ( 'NONE', *, *, #41581, .F. ) ;
#57706 = CARTESIAN_POINT ( 'NONE',  ( 94.99999999999998579, 92.66308142843935514, 82.65781250086715204 ) ) ;
#57707 = CARTESIAN_POINT ( 'NONE',  ( 97.64999999999999147, -209.9999999999999716, 75.71250000000000568 ) ) ;
#57708 = ORIENTED_EDGE ( 'NONE', *, *, #68176, .T. ) ;
#57709 = ORIENTED_EDGE ( 'NONE', *, *, #56364, .F. ) ;
#57710 = CIRCLE ( 'NONE', #13269, 77.49899999999999523 ) ;
#57711 = EDGE_CURVE ( 'NONE', #51588, #47714, #12578, .T. ) ;
#57712 = VERTEX_POINT ( 'NONE', #6909 ) ;
#57713 = ORIENTED_EDGE ( 'NONE', *, *, #42771, .T. ) ;
#57714 = CARTESIAN_POINT ( 'NONE',  ( 10.00000000000000178, 12.24744871391589029, 2.499999999999999556 ) ) ;
#57715 = AXIS2_PLACEMENT_3D ( 'NONE', #54325, #2851, #26849 ) ;
#57716 = DIRECTION ( 'NONE',  ( 0.000000000000000000, 0.000000000000000000, 1.000000000000000000 ) ) ;
#57717 = CARTESIAN_POINT ( 'NONE',  ( 10.00000000000000000, 76.41127070299273782, 12.93880638057342836 ) ) ;
#57718 = ADVANCED_FACE ( 'NONE', ( #69693 ), #573, .F. ) ;
#57719 = CARTESIAN_POINT ( 'NONE',  ( 0.000000000000000000, 17.28742895386190526, -75.54627589209924565 ) ) ;
#57720 = DIRECTION ( 'NONE',  ( -1.000000000000000000, -0.000000000000000000, 0.000000000000000000 ) ) ;
#57721 = DIRECTION ( 'NONE',  ( -1.000000000000000000, 0.000000000000000000, -0.000000000000000000 ) ) ;
#57722 = FACE_OUTER_BOUND ( 'NONE', #5433, .T. ) ;
#57723 = DIRECTION ( 'NONE',  ( 1.000000000000000000, 0.000000000000000000, 0.000000000000000000 ) ) ;
#57725 = ORIENTED_EDGE ( 'NONE', *, *, #42983, .T. ) ;
#57724 = EDGE_CURVE ( 'NONE', #19845, #45901, #8018, .T. ) ;
#57726 = CARTESIAN_POINT ( 'NONE',  ( -94.99999999999997158, -206.9400435732949575, 78.49062500173430124 ) ) ;
#57727 = VERTEX_POINT ( 'NONE', #13650 ) ;
#57728 = CARTESIAN_POINT ( 'NONE',  ( 7.400000000000003908, 1.056673655987569448E-14, 5.892267102770835596E-15 ) ) ;
#57729 = ORIENTED_EDGE ( 'NONE', *, *, #52108, .F. ) ;
#57731 = CARTESIAN_POINT ( 'NONE',  ( -93.67500000000003979, 87.70503267997129626, 79.49604166840096298 ) ) ;
#57730 = CARTESIAN_POINT ( 'NONE',  ( 94.99999999999998579, 93.05995642670504253, 80.39562500173431658 ) ) ;
#57732 = EDGE_CURVE ( 'NONE', #57170, #46225, #29365, .T. ) ;
#57733 = ORIENTED_EDGE ( 'NONE', *, *, #13332, .F. ) ;
#57734 = CARTESIAN_POINT ( 'NONE',  ( 94.99999999999998579, 92.66308142843935514, 80.75281250086715090 ) ) ;
#57735 = DIRECTION ( 'NONE',  ( 0.000000000000000000, 0.000000000000000000, 1.000000000000000000 ) ) ;
#57736 = CARTESIAN_POINT ( 'NONE',  ( 10.00000000000000000, -70.53064760720297954, -26.01480285779911839 ) ) ;
#57737 = CARTESIAN_POINT ( 'NONE',  ( 10.00000000000000000, -73.44644590900043113, -24.73286445877782924 ) ) ;
#57738 = VERTEX_POINT ( 'NONE', #63702 ) ;
#57740 = EDGE_CURVE ( 'NONE', #57704, #22794, #65483, .T. ) ;
#57739 = CARTESIAN_POINT ( 'NONE',  ( -93.67500000000003979, 92.29496732002878900, 80.26333333333332121 ) ) ;
#57741 = CARTESIAN_POINT ( 'NONE',  ( -3.000000000000000000, 23.50000000000000000, 1.499999999999997780 ) ) ;
#57742 = CARTESIAN_POINT ( 'NONE',  ( 10.00000000000000000, 0.000000000000000000, 0.000000000000000000 ) ) ;
#57743 = EDGE_LOOP ( 'NONE', ( #18561, #64639, #64301, #25900 ) ) ;
#57744 = ORIENTED_EDGE ( 'NONE', *, *, #5640, .F. ) ;
#57745 = AXIS2_PLACEMENT_3D ( 'NONE', #10497, #2413, #26026 ) ;
#57746 = EDGE_CURVE ( 'NONE', #16255, #31252, #28193, .T. ) ;
#57747 = EDGE_CURVE ( 'NONE', #52056, #51811, #70204, .T. ) ;
#57748 = CARTESIAN_POINT ( 'NONE',  ( 0.000000000000000000, -77.49459641780886443, -0.8261519478439277586 ) ) ;
#57749 = CARTESIAN_POINT ( 'NONE',  ( 10.00000000000000000, -10.41901085202050403, -40.68715046381940681 ) ) ;
#57750 = CARTESIAN_POINT ( 'NONE',  ( -100.0000000000000142, 95.00000000000002842, 90.00000000000000000 ) ) ;
#57751 = CARTESIAN_POINT ( 'NONE',  ( -97.30629616937497417, -211.3315407142195852, 76.51947916753381662 ) ) ;
#57752 = ORIENTED_EDGE ( 'NONE', *, *, #662, .T. ) ;
#57753 = FACE_OUTER_BOUND ( 'NONE', #34587, .T. ) ;
#57754 = EDGE_CURVE ( 'NONE', #5647, #30680, #71381, .T. ) ;
#57755 = EDGE_CURVE ( 'NONE', #28566, #60498, #23380, .T. ) ;
#57756 = CARTESIAN_POINT ( 'NONE',  ( 26.28306158492127764, -123.3838844133976522, 2.500000000000000000 ) ) ;
#57757 = CARTESIAN_POINT ( 'NONE',  ( 0.000000000000000000, 24.73286445877704764, 73.44644590900067271 ) ) ;
#57758 = CARTESIAN_POINT ( 'NONE',  ( 97.30629616937498838, 88.66845928578035796, 75.93739583420050110 ) ) ;
#57759 = DIRECTION ( 'NONE',  ( -1.000000000000000000, 0.000000000000000000, 0.000000000000000000 ) ) ;
#57760 = CYLINDRICAL_SURFACE ( 'NONE', #55285, 82.00000000000000000 ) ;
#57761 = CYLINDRICAL_SURFACE ( 'NONE', #180, 16.00000000000000000 ) ;
#57762 = CARTESIAN_POINT ( 'NONE',  ( 97.65000000002595471, -210.0000000000000853, -74.99999999999342037 ) ) ;
#57763 = DIRECTION ( 'NONE',  ( 0.000000000000000000, 0.000000000000000000, 1.000000000000000000 ) ) ;
#57764 = DIRECTION ( 'NONE',  ( -1.000000000000000000, 0.000000000000000000, 0.000000000000000000 ) ) ;
#57765 = CARTESIAN_POINT ( 'NONE',  ( 94.99999999999998579, 87.33691857156068750, 86.15031250086717307 ) ) ;
#57766 = DIRECTION ( 'NONE',  ( 1.000000000000000000, 0.000000000000000000, 0.000000000000000000 ) ) ;
#57767 = LINE ( 'NONE', #22444, #55422 ) ;
#57768 = ORIENTED_EDGE ( 'NONE', *, *, #63252, .F. ) ;
#57769 = AXIS2_PLACEMENT_3D ( 'NONE', #65705, #49144, #54787 ) ;
#57770 = DIRECTION ( 'NONE',  ( -1.000000000000000000, -0.000000000000000000, 0.000000000000000000 ) ) ;
#57771 = CIRCLE ( 'NONE', #26571, 77.49900000000000944 ) ;
#57772 = CARTESIAN_POINT ( 'NONE',  ( -92.69370383062505425, 91.33154071421968467, 81.12322916753380753 ) ) ;
#57773 = CIRCLE ( 'NONE', #9728, 31.99999999999998579 ) ;
#57774 = CARTESIAN_POINT ( 'NONE',  ( 92.69370383062501162, -208.6684592857803011, 87.04989583420048405 ) ) ;
#57775 = ORIENTED_EDGE ( 'NONE', *, *, #13913, .T. ) ;
#57776 = FACE_OUTER_BOUND ( 'NONE', #58560, .T. ) ;
#57777 = CARTESIAN_POINT ( 'NONE',  ( 93.67499999999999716, 87.70503267997126784, 87.01020833506763097 ) ) ;
#57778 = CARTESIAN_POINT ( 'NONE',  ( 0.000000000000000000, 74.18225833017937987, -34.94270380257559339 ) ) ;
#57779 = CIRCLE ( 'NONE', #28950, 82.00000000000000000 ) ;
#57780 = CIRCLE ( 'NONE', #40991, 20.20000000000036522 ) ;
#57781 = DIRECTION ( 'NONE',  ( 0.000000000000000000, 0.000000000000000000, 1.000000000000000000 ) ) ;
#57782 = DIRECTION ( 'NONE',  ( 1.000000000000000000, 0.000000000000000000, 0.000000000000000000 ) ) ;
#57783 = ORIENTED_EDGE ( 'NONE', *, *, #39901, .F. ) ;
#57784 = EDGE_CURVE ( 'NONE', #2928, #17937, #13630, .T. ) ;
#57785 = CIRCLE ( 'NONE', #36207, 14.09999999999999964 ) ;
#57786 = VERTEX_POINT ( 'NONE', #52025 ) ;
#57787 = ADVANCED_FACE ( 'NONE', ( #17814 ), #69055, .F. ) ;
#57788 = CARTESIAN_POINT ( 'NONE',  ( 92.69370383062501162, -211.3315407142195852, 80.32947916753381890 ) ) ;
#57789 = DIRECTION ( 'NONE',  ( -1.000000000000000000, -0.000000000000000000, -0.000000000000000000 ) ) ;
#57790 = CARTESIAN_POINT ( 'NONE',  ( 97.65000000000009095, 91.52997821335246442, 80.84541666666663673 ) ) ;
#57791 = ADVANCED_FACE ( 'NONE', ( #12175 ), #46775, .F. ) ;
#57792 =( BOUNDED_CURVE ( )  B_SPLINE_CURVE ( 2, ( #28539, #29277, #761, #40955, #28173, #63888, #58230 ),
 .UNSPECIFIED., .F., .F. ) 
 B_SPLINE_CURVE_WITH_KNOTS ( ( 3, 2, 2, 3 ),
 ( 0.7831899741065913023, 0.7902457405788253508, 0.7973015061197077369, 0.8043570860654217780 ),
 .UNSPECIFIED. ) 
 CURVE ( )  GEOMETRIC_REPRESENTATION_ITEM ( )  RATIONAL_B_SPLINE_CURVE ( ( 1.000000000000000000, 0.8660254037844387076, 1.000000000000000000, 0.8660254037844387076, 1.000000000000000000, 0.8660289278581336792, 0.9999929520380047565 ) ) 
 REPRESENTATION_ITEM ( '' )  );
#57793 = CARTESIAN_POINT ( 'NONE',  ( 0.000000000000000000, -71.21200624218768382, -40.65526001592689909 ) ) ;
#57794 = CARTESIAN_POINT ( 'NONE',  ( 94.99999999999998579, 93.05995642670504253, 83.57062500173429953 ) ) ;
#57795 = DIRECTION ( 'NONE',  ( 0.000000000000000000, 0.000000000000000000, -1.000000000000000000 ) ) ;
#57796 = CARTESIAN_POINT ( 'NONE',  ( 92.35000000000000853, -209.9999999999999716, 84.92000000000000171 ) ) ;
#57797 = EDGE_CURVE ( 'NONE', #18834, #1870, #58043, .T. ) ;
#57798 = ORIENTED_EDGE ( 'NONE', *, *, #31878, .F. ) ;
#57799 = ORIENTED_EDGE ( 'NONE', *, *, #45783, .T. ) ;
#57800 = ORIENTED_EDGE ( 'NONE', *, *, #69019, .F. ) ;
#57801 = ORIENTED_EDGE ( 'NONE', *, *, #65110, .T. ) ;
#57802 = DIRECTION ( 'NONE',  ( 1.000000000000000000, 0.000000000000000000, 0.000000000000000000 ) ) ;
#57803 = CARTESIAN_POINT ( 'NONE',  ( -97.30629616937501680, 88.66845928578038638, 88.58447916753382856 ) ) ;
#57804 = EDGE_CURVE ( 'NONE', #32364, #49560, #23833, .T. ) ;
#57805 = CARTESIAN_POINT ( 'NONE',  ( 2.712167343862820434, 4.207632145829745873, -6.000000000000002665 ) ) ;
#57806 = FACE_OUTER_BOUND ( 'NONE', #65461, .T. ) ;
#57807 = CARTESIAN_POINT ( 'NONE',  ( 92.35000000000002274, -208.4700217866474645, 77.96145833506763267 ) ) ;
#57808 = CARTESIAN_POINT ( 'NONE',  ( 94.99999999999998579, 93.05995642670504253, 77.14124999999999943 ) ) ;
#57809 = VERTEX_POINT ( 'NONE', #37344 ) ;
#57810 = CARTESIAN_POINT ( 'NONE',  ( 0.000000000000000000, 0.000000000000000000, -175.0000000000000000 ) ) ;
#57811 = VERTEX_POINT ( 'NONE', #9491 ) ;
#57812 = CARTESIAN_POINT ( 'NONE',  ( 0.000000000000000000, 0.000000000000000000, 40.80000000000001847 ) ) ;
#57813 = ORIENTED_EDGE ( 'NONE', *, *, #25484, .F. ) ;
#57814 = CARTESIAN_POINT ( 'NONE',  ( 92.35000752690150705, -211.5299825590110743, 88.22729196900364457 ) ) ;
#57815 = CARTESIAN_POINT ( 'NONE',  ( -93.84685191531254134, 91.99731107132950569, 80.06489583420048461 ) ) ;
#57816 = ADVANCED_FACE ( 'NONE', ( #21133, #3509 ), #26414, .T. ) ;
#57817 = CARTESIAN_POINT ( 'NONE',  ( 92.69370383062498320, 90.00000000000002842, 88.53156250086716739 ) ) ;
#57818 = ORIENTED_EDGE ( 'NONE', *, *, #7280, .T. ) ;
#57819 = LINE ( 'NONE', #36350, #53759 ) ;
#57820 = CARTESIAN_POINT ( 'NONE',  ( 10.00000000000000000, -36.88895765772637247, 6.736453364083436313 ) ) ;
#57821 = CARTESIAN_POINT ( 'NONE',  ( 92.34999999999998010, -211.5299782133523934, 85.60791666666665378 ) ) ;
#57822 =( GEOMETRIC_REPRESENTATION_CONTEXT ( 3 ) GLOBAL_UNCERTAINTY_ASSIGNED_CONTEXT ( ( #61049 ) ) GLOBAL_UNIT_ASSIGNED_CONTEXT ( ( #33615, #44543, #39272 ) ) REPRESENTATION_CONTEXT ( 'NONE', 'WORKASPACE' ) );
#57823 = CIRCLE ( 'NONE', #16979, 82.00000000000000000 ) ;
#57824 = CARTESIAN_POINT ( 'NONE',  ( 5.000000000000000000, -33.71516098798792171, 74.74816331893418919 ) ) ;
#57825 = VERTEX_POINT ( 'NONE', #31680 ) ;
#57826 = LINE ( 'NONE', #45443, #43522 ) ;
#57827 = VECTOR ( 'NONE', #53124, 1000.000000000000000 ) ;
#57828 = CARTESIAN_POINT ( 'NONE',  ( -96.15314808468747287, -208.0026889286704943, 77.47197916753380298 ) ) ;
#57829 = ORIENTED_EDGE ( 'NONE', *, *, #65449, .T. ) ;
#57830 = AXIS2_PLACEMENT_3D ( 'NONE', #69300, #6884, #1662 ) ;
#57831 = EDGE_LOOP ( 'NONE', ( #67544, #16459, #29738, #5846 ) ) ;
#57832 = DIRECTION ( 'NONE',  ( -1.000000000000000000, 0.000000000000000000, 0.000000000000000000 ) ) ;
#57833 = EDGE_CURVE ( 'NONE', #56093, #45747, #25678, .T. ) ;
#57834 = VECTOR ( 'NONE', #23891, 1000.000000000000000 ) ;
#57835 = ORIENTED_EDGE ( 'NONE', *, *, #57120, .T. ) ;
#57836 = EDGE_CURVE ( 'NONE', #37739, #51621, #26595, .T. ) ;
#57837 = DIRECTION ( 'NONE',  ( -0.9730327541852497042, 0.2306669878475623159, 0.000000000000000000 ) ) ;
#57838 = LINE ( 'NONE', #39432, #71244 ) ;
#57839 = EDGE_LOOP ( 'NONE', ( #19718, #64271, #2748, #48630 ) ) ;
#57840 = CARTESIAN_POINT ( 'NONE',  ( -92.69370383062498320, -211.3315407142195852, 88.79614583420050167 ) ) ;
#57841 = ORIENTED_EDGE ( 'NONE', *, *, #50061, .F. ) ;
#57842 = CARTESIAN_POINT ( 'NONE',  ( -96.32499999999996021, -207.7050326799711968, 81.63916666666666799 ) ) ;
#57843 = CARTESIAN_POINT ( 'NONE',  ( 0.000000000000000000, -41.81611651403859042, -3.925862922256606602 ) ) ;
#57844 = VERTEX_POINT ( 'NONE', #9122 ) ;
#57845 = VERTEX_POINT ( 'NONE', #15128 ) ;
#57846 = CARTESIAN_POINT ( 'NONE',  ( -3.000000000000000000, 8.688484142253939169, 21.88630264137371029 ) ) ;
#57847 = CIRCLE ( 'NONE', #51871, 42.00000000000000000 ) ;
#57848 = LINE ( 'NONE', #56367, #48164 ) ;
#57849 = CARTESIAN_POINT ( 'NONE',  ( 92.69370383062498320, 91.33154071421968467, 85.77989583420048803 ) ) ;
#57850 = DIRECTION ( 'NONE',  ( -1.000000000000000000, 0.000000000000000000, -0.000000000000000000 ) ) ;
#57851 = AXIS2_PLACEMENT_3D ( 'NONE', #68596, #17083, #5815 ) ;
#57852 = CARTESIAN_POINT ( 'NONE',  ( 11.99999999999999822, 69.42325613327440692, 34.44570377933622041 ) ) ;
#57853 = DIRECTION ( 'NONE',  ( 1.000000000000000000, 0.000000000000000000, 0.000000000000000000 ) ) ;
#57854 = CARTESIAN_POINT ( 'NONE',  ( 10.00000000000000000, 70.52718814184294160, -26.02418014898236720 ) ) ;
#57855 = CARTESIAN_POINT ( 'NONE',  ( -7.499999999999992895, 2.289750019674042456E-15, 0.000000000000000000 ) ) ;
#57856 = DIRECTION ( 'NONE',  ( 2.603472992746261562E-14, 2.546204323184492723E-14, -1.000000000000000000 ) ) ;
#57857 = DIRECTION ( 'NONE',  ( -1.000000000000000000, -0.000000000000000000, 0.000000000000000000 ) ) ;
#57858 = CARTESIAN_POINT ( 'NONE',  ( 10.00000000000000000, 51.02545421589402252, -55.20638768913705263 ) ) ;
#57859 = CARTESIAN_POINT ( 'NONE',  ( 12.00000000000000000, -22.32062822937469093, 14.36278369418830181 ) ) ;
#57860 = CARTESIAN_POINT ( 'NONE',  ( 0.000000000000000000, -30.80686688397025108, 21.53537804866070715 ) ) ;
#57861 = DIRECTION ( 'NONE',  ( -1.000000000000000000, 0.000000000000000000, 0.000000000000000000 ) ) ;
#57862 = ADVANCED_FACE ( 'NONE', ( #49701 ), #66999, .T. ) ;
#57863 = DIRECTION ( 'NONE',  ( 0.1850432970638667407, -0.9827303690289282967, 0.000000000000000000 ) ) ;
#57864 = VERTEX_POINT ( 'NONE', #60283 ) ;
#57865 = DIRECTION ( 'NONE',  ( 0.000000000000000000, -0.2334453638558922350, -0.9723699203976797767 ) ) ;
#57866 = CYLINDRICAL_SURFACE ( 'NONE', #29902, 16.00000000000000000 ) ;
#57867 = CARTESIAN_POINT ( 'NONE',  ( 12.00000000000000000, 6.762365576493310826, -25.66652317338400735 ) ) ;
#57868 = LINE ( 'NONE', #69510, #22183 ) ;
#57869 =( GEOMETRIC_REPRESENTATION_CONTEXT ( 3 ) GLOBAL_UNCERTAINTY_ASSIGNED_CONTEXT ( ( #4620 ) ) GLOBAL_UNIT_ASSIGNED_CONTEXT ( ( #71885, #3137, #71516 ) ) REPRESENTATION_CONTEXT ( 'NONE', 'WORKASPACE' ) );
#57870 = CIRCLE ( 'NONE', #51852, 31.99999999999998934 ) ;
#57871 = PLANE ( 'NONE',  #31943 ) ;
#57872 = CARTESIAN_POINT ( 'NONE',  ( 92.69370383062501162, -208.6684592857803011, 85.93864583420048575 ) ) ;
#57873 = AXIS2_PLACEMENT_3D ( 'NONE', #32758, #50435, #55709 ) ;
#57874 = ORIENTED_EDGE ( 'NONE', *, *, #53622, .T. ) ;
#57875 = ADVANCED_FACE ( 'NONE', ( #14014 ), #15501, .T. ) ;
#57876 = ORIENTED_EDGE ( 'NONE', *, *, #15871, .F. ) ;
#57877 = EDGE_CURVE ( 'NONE', #19049, #27761, #20770, .T. ) ;
#57878 = VECTOR ( 'NONE', #67808, 1000.000000000000000 ) ;
#57879 = CARTESIAN_POINT ( 'NONE',  ( -97.65000000000004832, -208.4700217866474929, 86.13708333333332234 ) ) ;
#57880 = ORIENTED_EDGE ( 'NONE', *, *, #73220, .F. ) ;
#57881 = FACE_OUTER_BOUND ( 'NONE', #71246, .T. ) ;
#57882 = AXIS2_PLACEMENT_3D ( 'NONE', #60401, #2907, #43109 ) ;
#57883 = CARTESIAN_POINT ( 'NONE',  ( 1.560000000000000053, 0.000000000000000000, -1.499999999999999556 ) ) ;
#57884 = ORIENTED_EDGE ( 'NONE', *, *, #9744, .T. ) ;
#57885 = CARTESIAN_POINT ( 'NONE',  ( 97.30629616937498838, -208.6684592857803011, 83.82197916753382572 ) ) ;
#57886 = ADVANCED_FACE ( 'NONE', ( #26038 ), #25317, .T. ) ;
#57887 = EDGE_CURVE ( 'NONE', #51530, #33478, #71897, .T. ) ;
#57888 = VERTEX_POINT ( 'NONE', #43364 ) ;
#57889 = CARTESIAN_POINT ( 'NONE',  ( 5.000000000000000000, 2.663952781846149254, 41.91543099594818500 ) ) ;
#57890 = ORIENTED_EDGE ( 'NONE', *, *, #43055, .T. ) ;
#57891 = VECTOR ( 'NONE', #32615, 1000.000000000000000 ) ;
#57892 = ORIENTED_EDGE ( 'NONE', *, *, #42788, .T. ) ;
#57893 = FACE_OUTER_BOUND ( 'NONE', #29055, .T. ) ;
#57894 = CIRCLE ( 'NONE', #11088, 82.00000000000000000 ) ;
#57895 = SHAPE_REPRESENTATION_RELATIONSHIP ( 'NONE' , 'NONE' ,  #31559, #34586 ) ;
#57896 = CYLINDRICAL_SURFACE ( 'NONE', #43663, 2.649999999999985700 ) ;
#57897 = VERTEX_POINT ( 'NONE', #72627 ) ;
#57898 = DIRECTION ( 'NONE',  ( 2.628368902995175337E-16, 1.000000000000000000, 0.000000000000000000 ) ) ;
#57899 = CARTESIAN_POINT ( 'NONE',  ( 97.64999999999997726, -208.4700217866474645, 87.27479166840096525 ) ) ;
#57900 = EDGE_LOOP ( 'NONE', ( #54, #51431, #67316, #36238 ) ) ;
#57901 = CARTESIAN_POINT ( 'NONE',  ( -97.65000000000001990, 90.00000000000004263, 84.28499999999999659 ) ) ;
#57902 = ORIENTED_EDGE ( 'NONE', *, *, #13218, .T. ) ;
#57903 = DIRECTION ( 'NONE',  ( 0.000000000000000000, -0.7604059656000368150, 0.6494480483301767748 ) ) ;
#57904 = ADVANCED_FACE ( 'NONE', ( #3879 ), #42607, .T. ) ;
#57905 = ORIENTED_EDGE ( 'NONE', *, *, #8821, .T. ) ;
#57906 = VERTEX_POINT ( 'NONE', #37713 ) ;
#57907 = FILL_AREA_STYLE_COLOUR ( '', #25448 ) ;
#57908 = ORIENTED_EDGE ( 'NONE', *, *, #5012, .F. ) ;
#57909 = CARTESIAN_POINT ( 'NONE',  ( 0.000000000000000000, 0.000000000000000000, 0.000000000000000000 ) ) ;
#57910 = CYLINDRICAL_SURFACE ( 'NONE', #42632, 82.00000000000000000 ) ;
#57911 = VERTEX_POINT ( 'NONE', #61381 ) ;
#57912 = ORIENTED_EDGE ( 'NONE', *, *, #38907, .F. ) ;
#57913 = EDGE_LOOP ( 'NONE', ( #46425, #52172, #47336, #54934, #727 ) ) ;
#57914 = CARTESIAN_POINT ( 'NONE',  ( 0.000000000000000000, 51.02545421589324803, 55.20638768913779870 ) ) ;
#57915 = CARTESIAN_POINT ( 'NONE',  ( 0.000000000000000000, -76.69515212746036070, 29.01471420065537643 ) ) ;
#57916 = CARTESIAN_POINT ( 'NONE',  ( -96.32500000000001705, 87.70503267997129626, 87.56583333333333030 ) ) ;
#57917 = EDGE_CURVE ( 'NONE', #51812, #66208, #72609, .T. ) ;
#57918 = VERTEX_POINT ( 'NONE', #65543 ) ;
#57919 = DIRECTION ( 'NONE',  ( 0.000000000000000000, 0.000000000000000000, 1.000000000000000000 ) ) ;
#57920 = EDGE_LOOP ( 'NONE', ( #16553, #34931, #32039, #64487 ) ) ;
#57921 = CARTESIAN_POINT ( 'NONE',  ( 96.32499999999997442, 92.29496732002878900, 75.18333333333332291 ) ) ;
#57922 = CARTESIAN_POINT ( 'NONE',  ( -96.15314808468747287, -208.0026889286704943, 87.63197916753379957 ) ) ;
#57923 = ORIENTED_EDGE ( 'NONE', *, *, #2588, .F. ) ;
#57924 = ADVANCED_FACE ( 'NONE', ( #36959 ), #59908, .T. ) ;
#57925 = LINE ( 'NONE', #64307, #21792 ) ;
#57926 = CARTESIAN_POINT ( 'NONE',  ( 92.71977365048361719, -211.1627451397776269, 74.94226573542110259 ) ) ;
#57927 = CARTESIAN_POINT ( 'NONE',  ( 97.65000000000004832, 88.47002178664756400, 81.37458333333333371 ) ) ;
#57928 = CARTESIAN_POINT ( 'NONE',  ( -97.30629616937497417, -208.6684592857803295, 75.61989583420047722 ) ) ;
#57929 = DIRECTION ( 'NONE',  ( 0.000000000000000000, 0.3090169943749411785, 0.9510565162951556406 ) ) ;
#57930 = DIRECTION ( 'NONE',  ( -1.000000000000000000, -0.000000000000000000, 0.000000000000000000 ) ) ;
#57931 = AXIS2_PLACEMENT_3D ( 'NONE', #40048, #58440, #57340 ) ;
#57932 = CARTESIAN_POINT ( 'NONE',  ( 0.000000000000000000, 0.000000000000000000, 0.000000000000000000 ) ) ;
#57933 = DIRECTION ( 'NONE',  ( 1.343011723336882952E-16, -1.000000000000000000, 0.000000000000000000 ) ) ;
#57934 = DIRECTION ( 'NONE',  ( 0.000000000000000000, 0.000000000000000000, -1.000000000000000000 ) ) ;
#57935 = CYLINDRICAL_SURFACE ( 'NONE', #11561, 42.00000000000000000 ) ;
#57936 = CARTESIAN_POINT ( 'NONE',  ( -96.15314808468751551, 88.00268892867056536, 78.95364583420047211 ) ) ;
#57937 = DIRECTION ( 'NONE',  ( -1.000000000000000000, 0.000000000000000000, 0.000000000000000000 ) ) ;
#57938 = DIRECTION ( 'NONE',  ( -1.000000000000000000, 0.000000000000000000, -0.000000000000000000 ) ) ;
#57939 = AXIS2_PLACEMENT_3D ( 'NONE', #65319, #13427, #29972 ) ;
#57940 = ORIENTED_EDGE ( 'NONE', *, *, #33896, .T. ) ;
#57941 = DIRECTION ( 'NONE',  ( 0.000000000000000000, 0.000000000000000000, -1.000000000000000000 ) ) ;
#57942 = CIRCLE ( 'NONE', #61585, 32.00000000000000000 ) ;
#57943 = CARTESIAN_POINT ( 'NONE',  ( 10.00000000000000000, -33.80338159004296017, 16.23288003029484727 ) ) ;
#57944 = LINE ( 'NONE', #73362, #56236 ) ;
#57945 = CYLINDRICAL_SURFACE ( 'NONE', #58674, 42.00000000000000000 ) ;
#57946 = DIRECTION ( 'NONE',  ( 0.000000000000000000, 0.4539904997395414754, 0.8910065241883706744 ) ) ;
#57947 = CARTESIAN_POINT ( 'NONE',  ( 0.000000000000000000, -55.20638768913724448, -51.02545421589383068 ) ) ;
#57948 = CARTESIAN_POINT ( 'NONE',  ( -97.30629616937497417, -208.6684592857803011, 77.68364583420047609 ) ) ;
#57949 = DIRECTION ( 'NONE',  ( -0.000000000000000000, -0.000000000000000000, 1.000000000000000000 ) ) ;
#57950 = ORIENTED_EDGE ( 'NONE', *, *, #4115, .F. ) ;
#57951 = CARTESIAN_POINT ( 'NONE',  ( 0.000000000000000000, -26.79245525562690844, -32.34446384430000876 ) ) ;
#57952 = DIRECTION ( 'NONE',  ( -1.000000000000000000, 7.955419762439749020E-15, 2.563413034563919251E-14 ) ) ;
#57953 =( LENGTH_UNIT ( ) NAMED_UNIT ( * ) SI_UNIT ( .MILLI., .METRE. ) );
#57954 = DIRECTION ( 'NONE',  ( 1.000000000000000000, 0.000000000000000000, -0.000000000000000000 ) ) ;
#57955 = EDGE_CURVE ( 'NONE', #55521, #51812, #71526, .T. ) ;
#57956 = EDGE_CURVE ( 'NONE', #56878, #66338, #72996, .T. ) ;
#57957 = CARTESIAN_POINT ( 'NONE',  ( 12.75000000000274447, -119.9999999999951257, -70.59999999999966747 ) ) ;
#57958 = EDGE_LOOP ( 'NONE', ( #38351, #54465, #25148, #1279 ) ) ;
#57960 = EDGE_CURVE ( 'NONE', #64440, #22274, #37816, .T. ) ;
#57959 = CARTESIAN_POINT ( 'NONE',  ( 10.00000000000000000, 0.000000000000000000, 0.000000000000000000 ) ) ;
#57961 = FACE_OUTER_BOUND ( 'NONE', #3662, .T. ) ;
#57962 = ORIENTED_EDGE ( 'NONE', *, *, #34809, .F. ) ;
#57963 = CARTESIAN_POINT ( 'NONE',  ( 92.69370383062501162, -209.9999999999999716, 85.19781250086714408 ) ) ;
#57964 = DIRECTION ( 'NONE',  ( 1.000000000000000000, 1.427937372958405461E-15, 7.962523111839130290E-16 ) ) ;
#57965 = ORIENTED_EDGE ( 'NONE', *, *, #39298, .T. ) ;
#57966 = DIRECTION ( 'NONE',  ( 0.000000000000000000, 0.000000000000000000, -1.000000000000000000 ) ) ;
#57967 = EDGE_CURVE ( 'NONE', #54604, #37783, #23437, .T. ) ;
#57968 = STYLED_ITEM ( 'NONE', ( #15636 ), #52570 ) ;
#57969 = ORIENTED_EDGE ( 'NONE', *, *, #12364, .T. ) ;
#57970 = DIRECTION ( 'NONE',  ( 0.000000000000000000, 0.000000000000000000, 1.000000000000000000 ) ) ;
#57971 = VERTEX_POINT ( 'NONE', #27137 ) ;
#57972 = CARTESIAN_POINT ( 'NONE',  ( -93.84685191531254134, 91.99731107132950569, 79.42989583420049371 ) ) ;
#57973 = CIRCLE ( 'NONE', #48359, 77.49899999999999523 ) ;
#57974 = ORIENTED_EDGE ( 'NONE', *, *, #67736, .F. ) ;
#57975 = ORIENTED_EDGE ( 'NONE', *, *, #33725, .F. ) ;
#57976 = EDGE_LOOP ( 'NONE', ( #13592, #60615, #53191, #56430 ) ) ;
#57977 = CARTESIAN_POINT ( 'NONE',  ( -24.50849501662245444, -109.8101191361138831, 2.500000000000000000 ) ) ;
#57978 = VERTEX_POINT ( 'NONE', #44830 ) ;
#57979 = DIRECTION ( 'NONE',  ( 0.000000000000000000, 0.000000000000000000, -1.000000000000000000 ) ) ;
#57980 = EDGE_CURVE ( 'NONE', #68833, #32793, #68123, .T. ) ;
#57981 = VERTEX_POINT ( 'NONE', #1128 ) ;
#57982 = PLANE ( 'NONE',  #51667 ) ;
#57983 = ADVANCED_FACE ( 'NONE', ( #41307 ), #6724, .T. ) ;
#57984 = EDGE_CURVE ( 'NONE', #2989, #68435, #38999, .T. ) ;
#57985 = ORIENTED_EDGE ( 'NONE', *, *, #4675, .F. ) ;
#57986 = EDGE_LOOP ( 'NONE', ( #36190, #39395, #27912, #61686 ) ) ;
#57987 = AXIS2_PLACEMENT_3D ( 'NONE', #7715, #65239, #13713 ) ;
#57988 = VERTEX_POINT ( 'NONE', #68505 ) ;
#57989 = CARTESIAN_POINT ( 'NONE',  ( 97.30629616937498838, -208.6684592857803011, 81.75822916753381264 ) ) ;
#57990 = VECTOR ( 'NONE', #63870, 1000.000000000000000 ) ;
#57991 = SHAPE_DEFINITION_REPRESENTATION ( #45226, #66992 ) ;
#57992 = CARTESIAN_POINT ( 'NONE',  ( -10.00000000000000000, 0.000000000000000000, 0.000000000000000000 ) ) ;
#57993 = CARTESIAN_POINT ( 'NONE',  ( 10.00000000000000000, -33.17418723428294669, -17.67226234102862747 ) ) ;
#57994 = DIRECTION ( 'NONE',  ( -0.000000000000000000, -0.000000000000000000, -1.000000000000000000 ) ) ;
#57995 = CARTESIAN_POINT ( 'NONE',  ( 0.000000000000000000, -120.0000000000000000, 5.500000000000000888 ) ) ;
#57996 = DIRECTION ( 'NONE',  ( -1.000000000000000000, -0.000000000000000000, -0.000000000000000000 ) ) ;
#57997 = CARTESIAN_POINT ( 'NONE',  ( -97.64999999999996305, -209.9999999999999716, 85.55499999999999261 ) ) ;
#57998 = CARTESIAN_POINT ( 'NONE',  ( -93.84685191531248449, -208.0026889286704943, 83.71614583420047495 ) ) ;
#57999 = CARTESIAN_POINT ( 'NONE',  ( -97.30629616937501680, 90.00000000000004263, 82.18156250086715886 ) ) ;
#58000 = EDGE_CURVE ( 'NONE', #70160, #62821, #67375, .T. ) ;
#58001 = ORIENTED_EDGE ( 'NONE', *, *, #44931, .T. ) ;
#58002 = CARTESIAN_POINT ( 'NONE',  ( 93.84685191531248449, 88.00268892867053694, 84.66864583420047552 ) ) ;
#58003 = ORIENTED_EDGE ( 'NONE', *, *, #30950, .T. ) ;
#58004 = CARTESIAN_POINT ( 'NONE',  ( -92.35000000053409508, 90.00005320149026034, 78.96687695417308817 ) ) ;
#58005 = DIRECTION ( 'NONE',  ( 0.000000000000000000, 0.000000000000000000, 1.000000000000000000 ) ) ;
#58006 = CARTESIAN_POINT ( 'NONE',  ( 11.99999999999999822, 59.75363087400153006, -56.15606465354896670 ) ) ;
#58007 = CARTESIAN_POINT ( 'NONE',  ( 0.000000000000000000, -23.29833615347104825, -3.418703333116803744 ) ) ;
#58008 = CARTESIAN_POINT ( 'NONE',  ( -92.69370383062498320, -208.6684592857803295, 85.56822916753380071 ) ) ;
#58009 = CARTESIAN_POINT ( 'NONE',  ( -3.000000000000000000, -13.04903810567675038, 19.60159698893425428 ) ) ;
#58010 = DIRECTION ( 'NONE',  ( -1.000000000000000000, -0.000000000000000000, -0.000000000000000000 ) ) ;
#58011 = CARTESIAN_POINT ( 'NONE',  ( 10.00000000000000000, 30.00120703465236716, -22.64427369931138756 ) ) ;
#58012 = CARTESIAN_POINT ( 'NONE',  ( -3.000000000000000000, 16.83928648764923253, 16.46020748918050458 ) ) ;
#58013 = VERTEX_POINT ( 'NONE', #69866 ) ;
#58014 = ORIENTED_EDGE ( 'NONE', *, *, #17134, .F. ) ;
#58015 = CARTESIAN_POINT ( 'NONE',  ( -95.00000000000002842, 93.05995642670501411, 79.04625000000000057 ) ) ;
#58016 = FACE_OUTER_BOUND ( 'NONE', #56115, .T. ) ;
#58017 = CARTESIAN_POINT ( 'NONE',  ( -92.69370383062502583, 91.33154071421968467, 88.10822916753380696 ) ) ;
#58018 = DIRECTION ( 'NONE',  ( -0.000000000000000000, -0.000000000000000000, -1.000000000000000000 ) ) ;
#58019 = DIRECTION ( 'NONE',  ( -1.000000000000000000, 0.000000000000000000, 0.000000000000000000 ) ) ;
#58020 = CIRCLE ( 'NONE', #67623, 77.49899999999999523 ) ;
#58021 = CARTESIAN_POINT ( 'NONE',  ( 93.67500000000001137, -207.7050326799711968, 77.90854166840097150 ) ) ;
#58022 = DIRECTION ( 'NONE',  ( 0.000000000000000000, -0.9238795325112822976, -0.3826834323651008285 ) ) ;
#58023 =( BOUNDED_CURVE ( )  B_SPLINE_CURVE ( 2, ( #21894, #15512, #26424, #10611, #50080, #49354, #67388 ),
 .UNSPECIFIED., .F., .F. ) 
 B_SPLINE_CURVE_WITH_KNOTS ( ( 3, 2, 2, 3 ),
 ( 0.1270039290057624060, 0.1340595452774234198, 0.1411153108183404170, 0.1481709449582802873 ),
 .UNSPECIFIED. ) 
 CURVE ( )  GEOMETRIC_REPRESENTATION_ITEM ( )  RATIONAL_B_SPLINE_CURVE ( ( 0.9999943314825013863, 0.8660282381031498833, 1.000000000000000000, 0.8660254037844387076, 1.000000000000000000, 0.8660278988209799689, 0.9999950100198486957 ) ) 
 REPRESENTATION_ITEM ( '' )  );
#58024 = ORIENTED_EDGE ( 'NONE', *, *, #55431, .F. ) ;
#58025 = CARTESIAN_POINT ( 'NONE',  ( -96.15314808468752972, 91.99731107132950569, 77.47197916753380298 ) ) ;
#58026 = PRODUCT_DEFINITION_FORMATION_WITH_SPECIFIED_SOURCE ( 'ANY', '', #59551, .NOT_KNOWN. ) ;
#58027 = FACE_OUTER_BOUND ( 'NONE', #52321, .T. ) ;
#58028 = CARTESIAN_POINT ( 'NONE',  ( 0.000000000000000000, 30.41916302227216562, -71.27951684757994144 ) ) ;
#58029 = DIRECTION ( 'NONE',  ( -1.000000000000000000, 0.000000000000000000, 0.000000000000000000 ) ) ;
#58030 = CARTESIAN_POINT ( 'NONE',  ( 16.30584220631899228, -140.9432449716519784, 5.500000000000000000 ) ) ;
#58031 = CARTESIAN_POINT ( 'NONE',  ( 4.999999999999999112, -40.68715046381937128, 10.41901085202062660 ) ) ;
#58032 = CARTESIAN_POINT ( 'NONE',  ( -97.30629616937495996, -209.9999999999999716, 87.26156250086715715 ) ) ;
#58033 = CARTESIAN_POINT ( 'NONE',  ( 95.00000000000000000, -213.0599564267049857, 83.17374999999999829 ) ) ;
#58034 = VECTOR ( 'NONE', #2717, 1000.000000000000000 ) ;
#58035 = AXIS2_PLACEMENT_3D ( 'NONE', #36302, #57770, #12994 ) ;
#58036 = CARTESIAN_POINT ( 'NONE',  ( 97.30629616937498838, 91.33154071421968467, 75.56697916753383026 ) ) ;
#58037 = EDGE_CURVE ( 'NONE', #7004, #8687, #16247, .T. ) ;
#58038 = CARTESIAN_POINT ( 'NONE',  ( -93.84685191531247028, -211.9973110713294489, 75.40822916753381833 ) ) ;
#58039 = DIRECTION ( 'NONE',  ( 0.000000000000000000, 0.000000000000000000, 1.000000000000000000 ) ) ;
#58040 = ORIENTED_EDGE ( 'NONE', *, *, #35725, .F. ) ;
#58041 = DIRECTION ( 'NONE',  ( 0.000000000000000000, -0.4539904997395541875, 0.8910065241883641241 ) ) ;
#58042 = CARTESIAN_POINT ( 'NONE',  ( 97.64999999999999147, -209.9999999999999716, 80.79249999999998977 ) ) ;
#58043 = LINE ( 'NONE', #52394, #30597 ) ;
#58044 = AXIS2_PLACEMENT_3D ( 'NONE', #6351, #24733, #24005 ) ;
#58045 = AXIS2_PLACEMENT_3D ( 'NONE', #8275, #1211, #23720 ) ;
#58046 = AXIS2_PLACEMENT_3D ( 'NONE', #11156, #4799, #33707 ) ;
#58047 = EDGE_CURVE ( 'NONE', #10469, #17740, #4228, .T. ) ;
#58048 = ADVANCED_FACE ( 'NONE', ( #9863 ), #62117, .T. ) ;
#58049 = EDGE_CURVE ( 'NONE', #38445, #72240, #19760, .T. ) ;
#58050 = LINE ( 'NONE', #58412, #39718 ) ;
#58051 = CARTESIAN_POINT ( 'NONE',  ( 95.00000000000000000, -212.6630814284392557, 77.73656250086713726 ) ) ;
#58052 = ORIENTED_EDGE ( 'NONE', *, *, #60526, .T. ) ;
#58053 = DIRECTION ( 'NONE',  ( -0.4279312458752977388, -0.9038112904824853189, 0.000000000000000000 ) ) ;
#58054 = VERTEX_POINT ( 'NONE', #46953 ) ;
#58055 = EDGE_CURVE ( 'NONE', #54369, #913, #8984, .T. ) ;
#58056 = CARTESIAN_POINT ( 'NONE',  ( 5.000000000000002665, 81.90746397400393164, -3.894527615416986333 ) ) ;
#58057 = ORIENTED_EDGE ( 'NONE', *, *, #39970, .T. ) ;
#58058 = EDGE_CURVE ( 'NONE', #25980, #21350, #55834, .T. ) ;
#58059 = CARTESIAN_POINT ( 'NONE',  ( 10.00000000000000000, 17.67226234102874116, -33.17418723428288274 ) ) ;
#58060 = ORIENTED_EDGE ( 'NONE', *, *, #37591, .T. ) ;
#58061 = ORIENTED_EDGE ( 'NONE', *, *, #68412, .T. ) ;
#58062 = ORIENTED_EDGE ( 'NONE', *, *, #58458, .T. ) ;
#58063 = FACE_OUTER_BOUND ( 'NONE', #62808, .T. ) ;
#58064 = VERTEX_POINT ( 'NONE', #56102 ) ;
#58065 = CIRCLE ( 'NONE', #4099, 31.99999999999998934 ) ;
#58066 = ORIENTED_EDGE ( 'NONE', *, *, #37534, .T. ) ;
#58067 = CARTESIAN_POINT ( 'NONE',  ( 92.69370383062498320, 91.33154071421968467, 84.03364583420049883 ) ) ;
#58068 = EDGE_CURVE ( 'NONE', #68327, #64494, #18583, .T. ) ;
#58069 = CARTESIAN_POINT ( 'NONE',  ( 95.00000000000000000, -213.0599564267049857, 76.18874999999999886 ) ) ;
#58070 = VERTEX_POINT ( 'NONE', #4989 ) ;
#58071 = AXIS2_PLACEMENT_3D ( 'NONE', #55347, #16236, #44451 ) ;
#58072 = CARTESIAN_POINT ( 'NONE',  ( -92.34999999999999432, -209.9999999999999716, 83.33250000000001023 ) ) ;
#58073 = EDGE_LOOP ( 'NONE', ( #12299, #38916, #54098, #67710 ) ) ;
#58074 = ORIENTED_EDGE ( 'NONE', *, *, #31733, .F. ) ;
#58075 = ORIENTED_EDGE ( 'NONE', *, *, #29840, .T. ) ;
#58077 = ORIENTED_EDGE ( 'NONE', *, *, #3601, .T. ) ;
#58076 = ADVANCED_FACE ( 'NONE', ( #27892 ), #50817, .F. ) ;
#58078 = EDGE_CURVE ( 'NONE', #28208, #65655, #60627, .T. ) ;
#58079 = CIRCLE ( 'NONE', #30423, 31.99999999999998934 ) ;
#58080 = CARTESIAN_POINT ( 'NONE',  ( 5.413716818265703381E-13, -119.9999999999995026, -72.00000000000031264 ) ) ;
#58081 = DIRECTION ( 'NONE',  ( -1.000000000000000000, -0.000000000000000000, 0.000000000000000000 ) ) ;
#58082 = CARTESIAN_POINT ( 'NONE',  ( 0.000000000000000000, -22.32062822937489344, 14.36278369418800160 ) ) ;
#58083 = CARTESIAN_POINT ( 'NONE',  ( -95.00000000000002842, 90.00000000000004263, 90.00000000000000000 ) ) ;
#58084 = LINE ( 'NONE', #52064, #39087 ) ;
#58085 = DIRECTION ( 'NONE',  ( 1.000000000000000000, 0.000000000000000000, 0.000000000000000000 ) ) ;
#58086 = DIRECTION ( 'NONE',  ( 0.000000000000000000, 0.000000000000000000, 1.000000000000000000 ) ) ;
#58087 = ORIENTED_EDGE ( 'NONE', *, *, #61211, .F. ) ;
#58088 = CARTESIAN_POINT ( 'NONE',  ( -94.99999999999997158, -206.9400435732949575, 77.85562500173429612 ) ) ;
#58089 = ORIENTED_EDGE ( 'NONE', *, *, #8668, .T. ) ;
#58090 = CARTESIAN_POINT ( 'NONE',  ( 14.53333333333331545, 0.000000000000000000, -1.466666666666671670 ) ) ;
#58091 = EDGE_CURVE ( 'NONE', #11947, #55143, #22633, .T. ) ;
#58092 = ORIENTED_EDGE ( 'NONE', *, *, #27744, .T. ) ;
#58094 = CARTESIAN_POINT ( 'NONE',  ( -92.35000000000005116, 88.47002178664754979, 78.91395833506763324 ) ) ;
#58093 = CARTESIAN_POINT ( 'NONE',  ( 96.32499999999998863, 87.70503267997126784, 78.22604166840096696 ) ) ;
#58095 = AXIS2_PLACEMENT_3D ( 'NONE', #26344, #72922, #54915 ) ;
#58096 = VERTEX_POINT ( 'NONE', #70593 ) ;
#58097 = CARTESIAN_POINT ( 'NONE',  ( 96.15314808468748708, 88.00268892867053694, 78.58322916753382970 ) ) ;
#58098 = AXIS2_PLACEMENT_3D ( 'NONE', #68599, #15598, #45300 ) ;
#58099 = CARTESIAN_POINT ( 'NONE',  ( 92.34999999999999432, 90.00000000000002842, 75.39499999999999602 ) ) ;
#58100 = CYLINDRICAL_SURFACE ( 'NONE', #9084, 31.99999999999998579 ) ;
#58101 = DIRECTION ( 'NONE',  ( -1.000000000000000000, -0.000000000000000000, -0.000000000000000000 ) ) ;
#58102 = LINE ( 'NONE', #47925, #37826 ) ;
#58103 = VERTEX_POINT ( 'NONE', #58975 ) ;
#58105 = DIRECTION ( 'NONE',  ( -0.000000000000000000, -0.000000000000000000, 1.000000000000000000 ) ) ;
#58104 = CIRCLE ( 'NONE', #59275, 82.00000000000000000 ) ;
#58106 = VECTOR ( 'NONE', #12800, 1000.000000000000000 ) ;
#58107 = DIRECTION ( 'NONE',  ( -1.000000000000000000, 0.000000000000000000, 0.000000000000000000 ) ) ;
#58108 = ORIENTED_EDGE ( 'NONE', *, *, #18162, .F. ) ;
#58109 = VERTEX_POINT ( 'NONE', #48421 ) ;
#58110 = DIRECTION ( 'NONE',  ( -1.000000000000000000, 0.000000000000000000, 0.000000000000000000 ) ) ;
#58111 = CARTESIAN_POINT ( 'NONE',  ( -21.33958957442910886, -129.9559990355020034, -5.500000000000000000 ) ) ;
#58112 = DIRECTION ( 'NONE',  ( 1.000000000000000000, 0.000000000000000000, 0.000000000000000000 ) ) ;
#58113 = CARTESIAN_POINT ( 'NONE',  ( -93.84685191531247028, -211.9973110713294489, 79.21822916753382060 ) ) ;
#58114 = EDGE_LOOP ( 'NONE', ( #62115, #39537, #4181, #49627 ) ) ;
#58115 = VECTOR ( 'NONE', #63277, 1000.000000000000000 ) ;
#58116 = DIRECTION ( 'NONE',  ( 1.000000000000000000, 1.427937372958405461E-15, 7.962523111839130290E-16 ) ) ;
#58117 = CARTESIAN_POINT ( 'NONE',  ( -97.20211296431911308, -211.3166576149945115, 74.94590613650854038 ) ) ;
#58118 = LINE ( 'NONE', #69763, #14018 ) ;
#58119 = CARTESIAN_POINT ( 'NONE',  ( 0.000000000000000000, -2.663952781846440576, 41.91543099594817789 ) ) ;
#58120 = DIRECTION ( 'NONE',  ( -0.000000000000000000, -0.3090169943749572767, -0.9510565162951503115 ) ) ;
#58121 = CARTESIAN_POINT ( 'NONE',  ( 11.99999999999999822, 74.65491531819118620, -8.830959090342659579 ) ) ;
#58122 = CARTESIAN_POINT ( 'NONE',  ( 0.000000000000000000, 15.33399622253481986, 80.55351364060595643 ) ) ;
#58123 = DIRECTION ( 'NONE',  ( 2.603472992746261562E-14, 2.546204323184492723E-14, -1.000000000000000000 ) ) ;
#58124 = CARTESIAN_POINT ( 'NONE',  ( 10.00000000000000000, 22.64427369931212297, -30.00120703465181293 ) ) ;
#58125 = AXIS2_PLACEMENT_3D ( 'NONE', #10766, #27296, #23169 ) ;
#58126 = CARTESIAN_POINT ( 'NONE',  ( 94.99999999999998579, 87.33691857156068750, 88.69031250086716511 ) ) ;
#58127 = PLANE ( 'NONE',  #15406 ) ;
#58128 = CARTESIAN_POINT ( 'NONE',  ( 0.000000000000000000, 0.000000000000000000, 0.000000000000000000 ) ) ;
#58129 = ORIENTED_EDGE ( 'NONE', *, *, #48438, .F. ) ;
#58130 = LINE ( 'NONE', #24298, #19595 ) ;
#58131 = EDGE_CURVE ( 'NONE', #34691, #45762, #9032, .T. ) ;
#58132 = CARTESIAN_POINT ( 'NONE',  ( -97.30629616937501680, 91.33154071421968467, 74.98489583420048632 ) ) ;
#58133 = AXIS2_PLACEMENT_3D ( 'NONE', #12474, #70339, #7942 ) ;
#58134 = ADVANCED_FACE ( 'NONE', ( #48786 ), #47682, .T. ) ;
#58135 = EDGE_CURVE ( 'NONE', #7305, #2169, #25127, .T. ) ;
#58136 = EDGE_CURVE ( 'NONE', #3895, #36077, #42418, .T. ) ;
#58137 = CARTESIAN_POINT ( 'NONE',  ( 95.00000000000000000, -212.6630814284392557, 86.62656250086715204 ) ) ;
#58138 = ORIENTED_EDGE ( 'NONE', *, *, #3360, .F. ) ;
#58139 = CIRCLE ( 'NONE', #36493, 31.99999999999998579 ) ;
#58141 = CARTESIAN_POINT ( 'NONE',  ( -16.06301359042743115, -102.7814171781257357, 5.500000000000000000 ) ) ;
#58140 = VECTOR ( 'NONE', #57954, 1000.000000000000000 ) ;
#58142 = ORIENTED_EDGE ( 'NONE', *, *, #14072, .F. ) ;
#58143 = CARTESIAN_POINT ( 'NONE',  ( 0.000000000000000000, -51.02545421589363883, 55.20638768913742922 ) ) ;
#58144 = AXIS2_PLACEMENT_3D ( 'NONE', #68221, #67474, #16718 ) ;
#58145 = CARTESIAN_POINT ( 'NONE',  ( 10.00000000000000000, 71.87247863392413194, 39.47590169984869135 ) ) ;
#58146 = ORIENTED_EDGE ( 'NONE', *, *, #43389, .T. ) ;
#58147 = EDGE_LOOP ( 'NONE', ( #9980, #11448 ) ) ;
#58148 = EDGE_CURVE ( 'NONE', #2581, #44188, #8580, .T. ) ;
#58149 = CARTESIAN_POINT ( 'NONE',  ( 96.15314808468748708, -208.0026889286704943, 82.60489583420049087 ) ) ;
#58150 = CARTESIAN_POINT ( 'NONE',  ( 0.000000000000000000, 0.000000000000000000, 52.00000000000002132 ) ) ;
#58152 = CARTESIAN_POINT ( 'NONE',  ( 10.00000000000000000, 22.74946021919133088, 29.81001611431016229 ) ) ;
#58151 = AXIS2_PLACEMENT_3D ( 'NONE', #39480, #57511, #16164 ) ;
#58153 = CARTESIAN_POINT ( 'NONE',  ( 0.000000000000000000, 2.663952781846728790, -41.91543099594814947 ) ) ;
#58154 = DIRECTION ( 'NONE',  ( 0.000000000000000000, 0.000000000000000000, -1.000000000000000000 ) ) ;
#58155 = CARTESIAN_POINT ( 'NONE',  ( -18.12185313557660038, -104.9634299478706794, 5.500000000000000000 ) ) ;
#58156 = CARTESIAN_POINT ( 'NONE',  ( 92.35000000000002274, -211.5299782133524502, 83.70291666666668107 ) ) ;
#58157 = CIRCLE ( 'NONE', #34113, 77.49900000000000944 ) ;
#58158 = ORIENTED_EDGE ( 'NONE', *, *, #47954, .T. ) ;
#58159 = VERTEX_POINT ( 'NONE', #36764 ) ;
#58160 = EDGE_LOOP ( 'NONE', ( #68798, #18052, #6218, #42733 ) ) ;
#58161 = ORIENTED_EDGE ( 'NONE', *, *, #11003, .F. ) ;
#58162 = FILL_AREA_STYLE ('',( #17567 ) ) ;
#58163 = EDGE_CURVE ( 'NONE', #51303, #72289, #59714, .T. ) ;
#58164 = EDGE_CURVE ( 'NONE', #32383, #13338, #33847, .T. ) ;
#58165 = CARTESIAN_POINT ( 'NONE',  ( -96.15314808468751551, 88.00268892867056536, 88.00239583420048461 ) ) ;
#58166 = CYLINDRICAL_SURFACE ( 'NONE', #11333, 31.99999999999998579 ) ;
#58167 = CARTESIAN_POINT ( 'NONE',  ( -26.29030328629083968, -123.6496510949466341, 5.500000000000000000 ) ) ;
#58168 = CARTESIAN_POINT ( 'NONE',  ( 93.67500000000001137, -207.7050326799711968, 76.00354166840097037 ) ) ;
#58169 = CARTESIAN_POINT ( 'NONE',  ( 96.32499999999998863, 87.70503267997126784, 76.87666666666666515 ) ) ;
#58170 = VERTEX_POINT ( 'NONE', #31492 ) ;
#58171 = CARTESIAN_POINT ( 'NONE',  ( -92.34999999999999432, -208.4700217866474645, 89.17979166840096639 ) ) ;
#58172 = VERTEX_POINT ( 'NONE', #54435 ) ;
#58173 = DIRECTION ( 'NONE',  ( -1.000000000000000000, 0.000000000000000000, 0.000000000000000000 ) ) ;
#58174 = ORIENTED_EDGE ( 'NONE', *, *, #14364, .F. ) ;
#58175 = FACE_OUTER_BOUND ( 'NONE', #51343, .T. ) ;
#58176 = CARTESIAN_POINT ( 'NONE',  ( -93.84685191531254134, 91.99731107132950569, 81.33489583420049485 ) ) ;
#58177 = CARTESIAN_POINT ( 'NONE',  ( 96.15314808468748708, 91.99731107132950569, 75.46114583420047950 ) ) ;
#58178 = ORIENTED_EDGE ( 'NONE', *, *, #4518, .T. ) ;
#58179 = DIRECTION ( 'NONE',  ( 0.000000000000000000, 0.000000000000000000, 1.000000000000000000 ) ) ;
#58180 = FACE_OUTER_BOUND ( 'NONE', #10412, .T. ) ;
#58181 = LINE ( 'NONE', #30340, #32972 ) ;
#58182 = CARTESIAN_POINT ( 'NONE',  ( -12.00000000000000000, 0.000000000000000000, 0.000000000000000000 ) ) ;
#58183 = ORIENTED_EDGE ( 'NONE', *, *, #66280, .F. ) ;
#58184 = LINE ( 'NONE', #34891, #54342 ) ;
#58185 = CARTESIAN_POINT ( 'NONE',  ( -95.00000000000002842, 93.05995642670504253, 81.66562500173431260 ) ) ;
#58186 = VERTEX_POINT ( 'NONE', #7830 ) ;
#58187 = ORIENTED_EDGE ( 'NONE', *, *, #54552, .T. ) ;
#58188 = CARTESIAN_POINT ( 'NONE',  ( 0.000000000000000000, 0.000000000000000000, -54.99999999999998579 ) ) ;
#58189 = ORIENTED_EDGE ( 'NONE', *, *, #41239, .T. ) ;
#58190 = DIRECTION ( 'NONE',  ( -1.000000000000000000, -0.000000000000000000, -0.000000000000000000 ) ) ;
#58191 = PLANE ( 'NONE',  #28116 ) ;
#58192 = ORIENTED_EDGE ( 'NONE', *, *, #48893, .F. ) ;
#58193 = CARTESIAN_POINT ( 'NONE',  ( -93.84685191531247028, -211.9973110713294489, 86.83822916753382515 ) ) ;
#58194 = ORIENTED_EDGE ( 'NONE', *, *, #49624, .F. ) ;
#58195 = AXIS2_PLACEMENT_3D ( 'NONE', #53420, #31222, #71799 ) ;
#58196 = CYLINDRICAL_SURFACE ( 'NONE', #23104, 31.99999999999998579 ) ;
#58197 = FACE_OUTER_BOUND ( 'NONE', #6914, .T. ) ;
#58198 = VECTOR ( 'NONE', #67327, 1000.000000000000000 ) ;
#58199 = ORIENTED_EDGE ( 'NONE', *, *, #42173, .T. ) ;
#58200 = ORIENTED_EDGE ( 'NONE', *, *, #61614, .T. ) ;
#58201 = CARTESIAN_POINT ( 'NONE',  ( 10.00000000000000000, -4.992566952385247170, 37.16516213103275845 ) ) ;
#58202 = AXIS2_PLACEMENT_3D ( 'NONE', #58409, #35840, #29824 ) ;
#58203 = CARTESIAN_POINT ( 'NONE',  ( -26.53422223201112828, -120.6595836127786043, 5.500000000000000000 ) ) ;
#58204 = CARTESIAN_POINT ( 'NONE',  ( 94.99999999999998579, 87.33691857156068750, 80.91156250086714863 ) ) ;
#58205 = CARTESIAN_POINT ( 'NONE',  ( 15.50000000000000000, 0.000000000000000000, 0.000000000000000000 ) ) ;
#58206 = CARTESIAN_POINT ( 'NONE',  ( -97.64999999990727986, 90.00001381026693537, 80.55392363656929433 ) ) ;
#58207 = DIRECTION ( 'NONE',  ( 0.000000000000000000, 0.000000000000000000, 1.000000000000000000 ) ) ;
#58208 = LINE ( 'NONE', #30730, #18369 ) ;
#58209 = DIRECTION ( 'NONE',  ( -1.000000000000000000, -0.000000000000000000, 0.000000000000000000 ) ) ;
#58210 = CARTESIAN_POINT ( 'NONE',  ( -93.67500000000003979, 92.29496732002878900, 84.15270833506762926 ) ) ;
#58211 = LINE ( 'NONE', #380, #38714 ) ;
#58212 = AXIS2_PLACEMENT_3D ( 'NONE', #49903, #21325, #36778 ) ;
#58213 = CARTESIAN_POINT ( 'NONE',  ( 10.00000000000000000, 0.000000000000000000, 0.000000000000000000 ) ) ;
#58214 = PRODUCT_RELATED_PRODUCT_CATEGORY ( 'part', '', ( #73401 ) ) ;
#58215 = EDGE_CURVE ( 'NONE', #58186, #63730, #54075, .T. ) ;
#58216 = FACE_OUTER_BOUND ( 'NONE', #39697, .T. ) ;
#58217 = CARTESIAN_POINT ( 'NONE',  ( -93.84685191531254134, 91.99731107132950569, 88.79614583420047325 ) ) ;
#58218 = DIRECTION ( 'NONE',  ( -0.000000000000000000, -0.000000000000000000, -1.000000000000000000 ) ) ;
#58219 = EDGE_CURVE ( 'NONE', #43524, #41055, #30744, .T. ) ;
#58220 = EDGE_CURVE ( 'NONE', #28951, #42454, #25854, .T. ) ;
#58221 = LINE ( 'NONE', #36389, #49253 ) ;
#58222 = AXIS2_PLACEMENT_3D ( 'NONE', #25487, #14573, #48418 ) ;
#58223 = ORIENTED_EDGE ( 'NONE', *, *, #22833, .F. ) ;
#58224 =( BOUNDED_CURVE ( )  B_SPLINE_CURVE ( 2, ( #33158, #60649, #56107, #27525, #66651, #26420, #15131 ),
 .UNSPECIFIED., .F., .F. ) 
 B_SPLINE_CURVE_WITH_KNOTS ( ( 3, 2, 2, 3 ),
 ( 0.7499999999999996669, 0.7569444444444439757, 0.7638888888888883955, 0.7708333333333328152 ),
 .UNSPECIFIED. ) 
 CURVE ( )  GEOMETRIC_REPRESENTATION_ITEM ( )  RATIONAL_B_SPLINE_CURVE ( ( 1.000000000000006439, 0.8660254037844322683, 1.000000000000000000, 0.8660254037844387076, 1.000000000000000000, 0.8660254037844493658, 0.9999999999999893419 ) ) 
 REPRESENTATION_ITEM ( '' )  );
#58225 = EDGE_CURVE ( 'NONE', #1094, #53605, #24747, .T. ) ;
#58226 = CARTESIAN_POINT ( 'NONE',  ( -97.64999999999996305, -209.9999999999999716, 90.00000000000000000 ) ) ;
#58227 = DIRECTION ( 'NONE',  ( 0.000000000000000000, -1.000000000000000000, -1.047444401652940007E-14 ) ) ;
#58228 = LINE ( 'NONE', #19475, #64749 ) ;
#58229 = CYLINDRICAL_SURFACE ( 'NONE', #17806, 2.649999999999985700 ) ;
#58230 = CARTESIAN_POINT ( 'NONE',  ( -97.64999999953592180, 89.99996903277666149, 77.38038495128051864 ) ) ;
#58231 = DIRECTION ( 'NONE',  ( -1.000000000000000000, -0.000000000000000000, -0.000000000000000000 ) ) ;
#58232 = AXIS2_PLACEMENT_3D ( 'NONE', #61134, #9625, #56616 ) ;
#58233 = CARTESIAN_POINT ( 'NONE',  ( 92.69370383062501162, -208.6684592857803011, 85.30364583420048064 ) ) ;
#58234 = EDGE_LOOP ( 'NONE', ( #49153, #36502, #73237, #32648 ) ) ;
#58235 = EDGE_LOOP ( 'NONE', ( #61573, #62604, #58138, #57425, #43428, #62709 ) ) ;
#58236 = ADVANCED_FACE ( 'NONE', ( #30008 ), #36028, .T. ) ;
#58237 = EDGE_CURVE ( 'NONE', #2536, #68158, #42639, .T. ) ;
#58238 = CARTESIAN_POINT ( 'NONE',  ( 11.99999999999999822, 0.000000000000000000, 0.000000000000000000 ) ) ;
#58239 = ORIENTED_EDGE ( 'NONE', *, *, #56654, .T. ) ;
#58240 = DIRECTION ( 'NONE',  ( -1.000000000000000000, 0.000000000000000000, 0.000000000000000000 ) ) ;
#58241 = CARTESIAN_POINT ( 'NONE',  ( 96.15314808468750130, -211.9973110713294489, 75.88447916753381151 ) ) ;
#58242 = CIRCLE ( 'NONE', #41451, 31.99999999999998579 ) ;
#58243 = ORIENTED_EDGE ( 'NONE', *, *, #55094, .T. ) ;
#58244 = VECTOR ( 'NONE', #20551, 1000.000000000000000 ) ;
#58245 = CARTESIAN_POINT ( 'NONE',  ( 93.84685191531251292, -211.9973110713294489, 78.47739583420049314 ) ) ;
#58246 = ORIENTED_EDGE ( 'NONE', *, *, #33894, .T. ) ;
#58247 = DIRECTION ( 'NONE',  ( -1.000000000000000000, 0.000000000000000000, 0.000000000000000000 ) ) ;
#58248 = EDGE_LOOP ( 'NONE', ( #38091, #46988 ) ) ;
#58249 = CIRCLE ( 'NONE', #663, 16.00000000000000000 ) ;
#58250 = VERTEX_POINT ( 'NONE', #19107 ) ;
#58251 = CARTESIAN_POINT ( 'NONE',  ( 23.41451323550360186, -132.5004227906269989, 5.500000000000000000 ) ) ;
#58252 = ADVANCED_FACE ( 'NONE', ( #18729 ), #42056, .F. ) ;
#58253 = CARTESIAN_POINT ( 'NONE',  ( 11.99999999999999822, 0.000000000000000000, 0.000000000000000000 ) ) ;
#58254 = AXIS2_PLACEMENT_3D ( 'NONE', #46930, #34909, #7442 ) ;
#58255 = ORIENTED_EDGE ( 'NONE', *, *, #63338, .F. ) ;
#58256 = PLANE ( 'NONE',  #13739 ) ;
#58257 = CARTESIAN_POINT ( 'NONE',  ( 97.64999999999997726, -208.4700217866474645, 86.63979166840097434 ) ) ;
#58258 = CARTESIAN_POINT ( 'NONE',  ( 96.32499999999998863, 87.70503267997126784, 88.30666666666665776 ) ) ;
#58259 = ORIENTED_EDGE ( 'NONE', *, *, #70782, .T. ) ;
#58260 = ORIENTED_EDGE ( 'NONE', *, *, #7902, .T. ) ;
#58261 = VERTEX_POINT ( 'NONE', #1864 ) ;
#58262 = CARTESIAN_POINT ( 'NONE',  ( 11.99999999999999822, 0.000000000000000000, 0.000000000000000000 ) ) ;
#58263 = VERTEX_POINT ( 'NONE', #4815 ) ;
#58264 = AXIS2_PLACEMENT_3D ( 'NONE', #57360, #22406, #28782 ) ;
#58265 = CARTESIAN_POINT ( 'NONE',  ( 93.67499999999999716, 87.70503267997126784, 85.10520833506762983 ) ) ;
#58266 = ORIENTED_EDGE ( 'NONE', *, *, #70886, .T. ) ;
#58267 = FILL_AREA_STYLE_COLOUR ( '', #19428 ) ;
#58268 = EDGE_LOOP ( 'NONE', ( #21948, #13399, #44862, #6052 ) ) ;
#58269 = DIRECTION ( 'NONE',  ( 0.000000000000000000, 0.000000000000000000, 1.000000000000000000 ) ) ;
#58270 = CONTEXT_DEPENDENT_SHAPE_REPRESENTATION ( #41702, #62663 ) ;
#58271 = CARTESIAN_POINT ( 'NONE',  ( 0.000000000000000000, 81.50828551894227303, 8.966570791700986476 ) ) ;
#58272 = VERTEX_POINT ( 'NONE', #67197 ) ;
#58273 = ORIENTED_EDGE ( 'NONE', *, *, #1342, .F. ) ;
#58274 = AXIS2_PLACEMENT_3D ( 'NONE', #4697, #15206, #21204 ) ;
#58275 = EDGE_LOOP ( 'NONE', ( #7659, #34694 ) ) ;
#58276 = DIRECTION ( 'NONE',  ( 0.000000000000000000, 0.8090169943749445647, 0.5877852522924770229 ) ) ;
#58277 = CARTESIAN_POINT ( 'NONE',  ( 11.99999999999999822, -55.19960302592104284, 51.03279382321070301 ) ) ;
#58278 = CARTESIAN_POINT ( 'NONE',  ( -92.35000000000005116, 91.52997821335253548, 89.10041666666667481 ) ) ;
#58279 = EDGE_LOOP ( 'NONE', ( #42514, #67141, #68631, #6382 ) ) ;
#58280 = CARTESIAN_POINT ( 'NONE',  ( 10.00000000000000000, 0.000000000000000000, 0.000000000000000000 ) ) ;
#58281 = CARTESIAN_POINT ( 'NONE',  ( 0.000000000000000000, 0.000000000000000000, 0.000000000000000000 ) ) ;
#58282 = ORIENTED_EDGE ( 'NONE', *, *, #23857, .F. ) ;
#58283 = CARTESIAN_POINT ( 'NONE',  ( 97.64999999999999147, 90.00000000000002842, 90.00000000000000000 ) ) ;
#58284 = CARTESIAN_POINT ( 'NONE',  ( -96.15314808468745866, -211.9973110713294489, 83.39864583420047950 ) ) ;
#58285 = ORIENTED_EDGE ( 'NONE', *, *, #25206, .T. ) ;
#58286 = CARTESIAN_POINT ( 'NONE',  ( 0.000000000000000000, 0.000000000000000000, 0.000000000000000000 ) ) ;
#58287 = CARTESIAN_POINT ( 'NONE',  ( 92.79788703567045616, -211.3166576149753269, 74.94590613650809985 ) ) ;
#58288 = LINE ( 'NONE', #42485, #27265 ) ;
#58289 = CARTESIAN_POINT ( 'NONE',  ( -94.99999999999997158, -207.3369185715606307, 76.78406250086712248 ) ) ;
#58290 = ADVANCED_FACE ( 'NONE', ( #27329 ), #55172, .T. ) ;
#58291 = CARTESIAN_POINT ( 'NONE',  ( 0.000000000000000000, 0.000000000000000000, 0.000000000000000000 ) ) ;
#58292 = AXIS2_PLACEMENT_3D ( 'NONE', #44503, #62158, #32820 ) ;
#58293 = LINE ( 'NONE', #39908, #54138 ) ;
#58294 = DIRECTION ( 'NONE',  ( 0.000000000000000000, 0.000000000000000000, -1.000000000000000000 ) ) ;
#58295 = ADVANCED_FACE ( 'NONE', ( #55915 ), #9681, .F. ) ;
#58296 = CARTESIAN_POINT ( 'NONE',  ( -1.250000000000000000, -12.36245420541525597, 0.000000000000000000 ) ) ;
#58297 = EDGE_CURVE ( 'NONE', #59396, #54682, #11447, .T. ) ;
#58298 = CARTESIAN_POINT ( 'NONE',  ( 1.560000000000000053, 0.000000000000000000, 0.000000000000000000 ) ) ;
#58299 = CARTESIAN_POINT ( 'NONE',  ( -93.84685191531254134, 91.99731107132950569, 77.36614583420046642 ) ) ;
#58300 = DIRECTION ( 'NONE',  ( -1.000000000000000000, -0.000000000000000000, -0.000000000000000000 ) ) ;
#58301 = CARTESIAN_POINT ( 'NONE',  ( 10.00000000000000000, -41.91543099594816368, -2.663952781846588014 ) ) ;
#58302 = EDGE_LOOP ( 'NONE', ( #24599, #3710, #68243, #44172 ) ) ;
#58303 = AXIS2_PLACEMENT_3D ( 'NONE', #20825, #15182, #48293 ) ;
#58304 = CARTESIAN_POINT ( 'NONE',  ( 0.000000000000000000, -120.0000000000000000, -2.500000000000000000 ) ) ;
#58305 = EDGE_CURVE ( 'NONE', #32358, #52599, #32969, .T. ) ;
#58307 = CARTESIAN_POINT ( 'NONE',  ( 0.000000000000000000, -37.58145647212455032, 16.68533520207890319 ) ) ;
#58306 = CIRCLE ( 'NONE', #18689, 77.49899999999999523 ) ;
#58308 = FACE_OUTER_BOUND ( 'NONE', #29119, .T. ) ;
#58309 = FACE_OUTER_BOUND ( 'NONE', #5139, .T. ) ;
#58310 = DIRECTION ( 'NONE',  ( 0.000000000000000000, 0.000000000000000000, -1.000000000000000000 ) ) ;
#58311 = DIRECTION ( 'NONE',  ( 0.000000000000000000, 0.000000000000000000, 1.000000000000000000 ) ) ;
#58312 = CARTESIAN_POINT ( 'NONE',  ( -97.30629616937495996, -209.9999999999999716, 75.83156250086716454 ) ) ;
#58313 = CYLINDRICAL_SURFACE ( 'NONE', #2610, 31.99999999999999289 ) ;
#58314 = AXIS2_PLACEMENT_3D ( 'NONE', #72688, #22710, #51258 ) ;
#58315 = AXIS2_PLACEMENT_3D ( 'NONE', #45646, #50512, #21946 ) ;
#58316 = EDGE_LOOP ( 'NONE', ( #38063, #64452, #62594, #14941 ) ) ;
#58317 = EDGE_CURVE ( 'NONE', #46805, #59461, #58249, .T. ) ;
#58318 = DIRECTION ( 'NONE',  ( 0.000000000000000000, 0.000000000000000000, 1.000000000000000000 ) ) ;
#58319 = CARTESIAN_POINT ( 'NONE',  ( 95.00000000000000000, -213.0599564267049857, 88.25374999999999659 ) ) ;
#58320 =( NAMED_UNIT ( * ) SI_UNIT ( $, .STERADIAN. ) SOLID_ANGLE_UNIT ( ) );
#58321 = DIRECTION ( 'NONE',  ( -1.000000000000000000, -0.000000000000000000, 0.000000000000000000 ) ) ;
#58322 = DIRECTION ( 'NONE',  ( -1.000000000000000000, -0.000000000000000000, -0.000000000000000000 ) ) ;
#58323 = ORIENTED_EDGE ( 'NONE', *, *, #51789, .T. ) ;
#58324 = EDGE_CURVE ( 'NONE', #43683, #15633, #10214, .T. ) ;
#58325 = CARTESIAN_POINT ( 'NONE',  ( 0.000000000000000000, 44.88180994100376608, 63.18004540533043922 ) ) ;
#58326 = EDGE_CURVE ( 'NONE', #67395, #20649, #27050, .T. ) ;
#58327 = DIRECTION ( 'NONE',  ( 1.000000000000000000, 0.000000000000000000, 0.000000000000000000 ) ) ;
#58328 = ORIENTED_EDGE ( 'NONE', *, *, #16720, .T. ) ;
#58329 = CARTESIAN_POINT ( 'NONE',  ( 97.30629616937498838, -209.9999999999999716, 83.61031250086713840 ) ) ;
#58330 = DIRECTION ( 'NONE',  ( -1.000000000000000000, -0.000000000000000000, 0.000000000000000000 ) ) ;
#58331 = ADVANCED_FACE ( 'NONE', ( #39003 ), #38634, .F. ) ;
#58332 = ORIENTED_EDGE ( 'NONE', *, *, #26142, .F. ) ;
#58333 = CARTESIAN_POINT ( 'NONE',  ( 0.000000000000000000, 0.000000000000000000, -175.0000000000000000 ) ) ;
#58334 = ORIENTED_EDGE ( 'NONE', *, *, #25456, .F. ) ;
#58335 = CARTESIAN_POINT ( 'NONE',  ( 92.35000000000002274, -209.9999907079572381, 84.99937468035460597 ) ) ;
#58336 = ORIENTED_EDGE ( 'NONE', *, *, #43564, .F. ) ;
#58337 = CARTESIAN_POINT ( 'NONE',  ( -97.30629616937501680, 90.00000000000004263, 80.91156250086716284 ) ) ;
#58338 = ORIENTED_EDGE ( 'NONE', *, *, #403, .T. ) ;
#58339 = VERTEX_POINT ( 'NONE', #10416 ) ;
#58340 = DIRECTION ( 'NONE',  ( 0.000000000000000000, 0.000000000000000000, 1.000000000000000000 ) ) ;
#58341 = ORIENTED_EDGE ( 'NONE', *, *, #53378, .F. ) ;
#58342 = CARTESIAN_POINT ( 'NONE',  ( 95.00000000000000000, -206.9400435732949575, 84.84062500173429555 ) ) ;
#58343 = DIRECTION ( 'NONE',  ( 0.000000000000000000, -0.8090169943749402348, -0.5877852522924830181 ) ) ;
#58344 = ORIENTED_EDGE ( 'NONE', *, *, #12629, .F. ) ;
#58345 = CARTESIAN_POINT ( 'NONE',  ( 2.117611129180199558, -93.54218975225703048, 5.500000000000000000 ) ) ;
#58346 = VERTEX_POINT ( 'NONE', #61193 ) ;
#58347 = FACE_BOUND ( 'NONE', #15504, .T. ) ;
#58348 = VECTOR ( 'NONE', #29410, 1000.000000000000000 ) ;
#58349 = ORIENTED_EDGE ( 'NONE', *, *, #37623, .F. ) ;
#58350 = VERTEX_POINT ( 'NONE', #9303 ) ;
#58351 = ORIENTED_EDGE ( 'NONE', *, *, #1426, .F. ) ;
#58352 = CARTESIAN_POINT ( 'NONE',  ( 97.30629616937498838, -208.6684592857803011, 83.02822916753379445 ) ) ;
#58353 = SHAPE_DEFINITION_REPRESENTATION ( #43387, #65179 ) ;
#58354 = DIRECTION ( 'NONE',  ( 0.000000000000000000, 0.000000000000000000, 1.000000000000000000 ) ) ;
#58355 = AXIS2_PLACEMENT_3D ( 'NONE', #39934, #68875, #17724 ) ;
#58356 = CARTESIAN_POINT ( 'NONE',  ( 92.34999999999999432, 88.47002178664752137, 84.97291666666667709 ) ) ;
#58357 = CARTESIAN_POINT ( 'NONE',  ( -19.90058851926621131, -132.5883508287165853, 2.500000000000000000 ) ) ;
#58358 = CIRCLE ( 'NONE', #41564, 31.99999999999999289 ) ;
#58359 = CARTESIAN_POINT ( 'NONE',  ( 15.00000000000000000, 6.762365576493647445, 25.66652317338391498 ) ) ;
#58360 = CARTESIAN_POINT ( 'NONE',  ( -95.00000000000002842, 86.94004357329504273, 82.53874999999999318 ) ) ;
#58361 = CARTESIAN_POINT ( 'NONE',  ( -93.84685191531247028, -211.9973110713294489, 83.50447916753381605 ) ) ;
#58362 = CARTESIAN_POINT ( 'NONE',  ( -95.00000000000002842, 87.33691857156074434, 81.70531250086715147 ) ) ;
#58363 = VERTEX_POINT ( 'NONE', #33335 ) ;
#58364 = AXIS2_PLACEMENT_3D ( 'NONE', #71499, #25651, #48588 ) ;
#58365 = CARTESIAN_POINT ( 'NONE',  ( 96.15314808468748708, 91.99731107132950569, 84.35114583420048007 ) ) ;
#58366 = VECTOR ( 'NONE', #56453, 1000.000000000000000 ) ;
#58367 = ORIENTED_EDGE ( 'NONE', *, *, #69511, .T. ) ;
#58368 = CARTESIAN_POINT ( 'NONE',  ( -97.65000000000001990, 90.00001683226682303, 78.64937441956426767 ) ) ;
#58369 = CYLINDRICAL_SURFACE ( 'NONE', #15517, 82.00000000000000000 ) ;
#58370 = DIRECTION ( 'NONE',  ( -1.000000000000000000, 0.000000000000000000, 0.000000000000000000 ) ) ;
#58371 = DIRECTION ( 'NONE',  ( -0.2306669878475622604, -0.9730327541852497042, 0.000000000000000000 ) ) ;
#58372 = CARTESIAN_POINT ( 'NONE',  ( 9.984461079971730157, -95.40710393340120277, 5.500000000000000000 ) ) ;
#58373 = CARTESIAN_POINT ( 'NONE',  ( -96.15314808468745866, -211.9973110713294489, 87.20864583420046756 ) ) ;
#58374 = LINE ( 'NONE', #13252, #23337 ) ;
#58375 = EDGE_CURVE ( 'NONE', #40854, #13145, #3698, .T. ) ;
#58376 = DIRECTION ( 'NONE',  ( -0.000000000000000000, -0.000000000000000000, 1.000000000000000000 ) ) ;
#58377 = LINE ( 'NONE', #12139, #57145 ) ;
#58378 = LINE ( 'NONE', #6877, #58689 ) ;
#58379 = ORIENTED_EDGE ( 'NONE', *, *, #17815, .F. ) ;
#58380 = CIRCLE ( 'NONE', #781, 31.99999999999998224 ) ;
#58381 = ORIENTED_EDGE ( 'NONE', *, *, #41039, .F. ) ;
#58382 = EDGE_CURVE ( 'NONE', #49489, #11010, #56297, .T. ) ;
#58383 = CARTESIAN_POINT ( 'NONE',  ( -95.00000000000002842, 86.94004357329504273, 79.36374999999999602 ) ) ;
#58384 = EDGE_CURVE ( 'NONE', #28568, #31708, #55547, .T. ) ;
#58385 = CARTESIAN_POINT ( 'NONE',  ( -97.30629616937501680, 90.00000000000004263, 89.64281250086713726 ) ) ;
#58386 = FACE_OUTER_BOUND ( 'NONE', #56305, .T. ) ;
#58387 = PLANE ( 'NONE',  #57830 ) ;
#58388 = DIRECTION ( 'NONE',  ( -1.000000000000000000, -0.000000000000000000, 0.000000000000000000 ) ) ;
#58389 = CARTESIAN_POINT ( 'NONE',  ( 2.117611129180199558, -93.54218975225703048, 5.500000000000000000 ) ) ;
#58390 = VERTEX_POINT ( 'NONE', #66102 ) ;
#58391 = CARTESIAN_POINT ( 'NONE',  ( -2.500000000000020428, -90.00000000000000000, -90.00000000000000000 ) ) ;
#58392 = EDGE_CURVE ( 'NONE', #779, #26982, #72809, .T. ) ;
#58393 = CARTESIAN_POINT ( 'NONE',  ( -10.00000000000000000, 0.000000000000000000, 0.000000000000000000 ) ) ;
#58394 = FACE_OUTER_BOUND ( 'NONE', #59452, .T. ) ;
#58395 = CIRCLE ( 'NONE', #41589, 37.49900000000000944 ) ;
#58396 = DIRECTION ( 'NONE',  ( -1.000000000000000000, 0.000000000000000000, 0.000000000000000000 ) ) ;
#58397 = CARTESIAN_POINT ( 'NONE',  ( 0.000000000000000000, -3.925862922255855647, -41.81611651403866858 ) ) ;
#58398 = CARTESIAN_POINT ( 'NONE',  ( 10.00000000000000000, 0.000000000000000000, 0.000000000000000000 ) ) ;
#58399 = CARTESIAN_POINT ( 'NONE',  ( -97.30629616937495996, -209.9999999999999716, 84.72156250086715090 ) ) ;
#58400 = CARTESIAN_POINT ( 'NONE',  ( -12.50000000000000000, -132.5000000000000000, -40.00000000000000000 ) ) ;
#58401 = EDGE_CURVE ( 'NONE', #19772, #15350, #29417, .T. ) ;
#58402 = VECTOR ( 'NONE', #56063, 1000.000000000000000 ) ;
#58403 = CARTESIAN_POINT ( 'NONE',  ( 92.69370383062498320, 91.33154071421968467, 77.68364583420047609 ) ) ;
#58404 = CARTESIAN_POINT ( 'NONE',  ( -93.84685191531247028, -211.9973110713294489, 76.04322916753382344 ) ) ;
#58405 = DIRECTION ( 'NONE',  ( -1.000000000000000000, -0.000000000000000000, -0.000000000000000000 ) ) ;
#58406 = ORIENTED_EDGE ( 'NONE', *, *, #49580, .F. ) ;
#58407 = CARTESIAN_POINT ( 'NONE',  ( 96.32499999999998863, 87.70503267997126784, 87.75104166840095843 ) ) ;
#58408 = DIRECTION ( 'NONE',  ( -1.000000000000000000, -0.000000000000000000, 0.000000000000000000 ) ) ;
#58409 = CARTESIAN_POINT ( 'NONE',  ( 95.00000000000000000, -209.9999999999999716, 90.00000000000000000 ) ) ;
#58410 = AXIS2_PLACEMENT_3D ( 'NONE', #63279, #30514, #36529 ) ;
#58411 = VECTOR ( 'NONE', #21779, 1000.000000000000114 ) ;
#58412 = CARTESIAN_POINT ( 'NONE',  ( 5.000000000000000000, -39.04073710021356192, 15.48615015657568073 ) ) ;
#58413 = CARTESIAN_POINT ( 'NONE',  ( 97.30629616937498838, -209.9999999999999716, 77.89531250086714920 ) ) ;
#58414 = EDGE_LOOP ( 'NONE', ( #28928, #25387, #52248, #40823 ) ) ;
#58415 = EDGE_CURVE ( 'NONE', #59175, #48516, #20596, .T. ) ;
#58416 = ADVANCED_FACE ( 'NONE', ( #14952 ), #37894, .T. ) ;
#58417 = CIRCLE ( 'NONE', #44042, 82.00000000000000000 ) ;
#58418 = CARTESIAN_POINT ( 'NONE',  ( 11.99999999999999822, 51.03279382321088065, 55.19960302592086521 ) ) ;
#58419 = ORIENTED_EDGE ( 'NONE', *, *, #2156, .T. ) ;
#58420 = LINE ( 'NONE', #64441, #27909 ) ;
#58421 = ORIENTED_EDGE ( 'NONE', *, *, #27582, .T. ) ;
#58422 = CARTESIAN_POINT ( 'NONE',  ( 11.99999999999999822, 49.70050353004889132, 59.46389618801982380 ) ) ;
#58423 = AXIS2_PLACEMENT_3D ( 'NONE', #47329, #70233, #46963 ) ;
#58424 = ORIENTED_EDGE ( 'NONE', *, *, #65471, .F. ) ;
#58425 = EDGE_LOOP ( 'NONE', ( #20031, #28178, #29317, #24052 ) ) ;
#58426 = ORIENTED_EDGE ( 'NONE', *, *, #73905, .F. ) ;
#58427 = DIRECTION ( 'NONE',  ( 0.000000000000000000, -0.3090169943749349057, -0.9510565162951577500 ) ) ;
#58428 = ORIENTED_EDGE ( 'NONE', *, *, #72713, .T. ) ;
#58429 = EDGE_LOOP ( 'NONE', ( #44560, #53530, #47338, #1332 ) ) ;
#58430 = CARTESIAN_POINT ( 'NONE',  ( 93.84685191531248449, 88.00268892867053694, 82.28739583420048120 ) ) ;
#58431 = DIRECTION ( 'NONE',  ( 0.000000000000000000, 0.000000000000000000, 1.000000000000000000 ) ) ;
#58432 = LINE ( 'NONE', #6926, #32067 ) ;
#58433 = VERTEX_POINT ( 'NONE', #72452 ) ;
#58434 = ORIENTED_EDGE ( 'NONE', *, *, #1433, .F. ) ;
#58435 = ORIENTED_EDGE ( 'NONE', *, *, #3599, .F. ) ;
#58436 = DIRECTION ( 'NONE',  ( -1.000000000000000000, 3.061616997868382648E-16, 0.000000000000000000 ) ) ;
#58437 = ORIENTED_EDGE ( 'NONE', *, *, #16617, .T. ) ;
#58438 = AXIS2_PLACEMENT_3D ( 'NONE', #12524, #47488, #35461 ) ;
#58439 = DIRECTION ( 'NONE',  ( 0.000000000000000000, 0.000000000000000000, 1.000000000000000000 ) ) ;
#58440 = DIRECTION ( 'NONE',  ( 1.000000000000000000, 0.000000000000000000, 0.000000000000000000 ) ) ;
#58441 = CARTESIAN_POINT ( 'NONE',  ( 10.00000000000000000, 37.22597642581158084, -5.202137450156524068 ) ) ;
#58442 = DIRECTION ( 'NONE',  ( -1.000000000000000000, 0.000000000000000000, 0.000000000000000000 ) ) ;
#58443 = DIRECTION ( 'NONE',  ( -0.000000000000000000, -0.000000000000000000, 1.000000000000000000 ) ) ;
#58444 = CARTESIAN_POINT ( 'NONE',  ( 0.000000000000000000, -10.96151621346461447, -35.95386929396268272 ) ) ;
#58445 = CARTESIAN_POINT ( 'NONE',  ( -92.34999999999999432, -208.4700217866474645, 80.92479166840098515 ) ) ;
#58446 = ORIENTED_EDGE ( 'NONE', *, *, #66727, .T. ) ;
#58447 = DIRECTION ( 'NONE',  ( -0.000000000000000000, -0.000000000000000000, -1.000000000000000000 ) ) ;
#58448 = ORIENTED_EDGE ( 'NONE', *, *, #51793, .F. ) ;
#58449 = ADVANCED_FACE ( 'NONE', ( #43909 ), #41460, .F. ) ;
#58451 = CARTESIAN_POINT ( 'NONE',  ( -97.65000000000001990, 91.52997821335253548, 76.69145833506763665 ) ) ;
#58450 = CARTESIAN_POINT ( 'NONE',  ( 92.34999999999999432, 91.52997821335252127, 78.59645833506763779 ) ) ;
#58452 =( BOUNDED_SURFACE ( )  B_SPLINE_SURFACE ( 1, 2, ( 
 ( #42841, #60151, #10104, #72861, #21367, #61250, #54855, #49575, #20267, #44326, #33028, #27383, #25913, #66517, #55223, #9735, #3747, #48839, #26648, #66155, #21006, #67255, #72504, #60512, #50324, #14632, #73250, #66874, #8993, #31917, #15364, #38311, #19148, #24420, #71009, #1538, #65032, #53731, #59015, #53001, #58628, #792, #19512, #6405, #1904, #29670, #35340, #70633, #13509, #24068, #47357, #36803, #52618, #30417, #7137, #1171, #46992, #30783, #46614, #64646, #42093, #35687, #25169, #63921, #53363, #36434, #59380, #2273, #24789, #65400, #70263, #52250, #69904, #30050, #7868, #18770, #47720, #48095, #13131, #6761, #42460, #69547, #58265, #13865, #29306, #18044, #40986, #18400, #64289, #41347, #12393, #41709, #23682, #12760, #36069, #7507, #71376, #45344, #27277, #19880, #67518, #4757, #25898, #16383, #25526, #61888, #60137, #42827, #33670, #31165, #16006, #5124, #67893, #59752, #50588, #73888, #31905, #56625, #37195, #22397, #10368, #22022, #33288, #55867, #54115, #39325, #20247, #44601, #48460, #43217, #4379, #73515, #66140, #14617, #8234, #2647, #28025, #62261, #44967, #27663, #71744, #38952, #8619, #10746, #50967, #68268, #65757, #37566, #60499, #16764, #8980, #14240, #50207, #31530, #56242, #54469, #73141, #3005, #48826, #21647, #35523, #46074, #23883, #70093, #47181, #617, #45724, #57351, #6948, #40060, #260, #57730, #56992, #46439, #63021, #23508, #1366, #39702, #35157, #69367, #69734, #989, #69009, #24257, #64111, #29136, #52072, #62641, #17495, #12592, #5863, #11117, #46819, #5497, #28393, #29872, #12220, #34789, #63372, #17863, #52435, #6236, #52824, #40809, #18234, #58450, #63744, #11838, #40424, #34041, #51329, #74265, #58093, #11480, #68646, #29499, #41175, #28772, #6595, #22782, #34408, #17128, #51712, #23151, #36262, #43026, #65588, #65220, #42650, #71574, #7333, #24980, #14055, #47915, #19702, #30608, #53936, #35885, #7691, #70834, #49015, #8443, #71196, #2831, #64473, #59958, #42291, #31354, #13691, #12948, #8059, #65967, #18960, #58833, #53556, #2093, #54667, #36628, #59573, #30249, #37393, #37005, #54306, #2474, #24612, #25361, #19335, #30980, #3195, #48288, #25720, #48659, #64849, #20071, #14439, #60327, #47549, #70453, #8805, #26085, #31722, #13328, #53188, #18596, #41536 ),
 ( #1724, #41909, #59200, #14809, #39235, #4666, #33203, #15924, #9547, #4296, #49395, #73429, #44879, #67801, #60690, #32463, #3928, #38857, #49750, #20460, #38490, #9169, #16295, #44511, #73047, #55778, #3561, #27184, #26824, #72673, #33577, #21175, #61800, #56147, #43772, #55405, #44126, #67050, #26459, #72321, #27573, #56534, #15557, #66691, #43414, #9908, #62165, #61050, #20820, #61429, #10281, #32829, #71946, #38111, #32092, #50112, #67428, #10651, #21553, #50501, #37756, #5037, #27942, #21936, #66336, #55032, #15177, #57266, #63659, #11390, #17041, #46726, #34324, #29405, #23062, #74173, #63286, #12500, #5771, #900, #39977, #35435, #35071, #68170, #39608, #41090, #23423, #45991, #171, #29052, #12128, #68919, #64023, #17405, #58002, #23787, #51982, #40340, #28678, #45253, #58365, #50872, #46354, #22688, #5410, #40715, #6506, #68554, #11745, #6865, #45636, #528, #51619, #62932, #34692, #69650, #69284, #57646, #17769, #52353, #62550, #6146, #18144, #73795, #22309, #16670, #11031, #33955, #56904, #28305, #51241, #19616, #7972, #13968, #1280, #71110, #53468, #42562, #2005, #24167, #19250, #54219, #30157, #47100, #18873, #41811, #65868, #47822, #70744, #36536, #48199, #70367, #59859, #70004, #30890, #53102, #64389, #2749, #18507, #59482, #48569, #36912, #29776, #65501, #42937, #24895, #25633, #7245, #14353, #53834, #8348, #2382, #42200, #41447, #31270, #64758, #13609, #12861, #13243, #65135, #71481, #36172, #59118, #52730, #35790, #19982, #37304, #60239, #58745, #7607, #25275, #1640, #24525, #47460, #30521, #71847, #43682, #15082, #27094, #60955, #31635, #49660, #54578, #61339, #21454, #26729, #26368, #72951, #3105, #4574, #38023, #67337, #39140, #16201, #44043, #14716, #49298, #50407, #9078, #66602, #72585, #25999, #15454, #32003, #66957, #44788, #8718, #4202, #38399, #38766, #44416, #9446, #67711, #33108, #21085, #48924, #9818, #15837, #32371, #27470, #66242, #32734, #61704, #10186, #56057, #55686, #20364, #50026, #43321, #3463, #55314, #73334, #21841, #37667, #60601, #54943, #72223, #20730, #3832, #16573, #23336, #17688, #73706, #27850, #74082, #45540, #10941, #22216, #57180, #62078, #69560, #69196, #5321, #45158, #46632, #28585, #68082, #62840, #33864, #28219, #12042, #34602, #34236, #11660, #40625 ) ),
 .UNSPECIFIED., .F., .F., .F. ) 
 B_SPLINE_SURFACE_WITH_KNOTS ( ( 2, 2 ),
 ( 3, 2, 2, 2, 2, 2, 2, 2, 2, 2, 2, 2, 2, 2, 2, 2, 2, 2, 2, 2, 2, 2, 2, 2, 2, 2, 2, 2, 2, 2, 2, 2, 2, 2, 2, 2, 2, 2, 2, 2, 2, 2, 2, 2, 2, 2, 2, 2, 2, 2, 2, 2, 2, 2, 2, 2, 2, 2, 2, 2, 2, 2, 2, 2, 2, 2, 2, 2, 2, 2, 2, 2, 2, 2, 2, 2, 2, 2, 2, 2, 2, 2, 2, 2, 2, 2, 2, 2, 2, 2, 2, 2, 2, 2, 2, 2, 2, 2, 2, 2, 2, 2, 2, 2, 2, 2, 2, 2, 2, 2, 2, 2, 2, 2, 2, 2, 2, 2, 2, 2, 2, 2, 2, 2, 2, 2, 2, 2, 2, 2, 2, 2, 2, 2, 2, 2, 2, 2, 2, 2, 2, 2, 3 ),
 ( 0.000000000000000000, 1.000000000000000000 ),
 ( 0.000000000000000000, 0.006944444444444444059, 0.01388888888888888812, 0.02083333333333333218, 0.02777777777777777624, 0.03472222222222222376, 0.04166666666666666435, 0.04861111111111111188, 0.05555555555555555247, 0.06250000000000000000, 0.06944444444444444753, 0.07638888888888889506, 0.08333333333333332871, 0.09027777777777777624, 0.09722222222222222376, 0.1041666666666666713, 0.1111111111111111049, 0.1180555555555555525, 0.1250000000000000000, 0.1319444444444444475, 0.1388888888888888951, 0.1458333333333333426, 0.1527777777777777901, 0.1597222222222222099, 0.1666666666666666574, 0.1736111111111111049, 0.1805555555555555525, 0.1875000000000000000, 0.1944444444444444475, 0.2013888888888888951, 0.2083333333333333426, 0.2152777777777777901, 0.2222222222222222099, 0.2291666666666666574, 0.2361111111111111049, 0.2430555555555555525, 0.2500000000000000000, 0.2569444444444444198, 0.2638888888888888951, 0.2708333333333333148, 0.2777777777777777901, 0.2847222222222222099, 0.2916666666666666852, 0.2986111111111111049, 0.3055555555555555802, 0.3125000000000000000, 0.3194444444444444198, 0.3263888888888888951, 0.3333333333333333148, 0.3402777777777777901, 0.3472222222222222099, 0.3541666666666666852, 0.3611111111111111049, 0.3680555555555555802, 0.3750000000000000000, 0.3819444444444444198, 0.3888888888888888951, 0.3958333333333333148, 0.4027777777777777901, 0.4097222222222222099, 0.4166666666666666852, 0.4236111111111111049, 0.4305555555555555802, 0.4375000000000000000, 0.4444444444444444198, 0.4513888888888888951, 0.4583333333333333148, 0.4652777777777777901, 0.4722222222222222099, 0.4791666666666666852, 0.4861111111111111049, 0.4930555555555555802, 0.5000000000000000000, 0.5069444444444444198, 0.5138888888888888395, 0.5208333333333333703, 0.5277777777777777901, 0.5347222222222222099, 0.5416666666666666297, 0.5486111111111111605, 0.5555555555555555802, 0.5625000000000000000, 0.5694444444444444198, 0.5763888888888888395, 0.5833333333333333703, 0.5902777777777777901, 0.5972222222222222099, 0.6041666666666666297, 0.6111111111111111605, 0.6180555555555555802, 0.6250000000000000000, 0.6319444444444444198, 0.6388888888888888395, 0.6458333333333333703, 0.6527777777777777901, 0.6597222222222222099, 0.6666666666666666297, 0.6736111111111111605, 0.6805555555555555802, 0.6875000000000000000, 0.6944444444444444198, 0.7013888888888888395, 0.7083333333333333703, 0.7152777777777777901, 0.7222222222222222099, 0.7291666666666666297, 0.7361111111111111605, 0.7430555555555555802, 0.7500000000000000000, 0.7569444444444444198, 0.7638888888888888395, 0.7708333333333333703, 0.7777777777777777901, 0.7847222222222222099, 0.7916666666666666297, 0.7986111111111111605, 0.8055555555555555802, 0.8125000000000000000, 0.8194444444444444198, 0.8263888888888888395, 0.8333333333333333703, 0.8402777777777777901, 0.8472222222222222099, 0.8541666666666666297, 0.8611111111111111605, 0.8680555555555555802, 0.8750000000000000000, 0.8819444444444444198, 0.8888888888888888395, 0.8958333333333333703, 0.9027777777777777901, 0.9097222222222222099, 0.9166666666666666297, 0.9236111111111111605, 0.9305555555555555802, 0.9375000000000000000, 0.9444444444444444198, 0.9513888888888888395, 0.9583333333333333703, 0.9652777777777777901, 0.9722222222222222099, 0.9791666666666666297, 0.9842226981114291506 ),
 .UNSPECIFIED. ) 
 GEOMETRIC_REPRESENTATION_ITEM ( )  RATIONAL_B_SPLINE_SURFACE ( (
 ( 1.000000000000000000, 0.8660254037844387076, 1.000000000000000000, 0.8660254037844387076, 1.000000000000000000, 0.8660254037844387076, 1.000000000000000000, 0.8660254037844387076, 1.000000000000000000, 0.8660254037844387076, 1.000000000000000000, 0.8660254037844387076, 1.000000000000000000, 0.8660254037844387076, 1.000000000000000000, 0.8660254037844387076, 1.000000000000000000, 0.8660254037844387076, 1.000000000000000000, 0.8660254037844387076, 1.000000000000000000, 0.8660254037844387076, 1.000000000000000000, 0.8660254037844387076, 1.000000000000000000, 0.8660254037844387076, 1.000000000000000000, 0.8660254037844387076, 1.000000000000000000, 0.8660254037844387076, 1.000000000000000000, 0.8660254037844387076, 1.000000000000000000, 0.8660254037844387076, 1.000000000000000000, 0.8660254037844387076, 1.000000000000000000, 0.8660254037844387076, 1.000000000000000000, 0.8660254037844387076, 1.000000000000000000, 0.8660254037844387076, 1.000000000000000000, 0.8660254037844387076, 1.000000000000000000, 0.8660254037844387076, 1.000000000000000000, 0.8660254037844387076, 1.000000000000000000, 0.8660254037844387076, 1.000000000000000000, 0.8660254037844387076, 1.000000000000000000, 0.8660254037844387076, 1.000000000000000000, 0.8660254037844387076, 1.000000000000000000, 0.8660254037844387076, 1.000000000000000000, 0.8660254037844387076, 1.000000000000000000, 0.8660254037844387076, 1.000000000000000000, 0.8660254037844387076, 1.000000000000000000, 0.8660254037844387076, 1.000000000000000000, 0.8660254037844387076, 1.000000000000000000, 0.8660254037844387076, 1.000000000000000000, 0.8660254037844387076, 1.000000000000000000, 0.8660254037844387076, 1.000000000000000000, 0.8660254037844387076, 1.000000000000000000, 0.8660254037844387076, 1.000000000000000000, 0.8660254037844387076, 1.000000000000000000, 0.8660254037844387076, 1.000000000000000000, 0.8660254037844387076, 1.000000000000000000, 0.8660254037844387076, 1.000000000000000000, 0.8660254037844387076, 1.000000000000000000, 0.8660254037844387076, 1.000000000000000000, 0.8660254037844387076, 1.000000000000000000, 0.8660254037844387076, 1.000000000000000000, 0.8660254037844387076, 1.000000000000000000, 0.8660254037844387076, 1.000000000000000000, 0.8660254037844387076, 1.000000000000000000, 0.8660254037844387076, 1.000000000000000000, 0.8660254037844387076, 1.000000000000000000, 0.8660254037844387076, 1.000000000000000000, 0.8660254037844387076, 1.000000000000000000, 0.8660254037844387076, 1.000000000000000000, 0.8660254037844387076, 1.000000000000000000, 0.8660254037844387076, 1.000000000000000000, 0.8660254037844387076, 1.000000000000000000, 0.8660254037844387076, 1.000000000000000000, 0.8660254037844387076, 1.000000000000000000, 0.8660254037844387076, 1.000000000000000000, 0.8660254037844387076, 1.000000000000000000, 0.8660254037844387076, 1.000000000000000000, 0.8660254037844387076, 1.000000000000000000, 0.8660254037844387076, 1.000000000000000000, 0.8660254037844387076, 1.000000000000000000, 0.8660254037844387076, 1.000000000000000000, 0.8660254037844387076, 1.000000000000000000, 0.8660254037844387076, 1.000000000000000000, 0.8660254037844387076, 1.000000000000000000, 0.8660254037844387076, 1.000000000000000000, 0.8660254037844387076, 1.000000000000000000, 0.8660254037844387076, 1.000000000000000000, 0.8660254037844387076, 1.000000000000000000, 0.8660254037844387076, 1.000000000000000000, 0.8660254037844387076, 1.000000000000000000, 0.8660254037844387076, 1.000000000000000000, 0.8660254037844387076, 1.000000000000000000, 0.8660254037844387076, 1.000000000000000000, 0.8660254037844387076, 1.000000000000000000, 0.8660254037844387076, 1.000000000000000000, 0.8660254037844387076, 1.000000000000000000, 0.8660254037844387076, 1.000000000000000000, 0.8660254037844387076, 1.000000000000000000, 0.8660254037844387076, 1.000000000000000000, 0.8660254037844387076, 1.000000000000000000, 0.8660254037844387076, 1.000000000000000000, 0.8660254037844387076, 1.000000000000000000, 0.8660254037844387076, 1.000000000000000000, 0.8660254037844387076, 1.000000000000000000, 0.8660254037844387076, 1.000000000000000000, 0.8660254037844387076, 1.000000000000000000, 0.8660254037844387076, 1.000000000000000000, 0.8660254037844387076, 1.000000000000000000, 0.8660254037844387076, 1.000000000000000000, 0.8660254037844387076, 1.000000000000000000, 0.8660254037844387076, 1.000000000000000000, 0.8660254037844387076, 1.000000000000000000, 0.8660254037844387076, 1.000000000000000000, 0.8660254037844387076, 1.000000000000000000, 0.8660254037844387076, 1.000000000000000000, 0.8660254037844387076, 1.000000000000000000, 0.8660254037844387076, 1.000000000000000000, 0.8660254037844387076, 1.000000000000000000, 0.8660254037844387076, 1.000000000000000000, 0.8660254037844387076, 1.000000000000000000, 0.8660254037844387076, 1.000000000000000000, 0.8660254037844387076, 1.000000000000000000, 0.8660254037844387076, 1.000000000000000000, 0.8660254037844387076, 1.000000000000000000, 0.8660254037844387076, 1.000000000000000000, 0.8660254037844387076, 1.000000000000000000, 0.8660254037844387076, 1.000000000000000000, 0.8660254037844387076, 1.000000000000000000, 0.8660254037844387076, 1.000000000000000000, 0.8660254037844387076, 1.000000000000000000, 0.8660254037844387076, 1.000000000000000000, 0.8660254037844387076, 1.000000000000000000, 0.8660254037844387076, 1.000000000000000000, 0.8660254037844387076, 1.000000000000000000, 0.8660254037844387076, 1.000000000000000000, 0.8660254037844387076, 1.000000000000000000, 0.8660254037844387076, 1.000000000000000000, 0.8660254037844387076, 1.000000000000000000, 0.8660254037844387076, 1.000000000000000000, 0.8660254037844387076, 1.000000000000000000, 0.8660254037844387076, 1.000000000000000000, 0.8660254037844387076, 1.000000000000000000, 0.8660254037844387076, 1.000000000000000000, 0.8660254037844387076, 1.000000000000000000, 0.8660254037844387076, 1.000000000000000000, 0.8660254037844387076, 1.000000000000000000, 0.8660254037844387076, 1.000000000000000000, 0.8660254037844387076, 1.000000000000000000, 0.8660254037844387076, 1.000000000000000000, 0.8660254037844387076, 1.000000000000000000, 0.8660254037844387076, 1.000000000000000000, 0.8660254037844387076, 1.000000000000000000, 0.8660254037844387076, 1.000000000000000000, 0.8660254037844387076, 1.000000000000000000, 0.8660254037844387076, 1.000000000000000000, 0.9024573129378067327, 0.9469501470576184854),
 ( 1.000000000000000000, 0.8660254037844387076, 1.000000000000000000, 0.8660254037844387076, 1.000000000000000000, 0.8660254037844387076, 1.000000000000000000, 0.8660254037844387076, 1.000000000000000000, 0.8660254037844387076, 1.000000000000000000, 0.8660254037844387076, 1.000000000000000000, 0.8660254037844387076, 1.000000000000000000, 0.8660254037844387076, 1.000000000000000000, 0.8660254037844387076, 1.000000000000000000, 0.8660254037844387076, 1.000000000000000000, 0.8660254037844387076, 1.000000000000000000, 0.8660254037844387076, 1.000000000000000000, 0.8660254037844387076, 1.000000000000000000, 0.8660254037844387076, 1.000000000000000000, 0.8660254037844387076, 1.000000000000000000, 0.8660254037844387076, 1.000000000000000000, 0.8660254037844387076, 1.000000000000000000, 0.8660254037844387076, 1.000000000000000000, 0.8660254037844387076, 1.000000000000000000, 0.8660254037844387076, 1.000000000000000000, 0.8660254037844387076, 1.000000000000000000, 0.8660254037844387076, 1.000000000000000000, 0.8660254037844387076, 1.000000000000000000, 0.8660254037844387076, 1.000000000000000000, 0.8660254037844387076, 1.000000000000000000, 0.8660254037844387076, 1.000000000000000000, 0.8660254037844387076, 1.000000000000000000, 0.8660254037844387076, 1.000000000000000000, 0.8660254037844387076, 1.000000000000000000, 0.8660254037844387076, 1.000000000000000000, 0.8660254037844387076, 1.000000000000000000, 0.8660254037844387076, 1.000000000000000000, 0.8660254037844387076, 1.000000000000000000, 0.8660254037844387076, 1.000000000000000000, 0.8660254037844387076, 1.000000000000000000, 0.8660254037844387076, 1.000000000000000000, 0.8660254037844387076, 1.000000000000000000, 0.8660254037844387076, 1.000000000000000000, 0.8660254037844387076, 1.000000000000000000, 0.8660254037844387076, 1.000000000000000000, 0.8660254037844387076, 1.000000000000000000, 0.8660254037844387076, 1.000000000000000000, 0.8660254037844387076, 1.000000000000000000, 0.8660254037844387076, 1.000000000000000000, 0.8660254037844387076, 1.000000000000000000, 0.8660254037844387076, 1.000000000000000000, 0.8660254037844387076, 1.000000000000000000, 0.8660254037844387076, 1.000000000000000000, 0.8660254037844387076, 1.000000000000000000, 0.8660254037844387076, 1.000000000000000000, 0.8660254037844387076, 1.000000000000000000, 0.8660254037844387076, 1.000000000000000000, 0.8660254037844387076, 1.000000000000000000, 0.8660254037844387076, 1.000000000000000000, 0.8660254037844387076, 1.000000000000000000, 0.8660254037844387076, 1.000000000000000000, 0.8660254037844387076, 1.000000000000000000, 0.8660254037844387076, 1.000000000000000000, 0.8660254037844387076, 1.000000000000000000, 0.8660254037844387076, 1.000000000000000000, 0.8660254037844387076, 1.000000000000000000, 0.8660254037844387076, 1.000000000000000000, 0.8660254037844387076, 1.000000000000000000, 0.8660254037844387076, 1.000000000000000000, 0.8660254037844387076, 1.000000000000000000, 0.8660254037844387076, 1.000000000000000000, 0.8660254037844387076, 1.000000000000000000, 0.8660254037844387076, 1.000000000000000000, 0.8660254037844387076, 1.000000000000000000, 0.8660254037844387076, 1.000000000000000000, 0.8660254037844387076, 1.000000000000000000, 0.8660254037844387076, 1.000000000000000000, 0.8660254037844387076, 1.000000000000000000, 0.8660254037844387076, 1.000000000000000000, 0.8660254037844387076, 1.000000000000000000, 0.8660254037844387076, 1.000000000000000000, 0.8660254037844387076, 1.000000000000000000, 0.8660254037844387076, 1.000000000000000000, 0.8660254037844387076, 1.000000000000000000, 0.8660254037844387076, 1.000000000000000000, 0.8660254037844387076, 1.000000000000000000, 0.8660254037844387076, 1.000000000000000000, 0.8660254037844387076, 1.000000000000000000, 0.8660254037844387076, 1.000000000000000000, 0.8660254037844387076, 1.000000000000000000, 0.8660254037844387076, 1.000000000000000000, 0.8660254037844387076, 1.000000000000000000, 0.8660254037844387076, 1.000000000000000000, 0.8660254037844387076, 1.000000000000000000, 0.8660254037844387076, 1.000000000000000000, 0.8660254037844387076, 1.000000000000000000, 0.8660254037844387076, 1.000000000000000000, 0.8660254037844387076, 1.000000000000000000, 0.8660254037844387076, 1.000000000000000000, 0.8660254037844387076, 1.000000000000000000, 0.8660254037844387076, 1.000000000000000000, 0.8660254037844387076, 1.000000000000000000, 0.8660254037844387076, 1.000000000000000000, 0.8660254037844387076, 1.000000000000000000, 0.8660254037844387076, 1.000000000000000000, 0.8660254037844387076, 1.000000000000000000, 0.8660254037844387076, 1.000000000000000000, 0.8660254037844387076, 1.000000000000000000, 0.8660254037844387076, 1.000000000000000000, 0.8660254037844387076, 1.000000000000000000, 0.8660254037844387076, 1.000000000000000000, 0.8660254037844387076, 1.000000000000000000, 0.8660254037844387076, 1.000000000000000000, 0.8660254037844387076, 1.000000000000000000, 0.8660254037844387076, 1.000000000000000000, 0.8660254037844387076, 1.000000000000000000, 0.8660254037844387076, 1.000000000000000000, 0.8660254037844387076, 1.000000000000000000, 0.8660254037844387076, 1.000000000000000000, 0.8660254037844387076, 1.000000000000000000, 0.8660254037844387076, 1.000000000000000000, 0.8660254037844387076, 1.000000000000000000, 0.8660254037844387076, 1.000000000000000000, 0.8660254037844387076, 1.000000000000000000, 0.8660254037844387076, 1.000000000000000000, 0.8660254037844387076, 1.000000000000000000, 0.8660254037844387076, 1.000000000000000000, 0.8660254037844387076, 1.000000000000000000, 0.8660254037844387076, 1.000000000000000000, 0.8660254037844387076, 1.000000000000000000, 0.8660254037844387076, 1.000000000000000000, 0.8660254037844387076, 1.000000000000000000, 0.8660254037844387076, 1.000000000000000000, 0.8660254037844387076, 1.000000000000000000, 0.8660254037844387076, 1.000000000000000000, 0.8660254037844387076, 1.000000000000000000, 0.8660254037844387076, 1.000000000000000000, 0.8660254037844387076, 1.000000000000000000, 0.8660254037844387076, 1.000000000000000000, 0.8660254037844387076, 1.000000000000000000, 0.8660254037844387076, 1.000000000000000000, 0.8660254037844387076, 1.000000000000000000, 0.8660254037844387076, 1.000000000000000000, 0.8660254037844387076, 1.000000000000000000, 0.8660254037844387076, 1.000000000000000000, 0.8660254037844387076, 1.000000000000000000, 0.9024573129378067327, 0.9469501470576184854) ) ) 
 REPRESENTATION_ITEM ( '' )  SURFACE ( )  );
#58453 = EDGE_LOOP ( 'NONE', ( #5230, #53609, #10987, #26922 ) ) ;
#58454 = CARTESIAN_POINT ( 'NONE',  ( 97.30629616937498838, 91.33154071421968467, 80.64697916753382856 ) ) ;
#58455 = AXIS2_PLACEMENT_3D ( 'NONE', #19532, #53025, #48846 ) ;
#58456 = CYLINDRICAL_SURFACE ( 'NONE', #73359, 37.49900000000000233 ) ;
#58457 = CARTESIAN_POINT ( 'NONE',  ( 0.000000000000000000, 0.000000000000000000, -270.0000000000000000 ) ) ;
#58458 = EDGE_CURVE ( 'NONE', #30220, #6668, #74319, .T. ) ;
#58459 = CARTESIAN_POINT ( 'NONE',  ( 94.99999999999998579, 90.00000000000002842, 90.00000000000000000 ) ) ;
#58460 = CYLINDRICAL_SURFACE ( 'NONE', #70215, 31.99999999999999289 ) ;
#58461 = ORIENTED_EDGE ( 'NONE', *, *, #56809, .F. ) ;
#58462 = DIRECTION ( 'NONE',  ( 0.8571673007021122226, 0.000000000000000000, 0.5150380749100542666 ) ) ;
#58463 = LINE ( 'NONE', #30994, #15603 ) ;
#58464 = EDGE_LOOP ( 'NONE', ( #15407, #35201, #13130, #45429 ) ) ;
#58465 = EDGE_CURVE ( 'NONE', #34514, #9311, #68320, .T. ) ;
#58466 = VECTOR ( 'NONE', #38163, 1000.000000000000000 ) ;
#58467 = ORIENTED_EDGE ( 'NONE', *, *, #13212, .T. ) ;
#58468 = ADVANCED_FACE ( 'NONE', ( #16815 ), #28825, .F. ) ;
#58469 = PRODUCT_DEFINITION_SHAPE ( 'NONE', 'NONE',  #74359 ) ;
#58470 = LINE ( 'NONE', #4877, #5729 ) ;
#58471 = VECTOR ( 'NONE', #53677, 1000.000000000000000 ) ;
#58472 = AXIS2_PLACEMENT_3D ( 'NONE', #24471, #2323, #42504 ) ;
#58473 = CARTESIAN_POINT ( 'NONE',  ( -3.101151694651716806, -3.983051926191232717, -0.6020238742160465284 ) ) ;
#58474 = CARTESIAN_POINT ( 'NONE',  ( -97.65000000000003411, -208.4700217866474929, 75.97708333333333997 ) ) ;
#58475 = CARTESIAN_POINT ( 'NONE',  ( -97.30629616937497417, -211.3315407142195852, 77.15447916753382174 ) ) ;
#58476 = ORIENTED_EDGE ( 'NONE', *, *, #18994, .F. ) ;
#58477 = CIRCLE ( 'NONE', #21214, 82.00000000000000000 ) ;
#58478 = EDGE_CURVE ( 'NONE', #40782, #70651, #34459, .T. ) ;
#58479 = LINE ( 'NONE', #17519, #71497 ) ;
#58480 = DIRECTION ( 'NONE',  ( 1.000000000000000000, 0.000000000000000000, 0.000000000000000000 ) ) ;
#58481 = LINE ( 'NONE', #1390, #2250 ) ;
#58482 = DIRECTION ( 'NONE',  ( -0.000000000000000000, -0.000000000000000000, 1.000000000000000000 ) ) ;
#58483 = CARTESIAN_POINT ( 'NONE',  ( -15.06715634359041900, 1.845194478843074636E-15, 0.000000000000000000 ) ) ;
#58484 = LINE ( 'NONE', #6978, #31237 ) ;
#58485 = CYLINDRICAL_SURFACE ( 'NONE', #4917, 77.49899999999999523 ) ;
#58486 = DIRECTION ( 'NONE',  ( -0.2306669878475648139, -0.9730327541852491491, 0.000000000000000000 ) ) ;
#58487 = AXIS2_PLACEMENT_3D ( 'NONE', #6473, #69244, #34659 ) ;
#58488 = DIRECTION ( 'NONE',  ( 0.000000000000000000, -0.4539904997395352027, -0.8910065241883737830 ) ) ;
#58489 = EDGE_CURVE ( 'NONE', #71472, #43291, #60675, .T. ) ;
#58490 = EDGE_CURVE ( 'NONE', #44844, #11817, #57403, .T. ) ;
#58491 = CARTESIAN_POINT ( 'NONE',  ( 92.69370383062498320, 90.00000000000002842, 87.89656250086714806 ) ) ;
#58492 = CARTESIAN_POINT ( 'NONE',  ( -94.99999999999997158, -207.3369185715606307, 87.10281250086715943 ) ) ;
#58493 = FACE_OUTER_BOUND ( 'NONE', #25736, .T. ) ;
#58494 = VERTEX_POINT ( 'NONE', #17543 ) ;
#58495 = CARTESIAN_POINT ( 'NONE',  ( -93.67500000000003979, 92.29496732002878900, 81.53333333333333144 ) ) ;
#58496 = CARTESIAN_POINT ( 'NONE',  ( -96.32499999999996021, -212.2949673200287179, 82.48583333333333201 ) ) ;
#58497 = CARTESIAN_POINT ( 'NONE',  ( -97.30629616937501680, 88.66845928578038638, 76.99572916753380980 ) ) ;
#58498 = ADVANCED_FACE ( 'NONE', ( #57776 ), #5176, .T. ) ;
#58499 = CARTESIAN_POINT ( 'NONE',  ( 93.84685191531251292, -211.9973110713294489, 87.84364583420047268 ) ) ;
#58500 = ORIENTED_EDGE ( 'NONE', *, *, #43706, .T. ) ;
#58501 = EDGE_CURVE ( 'NONE', #63724, #42793, #3058, .T. ) ;
#58502 =( REPRESENTATION_RELATIONSHIP ('NONE','NONE', #31117, #50888 ) REPRESENTATION_RELATIONSHIP_WITH_TRANSFORMATION ( #44778 )SHAPE_REPRESENTATION_RELATIONSHIP( ) );
#58503 = VERTEX_POINT ( 'NONE', #34841 ) ;
#58504 = AXIS2_PLACEMENT_3D ( 'NONE', #70199, #2938, #30720 ) ;
#58505 = EDGE_LOOP ( 'NONE', ( #52323, #36052, #61309, #1089 ) ) ;
#58506 = CIRCLE ( 'NONE', #26093, 12.49999999999999645 ) ;
#58507 = ADVANCED_FACE ( 'NONE', ( #17181 ), #34095, .F. ) ;
#58508 = DIRECTION ( 'NONE',  ( -0.000000000000000000, -0.000000000000000000, 1.000000000000000000 ) ) ;
#58509 = DIRECTION ( 'NONE',  ( 0.000000000000000000, -0.000000000000000000, 1.000000000000000000 ) ) ;
#58510 = AXIS2_PLACEMENT_3D ( 'NONE', #51535, #46273, #52274 ) ;
#58511 = ORIENTED_EDGE ( 'NONE', *, *, #45139, .T. ) ;
#58512 = VECTOR ( 'NONE', #55438, 1000.000000000000000 ) ;
#58513 = ORIENTED_EDGE ( 'NONE', *, *, #64352, .T. ) ;
#58514 = CARTESIAN_POINT ( 'NONE',  ( 93.84685191531251292, -211.9973110713294489, 82.28739583420048120 ) ) ;
#58515 = CARTESIAN_POINT ( 'NONE',  ( 14.59956846177685996, -138.4757300459248484, -5.500000000000000000 ) ) ;
#58516 = DIRECTION ( 'NONE',  ( -1.000000000000000000, -1.343011723336883198E-16, -0.000000000000000000 ) ) ;
#58517 = CARTESIAN_POINT ( 'NONE',  ( 5.000000000000000000, 6.074766241781102566E-16, -0.5080592402122449114 ) ) ;
#58518 = DIRECTION ( 'NONE',  ( -1.000000000000000000, -0.000000000000000000, -0.000000000000000000 ) ) ;
#58519 = CARTESIAN_POINT ( 'NONE',  ( 0.000000000000000000, -120.0000000000000000, -2.500000000000000000 ) ) ;
#58520 = CARTESIAN_POINT ( 'NONE',  ( 95.00000000000000000, -213.0599564267049857, 84.44375000000000853 ) ) ;
#58521 = ORIENTED_EDGE ( 'NONE', *, *, #55945, .F. ) ;
#58522 = ORIENTED_EDGE ( 'NONE', *, *, #25151, .T. ) ;
#58523 = VERTEX_POINT ( 'NONE', #62317 ) ;
#58524 = VERTEX_POINT ( 'NONE', #40113 ) ;
#58525 = SURFACE_SIDE_STYLE ('',( #12658 ) ) ;
#58526 = AXIS2_PLACEMENT_3D ( 'NONE', #10064, #40128, #63084 ) ;
#58527 =( LENGTH_UNIT ( ) NAMED_UNIT ( * ) SI_UNIT ( .MILLI., .METRE. ) );
#58528 = CARTESIAN_POINT ( 'NONE',  ( -97.30629616937501680, 91.33154071421968467, 86.57364583420047666 ) ) ;
#58529 = CARTESIAN_POINT ( 'NONE',  ( 0.000000000000000000, -120.0000000000000000, 5.500000000000000000 ) ) ;
#58530 = CYLINDRICAL_SURFACE ( 'NONE', #56960, 2.499999999999999556 ) ;
#58531 = CARTESIAN_POINT ( 'NONE',  ( 92.69370383062501162, -208.6684592857803011, 88.31989583420046586 ) ) ;
#58532 = CARTESIAN_POINT ( 'NONE',  ( 93.67499999999998295, 92.29496732002878900, 79.73416666666666686 ) ) ;
#58533 = AXIS2_PLACEMENT_3D ( 'NONE', #52996, #18394, #24413 ) ;
#58534 = ORIENTED_EDGE ( 'NONE', *, *, #23597, .T. ) ;
#58535 = CARTESIAN_POINT ( 'NONE',  ( -92.34999999999999432, -209.9999999999999716, 87.85687500173429498 ) ) ;
#58536 = ORIENTED_EDGE ( 'NONE', *, *, #10429, .F. ) ;
#58537 = DIRECTION ( 'NONE',  ( 0.000000000000000000, 0.000000000000000000, 1.000000000000000000 ) ) ;
#58538 = VERTEX_POINT ( 'NONE', #669 ) ;
#58539 = CARTESIAN_POINT ( 'NONE',  ( -95.00000000000002842, 86.94004357329504273, 87.69812500173429726 ) ) ;
#58540 = CARTESIAN_POINT ( 'NONE',  ( 96.15314808468748708, 91.99731107132950569, 76.09614583420047040 ) ) ;
#58541 = VERTEX_POINT ( 'NONE', #33727 ) ;
#58542 = DIRECTION ( 'NONE',  ( -1.000000000000000000, 0.000000000000000000, -0.000000000000000000 ) ) ;
#58543 = PLANE ( 'NONE',  #13663 ) ;
#58544 = CARTESIAN_POINT ( 'NONE',  ( 10.00000000000000000, -6.555932627142676772, 37.01155633439056203 ) ) ;
#58545 = EDGE_CURVE ( 'NONE', #69481, #7050, #67895, .T. ) ;
#58546 = CYLINDRICAL_SURFACE ( 'NONE', #58727, 2.649999999999985700 ) ;
#58547 = ORIENTED_EDGE ( 'NONE', *, *, #3514, .T. ) ;
#58548 = CARTESIAN_POINT ( 'NONE',  ( -92.35000000045957336, 90.00004935162611730, 87.22187670868784437 ) ) ;
#58549 = LINE ( 'NONE', #18692, #58761 ) ;
#58550 = EDGE_LOOP ( 'NONE', ( #5606, #57617, #47443, #25314 ) ) ;
#58551 = EDGE_CURVE ( 'NONE', #73369, #50841, #39373, .T. ) ;
#58552 = VERTEX_POINT ( 'NONE', #51019 ) ;
#58553 = DIRECTION ( 'NONE',  ( 1.000000000000000000, 0.000000000000000000, 0.000000000000000000 ) ) ;
#58554 = ADVANCED_FACE ( 'NONE', ( #21249 ), #38189, .F. ) ;
#58555 = EDGE_CURVE ( 'NONE', #50077, #30232, #70245, .T. ) ;
#58556 = DIRECTION ( 'NONE',  ( 0.000000000000000000, 0.000000000000000000, 1.000000000000000000 ) ) ;
#58557 = CARTESIAN_POINT ( 'NONE',  ( -97.65000000002666525, 90.00000000000008527, -74.99999999999992895 ) ) ;
#58558 = ORIENTED_EDGE ( 'NONE', *, *, #29121, .T. ) ;
#58559 = CARTESIAN_POINT ( 'NONE',  ( -94.99999999999997158, -212.6630814284392557, 86.78531250086716398 ) ) ;
#58560 = EDGE_LOOP ( 'NONE', ( #70231, #42804, #22550, #22204 ) ) ;
#58561 = CIRCLE ( 'NONE', #51368, 77.49899999999999523 ) ;
#58562 = DIRECTION ( 'NONE',  ( 0.000000000000000000, -0.4539904997395351471, -0.8910065241883737830 ) ) ;
#58563 = VERTEX_POINT ( 'NONE', #15996 ) ;
#58564 = CIRCLE ( 'NONE', #40540, 31.99999999999999289 ) ;
#58565 = ORIENTED_EDGE ( 'NONE', *, *, #16114, .T. ) ;
#58566 = PLANE ( 'NONE',  #18639 ) ;
#58567 = AXIS2_PLACEMENT_3D ( 'NONE', #24998, #41928, #14077 ) ;
#58569 = EDGE_CURVE ( 'NONE', #19761, #11722, #1884, .T. ) ;
#58568 = CARTESIAN_POINT ( 'NONE',  ( 0.000000000000000000, -30.84782396557233142, 21.32104025579104345 ) ) ;
#58570 = CARTESIAN_POINT ( 'NONE',  ( 94.99999999999998579, 87.33691857156068750, 80.27656250086714351 ) ) ;
#58571 = AXIS2_PLACEMENT_3D ( 'NONE', #9110, #8378, #55343 ) ;
#58572 = CARTESIAN_POINT ( 'NONE',  ( 6.938893903907228378E-15, 1.932465207890948911E-15, 15.77977592589476608 ) ) ;
#58573 = LINE ( 'NONE', #1845, #2586 ) ;
#58574 = CARTESIAN_POINT ( 'NONE',  ( -14.87942725330654348, -141.9795960975983178, -5.500000000000000000 ) ) ;
#58575 = CARTESIAN_POINT ( 'NONE',  ( -31.74999999999995737, 0.000000000000000000, 0.000000000000000000 ) ) ;
#58576 = ADVANCED_FACE ( 'NONE', ( #9623 ), #44956, .T. ) ;
#58577 = DIRECTION ( 'NONE',  ( 0.000000000000000000, 0.000000000000000000, 1.000000000000000000 ) ) ;
#58578 = DIRECTION ( 'NONE',  ( 1.000000000000000000, -0.000000000000000000, -0.000000000000000000 ) ) ;
#58579 = DIRECTION ( 'NONE',  ( -0.000000000000000000, -0.000000000000000000, 1.000000000000000000 ) ) ;
#58580 = CARTESIAN_POINT ( 'NONE',  ( 95.00000000000000000, -206.9400435732949575, 85.47562500173430067 ) ) ;
#58581 = CARTESIAN_POINT ( 'NONE',  ( -19.90058851926621131, -132.5883508287165853, 5.500000000000000000 ) ) ;
#58582 = CARTESIAN_POINT ( 'NONE',  ( -96.15314808468752972, 91.99731107132950569, 85.09197916753380753 ) ) ;
#58583 = EDGE_CURVE ( 'NONE', #58994, #29135, #5115, .T. ) ;
#58584 = EDGE_CURVE ( 'NONE', #54986, #11705, #4000, .T. ) ;
#58585 = CARTESIAN_POINT ( 'NONE',  ( -92.35000000018069954, 89.99996905681452120, 78.33187387208522523 ) ) ;
#58586 = VECTOR ( 'NONE', #34111, 1000.000000000000000 ) ;
#58587 = AXIS2_PLACEMENT_3D ( 'NONE', #51763, #311, #62356 ) ;
#58588 = CIRCLE ( 'NONE', #1005, 32.00000000000000711 ) ;
#58589 = VECTOR ( 'NONE', #63689, 1000.000000000000000 ) ;
#58590 = DIRECTION ( 'NONE',  ( -1.000000000000000000, 0.000000000000000000, -0.000000000000000000 ) ) ;
#58591 = ORIENTED_EDGE ( 'NONE', *, *, #66488, .T. ) ;
#58592 = MECHANICAL_DESIGN_GEOMETRIC_PRESENTATION_REPRESENTATION (  '', ( #32177 ), #69428 ) ;
#58593 = CARTESIAN_POINT ( 'NONE',  ( -8.637688417678527131, 13.69818742750669394, 42.00000000000001421 ) ) ;
#58594 = DIRECTION ( 'NONE',  ( -1.000000000000000000, 0.000000000000000000, -0.000000000000000000 ) ) ;
#58595 = CARTESIAN_POINT ( 'NONE',  ( 0.000000000000000000, 40.98264845739749518, 9.188173127307448951 ) ) ;
#58596 = CARTESIAN_POINT ( 'NONE',  ( -3.000000000000000000, 20.85821328998741109, 10.92862929874522315 ) ) ;
#58597 = CARTESIAN_POINT ( 'NONE',  ( 97.30629616937498838, -208.6684592857803011, 81.28197916753381946 ) ) ;
#58598 = ORIENTED_EDGE ( 'NONE', *, *, #331, .T. ) ;
#58599 = ORIENTED_EDGE ( 'NONE', *, *, #70861, .F. ) ;
#58600 = FACE_OUTER_BOUND ( 'NONE', #40396, .T. ) ;
#58601 = ORIENTED_EDGE ( 'NONE', *, *, #4932, .F. ) ;
#58602 = CARTESIAN_POINT ( 'NONE',  ( 4.999999999999999112, -41.81611651403859042, -3.925862922256606602 ) ) ;
#58603 = CARTESIAN_POINT ( 'NONE',  ( 92.69370383062501162, -208.6684592857803295, 75.61989583420047722 ) ) ;
#58604 = VECTOR ( 'NONE', #67130, 1000.000000000000000 ) ;
#58605 = VERTEX_POINT ( 'NONE', #34031 ) ;
#58606 = CARTESIAN_POINT ( 'NONE',  ( 92.69370383062501162, -208.6684592857803011, 80.22364583420048234 ) ) ;
#58607 = CIRCLE ( 'NONE', #44184, 31.99999999999998934 ) ;
#58608 = CIRCLE ( 'NONE', #14175, 31.99999999999999289 ) ;
#58609 = ORIENTED_EDGE ( 'NONE', *, *, #18248, .T. ) ;
#58610 = DIRECTION ( 'NONE',  ( 0.000000000000000000, 0.000000000000000000, 1.000000000000000000 ) ) ;
#58611 = VERTEX_POINT ( 'NONE', #28013 ) ;
#58612 = VERTEX_POINT ( 'NONE', #56979 ) ;
#58613 = CARTESIAN_POINT ( 'NONE',  ( 15.00000000000000000, -0.9646360437375368635, -23.52805723605589705 ) ) ;
#58614 = VECTOR ( 'NONE', #14736, 1000.000000000000000 ) ;
#58615 = DIRECTION ( 'NONE',  ( -1.000000000000000000, 0.000000000000000000, 0.000000000000000000 ) ) ;
#58616 = CIRCLE ( 'NONE', #55024, 31.99999999999999645 ) ;
#58617 = VERTEX_POINT ( 'NONE', #39314 ) ;
#58618 = CARTESIAN_POINT ( 'NONE',  ( -95.00000000000002842, 93.05995642670504253, 84.12624999999999886 ) ) ;
#58619 = CARTESIAN_POINT ( 'NONE',  ( 95.00000000000000000, -213.0599564267049857, 83.88812500173429498 ) ) ;
#58620 = CARTESIAN_POINT ( 'NONE',  ( 93.67499999999998295, 92.29496732002878900, 89.89416666666666345 ) ) ;
#58621 = EDGE_LOOP ( 'NONE', ( #6472, #33296, #41280, #65003 ) ) ;
#58622 = CARTESIAN_POINT ( 'NONE',  ( 97.64999999999999147, 89.99999988321010846, 84.68187499741277691 ) ) ;
#58623 = CARTESIAN_POINT ( 'NONE',  ( 0.000000000000000000, 0.000000000000000000, 42.00000000000001421 ) ) ;
#58624 = ORIENTED_EDGE ( 'NONE', *, *, #4695, .T. ) ;
#58625 = ORIENTED_EDGE ( 'NONE', *, *, #17800, .F. ) ;
#58626 = CARTESIAN_POINT ( 'NONE',  ( 10.00000000000000000, 0.6853352020790449695, 37.58145647212454321 ) ) ;
#58627 = ORIENTED_EDGE ( 'NONE', *, *, #73044, .T. ) ;
#58628 = CARTESIAN_POINT ( 'NONE',  ( 96.32499999999997442, 92.29496732002878900, 87.32770833506762642 ) ) ;
#58629 = CIRCLE ( 'NONE', #23860, 77.49900000000000944 ) ;
#58630 = ADVANCED_FACE ( 'NONE', ( #49831 ), #26901, .T. ) ;
#58631 = ORIENTED_EDGE ( 'NONE', *, *, #62785, .T. ) ;
#58632 = ORIENTED_EDGE ( 'NONE', *, *, #52049, .T. ) ;
#58633 = CARTESIAN_POINT ( 'NONE',  ( -96.32499999999996021, -212.2949673200287179, 78.12020833506763040 ) ) ;
#58634 = CARTESIAN_POINT ( 'NONE',  ( 10.00000000000000000, -78.73519480814971416, 22.90783923731600069 ) ) ;
#58635 = ORIENTED_EDGE ( 'NONE', *, *, #38792, .F. ) ;
#58636 = AXIS2_PLACEMENT_3D ( 'NONE', #20709, #3447, #61317 ) ;
#58637 = ORIENTED_EDGE ( 'NONE', *, *, #42465, .F. ) ;
#58638 = EDGE_CURVE ( 'NONE', #68126, #46710, #73503, .T. ) ;
#58639 = AXIS2_PLACEMENT_3D ( 'NONE', #60052, #31811, #32555 ) ;
#58640 = ORIENTED_EDGE ( 'NONE', *, *, #10185, .T. ) ;
#58641 = DIRECTION ( 'NONE',  ( 0.000000000000000000, -0.000000000000000000, -1.000000000000000000 ) ) ;
#58642 = CARTESIAN_POINT ( 'NONE',  ( 10.00000000000000000, -27.13269053701078448, -25.88420570971428702 ) ) ;
#58643 = CIRCLE ( 'NONE', #37021, 31.99999999999999645 ) ;
#58644 = AXIS2_PLACEMENT_3D ( 'NONE', #68860, #68109, #5344 ) ;
#58645 = EDGE_CURVE ( 'NONE', #60587, #30754, #39095, .T. ) ;
#58646 = CARTESIAN_POINT ( 'NONE',  ( -95.00000000000002842, 86.94004357329504273, 87.61875000000000568 ) ) ;
#58647 = ORIENTED_EDGE ( 'NONE', *, *, #35787, .F. ) ;
#58648 = DIRECTION ( 'NONE',  ( 0.000000000000000000, 0.000000000000000000, 1.000000000000000000 ) ) ;
#58649 = STYLED_ITEM ( 'NONE', ( #38722 ), #36889 ) ;
#58650 = LINE ( 'NONE', #30070, #29852 ) ;
#58651 = ORIENTED_EDGE ( 'NONE', *, *, #44669, .F. ) ;
#58652 = DIRECTION ( 'NONE',  ( 0.000000000000000000, 0.3090169943749450088, 0.9510565162951544194 ) ) ;
#58653 = CARTESIAN_POINT ( 'NONE',  ( -92.69370383062498320, -209.9999999999999716, 82.97531250086714749 ) ) ;
#58655 = ORIENTED_EDGE ( 'NONE', *, *, #53060, .F. ) ;
#58654 = EDGE_CURVE ( 'NONE', #73858, #15718, #74250, .T. ) ;
#58656 = DIRECTION ( 'NONE',  ( -1.000000000000000000, -0.000000000000000000, 0.000000000000000000 ) ) ;
#58657 = LINE ( 'NONE', #40258, #23570 ) ;
#58658 = DIRECTION ( 'NONE',  ( 0.000000000000000000, 0.000000000000000000, -1.000000000000000000 ) ) ;
#58659 = DIRECTION ( 'NONE',  ( 0.000000000000000000, -0.9781476007338041345, 0.2079116908177663092 ) ) ;
#58660 = DIRECTION ( 'NONE',  ( -1.000000000000000000, -0.000000000000000000, 0.000000000000000000 ) ) ;
#58661 = CARTESIAN_POINT ( 'NONE',  ( 10.00000000000000000, -37.58145647212455032, 0.6853352020789044152 ) ) ;
#58662 = CARTESIAN_POINT ( 'NONE',  ( 6.000000000000000000, -81.96053171279903893, 2.543863470248107994 ) ) ;
#58663 = DIRECTION ( 'NONE',  ( -1.000000000000000000, -0.000000000000000000, -0.000000000000000000 ) ) ;
#58664 = EDGE_CURVE ( 'NONE', #19127, #1038, #51315, .T. ) ;
#58665 = CARTESIAN_POINT ( 'NONE',  ( 93.67499999999999716, 87.70503267997126784, 88.20083333333332121 ) ) ;
#58666 = EDGE_CURVE ( 'NONE', #73333, #69147, #58306, .T. ) ;
#58667 = CARTESIAN_POINT ( 'NONE',  ( -93.84685191531254134, 91.99731107132950569, 79.27114583420046756 ) ) ;
#58668 = CARTESIAN_POINT ( 'NONE',  ( 0.000000000000000000, 0.000000000000000000, -125.0000000000000000 ) ) ;
#58669 = LINE ( 'NONE', #63219, #9835 ) ;
#58670 =( BOUNDED_CURVE ( )  B_SPLINE_CURVE ( 2, ( #31931, #37225, #54870, #49958, #42491, #43248, #13893 ),
 .UNSPECIFIED., .F., .F. ) 
 B_SPLINE_CURVE_WITH_KNOTS ( ( 3, 2, 2, 3 ),
 ( 0.2708333333333337034, 0.2777777777777781232, 0.2847222222222224874, 0.2916666666666669072 ),
 .UNSPECIFIED. ) 
 CURVE ( )  GEOMETRIC_REPRESENTATION_ITEM ( )  RATIONAL_B_SPLINE_CURVE ( ( 0.9999999999999924505, 0.8660254037844462571, 1.000000000000000000, 0.8660254037844387076, 1.000000000000000000, 0.8660254037844343777, 1.000000000000004219 ) ) 
 REPRESENTATION_ITEM ( '' )  );
#58671 = VECTOR ( 'NONE', #28382, 1000.000000000000114 ) ;
#58672 = CARTESIAN_POINT ( 'NONE',  ( 10.00000000000000000, -12.26510123303234501, -35.53030884539098366 ) ) ;
#58673 = AXIS2_PLACEMENT_3D ( 'NONE', #71510, #43351, #37698 ) ;
#58674 = AXIS2_PLACEMENT_3D ( 'NONE', #12073, #28615, #7180 ) ;
#58675 = CARTESIAN_POINT ( 'NONE',  ( 6.719258119307966126, -15.35072898742050462, -1.199999999999999956 ) ) ;
#58676 = DIRECTION ( 'NONE',  ( -0.9730327541852497042, 0.2306669878475622604, 0.000000000000000000 ) ) ;
#58677 = EDGE_CURVE ( 'NONE', #42699, #24045, #10326, .T. ) ;
#58678 = EDGE_CURVE ( 'NONE', #40792, #5889, #6684, .T. ) ;
#58680 = CIRCLE ( 'NONE', #26244, 82.00000000000000000 ) ;
#58679 = CARTESIAN_POINT ( 'NONE',  ( 0.000000000000000000, -17.28742895386031719, -75.54627589209962935 ) ) ;
#58681 = FACE_OUTER_BOUND ( 'NONE', #62371, .T. ) ;
#58682 = CARTESIAN_POINT ( 'NONE',  ( -3.000000000000000000, -3.948201729842038432, -23.21447184625298021 ) ) ;
#58683 = CARTESIAN_POINT ( 'NONE',  ( -92.69370383062498320, -208.6684592857803011, 76.83697916753382628 ) ) ;
#58684 = AXIS2_PLACEMENT_3D ( 'NONE', #49250, #9029, #60907 ) ;
#58685 = CARTESIAN_POINT ( 'NONE',  ( 5.000000000000000000, -0.4878135028931873673, -6.000000000000001776 ) ) ;
#58686 = VERTEX_POINT ( 'NONE', #22012 ) ;
#58687 = CARTESIAN_POINT ( 'NONE',  ( 10.00000000000000000, 0.000000000000000000, 0.000000000000000000 ) ) ;
#58688 = CARTESIAN_POINT ( 'NONE',  ( 2.861260715122138586E-12, -120.0000000000000000, -75.00000000000000000 ) ) ;
#58690 = CARTESIAN_POINT ( 'NONE',  ( 10.00000000000000000, 0.000000000000000000, 0.000000000000000000 ) ) ;
#58689 = VECTOR ( 'NONE', #18519, 1000.000000000000000 ) ;
#58691 = CARTESIAN_POINT ( 'NONE',  ( 2.184357737007946383E-12, -120.0000000000000000, -48.99999999999997158 ) ) ;
#58692 = CIRCLE ( 'NONE', #23866, 16.00000000000000000 ) ;
#58694 = CARTESIAN_POINT ( 'NONE',  ( 10.00000000000000178, 0.000000000000000000, 0.000000000000000000 ) ) ;
#58693 = AXIS2_PLACEMENT_3D ( 'NONE', #48166, #71075, #42904 ) ;
#58695 = ORIENTED_EDGE ( 'NONE', *, *, #50351, .F. ) ;
#58696 = AXIS2_PLACEMENT_3D ( 'NONE', #55722, #32035, #31674 ) ;
#58697 = CARTESIAN_POINT ( 'NONE',  ( 92.34999999999999432, 90.00000000000002842, 86.18999999999999773 ) ) ;
#58698 = DIRECTION ( 'NONE',  ( 0.000000000000000000, 0.000000000000000000, 1.000000000000000000 ) ) ;
#58699 = ORIENTED_EDGE ( 'NONE', *, *, #52550, .T. ) ;
#58700 = AXIS2_PLACEMENT_3D ( 'NONE', #15972, #43085, #55081 ) ;
#58701 = CARTESIAN_POINT ( 'NONE',  ( 97.30629616937498838, -209.9999999999999716, 84.24531250086714351 ) ) ;
#58702 = CARTESIAN_POINT ( 'NONE',  ( 92.69370383062501162, -209.9999999999999716, 87.26156250086715715 ) ) ;
#58703 = ORIENTED_EDGE ( 'NONE', *, *, #19180, .F. ) ;
#58704 = CARTESIAN_POINT ( 'NONE',  ( 96.15314808468748708, -208.0026889286704943, 88.31989583420048007 ) ) ;
#58705 = VERTEX_POINT ( 'NONE', #16753 ) ;
#58706 = CARTESIAN_POINT ( 'NONE',  ( 10.00000000000000000, 0.000000000000000000, 0.000000000000000000 ) ) ;
#58707 = ORIENTED_EDGE ( 'NONE', *, *, #72738, .T. ) ;
#58708 = CARTESIAN_POINT ( 'NONE',  ( -95.00000000000002842, 92.66308142843932671, 81.38781250086715602 ) ) ;
#58709 = EDGE_LOOP ( 'NONE', ( #35270, #8591, #20316, #70470, #7268, #35511 ) ) ;
#58710 = EDGE_LOOP ( 'NONE', ( #4636, #29132, #5925, #42088 ) ) ;
#58711 = DIRECTION ( 'NONE',  ( -0.4796670183876294291, 0.8774505977381983346, 0.000000000000000000 ) ) ;
#58712 = EDGE_CURVE ( 'NONE', #18161, #21517, #61132, .T. ) ;
#58713 = ORIENTED_EDGE ( 'NONE', *, *, #55919, .T. ) ;
#58714 = CARTESIAN_POINT ( 'NONE',  ( 97.65000000002652314, 90.00000000000005684, -75.00000000000007105 ) ) ;
#58715 = CYLINDRICAL_SURFACE ( 'NONE', #34415, 31.99999999999998579 ) ;
#58716 = EDGE_CURVE ( 'NONE', #44099, #45217, #23532, .T. ) ;
#58717 = AXIS2_PLACEMENT_3D ( 'NONE', #34319, #28674, #67423 ) ;
#58718 = ORIENTED_EDGE ( 'NONE', *, *, #14188, .T. ) ;
#58719 = DIRECTION ( 'NONE',  ( 0.000000000000000000, 0.000000000000000000, 1.000000000000000000 ) ) ;
#58720 = EDGE_CURVE ( 'NONE', #64725, #1126, #50078, .T. ) ;
#58721 = ORIENTED_EDGE ( 'NONE', *, *, #68445, .T. ) ;
#58722 = CARTESIAN_POINT ( 'NONE',  ( 5.000000000000000000, -16.65560815589439159, 38.55633173627004595 ) ) ;
#58723 = AXIS2_PLACEMENT_3D ( 'NONE', #54280, #47889, #2807 ) ;
#58724 = ORIENTED_EDGE ( 'NONE', *, *, #31062, .T. ) ;
#58725 = CIRCLE ( 'NONE', #32242, 15.69999999999999929 ) ;
#58726 = EDGE_CURVE ( 'NONE', #47064, #11565, #11502, .T. ) ;
#58727 = AXIS2_PLACEMENT_3D ( 'NONE', #24344, #7044, #70183 ) ;
#58728 = EDGE_LOOP ( 'NONE', ( #57411, #4203, #18972, #59919 ) ) ;
#58729 = ORIENTED_EDGE ( 'NONE', *, *, #6285, .F. ) ;
#58730 = CARTESIAN_POINT ( 'NONE',  ( 95.00000000000000000, -207.3369185715606307, 81.22906250086715829 ) ) ;
#58731 = CARTESIAN_POINT ( 'NONE',  ( 10.00000000000000000, 17.67226234102826510, 33.17418723428314564 ) ) ;
#58732 = APPLICATION_PROTOCOL_DEFINITION ( 'draft international standard', 'automotive_design', 1998, #66202 ) ;
#58733 = CARTESIAN_POINT ( 'NONE',  ( 0.000000000000000000, 0.000000000000000000, 0.000000000000000000 ) ) ;
#58734 = AXIS2_PLACEMENT_3D ( 'NONE', #24373, #7452, #29619 ) ;
#58735 = DIRECTION ( 'NONE',  ( -0.8571673007021122226, 1.049727191138618572E-16, 0.5150380749100542666 ) ) ;
#58736 = CARTESIAN_POINT ( 'NONE',  ( 96.32499999999998863, -207.7050326799711968, 78.99333333333332519 ) ) ;
#58737 = ADVANCED_FACE ( 'NONE', ( #34778 ), #46428, .T. ) ;
#58738 = CIRCLE ( 'NONE', #14293, 77.49900000000002365 ) ;
#58739 = CARTESIAN_POINT ( 'NONE',  ( 0.000000000000000000, 0.000000000000000000, 0.000000000000000000 ) ) ;
#58740 = CARTESIAN_POINT ( 'NONE',  ( 0.000000000000000000, 36.88895765772633695, 6.736453364083687667 ) ) ;
#58741 = DIRECTION ( 'NONE',  ( 1.000000000000000000, 0.000000000000000000, 0.000000000000000000 ) ) ;
#58742 = CARTESIAN_POINT ( 'NONE',  ( -96.15314808468747287, -208.0026889286704943, 84.45697916753380241 ) ) ;
#58743 = CARTESIAN_POINT ( 'NONE',  ( -97.30629616937501680, 88.66845928578038638, 82.23447916753383424 ) ) ;
#58744 = ORIENTED_EDGE ( 'NONE', *, *, #13557, .F. ) ;
#58745 = CARTESIAN_POINT ( 'NONE',  ( 96.15314808468748708, 88.00268892867053694, 79.69447916753379957 ) ) ;
#58746 = ORIENTED_EDGE ( 'NONE', *, *, #70578, .F. ) ;
#58747 = CARTESIAN_POINT ( 'NONE',  ( 95.00000000000000000, -209.9999999999999716, 90.00000000000000000 ) ) ;
#58748 = DIRECTION ( 'NONE',  ( 0.000000000000000000, 0.5000000000000028866, 0.8660254037844369313 ) ) ;
#58749 = EDGE_CURVE ( 'NONE', #21235, #2959, #47171, .T. ) ;
#58750 = DIRECTION ( 'NONE',  ( -1.000000000000000000, -0.000000000000000000, -0.000000000000000000 ) ) ;
#58751 = LINE ( 'NONE', #24172, #36718 ) ;
#58752 = DIRECTION ( 'NONE',  ( 0.000000000000000000, 0.8910065241883656784, 0.4539904997395510788 ) ) ;
#58753 = AXIS2_PLACEMENT_3D ( 'NONE', #8730, #26009, #66612 ) ;
#58754 = CARTESIAN_POINT ( 'NONE',  ( -92.69370383062498320, -209.9999999999999716, 84.88031250086713442 ) ) ;
#58755 = DIRECTION ( 'NONE',  ( -1.000000000000000000, -0.000000000000000000, 0.000000000000000000 ) ) ;
#58756 = CARTESIAN_POINT ( 'NONE',  ( 0.000000000000000000, -31.52238457039579345, -27.75498641678775158 ) ) ;
#58757 = DIRECTION ( 'NONE',  ( 0.000000000000000000, 0.7604059656000322631, -0.6494480483301821039 ) ) ;
#58758 = FACE_OUTER_BOUND ( 'NONE', #65207, .T. ) ;
#58759 = EDGE_LOOP ( 'NONE', ( #27836, #16496, #50990, #70348 ) ) ;
#58760 = AXIS2_PLACEMENT_3D ( 'NONE', #2704, #25584, #7566 ) ;
#58761 = VECTOR ( 'NONE', #7047, 1000.000000000000000 ) ;
#58762 = ORIENTED_EDGE ( 'NONE', *, *, #39675, .F. ) ;
#58763 = AXIS2_PLACEMENT_3D ( 'NONE', #54452, #65377, #25147 ) ;
#58764 = CARTESIAN_POINT ( 'NONE',  ( 12.00000000000000000, -3.948201729842032215, 23.21447184625297666 ) ) ;
#58765 = EDGE_CURVE ( 'NONE', #21866, #45116, #37151, .T. ) ;
#58766 = DIRECTION ( 'NONE',  ( 0.000000000000000000, 0.000000000000000000, 1.000000000000000000 ) ) ;
#58767 = EDGE_CURVE ( 'NONE', #67688, #8512, #51110, .T. ) ;
#58768 = LINE ( 'NONE', #22048, #12885 ) ;
#58769 = DIRECTION ( 'NONE',  ( 1.000000000000000000, 0.000000000000000000, 0.000000000000000000 ) ) ;
#58770 = CARTESIAN_POINT ( 'NONE',  ( 0.000000000000000000, 23.50000000000000000, -1.500000000000001332 ) ) ;
#58771 = DIRECTION ( 'NONE',  ( -1.000000000000000000, 0.000000000000000000, 0.000000000000000000 ) ) ;
#58772 = CARTESIAN_POINT ( 'NONE',  ( 0.000000000000000000, 72.35160999960817207, 20.41045688087850607 ) ) ;
#58773 = ORIENTED_EDGE ( 'NONE', *, *, #31579, .F. ) ;
#58774 = DIRECTION ( 'NONE',  ( 1.000000000000000000, 0.000000000000000000, 0.000000000000000000 ) ) ;
#58775 = LINE ( 'NONE', #30186, #52575 ) ;
#58776 = DIRECTION ( 'NONE',  ( -1.000000000000000000, -0.000000000000000000, 0.000000000000000000 ) ) ;
#58777 = FACE_OUTER_BOUND ( 'NONE', #72924, .T. ) ;
#58778 = DIRECTION ( 'NONE',  ( 0.000000000000000000, 0.000000000000000000, 1.000000000000000000 ) ) ;
#58779 = CARTESIAN_POINT ( 'NONE',  ( -93.84685191531247028, -211.9973110713294489, 85.56822916753381492 ) ) ;
#58780 = DIRECTION ( 'NONE',  ( -1.000000000000000000, 0.000000000000000000, -0.000000000000000000 ) ) ;
#58781 = VECTOR ( 'NONE', #69562, 1000.000000000000114 ) ;
#58782 = LINE ( 'NONE', #54258, #2228 ) ;
#58783 = AXIS2_PLACEMENT_3D ( 'NONE', #49155, #31856, #20591 ) ;
#58784 = CARTESIAN_POINT ( 'NONE',  ( -92.69370383062498320, -209.9999999999999716, 74.87906250086714977 ) ) ;
#58785 = DIRECTION ( 'NONE',  ( -1.000000000000000000, -0.000000000000000000, 0.000000000000000000 ) ) ;
#58786 = ORIENTED_EDGE ( 'NONE', *, *, #21613, .T. ) ;
#58787 = DIRECTION ( 'NONE',  ( -1.000000000000000000, 0.000000000000000000, 0.000000000000000000 ) ) ;
#58788 = DIRECTION ( 'NONE',  ( -1.000000000000000000, -0.000000000000000000, -0.000000000000000000 ) ) ;
#58789 = VECTOR ( 'NONE', #59123, 1000.000000000000000 ) ;
#58790 = CARTESIAN_POINT ( 'NONE',  ( 94.99999999999998579, 93.05995642670504253, 85.47562500173430067 ) ) ;
#58791 = CIRCLE ( 'NONE', #25, 42.00000000000000000 ) ;
#58792 = CARTESIAN_POINT ( 'NONE',  ( -96.15314808468751551, 88.00268892867056536, 76.57239583420049200 ) ) ;
#58793 = CARTESIAN_POINT ( 'NONE',  ( 92.69370383062501162, -208.6684592857803011, 75.61989583420047722 ) ) ;
#58794 = ORIENTED_EDGE ( 'NONE', *, *, #43975, .F. ) ;
#58795 = EDGE_CURVE ( 'NONE', #29381, #66094, #44838, .T. ) ;
#58796 = DIRECTION ( 'NONE',  ( 0.000000000000000000, 0.000000000000000000, 1.000000000000000000 ) ) ;
#58797 = VERTEX_POINT ( 'NONE', #52061 ) ;
#58798 = CARTESIAN_POINT ( 'NONE',  ( 11.99999999999999822, 75.16055320797057959, -18.89407956138179046 ) ) ;
#58799 = ORIENTED_EDGE ( 'NONE', *, *, #36083, .F. ) ;
#58800 = CARTESIAN_POINT ( 'NONE',  ( 0.000000000000000000, 37.22597642581158084, -5.202137450156524068 ) ) ;
#58801 = VECTOR ( 'NONE', #29128, 1000.000000000000114 ) ;
#58802 = VECTOR ( 'NONE', #63383, 1000.000000000000000 ) ;
#58803 = VERTEX_POINT ( 'NONE', #69352 ) ;
#58804 = ORIENTED_EDGE ( 'NONE', *, *, #64101, .F. ) ;
#58805 = EDGE_CURVE ( 'NONE', #34202, #4754, #42696, .T. ) ;
#58806 = AXIS2_PLACEMENT_3D ( 'NONE', #15155, #55384, #49368 ) ;
#58807 = ORIENTED_EDGE ( 'NONE', *, *, #61781, .F. ) ;
#58808 = CIRCLE ( 'NONE', #15606, 42.00000000000000000 ) ;
#58809 = CARTESIAN_POINT ( 'NONE',  ( 11.99999999999999822, -69.42325613327466272, 34.44570377933573724 ) ) ;
#58810 = EDGE_CURVE ( 'NONE', #30842, #43302, #57338, .T. ) ;
#58811 = ORIENTED_EDGE ( 'NONE', *, *, #10287, .F. ) ;
#58812 = VERTEX_POINT ( 'NONE', #35873 ) ;
#58813 = CARTESIAN_POINT ( 'NONE',  ( 94.99999999999998579, 87.33691857156068750, 78.53031250086715431 ) ) ;
#58814 = CARTESIAN_POINT ( 'NONE',  ( 0.000000000000000000, -66.50666863321971789, -39.78640506895676054 ) ) ;
#58815 = CARTESIAN_POINT ( 'NONE',  ( 23.41451323550360186, -132.5004227906269989, 5.500000000000000000 ) ) ;
#58816 = VERTEX_POINT ( 'NONE', #58824 ) ;
#58817 = EDGE_CURVE ( 'NONE', #2983, #23472, #27105, .T. ) ;
#58818 = ORIENTED_EDGE ( 'NONE', *, *, #71785, .T. ) ;
#58819 = EDGE_CURVE ( 'NONE', #4632, #61610, #46339, .T. ) ;
#58820 = ORIENTED_EDGE ( 'NONE', *, *, #69495, .T. ) ;
#58821 = CARTESIAN_POINT ( 'NONE',  ( 0.000000000000000000, 46.21855187248719687, -62.20884554313968806 ) ) ;
#58822 = ORIENTED_EDGE ( 'NONE', *, *, #31050, .T. ) ;
#58823 = CARTESIAN_POINT ( 'NONE',  ( 0.000000000000000000, 0.000000000000000000, 0.000000000000000000 ) ) ;
#58824 = CARTESIAN_POINT ( 'NONE',  ( 0.000000000000000000, -58.39081064771713869, -50.95692526931392052 ) ) ;
#58825 = CARTESIAN_POINT ( 'NONE',  ( 10.00000000000000000, -55.16347631942997509, -60.67117009219195722 ) ) ;
#58826 = DIRECTION ( 'NONE',  ( -1.000000000000000000, 0.000000000000000000, 0.000000000000000000 ) ) ;
#58827 = DIRECTION ( 'NONE',  ( -1.000000000000000000, 0.000000000000000000, 0.000000000000000000 ) ) ;
#58828 = DIRECTION ( 'NONE',  ( 0.000000000000000000, 0.000000000000000000, 1.000000000000000000 ) ) ;
#58829 = DIRECTION ( 'NONE',  ( -1.000000000000000000, 0.000000000000000000, 0.000000000000000000 ) ) ;
#58830 = CARTESIAN_POINT ( 'NONE',  ( -94.99999999999997158, -213.0599564267049857, 80.71312500173431204 ) ) ;
#58831 = LINE ( 'NONE', #7330, #6278 ) ;
#58832 = EDGE_LOOP ( 'NONE', ( #15313, #55209, #8331, #1832 ) ) ;
#58834 = CARTESIAN_POINT ( 'NONE',  ( -93.67500000000003979, 87.70503267997129626, 76.32104166840096582 ) ) ;
#58833 = CARTESIAN_POINT ( 'NONE',  ( 92.34999999999999432, 91.52997821335252127, 76.05645833506761733 ) ) ;
#58835 = VECTOR ( 'NONE', #15171, 1000.000000000000000 ) ;
#58836 = ORIENTED_EDGE ( 'NONE', *, *, #4241, .F. ) ;
#58837 = CARTESIAN_POINT ( 'NONE',  ( 96.15314808468748708, 91.99731107132950569, 81.33489583420049485 ) ) ;
#58838 = EDGE_CURVE ( 'NONE', #24230, #64851, #21096, .T. ) ;
#58839 = CARTESIAN_POINT ( 'NONE',  ( 10.00000000000000000, -35.53030884539094103, 12.26510123303246935 ) ) ;
#58840 = LINE ( 'NONE', #18965, #36668 ) ;
#58841 = CARTESIAN_POINT ( 'NONE',  ( 5.000000000000000000, 50.23322058963348979, 64.81221759200361987 ) ) ;
#58842 = FACE_OUTER_BOUND ( 'NONE', #49202, .T. ) ;
#58843 = DIRECTION ( 'NONE',  ( 0.000000000000000000, 0.4999999999999931166, -0.8660254037844427044 ) ) ;
#58844 = AXIS2_PLACEMENT_3D ( 'NONE', #11413, #26850, #62189 ) ;
#58845 = ADVANCED_BREP_SHAPE_REPRESENTATION ( '', ( #37031, #43395 ), #46970 ) ;
#58846 = ORIENTED_EDGE ( 'NONE', *, *, #48443, .T. ) ;
#58847 = FACE_OUTER_BOUND ( 'NONE', #3707, .T. ) ;
#58848 = CYLINDRICAL_SURFACE ( 'NONE', #55198, 82.00000000000000000 ) ;
#58849 = ORIENTED_EDGE ( 'NONE', *, *, #42612, .F. ) ;
#58850 = ORIENTED_EDGE ( 'NONE', *, *, #5445, .F. ) ;
#58851 = CIRCLE ( 'NONE', #20415, 31.99999999999998934 ) ;
#58852 = EDGE_CURVE ( 'NONE', #14528, #37162, #30708, .T. ) ;
#58853 = CARTESIAN_POINT ( 'NONE',  ( 10.00000000000000000, 65.58780272294076497, 36.73666225445916211 ) ) ;
#58854 = DIRECTION ( 'NONE',  ( -1.000000000000000000, 0.000000000000000000, -0.000000000000000000 ) ) ;
#58855 = CARTESIAN_POINT ( 'NONE',  ( 97.64999999999999147, -209.9999999999999716, 90.00000000000000000 ) ) ;
#58856 = DIRECTION ( 'NONE',  ( -1.000000000000000000, -0.000000000000000000, 0.000000000000000000 ) ) ;
#58857 = CARTESIAN_POINT ( 'NONE',  ( -92.69370383062498320, -208.6684592857803011, 77.47197916753381719 ) ) ;
#58858 = EDGE_CURVE ( 'NONE', #18340, #61621, #39124, .T. ) ;
#58859 = ORIENTED_EDGE ( 'NONE', *, *, #13347, .T. ) ;
#58860 = AXIS2_PLACEMENT_3D ( 'NONE', #27867, #73719, #38785 ) ;
#58861 = LINE ( 'NONE', #26110, #29468 ) ;
#58862 = AXIS2_PLACEMENT_3D ( 'NONE', #49517, #48776, #4052 ) ;
#58863 = VECTOR ( 'NONE', #72316, 1000.000000000000114 ) ;
#58864 = AXIS2_PLACEMENT_3D ( 'NONE', #22321, #38870, #44892 ) ;
#58865 = DIRECTION ( 'NONE',  ( 1.000000000000000000, 0.000000000000000000, 0.000000000000000000 ) ) ;
#58866 = CARTESIAN_POINT ( 'NONE',  ( 11.99999999999999822, 63.97538442413500093, -51.29473840253155714 ) ) ;
#58867 = DIRECTION ( 'NONE',  ( -1.000000000000000000, 0.000000000000000000, 0.000000000000000000 ) ) ;
#58868 = DIRECTION ( 'NONE',  ( 1.000000000000000000, 0.000000000000000000, 0.000000000000000000 ) ) ;
#58869 = CARTESIAN_POINT ( 'NONE',  ( 0.000000000000000000, -35.47612816024506088, -22.48208911017539435 ) ) ;
#58870 = FACE_OUTER_BOUND ( 'NONE', #25897, .T. ) ;
#58871 = AXIS2_PLACEMENT_3D ( 'NONE', #70721, #19227, #48546 ) ;
#58872 = FACE_OUTER_BOUND ( 'NONE', #35764, .T. ) ;
#58873 = CIRCLE ( 'NONE', #21605, 2.375000000000000444 ) ;
#58874 = CARTESIAN_POINT ( 'NONE',  ( -92.34999999999999432, -209.9999999999999716, 76.34749999999999659 ) ) ;
#58875 = PLANE ( 'NONE',  #67031 ) ;
#58876 = CARTESIAN_POINT ( 'NONE',  ( 97.30629616937498838, 90.00000000000002842, 82.49906250086715431 ) ) ;
#58877 = CARTESIAN_POINT ( 'NONE',  ( -97.30629616937497417, -211.3315407142195852, 86.04447916753382231 ) ) ;
#58878 = CARTESIAN_POINT ( 'NONE',  ( 10.00000000000000000, -37.16516213103280108, 4.992566952384862589 ) ) ;
#58879 = ORIENTED_EDGE ( 'NONE', *, *, #7958, .T. ) ;
#58880 = CARTESIAN_POINT ( 'NONE',  ( 0.000000000000000000, -39.04073710021332744, -15.48615015657624028 ) ) ;
#58881 = CARTESIAN_POINT ( 'NONE',  ( -93.67499999999998295, -207.7050326799711968, 82.80333333333332746 ) ) ;
#58882 = CARTESIAN_POINT ( 'NONE',  ( -93.84685191531254134, 91.99731107132950569, 76.73114583420047552 ) ) ;
#58883 = AXIS2_PLACEMENT_3D ( 'NONE', #26593, #65720, #25852 ) ;
#58884 = CARTESIAN_POINT ( 'NONE',  ( 92.69370383062501162, -211.3315407142195852, 87.79072916753381151 ) ) ;
#58885 = ORIENTED_EDGE ( 'NONE', *, *, #1852, .T. ) ;
#58886 = EDGE_CURVE ( 'NONE', #38466, #15320, #12682, .T. ) ;
#58887 = ORIENTED_EDGE ( 'NONE', *, *, #67297, .F. ) ;
#58888 = ORIENTED_EDGE ( 'NONE', *, *, #70742, .F. ) ;
#58889 = VECTOR ( 'NONE', #25296, 1000.000000000000000 ) ;
#58891 = CIRCLE ( 'NONE', #72081, 77.49899999999998101 ) ;
#58890 = FACE_OUTER_BOUND ( 'NONE', #35097, .T. ) ;
#58892 = ADVANCED_FACE ( 'NONE', ( #8794 ), #8434, .T. ) ;
#58893 = LINE ( 'NONE', #5923, #70237 ) ;
#58894 = AXIS2_PLACEMENT_3D ( 'NONE', #25078, #43130, #2568 ) ;
#58895 = ORIENTED_EDGE ( 'NONE', *, *, #66475, .T. ) ;
#58896 = EDGE_CURVE ( 'NONE', #71554, #71724, #18950, .T. ) ;
#58897 = VERTEX_POINT ( 'NONE', #13320 ) ;
#58898 = LINE ( 'NONE', #13752, #30000 ) ;
#58899 = CARTESIAN_POINT ( 'NONE',  ( 92.69370383062501162, -209.9999999999999716, 80.91156250086716284 ) ) ;
#58900 = DIRECTION ( 'NONE',  ( -1.000000000000000000, -0.000000000000000000, 0.000000000000000000 ) ) ;
#58901 = CYLINDRICAL_SURFACE ( 'NONE', #6421, 2.649999999999999467 ) ;
#58902 = DIRECTION ( 'NONE',  ( 0.000000000000000000, 0.000000000000000000, 1.000000000000000000 ) ) ;
#58903 =( BOUNDED_CURVE ( )  B_SPLINE_CURVE ( 2, ( #28140, #69122, #16497, #62382, #10859, #51076, #68389 ),
 .UNSPECIFIED., .F., .F. ) 
 B_SPLINE_CURVE_WITH_KNOTS ( ( 3, 2, 2, 3 ),
 ( 0.8541666666666666297, 0.8611111111111110494, 0.8680555555555554692, 0.8749999999999997780 ),
 .UNSPECIFIED. ) 
 CURVE ( )  GEOMETRIC_REPRESENTATION_ITEM ( )  RATIONAL_B_SPLINE_CURVE ( ( 1.000000000000000000, 0.8660254037844387076, 1.000000000000000000, 0.8660254037844387076, 1.000000000000000000, 0.8660254037844430375, 0.9999999999999956701 ) ) 
 REPRESENTATION_ITEM ( '' )  );
#58904 = CARTESIAN_POINT ( 'NONE',  ( 10.00000000000000000, -37.48860685352290290, -0.8828120875904512665 ) ) ;
#58905 = DIRECTION ( 'NONE',  ( 0.2306669878475647861, 0.9730327541852491491, 0.000000000000000000 ) ) ;
#58906 = CARTESIAN_POINT ( 'NONE',  ( 93.67500000000001137, -212.2949673200287179, 84.39083333333333314 ) ) ;
#58907 = VECTOR ( 'NONE', #68479, 1000.000000000000000 ) ;
#58908 = ORIENTED_EDGE ( 'NONE', *, *, #69370, .T. ) ;
#58909 = ADVANCED_FACE ( 'NONE', ( #42641 ), #25712, .T. ) ;
#58910 = VERTEX_POINT ( 'NONE', #25351 ) ;
#58911 = ORIENTED_EDGE ( 'NONE', *, *, #72797, .F. ) ;
#58912 = ORIENTED_EDGE ( 'NONE', *, *, #6291, .T. ) ;
#58913 = DIRECTION ( 'NONE',  ( 0.000000000000000000, 0.000000000000000000, -1.000000000000000000 ) ) ;
#58914 = AXIS2_PLACEMENT_3D ( 'NONE', #39886, #45153, #35351 ) ;
#58915 =( NAMED_UNIT ( * ) SI_UNIT ( $, .STERADIAN. ) SOLID_ANGLE_UNIT ( ) );
#58916 = CARTESIAN_POINT ( 'NONE',  ( -97.30629616937501680, 90.00000000000004263, 86.62656250086715204 ) ) ;
#58917 = DIRECTION ( 'NONE',  ( 0.000000000000000000, -0.000000000000000000, -1.000000000000000000 ) ) ;
#58918 = AXIS2_PLACEMENT_3D ( 'NONE', #67652, #30923, #65905 ) ;
#58919 = CARTESIAN_POINT ( 'NONE',  ( 50.00005079999999680, 0.000000000000000000, 0.000000000000000000 ) ) ;
#58920 = CARTESIAN_POINT ( 'NONE',  ( 92.69370383062501162, -211.3315407142195852, 88.42572916753380241 ) ) ;
#58921 = CARTESIAN_POINT ( 'NONE',  ( 96.32499999999998863, 87.70503267997126784, 80.05166666666666231 ) ) ;
#58922 = ORIENTED_EDGE ( 'NONE', *, *, #61870, .T. ) ;
#58923 = CARTESIAN_POINT ( 'NONE',  ( -94.99999999999997158, -206.9400435732949575, 88.65062500173431204 ) ) ;
#58924 = VERTEX_POINT ( 'NONE', #26076 ) ;
#58925 = LINE ( 'NONE', #64939, #8625 ) ;
#58926 = EDGE_CURVE ( 'NONE', #5866, #10267, #40324, .T. ) ;
#58927 = ORIENTED_EDGE ( 'NONE', *, *, #5710, .T. ) ;
#58928 = CARTESIAN_POINT ( 'NONE',  ( -96.32500000000001705, 92.29496732002878900, 84.89354166840095672 ) ) ;
#58929 = CARTESIAN_POINT ( 'NONE',  ( 97.30629616937498838, 90.00000000000002842, 76.62531250086713897 ) ) ;
#58930 = EDGE_CURVE ( 'NONE', #12008, #10460, #64839, .T. ) ;
#58931 = ORIENTED_EDGE ( 'NONE', *, *, #73385, .F. ) ;
#58932 = CARTESIAN_POINT ( 'NONE',  ( 11.99999999999999822, 0.000000000000000000, 0.000000000000000000 ) ) ;
#58933 = CARTESIAN_POINT ( 'NONE',  ( 11.99999999999999822, 0.000000000000000000, 0.000000000000000000 ) ) ;
#58934 = DIRECTION ( 'NONE',  ( -1.000000000000000000, 0.000000000000000000, 0.000000000000000000 ) ) ;
#58935 = DIRECTION ( 'NONE',  ( 0.000000000000000000, 0.5000000000000012212, 0.8660254037844379305 ) ) ;
#58936 = ORIENTED_EDGE ( 'NONE', *, *, #28273, .T. ) ;
#58937 = CARTESIAN_POINT ( 'NONE',  ( 10.00000000000000000, 0.000000000000000000, 0.000000000000000000 ) ) ;
#58938 = EDGE_CURVE ( 'NONE', #63634, #21751, #66325, .T. ) ;
#58939 = CARTESIAN_POINT ( 'NONE',  ( -92.69370383062499741, -210.9303163890424173, 74.68334086212730938 ) ) ;
#58940 = ORIENTED_EDGE ( 'NONE', *, *, #23292, .T. ) ;
#58941 = ORIENTED_EDGE ( 'NONE', *, *, #28074, .F. ) ;
#58942 = DIRECTION ( 'NONE',  ( -1.000000000000000000, 0.000000000000000000, 0.000000000000000000 ) ) ;
#58943 = EDGE_CURVE ( 'NONE', #24336, #19951, #63154, .T. ) ;
#58944 = DIRECTION ( 'NONE',  ( -1.000000000000000000, 0.000000000000000000, 0.000000000000000000 ) ) ;
#58945 = LINE ( 'NONE', #53294, #32877 ) ;
#58946 = CARTESIAN_POINT ( 'NONE',  ( -94.99999999999997158, -207.3369185715606307, 87.10281250086715943 ) ) ;
#58947 = ORIENTED_EDGE ( 'NONE', *, *, #53632, .F. ) ;
#58948 = CARTESIAN_POINT ( 'NONE',  ( -93.67499999999998295, -212.2949673200287179, 82.59166666666665435 ) ) ;
#58949 = ORIENTED_EDGE ( 'NONE', *, *, #5397, .F. ) ;
#58950 = VERTEX_POINT ( 'NONE', #59564 ) ;
#58951 = VECTOR ( 'NONE', #38986, 1000.000000000000000 ) ;
#58952 = CIRCLE ( 'NONE', #22942, 82.00000000000000000 ) ;
#58953 = DIRECTION ( 'NONE',  ( 1.000000000000000000, 0.000000000000000000, -0.000000000000000000 ) ) ;
#58954 = VECTOR ( 'NONE', #50895, 1000.000000000000114 ) ;
#58955 = CARTESIAN_POINT ( 'NONE',  ( 92.69370383062498320, 91.33154071421968467, 89.11364583420049712 ) ) ;
#58956 = DIRECTION ( 'NONE',  ( -0.000000000000000000, -0.000000000000000000, 1.000000000000000000 ) ) ;
#58957 = CARTESIAN_POINT ( 'NONE',  ( 97.30629616937498838, 88.66845928578035796, 80.38239583420049428 ) ) ;
#58958 = FACE_OUTER_BOUND ( 'NONE', #9445, .T. ) ;
#58959 = CARTESIAN_POINT ( 'NONE',  ( 0.000000000000000000, -72.35160999960831418, 20.41045688087797672 ) ) ;
#58960 = CARTESIAN_POINT ( 'NONE',  ( 10.00000000000000000, -41.76937507738831812, 62.50329211542423025 ) ) ;
#58961 = CARTESIAN_POINT ( 'NONE',  ( 10.00000000000000000, 36.88895765772633695, 6.736453364083687667 ) ) ;
#58962 = DIRECTION ( 'NONE',  ( -1.000000000000000000, 0.000000000000000000, 0.000000000000000000 ) ) ;
#58963 = FACE_OUTER_BOUND ( 'NONE', #42735, .T. ) ;
#58964 = DIRECTION ( 'NONE',  ( 0.000000000000000000, -0.3090169943749350168, -0.9510565162951576390 ) ) ;
#58965 = LINE ( 'NONE', #30370, #69636 ) ;
#58966 = CIRCLE ( 'NONE', #42121, 37.49900000000000233 ) ;
#58967 = FACE_OUTER_BOUND ( 'NONE', #72542, .T. ) ;
#58968 = CARTESIAN_POINT ( 'NONE',  ( -96.15314808468751551, 88.00268892867056536, 85.30364583420046642 ) ) ;
#58969 = VECTOR ( 'NONE', #69744, 1000.000000000000000 ) ;
#58970 = DIRECTION ( 'NONE',  ( -0.000000000000000000, -0.000000000000000000, 1.000000000000000000 ) ) ;
#58971 = AXIS2_PLACEMENT_3D ( 'NONE', #34895, #57832, #6337 ) ;
#58972 = AXIS2_PLACEMENT_3D ( 'NONE', #12712, #18721, #36757 ) ;
#58973 = DIRECTION ( 'NONE',  ( 0.000000000000000000, 0.000000000000000000, -1.000000000000000000 ) ) ;
#58974 = ORIENTED_EDGE ( 'NONE', *, *, #47359, .T. ) ;
#58975 = CARTESIAN_POINT ( 'NONE',  ( -15.70000000000052687, -119.9999999999998721, -70.59999999999959641 ) ) ;
#58976 = DIRECTION ( 'NONE',  ( 0.000000000000000000, 0.7071067811865487940, -0.7071067811865462405 ) ) ;
#58977 = DIRECTION ( 'NONE',  ( 1.000000000000000000, 0.000000000000000000, 0.000000000000000000 ) ) ;
#58978 = EDGE_CURVE ( 'NONE', #64121, #11255, #54297, .T. ) ;
#58979 = EDGE_CURVE ( 'NONE', #29678, #66220, #71187, .T. ) ;
#58980 = DIRECTION ( 'NONE',  ( 0.000000000000000000, -0.5877852522924779111, -0.8090169943749440096 ) ) ;
#58981 = CARTESIAN_POINT ( 'NONE',  ( 95.00000000000000000, -207.3369185715606307, 83.29281250086717137 ) ) ;
#58982 = EDGE_CURVE ( 'NONE', #15793, #46178, #31881, .T. ) ;
#58983 = ORIENTED_EDGE ( 'NONE', *, *, #39505, .T. ) ;
#58984 = EDGE_CURVE ( 'NONE', #39405, #47714, #14430, .T. ) ;
#58985 = ORIENTED_EDGE ( 'NONE', *, *, #9347, .F. ) ;
#58986 = DIRECTION ( 'NONE',  ( 1.000000000000000000, -7.331661483372147883E-15, -2.592266024478009537E-14 ) ) ;
#58987 = ORIENTED_EDGE ( 'NONE', *, *, #69753, .T. ) ;
#58988 = CARTESIAN_POINT ( 'NONE',  ( -97.64999999999996305, -209.9999999999999716, 88.09499999999999886 ) ) ;
#58989 = ADVANCED_FACE ( 'NONE', ( #19325 ), #71565, .T. ) ;
#58990 = CARTESIAN_POINT ( 'NONE',  ( 97.30629616937498838, -211.3315407142195852, 75.93739583420050110 ) ) ;
#58991 = ORIENTED_EDGE ( 'NONE', *, *, #29050, .F. ) ;
#58992 = CARTESIAN_POINT ( 'NONE',  ( 96.15314808468748708, -208.0026889286704943, 79.42989583420049371 ) ) ;
#58993 = CIRCLE ( 'NONE', #25404, 31.99999999999999645 ) ;
#58994 = VERTEX_POINT ( 'NONE', #7683 ) ;
#58995 = DIRECTION ( 'NONE',  ( -1.000000000000000000, 0.000000000000000000, 0.000000000000000000 ) ) ;
#58996 = EDGE_LOOP ( 'NONE', ( #4187, #60815, #63860, #29112 ) ) ;
#58997 = AXIS2_PLACEMENT_3D ( 'NONE', #28150, #39822, #62772 ) ;
#58998 = ORIENTED_EDGE ( 'NONE', *, *, #23330, .T. ) ;
#58999 = AXIS2_PLACEMENT_3D ( 'NONE', #48942, #30911, #31288 ) ;
#59000 = DIRECTION ( 'NONE',  ( 0.000000000000000000, 0.4539904997395477482, -0.8910065241883673437 ) ) ;
#59001 = ORIENTED_EDGE ( 'NONE', *, *, #41579, .F. ) ;
#59002 = CARTESIAN_POINT ( 'NONE',  ( 10.00000000000000000, 68.67312586195046720, -35.91791733033402068 ) ) ;
#59003 = CARTESIAN_POINT ( 'NONE',  ( 96.32499999999998863, -207.7050326799711968, 82.24770833506762813 ) ) ;
#59004 = CARTESIAN_POINT ( 'NONE',  ( 92.34999999999999432, 90.00000000000002842, 88.09499999999999886 ) ) ;
#59005 = ORIENTED_EDGE ( 'NONE', *, *, #24929, .T. ) ;
#59006 = CARTESIAN_POINT ( 'NONE',  ( 12.00000000000000000, 26.49999999999999645, 1.499999999999995781 ) ) ;
#59007 = AXIS2_PLACEMENT_3D ( 'NONE', #56249, #67153, #73150 ) ;
#59008 = FACE_BOUND ( 'NONE', #35243, .T. ) ;
#59009 = ORIENTED_EDGE ( 'NONE', *, *, #32684, .F. ) ;
#59010 = VERTEX_POINT ( 'NONE', #30599 ) ;
#59011 = CARTESIAN_POINT ( 'NONE',  ( -96.15314808468751551, 88.00268892867056536, 86.73239583420048859 ) ) ;
#59012 = CARTESIAN_POINT ( 'NONE',  ( 93.84685191531248449, 91.99731107132950569, 84.45697916753380241 ) ) ;
#59013 = EDGE_CURVE ( 'NONE', #14636, #51420, #53545, .T. ) ;
#59014 = ORIENTED_EDGE ( 'NONE', *, *, #58324, .F. ) ;
#59015 = CARTESIAN_POINT ( 'NONE',  ( 93.67499999999998295, 92.29496732002878900, 87.43354166840096298 ) ) ;
#59016 =( NAMED_UNIT ( * ) SI_UNIT ( $, .STERADIAN. ) SOLID_ANGLE_UNIT ( ) );
#59017 = ORIENTED_EDGE ( 'NONE', *, *, #29514, .F. ) ;
#59018 = FACE_BOUND ( 'NONE', #8902, .T. ) ;
#59019 = CIRCLE ( 'NONE', #63800, 82.00000000000000000 ) ;
#59020 = EDGE_CURVE ( 'NONE', #14313, #15645, #43928, .T. ) ;
#59021 = EDGE_CURVE ( 'NONE', #23903, #42454, #8049, .T. ) ;
#59022 = CARTESIAN_POINT ( 'NONE',  ( -93.67499999999998295, -207.7050326799711968, 75.18333333333332291 ) ) ;
#59023 = ORIENTED_EDGE ( 'NONE', *, *, #213, .T. ) ;
#59024 = AXIS2_PLACEMENT_3D ( 'NONE', #54023, #38199, #66050 ) ;
#59025 = VERTEX_POINT ( 'NONE', #19692 ) ;
#59026 = EDGE_LOOP ( 'NONE', ( #10824, #68883, #21503, #32343 ) ) ;
#59027 = LINE ( 'NONE', #48104, #69695 ) ;
#59028 = CIRCLE ( 'NONE', #26592, 82.00000000000000000 ) ;
#59029 = LINE ( 'NONE', #23332, #7289 ) ;
#59030 = CARTESIAN_POINT ( 'NONE',  ( -95.00000000000002842, 93.05995642670501411, 85.39624999999998067 ) ) ;
#59031 = ORIENTED_EDGE ( 'NONE', *, *, #10154, .T. ) ;
#59032 = EDGE_CURVE ( 'NONE', #61902, #38392, #44500, .T. ) ;
#59033 = CARTESIAN_POINT ( 'NONE',  ( 97.30629616937500259, 90.00000000000002842, 74.79348190356851944 ) ) ;
#59034 = CYLINDRICAL_SURFACE ( 'NONE', #56340, 2.649999999999985700 ) ;
#59035 = ORIENTED_EDGE ( 'NONE', *, *, #12463, .F. ) ;
#59036 = DIRECTION ( 'NONE',  ( 0.000000000000000000, -0.7604059656000227152, -0.6494480483301934282 ) ) ;
#59037 = CARTESIAN_POINT ( 'NONE',  ( -97.30629616937495996, -209.9999999999999716, 81.38781250086714181 ) ) ;
#59038 = ORIENTED_EDGE ( 'NONE', *, *, #30623, .T. ) ;
#59039 = LINE ( 'NONE', #7527, #67472 ) ;
#59040 = FACE_OUTER_BOUND ( 'NONE', #55554, .T. ) ;
#59041 = DIRECTION ( 'NONE',  ( 0.000000000000000000, 0.000000000000000000, -1.000000000000000000 ) ) ;
#59042 = CARTESIAN_POINT ( 'NONE',  ( 7.103376864691351012E-17, -120.0000000000000000, -90.00000000000000000 ) ) ;
#59043 = CARTESIAN_POINT ( 'NONE',  ( 6.000000000000000000, -3.894527615417333610, -81.90746397400393164 ) ) ;
#59044 =( NAMED_UNIT ( * ) PLANE_ANGLE_UNIT ( ) SI_UNIT ( $, .RADIAN. ) );
#59045 = CARTESIAN_POINT ( 'NONE',  ( -3.000000000000000000, -1.278221433540145391, -26.51162292216073979 ) ) ;
#59046 = DIRECTION ( 'NONE',  ( 1.000000000000000000, -3.061616997868382648E-16, -0.000000000000000000 ) ) ;
#59047 = CYLINDRICAL_SURFACE ( 'NONE', #26685, 82.00000000000000000 ) ;
#59048 = CARTESIAN_POINT ( 'NONE',  ( 10.00000000000000000, -9.188173127307592836, 40.98264845739746676 ) ) ;
#59049 = CARTESIAN_POINT ( 'NONE',  ( -93.84685191531254134, 91.99731107132950569, 89.58989583420049030 ) ) ;
#59050 = CARTESIAN_POINT ( 'NONE',  ( -19.90058851926621131, -132.5883508287165853, -5.500000000000000000 ) ) ;
#59051 = DIRECTION ( 'NONE',  ( 0.000000000000000000, -0.8910065241883627918, -0.4539904997395567965 ) ) ;
#59052 = FACE_OUTER_BOUND ( 'NONE', #18872, .T. ) ;
#59053 =( GEOMETRIC_REPRESENTATION_CONTEXT ( 3 ) GLOBAL_UNCERTAINTY_ASSIGNED_CONTEXT ( ( #37605 ) ) GLOBAL_UNIT_ASSIGNED_CONTEXT ( ( #34955, #52603, #18032 ) ) REPRESENTATION_CONTEXT ( 'NONE', 'WORKASPACE' ) );
#59054 = AXIS2_PLACEMENT_3D ( 'NONE', #24810, #53024, #30802 ) ;
#59055 = DIRECTION ( 'NONE',  ( -1.000000000000000000, 0.000000000000000000, 0.000000000000000000 ) ) ;
#59056 = CARTESIAN_POINT ( 'NONE',  ( 10.00000000000000000, -0.6853352020787742971, -37.58145647212455032 ) ) ;
#59057 = CARTESIAN_POINT ( 'NONE',  ( -2.981742216678212820, 0.000000000000000000, 0.000000000000000000 ) ) ;
#59058 = AXIS2_PLACEMENT_3D ( 'NONE', #28983, #68855, #51917 ) ;
#59059 = CARTESIAN_POINT ( 'NONE',  ( 0.000000000000000000, 0.000000000000000000, 0.000000000000000000 ) ) ;
#59060 = CARTESIAN_POINT ( 'NONE',  ( -96.15314808468745866, -211.9973110713294489, 75.30239583420048177 ) ) ;
#59061 = AXIS2_PLACEMENT_3D ( 'NONE', #42850, #36095, #7530 ) ;
#59062 = CARTESIAN_POINT ( 'NONE',  ( 0.000000000000000000, 72.35432306680455383, 20.40083707023012494 ) ) ;
#59063 =( REPRESENTATION_RELATIONSHIP ('NONE','NONE', #31117, #33525 ) REPRESENTATION_RELATIONSHIP_WITH_TRANSFORMATION ( #45529 )SHAPE_REPRESENTATION_RELATIONSHIP( ) );
#59064 = VECTOR ( 'NONE', #54376, 1000.000000000000000 ) ;
#59065 = ORIENTED_EDGE ( 'NONE', *, *, #20456, .F. ) ;
#59066 = DIRECTION ( 'NONE',  ( 1.427937372958396981E-15, -1.000000000000000000, 1.065814103640131031E-14 ) ) ;
#59067 = DIRECTION ( 'NONE',  ( 2.603472992746261562E-14, 2.546204323184492723E-14, -1.000000000000000000 ) ) ;
#59068 = CARTESIAN_POINT ( 'NONE',  ( 0.000000000000000000, 41.91543099594818500, -2.663952781846294915 ) ) ;
#59069 = LINE ( 'NONE', #25225, #12567 ) ;
#59070 = VECTOR ( 'NONE', #39528, 1000.000000000000000 ) ;
#59071 = AXIS2_PLACEMENT_3D ( 'NONE', #3925, #61046, #53934 ) ;
#59072 = EDGE_CURVE ( 'NONE', #15793, #49934, #33193, .T. ) ;
#59073 = CIRCLE ( 'NONE', #57851, 31.99999999999999289 ) ;
#59074 = DIRECTION ( 'NONE',  ( -1.000000000000000000, 0.000000000000000000, 0.000000000000000000 ) ) ;
#59075 = ORIENTED_EDGE ( 'NONE', *, *, #7974, .T. ) ;
#59076 = EDGE_CURVE ( 'NONE', #60432, #24766, #53418, .T. ) ;
#59077 = DIRECTION ( 'NONE',  ( 0.000000000000000000, 0.000000000000000000, 1.000000000000000000 ) ) ;
#59078 = ORIENTED_EDGE ( 'NONE', *, *, #37772, .T. ) ;
#59079 = ADVANCED_FACE ( 'NONE', ( #45240 ), #66681, .T. ) ;
#59080 = CARTESIAN_POINT ( 'NONE',  ( 95.00000000000000000, -207.3369185715606307, 85.67406250086715147 ) ) ;
#59081 = CARTESIAN_POINT ( 'NONE',  ( 93.84685191531249870, -208.0026889286704943, 89.69572916753382685 ) ) ;
#59082 = ORIENTED_EDGE ( 'NONE', *, *, #65104, .T. ) ;
#59083 = CARTESIAN_POINT ( 'NONE',  ( 93.84685191531251292, -211.9973110713294489, 89.27239583420049485 ) ) ;
#59084 = VERTEX_POINT ( 'NONE', #72312 ) ;
#59085 = FACE_BOUND ( 'NONE', #72744, .T. ) ;
#59086 = ORIENTED_EDGE ( 'NONE', *, *, #58645, .F. ) ;
#59087 = CARTESIAN_POINT ( 'NONE',  ( -92.69370383062502583, 88.66845928578038638, 81.17614583420048291 ) ) ;
#59088 = EDGE_LOOP ( 'NONE', ( #65573, #8685, #67589, #31614 ) ) ;
#59089 = ORIENTED_EDGE ( 'NONE', *, *, #35146, .F. ) ;
#59090 = DIRECTION ( 'NONE',  ( 1.000000000000000000, -3.061616997868382648E-16, -0.000000000000000000 ) ) ;
#59091 = ORIENTED_EDGE ( 'NONE', *, *, #66041, .F. ) ;
#59092 = CARTESIAN_POINT ( 'NONE',  ( 97.65000000000000568, -208.4700217866474645, 84.73479166840094479 ) ) ;
#59093 = ADVANCED_FACE ( 'NONE', ( #16658 ), #9536, .T. ) ;
#59094 = EDGE_CURVE ( 'NONE', #19675, #32344, #49380, .T. ) ;
#59095 = EDGE_LOOP ( 'NONE', ( #34557, #25031, #50018, #37568, #20685, #54218 ) ) ;
#59096 = DIRECTION ( 'NONE',  ( 0.000000000000000000, 0.000000000000000000, 1.000000000000000000 ) ) ;
#59097 = ORIENTED_EDGE ( 'NONE', *, *, #10942, .F. ) ;
#59098 = DIRECTION ( 'NONE',  ( 0.000000000000000000, 0.2334453638559060851, -0.9723699203976764460 ) ) ;
#59099 = ORIENTED_EDGE ( 'NONE', *, *, #72039, .T. ) ;
#59100 =( GEOMETRIC_REPRESENTATION_CONTEXT ( 3 ) GLOBAL_UNCERTAINTY_ASSIGNED_CONTEXT ( ( #37754 ) ) GLOBAL_UNIT_ASSIGNED_CONTEXT ( ( #47260, #34866, #6306 ) ) REPRESENTATION_CONTEXT ( 'NONE', 'WORKASPACE' ) );
#59101 = VECTOR ( 'NONE', #8077, 1000.000000000000000 ) ;
#59102 = VERTEX_POINT ( 'NONE', #33566 ) ;
#59103 = ORIENTED_EDGE ( 'NONE', *, *, #10502, .F. ) ;
#59104 = CARTESIAN_POINT ( 'NONE',  ( 97.30629616937498838, -209.9999999999999716, 77.26031250086714408 ) ) ;
#59106 = EDGE_CURVE ( 'NONE', #15149, #27433, #20994, .T. ) ;
#59105 = CYLINDRICAL_SURFACE ( 'NONE', #56903, 16.00000000000000000 ) ;
#59107 = EDGE_CURVE ( 'NONE', #33770, #47439, #61958, .T. ) ;
#59108 = ITEM_DEFINED_TRANSFORMATION ( 'NONE', 'NONE', #56796,  #43395 ) ;
#59110 = DIRECTION ( 'NONE',  ( 0.000000000000000000, 0.9510565162951510887, -0.3090169943749551673 ) ) ;
#59109 = AXIS2_PLACEMENT_3D ( 'NONE', #51093, #74016, #51460 ) ;
#59111 = CARTESIAN_POINT ( 'NONE',  ( 11.99999999999999822, 59.03342792756263435, 46.54456581323825048 ) ) ;
#59112 = CARTESIAN_POINT ( 'NONE',  ( -97.64999999999996305, -209.9999999999999716, 75.39499999999999602 ) ) ;
#59113 = LINE ( 'NONE', #24518, #68522 ) ;
#59114 = DIRECTION ( 'NONE',  ( 0.000000000000000000, 0.000000000000000000, -1.000000000000000000 ) ) ;
#59115 = CARTESIAN_POINT ( 'NONE',  ( -92.69370383062498320, -208.6684592857803011, 84.29822916753380468 ) ) ;
#59116 = CARTESIAN_POINT ( 'NONE',  ( -95.00000000000002842, 92.66308142843932671, 82.02281250086714692 ) ) ;
#59117 = VERTEX_POINT ( 'NONE', #62541 ) ;
#59118 = CARTESIAN_POINT ( 'NONE',  ( 93.84685191531248449, 91.99731107132950569, 80.01197916753380923 ) ) ;
#59119 = AXIS2_PLACEMENT_3D ( 'NONE', #32187, #49853, #27287 ) ;
#59120 =( BOUNDED_CURVE ( )  B_SPLINE_CURVE ( 2, ( #10805, #51383, #50643, #67949, #68700, #5554, #67202 ),
 .UNSPECIFIED., .F., .F. ) 
 B_SPLINE_CURVE_WITH_KNOTS ( ( 3, 2, 2, 3 ),
 ( 0.3333333333333333703, 0.3402777777777777901, 0.3472222222222221544, 0.3541666666666665741 ),
 .UNSPECIFIED. ) 
 CURVE ( )  GEOMETRIC_REPRESENTATION_ITEM ( )  RATIONAL_B_SPLINE_CURVE ( ( 0.9999999999999988898, 0.8660254037844398178, 1.000000000000000000, 0.8660254037844387076, 1.000000000000000000, 0.8660254037844408170, 0.9999999999999978906 ) ) 
 REPRESENTATION_ITEM ( '' )  );
#59121 = ORIENTED_EDGE ( 'NONE', *, *, #51648, .T. ) ;
#59122 = CARTESIAN_POINT ( 'NONE',  ( 0.000000000000000000, -6.555932627142143865, -37.01155633439065440 ) ) ;
#59123 = DIRECTION ( 'NONE',  ( -1.000000000000000000, 0.000000000000000000, 0.000000000000000000 ) ) ;
#59124 = DIRECTION ( 'NONE',  ( 2.603472992745699578E-14, -2.546204323184531851E-14, 1.000000000000000000 ) ) ;
#59125 = CARTESIAN_POINT ( 'NONE',  ( 2.449999999999998845, 0.000000000000000000, -0.3851141460153411078 ) ) ;
#59126 = CARTESIAN_POINT ( 'NONE',  ( 10.00000000000000000, -66.50666863322028632, 39.78640506895582973 ) ) ;
#59127 = CARTESIAN_POINT ( 'NONE',  ( -92.69370383062498320, -211.3315407142195852, 84.19239583420048234 ) ) ;
#59128 = CARTESIAN_POINT ( 'NONE',  ( 22.08297821871651934, -111.8242998470044540, 5.500000000000000000 ) ) ;
#59129 = DIRECTION ( 'NONE',  ( 0.000000000000000000, 0.000000000000000000, 1.000000000000000000 ) ) ;
#59130 = AXIS2_PLACEMENT_3D ( 'NONE', #14500, #37459, #2543 ) ;
#59131 = ORIENTED_EDGE ( 'NONE', *, *, #47218, .T. ) ;
#59132 = CIRCLE ( 'NONE', #50733, 31.99999999999999289 ) ;
#59133 = ORIENTED_EDGE ( 'NONE', *, *, #577, .T. ) ;
#59134 = CARTESIAN_POINT ( 'NONE',  ( -93.09170270117418511, 88.16127723152901297, 74.99909419456534465 ) ) ;
#59135 = DIRECTION ( 'NONE',  ( -1.000000000000000000, 5.236901059551556403E-15, 2.618450529775778123E-14 ) ) ;
#59136 = CARTESIAN_POINT ( 'NONE',  ( -93.84685191531254134, 91.99731107132950569, 89.43114583420047836 ) ) ;
#59137 = LINE ( 'NONE', #36195, #36994 ) ;
#59138 = DIRECTION ( 'NONE',  ( 0.1850432970638682395, -0.9827303690289279636, 0.000000000000000000 ) ) ;
#59139 = FACE_OUTER_BOUND ( 'NONE', #38022, .T. ) ;
#59140 = CARTESIAN_POINT ( 'NONE',  ( 21.85433023846371370, -135.0628101570779620, 5.500000000000000000 ) ) ;
#59141 = ORIENTED_EDGE ( 'NONE', *, *, #27425, .F. ) ;
#59142 = CARTESIAN_POINT ( 'NONE',  ( 10.00000000000000000, 72.35160999960817207, 20.41045688087850607 ) ) ;
#59143 = CARTESIAN_POINT ( 'NONE',  ( 2.600913415846943225E-12, -120.0000000000000000, -65.00000000000000000 ) ) ;
#59144 = CARTESIAN_POINT ( 'NONE',  ( 2.459674775249762302, 3.512261536898573354E-15, 1.958521724562357923E-15 ) ) ;
#59145 = DIRECTION ( 'NONE',  ( 0.000000000000000000, 0.000000000000000000, 1.000000000000000000 ) ) ;
#59146 = DIRECTION ( 'NONE',  ( 0.000000000000000000, 0.000000000000000000, 1.000000000000000000 ) ) ;
#59147 = CARTESIAN_POINT ( 'NONE',  ( -93.84685191531248449, -208.0026889286704943, 85.77989583420048803 ) ) ;
#59148 = CARTESIAN_POINT ( 'NONE',  ( -10.00000000000000000, 0.000000000000000000, 0.000000000000000000 ) ) ;
#59149 = EDGE_CURVE ( 'NONE', #12767, #16822, #62155, .T. ) ;
#59150 = CARTESIAN_POINT ( 'NONE',  ( 15.00000000000000000, -18.13022148937263012, -15.02647892043543898 ) ) ;
#59151 = PRODUCT_RELATED_PRODUCT_CATEGORY ( 'part', '', ( #66185 ) ) ;
#59152 = ADVANCED_FACE ( 'NONE', ( #61036 ), #9899, .F. ) ;
#59153 = CARTESIAN_POINT ( 'NONE',  ( -92.69370383062498320, -211.3315407142195852, 76.73114583420048973 ) ) ;
#59154 = CYLINDRICAL_SURFACE ( 'NONE', #1480, 31.99999999999998579 ) ;
#59155 = ORIENTED_EDGE ( 'NONE', *, *, #879, .T. ) ;
#59156 =( GEOMETRIC_REPRESENTATION_CONTEXT ( 3 ) GLOBAL_UNCERTAINTY_ASSIGNED_CONTEXT ( ( #43063 ) ) GLOBAL_UNIT_ASSIGNED_CONTEXT ( ( #64548, #20145, #54741 ) ) REPRESENTATION_CONTEXT ( 'NONE', 'WORKASPACE' ) );
#59157 = CARTESIAN_POINT ( 'NONE',  ( 10.00000000000000000, 0.000000000000000000, 0.000000000000000000 ) ) ;
#59158 = DIRECTION ( 'NONE',  ( -0.000000000000000000, -0.000000000000000000, 1.000000000000000000 ) ) ;
#59159 = CARTESIAN_POINT ( 'NONE',  ( -97.30629616937495996, -209.9999999999999716, 89.80156250086714920 ) ) ;
#59160 = EDGE_CURVE ( 'NONE', #34558, #3167, #43762, .T. ) ;
#59161 = CARTESIAN_POINT ( 'NONE',  ( 11.99999999999999822, 65.58780272294076497, 36.73666225445916211 ) ) ;
#59162 = CARTESIAN_POINT ( 'NONE',  ( 96.15314808468748708, -208.0026889286704943, 76.73114583420047552 ) ) ;
#59163 = ORIENTED_EDGE ( 'NONE', *, *, #16402, .T. ) ;
#59164 = ADVANCED_FACE ( 'NONE', ( #10271 ), #27932, .T. ) ;
#59165 = AXIS2_PLACEMENT_3D ( 'NONE', #54242, #65157, #36555 ) ;
#59166 = LINE ( 'NONE', #64813, #71976 ) ;
#59167 = ORIENTED_EDGE ( 'NONE', *, *, #69686, .T. ) ;
#59168 = AXIS2_PLACEMENT_3D ( 'NONE', #27901, #43735, #60654 ) ;
#59169 = EDGE_CURVE ( 'NONE', #55103, #34880, #49740, .T. ) ;
#59170 = DIRECTION ( 'NONE',  ( -1.000000000000000000, -0.000000000000000000, -0.000000000000000000 ) ) ;
#59171 = ORIENTED_EDGE ( 'NONE', *, *, #23264, .T. ) ;
#59172 = CIRCLE ( 'NONE', #50732, 31.99999999999998579 ) ;
#59173 = DIRECTION ( 'NONE',  ( -1.000000000000000000, 0.000000000000000000, 0.000000000000000000 ) ) ;
#59174 = AXIS2_PLACEMENT_3D ( 'NONE', #52563, #24008, #25106 ) ;
#59175 = VERTEX_POINT ( 'NONE', #61788 ) ;
#59176 = ORIENTED_EDGE ( 'NONE', *, *, #8257, .F. ) ;
#59177 = ORIENTED_EDGE ( 'NONE', *, *, #57457, .F. ) ;
#59178 = CARTESIAN_POINT ( 'NONE',  ( -92.35000000000003695, 90.00000000000004263, 90.00000000000000000 ) ) ;
#59179 = EDGE_CURVE ( 'NONE', #43284, #57981, #64223, .T. ) ;
#59180 = EDGE_CURVE ( 'NONE', #35421, #61359, #29523, .T. ) ;
#59181 = EDGE_LOOP ( 'NONE', ( #52419, #53069, #25795, #59998 ) ) ;
#59182 = EDGE_LOOP ( 'NONE', ( #71763, #72016, #42636, #40018 ) ) ;
#59183 = CARTESIAN_POINT ( 'NONE',  ( 94.99999999999998579, 92.66308142843935514, 81.38781250086715602 ) ) ;
#59184 = CARTESIAN_POINT ( 'NONE',  ( -10.00000000000000000, 0.000000000000000000, 0.000000000000000000 ) ) ;
#59185 = CARTESIAN_POINT ( 'NONE',  ( 92.35000000000000853, -209.9999999999999716, 75.39499999999999602 ) ) ;
#59186 = ORIENTED_EDGE ( 'NONE', *, *, #30950, .F. ) ;
#59187 = ORIENTED_EDGE ( 'NONE', *, *, #47773, .T. ) ;
#59188 = ORIENTED_EDGE ( 'NONE', *, *, #11438, .F. ) ;
#59189 = DIRECTION ( 'NONE',  ( -1.000000000000000000, -0.000000000000000000, -0.000000000000000000 ) ) ;
#59190 = ORIENTED_EDGE ( 'NONE', *, *, #70110, .T. ) ;
#59191 = CARTESIAN_POINT ( 'NONE',  ( -0.09991859744143775923, 0.8239637576285355758, -54.99999999999998579 ) ) ;
#59192 = DIRECTION ( 'NONE',  ( 0.000000000000000000, 0.000000000000000000, 1.000000000000000000 ) ) ;
#59193 = CARTESIAN_POINT ( 'NONE',  ( 0.000000000000000000, -30.41916302227061664, -71.27951684758058093 ) ) ;
#59194 = DIRECTION ( 'NONE',  ( -1.000000000000000000, 0.000000000000000000, 0.000000000000000000 ) ) ;
#59195 = CARTESIAN_POINT ( 'NONE',  ( 10.00000000000000000, 0.000000000000000000, 0.000000000000000000 ) ) ;
#59196 = CARTESIAN_POINT ( 'NONE',  ( 11.99999999999999822, 64.81221759200417409, -50.23322058963275794 ) ) ;
#59197 = DIRECTION ( 'NONE',  ( -1.000000000000000000, 0.000000000000000000, -0.000000000000000000 ) ) ;
#59198 = CARTESIAN_POINT ( 'NONE',  ( -97.64999999999994884, -208.4700217866474645, 77.96145833506763267 ) ) ;
#59199 = CARTESIAN_POINT ( 'NONE',  ( 5.999999999999999112, -59.75363087400035056, -56.15606465355020305 ) ) ;
#59201 = CARTESIAN_POINT ( 'NONE',  ( -96.32500000000001705, 92.29496732002878900, 74.73354166840096013 ) ) ;
#59200 = CARTESIAN_POINT ( 'NONE',  ( 93.84685191531248449, 91.99731107132950569, 89.53697916753381492 ) ) ;
#59202 = ORIENTED_EDGE ( 'NONE', *, *, #46177, .F. ) ;
#59203 = CARTESIAN_POINT ( 'NONE',  ( 93.84685191531248449, 91.99731107132950569, 76.36072916753381890 ) ) ;
#59204 = CARTESIAN_POINT ( 'NONE',  ( 15.00000000000000000, 24.81905959214260804, -9.408202855044828894 ) ) ;
#59205 = FACE_OUTER_BOUND ( 'NONE', #67996, .T. ) ;
#59206 = DIRECTION ( 'NONE',  ( 0.000000000000000000, 0.000000000000000000, -1.000000000000000000 ) ) ;
#59207 = CARTESIAN_POINT ( 'NONE',  ( 92.35004024445041182, -211.5300014484966766, 77.43229327564786502 ) ) ;
#59208 = LINE ( 'NONE', #70844, #64240 ) ;
#59209 = AXIS2_PLACEMENT_3D ( 'NONE', #71186, #32080, #20809 ) ;
#59210 = VERTEX_POINT ( 'NONE', #61418 ) ;
#59211 = DIRECTION ( 'NONE',  ( 1.000000000000000000, 0.000000000000000000, 0.000000000000000000 ) ) ;
#59212 = DIRECTION ( 'NONE',  ( -2.603472992746261562E-14, -2.546204323184492723E-14, 1.000000000000000000 ) ) ;
#59213 = ORIENTED_EDGE ( 'NONE', *, *, #54318, .T. ) ;
#59214 = AXIS2_PLACEMENT_3D ( 'NONE', #28637, #73386, #56495 ) ;
#59215 = ORIENTED_EDGE ( 'NONE', *, *, #29208, .F. ) ;
#59216 = CARTESIAN_POINT ( 'NONE',  ( 0.000000000000000000, -70.52718814184240159, -26.02418014898383802 ) ) ;
#59217 = DIRECTION ( 'NONE',  ( -1.000000000000000000, 0.000000000000000000, 0.000000000000000000 ) ) ;
#59218 = CARTESIAN_POINT ( 'NONE',  ( -92.35000000005462084, -210.0000170173125014, 88.49187441316038871 ) ) ;
#59219 = LINE ( 'NONE', #64870, #10135 ) ;
#59220 = VECTOR ( 'NONE', #71636, 1000.000000000000000 ) ;
#59221 = CARTESIAN_POINT ( 'NONE',  ( -94.99999999999997158, -207.3369185715606307, 77.57781250086715374 ) ) ;
#59222 = CIRCLE ( 'NONE', #63005, 42.00000000000000000 ) ;
#59223 = VERTEX_POINT ( 'NONE', #44114 ) ;
#59224 = ADVANCED_FACE ( 'NONE', ( #55769 ), #27174, .F. ) ;
#59225 = AXIS2_PLACEMENT_3D ( 'NONE', #62249, #44590, #67509 ) ;
#59226 = DIRECTION ( 'NONE',  ( -0.000000000000000000, -0.000000000000000000, 1.000000000000000000 ) ) ;
#59227 = AXIS2_PLACEMENT_3D ( 'NONE', #18713, #52560, #63494 ) ;
#59228 = CIRCLE ( 'NONE', #54396, 16.00000000000000000 ) ;
#59229 = FACE_OUTER_BOUND ( 'NONE', #21811, .T. ) ;
#59230 = LINE ( 'NONE', #70122, #3416 ) ;
#59231 = LINE ( 'NONE', #47947, #6835 ) ;
#59232 = CARTESIAN_POINT ( 'NONE',  ( 10.00000000000000000, -37.01155633439063308, 6.555932627142289526 ) ) ;
#59233 = CARTESIAN_POINT ( 'NONE',  ( -2.500000000000015543, -73.00000000000001421, -201.6999999999999886 ) ) ;
#59234 = EDGE_CURVE ( 'NONE', #6682, #27925, #54924, .T. ) ;
#59235 = CARTESIAN_POINT ( 'NONE',  ( 11.99999999999999822, 31.46837873494978055, 68.27212725128286763 ) ) ;
#59236 = DIRECTION ( 'NONE',  ( -1.000000000000000000, 0.000000000000000000, 0.000000000000000000 ) ) ;
#59237 = PLANE ( 'NONE',  #34018 ) ;
#59238 = EDGE_CURVE ( 'NONE', #4351, #8216, #66626, .T. ) ;
#59239 = DIRECTION ( 'NONE',  ( 1.000000000000000000, 0.000000000000000000, 0.000000000000000000 ) ) ;
#59240 = CARTESIAN_POINT ( 'NONE',  ( 93.84685191531248449, 88.00268892867053694, 83.55739583420049144 ) ) ;
#59241 = ADVANCED_FACE ( 'NONE', ( #69271 ), #18137, .F. ) ;
#59242 = CARTESIAN_POINT ( 'NONE',  ( -94.99999999999997158, -207.3369185715606307, 85.83281250086717762 ) ) ;
#59243 = DIRECTION ( 'NONE',  ( -1.000000000000000000, 0.000000000000000000, -0.000000000000000000 ) ) ;
#59244 = ORIENTED_EDGE ( 'NONE', *, *, #17060, .F. ) ;
#59245 = CARTESIAN_POINT ( 'NONE',  ( -97.65000000000001990, 90.00000000000004263, 81.74500000000000455 ) ) ;
#59246 = CARTESIAN_POINT ( 'NONE',  ( -96.32499999999996021, -207.7050326799711968, 79.73416666666666686 ) ) ;
#59247 = CARTESIAN_POINT ( 'NONE',  ( -97.30629616937501680, 90.00000000000004263, 77.57781250086713953 ) ) ;
#59248 = CARTESIAN_POINT ( 'NONE',  ( 93.84685191531251292, -211.9973110713294489, 85.93864583420048575 ) ) ;
#59249 = ORIENTED_EDGE ( 'NONE', *, *, #6145, .F. ) ;
#59250 = VECTOR ( 'NONE', #16801, 1000.000000000000000 ) ;
#59251 = ORIENTED_EDGE ( 'NONE', *, *, #56396, .T. ) ;
#59252 = EDGE_CURVE ( 'NONE', #26000, #24844, #70200, .T. ) ;
#59253 = EDGE_LOOP ( 'NONE', ( #6302, #1826, #61106, #33532 ) ) ;
#59254 = CARTESIAN_POINT ( 'NONE',  ( 0.000000000000000000, 63.18004540533092239, -44.88180994100307686 ) ) ;
#59255 = DIRECTION ( 'NONE',  ( 1.000000000000000000, 0.000000000000000000, 0.000000000000000000 ) ) ;
#59256 = AXIS2_PLACEMENT_3D ( 'NONE', #15324, #9698, #27345 ) ;
#59257 = EDGE_LOOP ( 'NONE', ( #11373, #15823, #53919, #6211 ) ) ;
#59258 = ORIENTED_EDGE ( 'NONE', *, *, #50637, .T. ) ;
#59259 = DIRECTION ( 'NONE',  ( 2.603472992746261562E-14, 2.546204323184492723E-14, -1.000000000000000000 ) ) ;
#59260 = CARTESIAN_POINT ( 'NONE',  ( 95.00000000000000000, -207.3369185715606307, 81.38781250086715602 ) ) ;
#59261 = EDGE_CURVE ( 'NONE', #63454, #54824, #71540, .T. ) ;
#59262 = CARTESIAN_POINT ( 'NONE',  ( 16.30584220631899228, -140.9432449716519784, 5.500000000000000000 ) ) ;
#59263 = ADVANCED_FACE ( 'NONE', ( #24159 ), #57634, .T. ) ;
#59264 = DIRECTION ( 'NONE',  ( -1.000000000000000000, 0.000000000000000000, 0.000000000000000000 ) ) ;
#59265 = VECTOR ( 'NONE', #57, 1000.000000000000114 ) ;
#59266 = CARTESIAN_POINT ( 'NONE',  ( 12.00000000000000000, -23.29833615347104470, 3.418703333116808629 ) ) ;
#59267 = DIRECTION ( 'NONE',  ( -1.000000000000000000, -0.000000000000000000, -0.000000000000000000 ) ) ;
#59268 = EDGE_CURVE ( 'NONE', #32344, #66338, #24206, .T. ) ;
#59269 = AXIS2_PLACEMENT_3D ( 'NONE', #39368, #5911, #66548 ) ;
#59270 = CARTESIAN_POINT ( 'NONE',  ( 0.000000000000000000, 0.000000000000000000, 0.000000000000000000 ) ) ;
#59271 = CARTESIAN_POINT ( 'NONE',  ( 92.35000000000000853, -209.9999999999999716, 84.28499999999999659 ) ) ;
#59272 = VERTEX_POINT ( 'NONE', #69639 ) ;
#59273 = ORIENTED_EDGE ( 'NONE', *, *, #2535, .F. ) ;
#59274 = VERTEX_POINT ( 'NONE', #40704 ) ;
#59275 = AXIS2_PLACEMENT_3D ( 'NONE', #43532, #49142, #9285 ) ;
#59276 = ORIENTED_EDGE ( 'NONE', *, *, #40586, .F. ) ;
#59277 = CYLINDRICAL_SURFACE ( 'NONE', #57442, 77.49899999999999523 ) ;
#59278 = AXIS2_PLACEMENT_3D ( 'NONE', #5900, #28060, #27310 ) ;
#59279 = CARTESIAN_POINT ( 'NONE',  ( -95.00000000000002842, 87.33691857156074434, 84.88031250086714863 ) ) ;
#59280 = CARTESIAN_POINT ( 'NONE',  ( 10.00000000000000000, -37.48860685352291711, 0.8828120875899322373 ) ) ;
#59281 = CARTESIAN_POINT ( 'NONE',  ( -10.00000000000000000, 0.000000000000000000, 0.000000000000000000 ) ) ;
#59282 = CARTESIAN_POINT ( 'NONE',  ( 92.69370383062501162, -208.6684592857803011, 88.95489583420048518 ) ) ;
#59283 = CARTESIAN_POINT ( 'NONE',  ( 97.64999999999999147, 90.00000000000002842, 76.34749999999999659 ) ) ;
#59284 = ORIENTED_EDGE ( 'NONE', *, *, #72887, .T. ) ;
#59285 = CARTESIAN_POINT ( 'NONE',  ( -92.34999999999999432, -208.4700217866474645, 88.54479166840097548 ) ) ;
#59286 = EDGE_LOOP ( 'NONE', ( #52584, #72580, #35990, #34595 ) ) ;
#59287 = PLANE ( 'NONE',  #45838 ) ;
#59288 = ORIENTED_EDGE ( 'NONE', *, *, #14501, .T. ) ;
#59289 = CARTESIAN_POINT ( 'NONE',  ( -97.65000000000001990, 91.52997821335253548, 84.94645833506763211 ) ) ;
#59290 = CARTESIAN_POINT ( 'NONE',  ( 97.30629616937498838, 90.00000000000002842, 86.94406250086716170 ) ) ;
#59291 = FACE_OUTER_BOUND ( 'NONE', #12808, .T. ) ;
#59292 = CIRCLE ( 'NONE', #41265, 32.50000000000000000 ) ;
#59293 = CARTESIAN_POINT ( 'NONE',  ( 10.00000000000000000, 59.03342792756263435, 46.54456581323825048 ) ) ;
#59294 = DIRECTION ( 'NONE',  ( -1.000000000000000000, 0.000000000000000000, 0.000000000000000000 ) ) ;
#59295 = DIRECTION ( 'NONE',  ( 0.000000000000000000, 0.000000000000000000, 1.000000000000000000 ) ) ;
#59296 = ORIENTED_EDGE ( 'NONE', *, *, #59683, .F. ) ;
#59297 = CARTESIAN_POINT ( 'NONE',  ( -9.974659986866640793E-15, -5.773502691896262640, -5.553418012614792509 ) ) ;
#59298 = CARTESIAN_POINT ( 'NONE',  ( -97.30629616937497417, -211.3315407142195852, 75.09072916753382287 ) ) ;
#59299 = ORIENTED_EDGE ( 'NONE', *, *, #4778, .T. ) ;
#59300 = ORIENTED_EDGE ( 'NONE', *, *, #57984, .F. ) ;
#59301 = FACE_BOUND ( 'NONE', #10822, .T. ) ;
#59302 = CYLINDRICAL_SURFACE ( 'NONE', #70804, 16.00000000000000000 ) ;
#59303 = VECTOR ( 'NONE', #47448, 1000.000000000000000 ) ;
#59304 = CARTESIAN_POINT ( 'NONE',  ( 3.000000000000000000, 3.113052163432572109E-16, -2.541999999999999815 ) ) ;
#59305 = CARTESIAN_POINT ( 'NONE',  ( -94.99999999999997158, -212.6630814284392557, 88.69031250086716511 ) ) ;
#59306 = ORIENTED_EDGE ( 'NONE', *, *, #53570, .F. ) ;
#59307 = CARTESIAN_POINT ( 'NONE',  ( 10.00000000000000000, 6.736453364083557105, 36.88895765772635826 ) ) ;
#59308 = ORIENTED_EDGE ( 'NONE', *, *, #55496, .T. ) ;
#59309 = VECTOR ( 'NONE', #41852, 1000.000000000000000 ) ;
#59310 = ADVANCED_FACE ( 'NONE', ( #64377 ), #17396, .T. ) ;
#59311 = EDGE_LOOP ( 'NONE', ( #12669, #59466, #4929, #37476 ) ) ;
#59312 = FACE_OUTER_BOUND ( 'NONE', #24863, .T. ) ;
#59313 = AXIS2_PLACEMENT_3D ( 'NONE', #56967, #18126, #25249 ) ;
#59314 = CARTESIAN_POINT ( 'NONE',  ( 94.99999999999998579, 92.66308142843935514, 89.00781250086716057 ) ) ;
#59315 = DIRECTION ( 'NONE',  ( -1.000000000000000000, -0.000000000000000000, -0.000000000000000000 ) ) ;
#59316 = CARTESIAN_POINT ( 'NONE',  ( 93.84685191531248449, 88.00268892867053694, 80.85864583420047325 ) ) ;
#59317 = CYLINDRICAL_SURFACE ( 'NONE', #59227, 16.00000000000000000 ) ;
#59318 = FACE_OUTER_BOUND ( 'NONE', #56856, .T. ) ;
#59319 = EDGE_CURVE ( 'NONE', #16870, #34217, #6730, .T. ) ;
#59320 = CYLINDRICAL_SURFACE ( 'NONE', #51692, 37.49900000000000233 ) ;
#59321 = DIRECTION ( 'NONE',  ( 0.000000000000000000, -0.1045284632676437703, 0.9945218953682742891 ) ) ;
#59322 = CARTESIAN_POINT ( 'NONE',  ( 0.000000000000000000, 72.35160999960817207, 20.41045688087850607 ) ) ;
#59323 = ADVANCED_FACE ( 'NONE', ( #68546 ), #57256, .T. ) ;
#59324 = CARTESIAN_POINT ( 'NONE',  ( 20.85212586905262100, -130.9402397935870965, 5.500000000000000000 ) ) ;
#59325 = CARTESIAN_POINT ( 'NONE',  ( 96.32499999999998863, 87.70503267997126784, 83.86166666666666458 ) ) ;
#59326 = CIRCLE ( 'NONE', #8929, 31.99999999999998579 ) ;
#59327 =( BOUNDED_CURVE ( )  B_SPLINE_CURVE ( 2, ( #53309, #65339, #1115, #24735, #46936, #47305, #69851 ),
 .UNSPECIFIED., .F., .F. ) 
 B_SPLINE_CURVE_WITH_KNOTS ( ( 3, 2, 2, 3 ),
 ( 0.2916666666666669072, 0.2986111111111113270, 0.3055555555555557468, 0.3125000000000001665 ),
 .UNSPECIFIED. ) 
 CURVE ( )  GEOMETRIC_REPRESENTATION_ITEM ( )  RATIONAL_B_SPLINE_CURVE ( ( 0.9999999999999956701, 0.8660254037844430375, 1.000000000000000000, 0.8660254037844387076, 1.000000000000000000, 0.8660254037844354880, 1.000000000000003109 ) ) 
 REPRESENTATION_ITEM ( '' )  );
#59328 = CIRCLE ( 'NONE', #41299, 31.99999999999999289 ) ;
#59329 = CARTESIAN_POINT ( 'NONE',  ( 10.00000000000000000, -63.97538442413463855, 51.29473840253199768 ) ) ;
#59330 = EDGE_CURVE ( 'NONE', #21721, #15149, #47089, .T. ) ;
#59331 = CARTESIAN_POINT ( 'NONE',  ( 0.000000000000000000, 3.925862922256769583, -41.81611651403857621 ) ) ;
#59332 = EDGE_LOOP ( 'NONE', ( #25807, #70246, #33450, #44684 ) ) ;
#59333 = AXIS2_PLACEMENT_3D ( 'NONE', #5897, #58868, #7362 ) ;
#59334 = CARTESIAN_POINT ( 'NONE',  ( -93.84685191531252713, 88.00268892867056536, 84.77447916753381207 ) ) ;
#59335 = AXIS2_PLACEMENT_3D ( 'NONE', #1577, #65439, #41747 ) ;
#59336 = DIRECTION ( 'NONE',  ( 1.000000000000000000, 0.000000000000000000, 0.000000000000000000 ) ) ;
#59337 = LINE ( 'NONE', #18361, #56064 ) ;
#59338 = VECTOR ( 'NONE', #30989, 1000.000000000000000 ) ;
#59339 = ORIENTED_EDGE ( 'NONE', *, *, #36059, .F. ) ;
#59340 =( BOUNDED_CURVE ( )  B_SPLINE_CURVE ( 2, ( #532, #46359, #175, #23067, #41452, #17046, #6509, #57650, #62937 ),
 .UNSPECIFIED., .F., .F. ) 
 B_SPLINE_CURVE_WITH_KNOTS ( ( 3, 2, 2, 2, 3 ),
 ( 0.8678591737214820245, 0.8749149270694132063, 0.8819706926102950373, 0.8890264581511769792, 0.8890265259358470784 ),
 .UNSPECIFIED. ) 
 CURVE ( )  GEOMETRIC_REPRESENTATION_ITEM ( )  RATIONAL_B_SPLINE_CURVE ( ( 1.000000000000000000, 0.8660254037844387076, 1.000000000000000000, 0.8660254037844387076, 1.000000000000000000, 0.8660254037844387076, 1.000000000000000000, 0.9999987129073719672, 0.9999974258394741522 ) ) 
 REPRESENTATION_ITEM ( '' )  );
#59341 = DIRECTION ( 'NONE',  ( 0.000000000000000000, 0.000000000000000000, 1.000000000000000000 ) ) ;
#59342 = CARTESIAN_POINT ( 'NONE',  ( 10.00000000000000000, 30.00120703465205452, 22.64427369931179967 ) ) ;
#59343 = EDGE_CURVE ( 'NONE', #11526, #44329, #29361, .T. ) ;
#59344 = LINE ( 'NONE', #9305, #11924 ) ;
#59345 = AXIS2_PLACEMENT_3D ( 'NONE', #67420, #27562, #21929 ) ;
#59346 = CARTESIAN_POINT ( 'NONE',  ( -97.64998530153626177, -208.4700133004854479, 76.05645774805350356 ) ) ;
#59347 = CARTESIAN_POINT ( 'NONE',  ( 92.69370383062501162, -208.6684592857803011, 82.76364583420048859 ) ) ;
#59348 = VERTEX_POINT ( 'NONE', #888 ) ;
#59349 = ORIENTED_EDGE ( 'NONE', *, *, #5311, .T. ) ;
#59350 = EDGE_CURVE ( 'NONE', #71222, #47809, #5401, .T. ) ;
#59351 = FACE_OUTER_BOUND ( 'NONE', #45069, .T. ) ;
#59352 = EDGE_LOOP ( 'NONE', ( #39699, #57139, #24383, #30412, #65160, #65842, #30956, #2578, #137, #32800, #45526, #35088, #34976, #40788, #58434, #61401, #48048, #72761, #41957, #55227, #45371, #57799, #2914, #49281, #6233, #26713, #26747, #64392, #66418, #37200, #36158, #58887, #10143, #22197, #37267, #14419, #60742, #22593, #64649, #11841, #39589, #37807, #39167, #73887, #62219, #2070, #3194, #1210, #49017, #19303, #18276, #54290, #41338, #47436, #16171, #24308, #10913, #22445, #49940, #39021, #56127, #67049, #17461, #21828, #14232, #69168, #64569, #5039, #24784, #12860, #46902, #66214, #54572, #68830, #15354, #67945, #57138, #4638, #71171, #42809, #19153, #16779, #8527, #19012, #12960, #38761, #19844, #69704, #27723, #57423, #516, #35358, #31909, #41923, #41550, #7702, #44801, #8126, #58987, #9025, #45795, #48935, #39687, #17138, #26428, #30847, #26444, #34784, #28268, #48079, #70552, #32282, #63119, #6957, #4484, #17103, #64265, #11570, #4253, #70523, #13785, #72499, #39187, #5141, #31317, #74232, #17729, #64542, #50738, #32170, #57969, #71165, #9790, #18195, #22276, #8513, #11091, #59031, #7803, #16873, #64711, #36231, #70638, #17284, #73500, #63298, #13563, #47997, #114, #40242, #58074, #4165, #44045, #68987, #34941, #68265, #68527, #40034, #38874, #1534, #18053, #42962, #49824, #2646, #74054 ) ) ;
#59353 = EDGE_CURVE ( 'NONE', #51767, #1192, #17030, .T. ) ;
#59354 = CARTESIAN_POINT ( 'NONE',  ( 10.00000000000000000, 0.000000000000000000, 0.000000000000000000 ) ) ;
#59355 = CARTESIAN_POINT ( 'NONE',  ( 15.00000000000000000, -0.9646360437375368635, -23.52805723605589705 ) ) ;
#59356 = ORIENTED_EDGE ( 'NONE', *, *, #24116, .T. ) ;
#59357 = CARTESIAN_POINT ( 'NONE',  ( 92.69370383062501162, -209.9999999999999716, 80.91156250086716284 ) ) ;
#59358 = ORIENTED_EDGE ( 'NONE', *, *, #68693, .T. ) ;
#59359 = CARTESIAN_POINT ( 'NONE',  ( 92.35000000000003695, 88.47002178664747873, 79.25791666666667368 ) ) ;
#59360 = EDGE_LOOP ( 'NONE', ( #28303, #52351, #20509, #47627 ) ) ;
#59361 = EDGE_LOOP ( 'NONE', ( #1923, #59583, #64457, #71824 ) ) ;
#59362 = CARTESIAN_POINT ( 'NONE',  ( -92.35000000000003695, 90.00000000000004263, 83.33250000000001023 ) ) ;
#59363 = CIRCLE ( 'NONE', #55767, 16.00000000000000000 ) ;
#59364 = PRESENTATION_STYLE_ASSIGNMENT (( #69890 ) ) ;
#59365 = CARTESIAN_POINT ( 'NONE',  ( -95.00000000000002842, 93.05995642670504253, 82.85625000000000284 ) ) ;
#59366 = VERTEX_POINT ( 'NONE', #54207 ) ;
#59367 = DIRECTION ( 'NONE',  ( 0.2867529058022011967, -0.9580045777625459946, 0.000000000000000000 ) ) ;
#59368 = CARTESIAN_POINT ( 'NONE',  ( 96.32499999999998863, -212.2949673200287179, 83.94104166840097037 ) ) ;
#59369 = CARTESIAN_POINT ( 'NONE',  ( 93.67499999999999716, 87.70503267997126784, 84.39083333333333314 ) ) ;
#59370 = ORIENTED_EDGE ( 'NONE', *, *, #30393, .F. ) ;
#59371 = CARTESIAN_POINT ( 'NONE',  ( 0.000000000000000000, -33.17418723428319538, 17.67226234102814431 ) ) ;
#59372 = CARTESIAN_POINT ( 'NONE',  ( 0.000000000000000000, -6.736453364083817341, 36.88895765772630142 ) ) ;
#59373 = AXIS2_PLACEMENT_3D ( 'NONE', #1067, #46897, #25060 ) ;
#59374 = EDGE_LOOP ( 'NONE', ( #30914, #19142, #19396, #33653 ) ) ;
#59375 = ORIENTED_EDGE ( 'NONE', *, *, #12716, .F. ) ;
#59376 = CARTESIAN_POINT ( 'NONE',  ( -92.69370383062504004, 90.00000000000004263, 88.21406250086714351 ) ) ;
#59377 = VECTOR ( 'NONE', #37342, 1000.000000000000000 ) ;
#59378 = CARTESIAN_POINT ( 'NONE',  ( 97.30629616937498838, 91.33154071421968467, 84.93322916753379559 ) ) ;
#59379 = ORIENTED_EDGE ( 'NONE', *, *, #3699, .F. ) ;
#59380 = CARTESIAN_POINT ( 'NONE',  ( 97.64999999999999147, 90.00000000000002842, 85.95187500173430806 ) ) ;
#59381 =( NAMED_UNIT ( * ) SI_UNIT ( $, .STERADIAN. ) SOLID_ANGLE_UNIT ( ) );
#59382 = ORIENTED_EDGE ( 'NONE', *, *, #25028, .F. ) ;
#59383 = PLANE ( 'NONE',  #21244 ) ;
#59384 = AXIS2_PLACEMENT_3D ( 'NONE', #71992, #60001, #20505 ) ;
#59385 = ORIENTED_EDGE ( 'NONE', *, *, #29089, .T. ) ;
#59386 = ORIENTED_EDGE ( 'NONE', *, *, #29134, .T. ) ;
#59387 = ORIENTED_EDGE ( 'NONE', *, *, #39901, .T. ) ;
#59388 = CARTESIAN_POINT ( 'NONE',  ( -93.26027265873601380, 91.51405112163766375, 74.79348190356853365 ) ) ;
#59390 = CIRCLE ( 'NONE', #16022, 16.00000000000000000 ) ;
#59389 = DIRECTION ( 'NONE',  ( 1.000000000000000000, 0.000000000000000000, 0.000000000000000000 ) ) ;
#59391 = CARTESIAN_POINT ( 'NONE',  ( -97.65000000000001990, 91.52997821335253548, 84.86708333333334053 ) ) ;
#59392 = VERTEX_POINT ( 'NONE', #71469 ) ;
#59393 = DIRECTION ( 'NONE',  ( 0.000000000000000000, 0.000000000000000000, -1.000000000000000000 ) ) ;
#59394 = AXIS2_PLACEMENT_3D ( 'NONE', #22553, #56775, #56015 ) ;
#59395 = CARTESIAN_POINT ( 'NONE',  ( 0.000000000000000000, 55.19960302592066625, 51.03279382321107249 ) ) ;
#59396 = VERTEX_POINT ( 'NONE', #54567 ) ;
#59397 = CARTESIAN_POINT ( 'NONE',  ( 10.00000000000000000, -65.59268652807183742, -36.72794159290312166 ) ) ;
#59398 = CARTESIAN_POINT ( 'NONE',  ( -93.84685191531248449, -208.0026889286704943, 83.08114583420048405 ) ) ;
#59399 = ORIENTED_EDGE ( 'NONE', *, *, #72073, .F. ) ;
#59400 = LINE ( 'NONE', #71764, #41072 ) ;
#59401 = FACE_OUTER_BOUND ( 'NONE', #53990, .T. ) ;
#59402 = DIRECTION ( 'NONE',  ( -1.000000000000000000, 0.000000000000000000, 0.000000000000000000 ) ) ;
#59403 = DIRECTION ( 'NONE',  ( -0.000000000000000000, 0.2079116908177663092, 0.9781476007338041345 ) ) ;
#59404 = CIRCLE ( 'NONE', #12536, 77.49900000000000944 ) ;
#59405 = EDGE_CURVE ( 'NONE', #70390, #40964, #36561, .T. ) ;
#59406 = EDGE_CURVE ( 'NONE', #14986, #6029, #16064, .T. ) ;
#59407 = CARTESIAN_POINT ( 'NONE',  ( -92.35000000000003695, 90.00000000000004263, 79.52249999999999375 ) ) ;
#59408 = CARTESIAN_POINT ( 'NONE',  ( 97.64999999999999147, 90.00000000000002842, 89.04749999999999943 ) ) ;
#59409 = CARTESIAN_POINT ( 'NONE',  ( 96.76339072695076027, -211.4937631030103375, 74.79348190356849102 ) ) ;
#59410 = EDGE_CURVE ( 'NONE', #32352, #32355, #7598, .T. ) ;
#59411 = LINE ( 'NONE', #58296, #68743 ) ;
#59412 = DIRECTION ( 'NONE',  ( 1.000000000000000000, 0.000000000000000000, 0.000000000000000000 ) ) ;
#59413 = CARTESIAN_POINT ( 'NONE',  ( -97.30629616937501680, 91.33154071421968467, 74.98489583420048632 ) ) ;
#59414 = DIRECTION ( 'NONE',  ( -1.000000000000000000, 0.000000000000000000, 0.000000000000000000 ) ) ;
#59415 = CARTESIAN_POINT ( 'NONE',  ( -10.00000000000000000, 0.000000000000000000, 0.000000000000000000 ) ) ;
#59416 = DIRECTION ( 'NONE',  ( 0.000000000000000000, 0.000000000000000000, 1.000000000000000000 ) ) ;
#59417 = EDGE_CURVE ( 'NONE', #51295, #32186, #1632, .T. ) ;
#59418 = CARTESIAN_POINT ( 'NONE',  ( 92.34999999999999432, 90.00000000000002842, 90.00000000000000000 ) ) ;
#59419 = CARTESIAN_POINT ( 'NONE',  ( 0.000000000000000000, 0.000000000000000000, 0.000000000000000000 ) ) ;
#59420 = AXIS2_PLACEMENT_3D ( 'NONE', #46154, #1068, #69086 ) ;
#59421 = DIRECTION ( 'NONE',  ( -0.4796670183876317051, 0.8774505977381971134, 0.000000000000000000 ) ) ;
#59422 = DIRECTION ( 'NONE',  ( 1.000000000000000000, 0.000000000000000000, 0.000000000000000000 ) ) ;
#59423 = CARTESIAN_POINT ( 'NONE',  ( 2.117611129180199558, -93.54218975225703048, -2.500000000000000444 ) ) ;
#59424 = CARTESIAN_POINT ( 'NONE',  ( -97.64999999999996305, -209.9999999999999716, 86.82500000000000284 ) ) ;
#59425 = CARTESIAN_POINT ( 'NONE',  ( 4.999999999999999112, -2.417244626924488049, -5.688952927922135139 ) ) ;
#59426 = EDGE_CURVE ( 'NONE', #53644, #45497, #53822, .T. ) ;
#59427 = ORIENTED_EDGE ( 'NONE', *, *, #50339, .F. ) ;
#59428 = VECTOR ( 'NONE', #73658, 1000.000000000000114 ) ;
#59429 = CARTESIAN_POINT ( 'NONE',  ( -92.34999999999999432, -209.9999999999999716, 90.00000000000000000 ) ) ;
#59430 = EDGE_CURVE ( 'NONE', #58523, #62043, #46821, .T. ) ;
#59431 = CIRCLE ( 'NONE', #53475, 77.49900000000002365 ) ;
#59432 = DIRECTION ( 'NONE',  ( -1.000000000000000000, -0.000000000000000000, 0.000000000000000000 ) ) ;
#59433 = CARTESIAN_POINT ( 'NONE',  ( 0.000000000000000000, 30.80686688397041451, -21.53537804866048688 ) ) ;
#59434 = CARTESIAN_POINT ( 'NONE',  ( 10.00000000000000000, -63.18004540533059554, 44.88180994100355292 ) ) ;
#59435 = EDGE_CURVE ( 'NONE', #45705, #40611, #47450, .T. ) ;
#59437 = EDGE_CURVE ( 'NONE', #63900, #39587, #19237, .T. ) ;
#59436 = AXIS2_PLACEMENT_3D ( 'NONE', #6550, #24215, #64808 ) ;
#59438 = CIRCLE ( 'NONE', #55838, 77.49899999999999523 ) ;
#59439 = ORIENTED_EDGE ( 'NONE', *, *, #60185, .F. ) ;
#59440 = CARTESIAN_POINT ( 'NONE',  ( 6.000000000000000000, -16.65972982744876774, -80.28980883073775487 ) ) ;
#59441 = EDGE_CURVE ( 'NONE', #15614, #41879, #18862, .T. ) ;
#59442 = FACE_OUTER_BOUND ( 'NONE', #52694, .T. ) ;
#59443 = VERTEX_POINT ( 'NONE', #13232 ) ;
#59444 = CARTESIAN_POINT ( 'NONE',  ( 97.30629616937498838, -209.9999999999999716, 84.88031250086713442 ) ) ;
#59445 = CARTESIAN_POINT ( 'NONE',  ( 92.69370383062501162, -209.9999999999999716, 88.53156250086716739 ) ) ;
#59446 = ORIENTED_EDGE ( 'NONE', *, *, #36143, .F. ) ;
#59447 = VECTOR ( 'NONE', #72411, 1000.000000000000000 ) ;
#59448 = DIRECTION ( 'NONE',  ( 0.000000000000000000, -0.9510565162951565288, 0.3090169943749384029 ) ) ;
#59449 = EDGE_CURVE ( 'NONE', #4529, #3167, #65398, .T. ) ;
#59450 = EDGE_LOOP ( 'NONE', ( #33763, #56640, #20365, #34185 ) ) ;
#59451 = CARTESIAN_POINT ( 'NONE',  ( 12.00000000000000000, 18.84667830672579569, -18.68964196561269375 ) ) ;
#59452 = EDGE_LOOP ( 'NONE', ( #28010, #20253, #22754, #21410, #60877 ) ) ;
#59453 = CARTESIAN_POINT ( 'NONE',  ( -97.30629616937501680, 90.00000000000004263, 80.27656250086714351 ) ) ;
#59454 = ORIENTED_EDGE ( 'NONE', *, *, #651, .F. ) ;
#59455 = VECTOR ( 'NONE', #33984, 1000.000000000000000 ) ;
#59456 = ORIENTED_EDGE ( 'NONE', *, *, #1490, .F. ) ;
#59457 = CARTESIAN_POINT ( 'NONE',  ( -22.53294031248082163, -134.0273518838794757, 5.500000000000000000 ) ) ;
#59458 = ORIENTED_EDGE ( 'NONE', *, *, #28596, .T. ) ;
#59459 = CYLINDRICAL_SURFACE ( 'NONE', #58133, 77.49899999999999523 ) ;
#59460 = CARTESIAN_POINT ( 'NONE',  ( 95.00000000000000000, -213.0599564267049857, 79.36374999999996760 ) ) ;
#59461 = VERTEX_POINT ( 'NONE', #20350 ) ;
#59462 = DIRECTION ( 'NONE',  ( -0.000000000000000000, -0.000000000000000000, 1.000000000000000000 ) ) ;
#59463 = VECTOR ( 'NONE', #49889, 1000.000000000000114 ) ;
#59464 = VERTEX_POINT ( 'NONE', #43310 ) ;
#59465 = LINE ( 'NONE', #7948, #1274 ) ;
#59466 = ORIENTED_EDGE ( 'NONE', *, *, #35721, .T. ) ;
#59467 = EDGE_LOOP ( 'NONE', ( #34156, #63067, #8890, #69183 ) ) ;
#59468 = ORIENTED_EDGE ( 'NONE', *, *, #38685, .F. ) ;
#59469 = CARTESIAN_POINT ( 'NONE',  ( 92.69370383062501162, -209.9999999999999716, 76.94281250086713442 ) ) ;
#59470 = CARTESIAN_POINT ( 'NONE',  ( 10.00000000000000000, -37.58145647212453611, -0.6853352020794456489 ) ) ;
#59471 = AXIS2_PLACEMENT_3D ( 'NONE', #31349, #54300, #71569 ) ;
#59472 = ITEM_DEFINED_TRANSFORMATION ( 'NONE', 'NONE', #5180,  #43395 ) ;
#59473 = CARTESIAN_POINT ( 'NONE',  ( 10.00000000000000178, 0.000000000000000000, 0.000000000000000000 ) ) ;
#59474 = ORIENTED_EDGE ( 'NONE', *, *, #71200, .F. ) ;
#59475 = CYLINDRICAL_SURFACE ( 'NONE', #20856, 16.00000000000000000 ) ;
#59476 = DIRECTION ( 'NONE',  ( -1.000000000000000000, -0.000000000000000000, -0.000000000000000000 ) ) ;
#59477 = CARTESIAN_POINT ( 'NONE',  ( -92.34999999999999432, -210.0000085086564070, 88.49187470744925577 ) ) ;
#59478 = LINE ( 'NONE', #2743, #13088 ) ;
#59479 = CARTESIAN_POINT ( 'NONE',  ( -93.84685191531247028, -211.9973110713294489, 80.96447916753380980 ) ) ;
#59480 = CARTESIAN_POINT ( 'NONE',  ( -96.15314808468752972, 91.99731107132950569, 77.63072916753381492 ) ) ;
#59481 = ORIENTED_EDGE ( 'NONE', *, *, #27061, .T. ) ;
#59482 = CARTESIAN_POINT ( 'NONE',  ( 94.99999999999998579, 92.66308142843935514, 81.22906250086715829 ) ) ;
#59483 = VERTEX_POINT ( 'NONE', #7956 ) ;
#59485 = CIRCLE ( 'NONE', #9026, 77.49899999999999523 ) ;
#59484 = DIRECTION ( 'NONE',  ( 0.08130631524009970801, -0.9966891607226786576, 0.000000000000000000 ) ) ;
#59486 = CARTESIAN_POINT ( 'NONE',  ( -92.35000000010064980, -209.9999769027738239, 83.41187580057901130 ) ) ;
#59487 = AXIS2_PLACEMENT_3D ( 'NONE', #20465, #37010, #59964 ) ;
#59488 = DIRECTION ( 'NONE',  ( 1.000000000000000000, 0.000000000000000000, 0.000000000000000000 ) ) ;
#59489 = CARTESIAN_POINT ( 'NONE',  ( 10.00000000000000000, 0.000000000000000000, 0.000000000000000000 ) ) ;
#59490 = CARTESIAN_POINT ( 'NONE',  ( -96.15314808468745866, -211.9973110713294489, 84.66864583420047552 ) ) ;
#59491 = EDGE_CURVE ( 'NONE', #71738, #14718, #60228, .T. ) ;
#59492 = CARTESIAN_POINT ( 'NONE',  ( 0.000000000000000000, 6.903761155837791819, 77.19088730480525840 ) ) ;
#59493 = LINE ( 'NONE', #7984, #59509 ) ;
#59494 = VECTOR ( 'NONE', #2611, 1000.000000000000000 ) ;
#59495 = DIRECTION ( 'NONE',  ( -1.000000000000000000, -0.000000000000000000, 0.000000000000000000 ) ) ;
#59496 = EDGE_LOOP ( 'NONE', ( #13105, #50084, #9352, #57798 ) ) ;
#59497 = EDGE_CURVE ( 'NONE', #18411, #56810, #71373, .T. ) ;
#59498 = VERTEX_POINT ( 'NONE', #13599 ) ;
#59499 = CARTESIAN_POINT ( 'NONE',  ( 0.000000000000000000, 41.91543099594818500, 2.663952781846294915 ) ) ;
#59500 = AXIS2_PLACEMENT_3D ( 'NONE', #52099, #46465, #69390 ) ;
#59501 = EDGE_CURVE ( 'NONE', #60926, #9559, #61806, .T. ) ;
#59502 = EDGE_CURVE ( 'NONE', #18143, #49623, #6574, .T. ) ;
#59503 = CARTESIAN_POINT ( 'NONE',  ( -97.65000000000001990, 90.00000000000004263, 76.03000000000000114 ) ) ;
#59504 = DIRECTION ( 'NONE',  ( -1.000000000000000000, -0.000000000000000000, 0.000000000000000000 ) ) ;
#59505 = CARTESIAN_POINT ( 'NONE',  ( -96.15314808468751551, 88.00268892867056536, 84.03364583420047040 ) ) ;
#59506 = CYLINDRICAL_SURFACE ( 'NONE', #46603, 16.00000000000000000 ) ;
#59507 = DIRECTION ( 'NONE',  ( -1.000000000000000000, 3.061616997868382648E-16, 0.000000000000000000 ) ) ;
#59508 = DIRECTION ( 'NONE',  ( -1.000000000000000000, -0.000000000000000000, -0.000000000000000000 ) ) ;
#59509 = VECTOR ( 'NONE', #46365, 1000.000000000000000 ) ;
#59510 = CARTESIAN_POINT ( 'NONE',  ( 12.00000000000000000, -4.261787119644964150, 26.19803753235780164 ) ) ;
#59511 = ORIENTED_EDGE ( 'NONE', *, *, #41231, .T. ) ;
#59512 = CARTESIAN_POINT ( 'NONE',  ( -92.69370383062502583, 88.66845928578038638, 76.57239583420046358 ) ) ;
#59513 = VECTOR ( 'NONE', #44135, 1000.000000000000000 ) ;
#59514 = DIRECTION ( 'NONE',  ( 0.000000000000000000, -0.6494480483301904306, 0.7604059656000252687 ) ) ;
#59515 = CARTESIAN_POINT ( 'NONE',  ( 6.000000000000000000, -76.69515212745996280, -29.01471420065643869 ) ) ;
#59516 = FACE_OUTER_BOUND ( 'NONE', #61316, .T. ) ;
#59518 = CARTESIAN_POINT ( 'NONE',  ( 0.000000000000000000, -8.966570791701281351, 81.50828551894223040 ) ) ;
#59517 =( GEOMETRIC_REPRESENTATION_CONTEXT ( 3 ) GLOBAL_UNCERTAINTY_ASSIGNED_CONTEXT ( ( #25565 ) ) GLOBAL_UNIT_ASSIGNED_CONTEXT ( ( #13293, #12550, #59539 ) ) REPRESENTATION_CONTEXT ( 'NONE', 'WORKASPACE' ) );
#59519 = ADVANCED_FACE ( 'NONE', ( #65853 ), #31258, .F. ) ;
#59520 = CARTESIAN_POINT ( 'NONE',  ( 97.64999999999999147, -209.9999999999999716, 82.69749999999999091 ) ) ;
#59521 = CARTESIAN_POINT ( 'NONE',  ( -97.30629616937497417, -208.6684592857803011, 83.39864583420050792 ) ) ;
#59522 =( NAMED_UNIT ( * ) SI_UNIT ( $, .STERADIAN. ) SOLID_ANGLE_UNIT ( ) );
#59523 = EDGE_CURVE ( 'NONE', #9512, #44823, #21833, .T. ) ;
#59524 = CARTESIAN_POINT ( 'NONE',  ( 10.00000000000000000, 30.84782396557248418, -21.32104025579081252 ) ) ;
#59525 = CARTESIAN_POINT ( 'NONE',  ( 10.00000000000000000, 60.67117009219136037, 55.16347631943062879 ) ) ;
#59526 = CARTESIAN_POINT ( 'NONE',  ( -92.69370383062498320, -208.6684592857803295, 78.10697916753383652 ) ) ;
#59527 = CARTESIAN_POINT ( 'NONE',  ( 10.00000000000000000, 0.000000000000000000, 0.000000000000000000 ) ) ;
#59528 = ORIENTED_EDGE ( 'NONE', *, *, #59699, .F. ) ;
#59529 = DIRECTION ( 'NONE',  ( 4.476705744456277943E-17, -1.000000000000000000, 0.000000000000000000 ) ) ;
#59530 = DIRECTION ( 'NONE',  ( 0.000000000000000000, 0.000000000000000000, 1.000000000000000000 ) ) ;
#59531 = CARTESIAN_POINT ( 'NONE',  ( -93.67500000000003979, 87.70503267997129626, 88.38604166840097776 ) ) ;
#59532 = EDGE_CURVE ( 'NONE', #37729, #12399, #15033, .T. ) ;
#59533 = EDGE_CURVE ( 'NONE', #73701, #45157, #21442, .T. ) ;
#59534 = DIRECTION ( 'NONE',  ( 0.000000000000000000, 0.000000000000000000, 1.000000000000000000 ) ) ;
#59535 = CARTESIAN_POINT ( 'NONE',  ( 93.84685191531251292, -211.9973110713294489, 88.00239583420048461 ) ) ;
#59536 = ORIENTED_EDGE ( 'NONE', *, *, #61458, .F. ) ;
#59537 = CARTESIAN_POINT ( 'NONE',  ( 12.00000000000000000, -11.95096189432345746, -23.69967320028757030 ) ) ;
#59538 = FACE_OUTER_BOUND ( 'NONE', #51402, .T. ) ;
#59539 =( NAMED_UNIT ( * ) SI_UNIT ( $, .STERADIAN. ) SOLID_ANGLE_UNIT ( ) );
#59540 = ORIENTED_EDGE ( 'NONE', *, *, #15374, .F. ) ;
#59541 = CARTESIAN_POINT ( 'NONE',  ( 16.84844760790522855, -103.5491698323862124, 5.500000000000000000 ) ) ;
#59542 = AXIS2_PLACEMENT_3D ( 'NONE', #18878, #65875, #3469 ) ;
#59543 = ORIENTED_EDGE ( 'NONE', *, *, #34376, .T. ) ;
#59544 = CARTESIAN_POINT ( 'NONE',  ( 10.00000000000000000, 0.000000000000000000, 0.000000000000000000 ) ) ;
#59545 = VECTOR ( 'NONE', #68255, 1000.000000000000000 ) ;
#59546 = ORIENTED_EDGE ( 'NONE', *, *, #30115, .F. ) ;
#59547 = ORIENTED_EDGE ( 'NONE', *, *, #22425, .T. ) ;
#59548 = ORIENTED_EDGE ( 'NONE', *, *, #28166, .T. ) ;
#59549 = FACE_OUTER_BOUND ( 'NONE', #34578, .T. ) ;
#59550 = ORIENTED_EDGE ( 'NONE', *, *, #25125, .T. ) ;
#59551 = PRODUCT ( 'housing cover', 'housing cover', '', ( #28664 ) ) ;
#59552 = VECTOR ( 'NONE', #25381, 1000.000000000000114 ) ;
#59553 = EDGE_LOOP ( 'NONE', ( #1140, #33656, #72238, #13496 ) ) ;
#59554 =( BOUNDED_CURVE ( )  B_SPLINE_CURVE ( 2, ( #6847, #23405, #881, #23769, #69631, #13221, #41069, #35772, #24153 ),
 .UNSPECIFIED., .F., .F. ) 
 B_SPLINE_CURVE_WITH_KNOTS ( ( 3, 2, 2, 2, 3 ),
 ( 0.5715170088666295944, 0.5785727743523535471, 0.5856285398932350450, 0.5926843054341166539, 0.5926843883797353607 ),
 .UNSPECIFIED. ) 
 CURVE ( )  GEOMETRIC_REPRESENTATION_ITEM ( )  RATIONAL_B_SPLINE_CURVE ( ( 1.000000000000000000, 0.8660254037844387076, 1.000000000000000000, 0.8660254037844387076, 1.000000000000000000, 0.8660254037844387076, 1.000000000000000000, 0.9999984250318816326, 0.9999968501007930888 ) ) 
 REPRESENTATION_ITEM ( '' )  );
#59555 = CARTESIAN_POINT ( 'NONE',  ( 92.69370383062498320, 91.33154071421968467, 78.31864583420050963 ) ) ;
#59556 = PLANE ( 'NONE',  #68425 ) ;
#59557 = DIRECTION ( 'NONE',  ( 0.000000000000000000, -0.9510565162951499785, -0.3090169943749582204 ) ) ;
#59558 = EDGE_LOOP ( 'NONE', ( #59968, #35133 ) ) ;
#59559 = VERTEX_POINT ( 'NONE', #44779 ) ;
#59560 = EDGE_LOOP ( 'NONE', ( #31511, #17872, #61386, #1030 ) ) ;
#59561 = CYLINDRICAL_SURFACE ( 'NONE', #25071, 11.59999999999999964 ) ;
#59562 = VERTEX_POINT ( 'NONE', #4192 ) ;
#59563 = DIRECTION ( 'NONE',  ( 1.000000000000000000, 0.000000000000000000, 0.000000000000000000 ) ) ;
#59564 = CARTESIAN_POINT ( 'NONE',  ( 11.59999999999999787, 1.420590287010929336E-15, 40.80000000000001847 ) ) ;
#59565 = AXIS2_PLACEMENT_3D ( 'NONE', #37256, #54532, #65822 ) ;
#59566 = CARTESIAN_POINT ( 'NONE',  ( -93.59478774260956868, 91.86781405990323890, 74.80441578173237360 ) ) ;
#59567 = DIRECTION ( 'NONE',  ( 0.000000000000000000, -0.000000000000000000, 1.000000000000000000 ) ) ;
#59568 = CARTESIAN_POINT ( 'NONE',  ( 6.250000000000005329, 3.980102097228899218E-16, 3.250000000000001332 ) ) ;
#59569 = DIRECTION ( 'NONE',  ( 0.000000000000000000, -0.1564344650402381687, 0.9876883405951365491 ) ) ;
#59570 = CARTESIAN_POINT ( 'NONE',  ( 11.99999999999999822, 81.96053171279901051, -2.543863470248673764 ) ) ;
#59571 = CARTESIAN_POINT ( 'NONE',  ( -94.99999999999997158, -213.0599564267049857, 76.90312500173429555 ) ) ;
#59572 = CARTESIAN_POINT ( 'NONE',  ( -96.15314808468751551, 88.00268892867056536, 89.27239583420049485 ) ) ;
#59574 = CARTESIAN_POINT ( 'NONE',  ( -92.35000000000003695, 90.00000000000004263, 75.79187500173429726 ) ) ;
#59573 = CARTESIAN_POINT ( 'NONE',  ( 97.64999999999999147, 90.00000000000002842, 75.79187500173429726 ) ) ;
#59575 = ORIENTED_EDGE ( 'NONE', *, *, #5179, .F. ) ;
#59576 = CARTESIAN_POINT ( 'NONE',  ( 92.69370383062498320, 90.00000000000002842, 77.73656250086715147 ) ) ;
#59577 = PLANE ( 'NONE',  #55339 ) ;
#59578 = CARTESIAN_POINT ( 'NONE',  ( 0.000000000000000000, 33.00180498840046539, 17.80606268964551120 ) ) ;
#59579 = CYLINDRICAL_SURFACE ( 'NONE', #23952, 16.00000000000000000 ) ;
#59580 = EDGE_CURVE ( 'NONE', #71482, #16336, #4939, .T. ) ;
#59581 = CARTESIAN_POINT ( 'NONE',  ( -97.64999999989191792, -209.9999848944890175, 78.64888723590522090 ) ) ;
#59582 = LINE ( 'NONE', #12956, #47423 ) ;
#59583 = ORIENTED_EDGE ( 'NONE', *, *, #3502, .T. ) ;
#59584 = EDGE_CURVE ( 'NONE', #66872, #56256, #72214, .T. ) ;
#59585 = CARTESIAN_POINT ( 'NONE',  ( 11.41210121379328335, -99.40233154247455616, -5.500000000000000000 ) ) ;
#59586 = LINE ( 'NONE', #52838, #4792 ) ;
#59587 = ORIENTED_EDGE ( 'NONE', *, *, #65721, .T. ) ;
#59588 = ADVANCED_FACE ( 'NONE', ( #3455 ), #56045, .F. ) ;
#59589 = VERTEX_POINT ( 'NONE', #20717 ) ;
#59590 = EDGE_CURVE ( 'NONE', #52067, #27833, #26717, .T. ) ;
#59591 = DIRECTION ( 'NONE',  ( 1.000000000000000000, 0.000000000000000000, 0.000000000000000000 ) ) ;
#59592 = CARTESIAN_POINT ( 'NONE',  ( 0.000000000000000000, -74.65491531819111515, 23.16904090965678265 ) ) ;
#59593 = CARTESIAN_POINT ( 'NONE',  ( 93.67500000000001137, -207.7050326799711968, 88.06854166840095388 ) ) ;
#59594 = DIRECTION ( 'NONE',  ( 0.000000000000000000, 0.000000000000000000, 1.000000000000000000 ) ) ;
#59595 = DIRECTION ( 'NONE',  ( 1.000000000000000000, 0.000000000000000000, 0.000000000000000000 ) ) ;
#59596 = CARTESIAN_POINT ( 'NONE',  ( 96.32499999999998863, 87.70503267997126784, 84.49666666666666970 ) ) ;
#59597 = EDGE_CURVE ( 'NONE', #37548, #57064, #4226, .T. ) ;
#59598 = AXIS2_PLACEMENT_3D ( 'NONE', #32376, #38030, #60960 ) ;
#59599 = ORIENTED_EDGE ( 'NONE', *, *, #21457, .T. ) ;
#59600 = DIRECTION ( 'NONE',  ( -1.000000000000000000, -0.000000000000000000, -0.000000000000000000 ) ) ;
#59601 = DIRECTION ( 'NONE',  ( 0.000000000000000000, 0.000000000000000000, 1.000000000000000000 ) ) ;
#59602 = CARTESIAN_POINT ( 'NONE',  ( 97.65000000000000568, 88.47002178664752137, 85.89895833506763267 ) ) ;
#59603 = CIRCLE ( 'NONE', #54808, 30.50000000000000000 ) ;
#59604 = FACE_OUTER_BOUND ( 'NONE', #12263, .T. ) ;
#59605 = DIRECTION ( 'NONE',  ( 0.9580045777625458836, 0.2867529058022011412, -0.000000000000000000 ) ) ;
#59606 = CARTESIAN_POINT ( 'NONE',  ( -10.00000000000000000, 0.000000000000000000, 0.000000000000000000 ) ) ;
#59608 = AXIS2_PLACEMENT_3D ( 'NONE', #14649, #60535, #62015 ) ;
#59607 = PRODUCT_DEFINITION_CONTEXT ( 'detailed design', #12386, 'design' ) ;
#59609 = DIRECTION ( 'NONE',  ( 1.000000000000000000, 1.427937372958405461E-15, 7.962523111839130290E-16 ) ) ;
#59610 = EDGE_CURVE ( 'NONE', #26168, #29955, #66593, .T. ) ;
#59611 = DIRECTION ( 'NONE',  ( -1.000000000000000000, 0.000000000000000000, 0.000000000000000000 ) ) ;
#59612 = EDGE_CURVE ( 'NONE', #64725, #62043, #38757, .T. ) ;
#59613 = CIRCLE ( 'NONE', #23593, 20.20000000000036522 ) ;
#59614 = AXIS2_PLACEMENT_3D ( 'NONE', #63580, #53393, #47019 ) ;
#59615 = CARTESIAN_POINT ( 'NONE',  ( 93.84685191531248449, 88.00268892867053694, 84.82739583420048746 ) ) ;
#59616 = CARTESIAN_POINT ( 'NONE',  ( -96.15314808468745866, -211.9973110713294489, 86.73239583420048859 ) ) ;
#59617 = DIRECTION ( 'NONE',  ( -1.000000000000000000, 0.000000000000000000, 0.000000000000000000 ) ) ;
#59618 = ORIENTED_EDGE ( 'NONE', *, *, #4778, .F. ) ;
#59619 = FACE_OUTER_BOUND ( 'NONE', #60209, .T. ) ;
#59620 = CARTESIAN_POINT ( 'NONE',  ( -97.64999999999994884, -208.4700217866474645, 81.69208333333332916 ) ) ;
#59621 = CARTESIAN_POINT ( 'NONE',  ( -97.30629616937501680, 88.66845928578038638, 75.09072916753380866 ) ) ;
#59622 = ADVANCED_FACE ( 'NONE', ( #10544 ), #37657, .T. ) ;
#59623 = EDGE_CURVE ( 'NONE', #61584, #11957, #61851, .T. ) ;
#59624 = VECTOR ( 'NONE', #50369, 1000.000000000000000 ) ;
#59625 = CARTESIAN_POINT ( 'NONE',  ( 96.15314808468750130, -211.9973110713294489, 84.13947916753380696 ) ) ;
#59626 = ORIENTED_EDGE ( 'NONE', *, *, #14957, .T. ) ;
#59627 = ORIENTED_EDGE ( 'NONE', *, *, #27213, .F. ) ;
#59628 = ORIENTED_EDGE ( 'NONE', *, *, #14075, .T. ) ;
#59629 = CARTESIAN_POINT ( 'NONE',  ( 92.69370383062498320, 90.00000000000002842, 89.80156250086714920 ) ) ;
#59630 = DIRECTION ( 'NONE',  ( 0.000000000000000000, 0.000000000000000000, -1.000000000000000000 ) ) ;
#59631 = ORIENTED_EDGE ( 'NONE', *, *, #12391, .T. ) ;
#59632 = FACE_OUTER_BOUND ( 'NONE', #30594, .T. ) ;
#59633 = CARTESIAN_POINT ( 'NONE',  ( 97.30629616937498838, -208.6684592857803295, 80.01197916753382344 ) ) ;
#59634 = DIRECTION ( 'NONE',  ( 0.000000000000000000, 0.3090169943749410120, 0.9510565162951556406 ) ) ;
#59635 = CARTESIAN_POINT ( 'NONE',  ( 11.99999999999999822, -44.88180994100419952, 63.18004540533013369 ) ) ;
#59636 = CARTESIAN_POINT ( 'NONE',  ( 96.32499999999998863, -212.2949673200287179, 80.68666666666665321 ) ) ;
#59637 = CARTESIAN_POINT ( 'NONE',  ( 10.00000000000000000, 49.70050353004889132, 59.46389618801982380 ) ) ;
#59638 = AXIS2_PLACEMENT_3D ( 'NONE', #21091, #15088, #10562 ) ;
#59639 = FACE_OUTER_BOUND ( 'NONE', #9857, .T. ) ;
#59640 = CARTESIAN_POINT ( 'NONE',  ( 92.35000000000002274, -211.5299782133524502, 81.16291666666666060 ) ) ;
#59641 = EDGE_CURVE ( 'NONE', #44992, #68450, #51055, .T. ) ;
#59642 = ORIENTED_EDGE ( 'NONE', *, *, #36187, .F. ) ;
#59643 = ORIENTED_EDGE ( 'NONE', *, *, #66787, .T. ) ;
#59644 = EDGE_LOOP ( 'NONE', ( #20055, #72183, #29792, #6659 ) ) ;
#59645 = ORIENTED_EDGE ( 'NONE', *, *, #48239, .T. ) ;
#59646 = DIRECTION ( 'NONE',  ( -1.000000000000000000, 0.000000000000000000, 0.000000000000000000 ) ) ;
#59647 =( NAMED_UNIT ( * ) SI_UNIT ( $, .STERADIAN. ) SOLID_ANGLE_UNIT ( ) );
#59648 = CARTESIAN_POINT ( 'NONE',  ( -97.30629616937501680, 90.00000000000004263, 84.72156250086715090 ) ) ;
#59649 = VECTOR ( 'NONE', #3247, 1000.000000000000000 ) ;
#59650 = CARTESIAN_POINT ( 'NONE',  ( -97.64999999992180335, 90.00001303125199570, 79.28395951162846700 ) ) ;
#59651 = ADVANCED_FACE ( 'NONE', ( #9437, #32362, #15829, #55305, #3822 ), #61694, .T. ) ;
#59652 = AXIS2_PLACEMENT_3D ( 'NONE', #62635, #69001, #28387 ) ;
#59653 = DIRECTION ( 'NONE',  ( -1.000000000000000000, -0.000000000000000000, -0.000000000000000000 ) ) ;
#59654 = CARTESIAN_POINT ( 'NONE',  ( 92.34999999999999432, 88.47002178664753558, 76.71791666666666742 ) ) ;
#59655 = ADVANCED_FACE ( 'NONE', ( #61329 ), #9810, .T. ) ;
#59656 = ORIENTED_EDGE ( 'NONE', *, *, #69316, .T. ) ;
#59657 = DIRECTION ( 'NONE',  ( -1.000000000000000000, -0.000000000000000000, -0.000000000000000000 ) ) ;
#59658 = ORIENTED_EDGE ( 'NONE', *, *, #37848, .T. ) ;
#59659 = DIRECTION ( 'NONE',  ( -1.000000000000000000, 0.000000000000000000, -0.000000000000000000 ) ) ;
#59660 = VECTOR ( 'NONE', #34173, 1000.000000000000000 ) ;
#59662 = ORIENTED_EDGE ( 'NONE', *, *, #72039, .F. ) ;
#59661 = EDGE_CURVE ( 'NONE', #3905, #3810, #40216, .T. ) ;
#59663 = CARTESIAN_POINT ( 'NONE',  ( -93.67500000000003979, 92.29496732002878900, 86.69270833506763552 ) ) ;
#59664 = CARTESIAN_POINT ( 'NONE',  ( 93.84685191531248449, 91.99731107132950569, 88.42572916753381662 ) ) ;
#59665 = DIRECTION ( 'NONE',  ( -0.000000000000000000, -0.000000000000000000, 1.000000000000000000 ) ) ;
#59666 = ADVANCED_FACE ( 'NONE', ( #16944 ), #431, .T. ) ;
#59667 = LINE ( 'NONE', #43864, #72181 ) ;
#59668 = CARTESIAN_POINT ( 'NONE',  ( 11.99999999999999822, -65.59268652807237743, 36.72794159290217664 ) ) ;
#59669 = CYLINDRICAL_SURFACE ( 'NONE', #36079, 77.49899999999999523 ) ;
#59670 = ORIENTED_EDGE ( 'NONE', *, *, #71088, .T. ) ;
#59671 = DIRECTION ( 'NONE',  ( 0.000000000000000000, 0.000000000000000000, 1.000000000000000000 ) ) ;
#59672 = FACE_BOUND ( 'NONE', #506, .T. ) ;
#59673 = ORIENTED_EDGE ( 'NONE', *, *, #36742, .F. ) ;
#59674 = AXIS2_PLACEMENT_3D ( 'NONE', #34851, #29557, #63808 ) ;
#59675 = ADVANCED_FACE ( 'NONE', ( #74069 ), #68455, .T. ) ;
#59676 = ORIENTED_EDGE ( 'NONE', *, *, #64085, .T. ) ;
#59677 = CARTESIAN_POINT ( 'NONE',  ( 11.99999999999999822, 0.000000000000000000, 0.000000000000000000 ) ) ;
#59678 = VECTOR ( 'NONE', #52805, 1000.000000000000000 ) ;
#59679 = DIRECTION ( 'NONE',  ( 1.000000000000000000, 0.000000000000000000, 0.000000000000000000 ) ) ;
#59680 = DIRECTION ( 'NONE',  ( 3.035766082959412415E-16, 1.000000000000000000, 0.000000000000000000 ) ) ;
#59681 = CARTESIAN_POINT ( 'NONE',  ( -92.69370383062498320, -209.9999999999999716, 83.76906250086716454 ) ) ;
#59682 = EDGE_LOOP ( 'NONE', ( #36439, #30467, #14683, #4360 ) ) ;
#59683 = EDGE_CURVE ( 'NONE', #62137, #16267, #71425, .T. ) ;
#59684 = LINE ( 'NONE', #48762, #42898 ) ;
#59685 = VERTEX_POINT ( 'NONE', #29314 ) ;
#59686 = ORIENTED_EDGE ( 'NONE', *, *, #2905, .T. ) ;
#59687 = DIRECTION ( 'NONE',  ( 0.000000000000000000, -0.3090169943749449533, -0.9510565162951543083 ) ) ;
#59688 = CARTESIAN_POINT ( 'NONE',  ( 96.15314808468748708, 91.99731107132950569, 89.58989583420049030 ) ) ;
#59689 = CARTESIAN_POINT ( 'NONE',  ( 0.000000000000000000, 0.000000000000000000, 0.000000000000000000 ) ) ;
#59690 = CARTESIAN_POINT ( 'NONE',  ( 96.15314808468748708, 91.99731107132950569, 79.90614583420047268 ) ) ;
#59691 = B_SPLINE_CURVE_WITH_KNOTS ( 'NONE', 3,
 ( #60416, #37849, #15273, #19795, #9264, #19425, #54760, #42741 ),
 .UNSPECIFIED., .F., .F.,
 ( 4, 2, 2, 4 ),
 ( 0.001653806717454685358, 0.002539064216007148531, 0.002981692965283379900, 0.003424321714559611270 ),
 .UNSPECIFIED. ) ;
#59692 = CARTESIAN_POINT ( 'NONE',  ( 0.000000000000000000, 0.000000000000000000, -0.3501037691048548561 ) ) ;
#59693 = CARTESIAN_POINT ( 'NONE',  ( 0.000000000000000000, -25.88420570971381807, -27.13269053701123212 ) ) ;
#59694 = CARTESIAN_POINT ( 'NONE',  ( 0.000000000000000000, 70.52718814184260054, 26.02418014898334420 ) ) ;
#59695 = CARTESIAN_POINT ( 'NONE',  ( -2.500000000000000000, 16.00000000000000000, -19.01812422950394676 ) ) ;
#59696 = CARTESIAN_POINT ( 'NONE',  ( 10.00000000000000000, 6.736453364083557105, 36.88895765772635826 ) ) ;
#59697 = EDGE_CURVE ( 'NONE', #28744, #39261, #31832, .T. ) ;
#59698 = DIRECTION ( 'NONE',  ( -1.000000000000000000, 0.000000000000000000, 0.000000000000000000 ) ) ;
#59699 = EDGE_CURVE ( 'NONE', #6205, #3726, #33854, .T. ) ;
#59700 = ADVANCED_FACE ( 'NONE', ( #17677 ), #57910, .T. ) ;
#59701 = CIRCLE ( 'NONE', #27255, 16.00000000000000000 ) ;
#59702 = CARTESIAN_POINT ( 'NONE',  ( -93.26027265873587169, -208.4859488783624215, 74.79348190356851944 ) ) ;
#59703 = PRODUCT_DEFINITION_CONTEXT ( 'detailed design', #5718, 'design' ) ;
#59704 = VECTOR ( 'NONE', #16484, 1000.000000000000000 ) ;
#59705 = DIRECTION ( 'NONE',  ( -1.000000000000000000, 0.000000000000000000, 0.000000000000000000 ) ) ;
#59706 = VERTEX_POINT ( 'NONE', #62829 ) ;
#59707 = CARTESIAN_POINT ( 'NONE',  ( -97.30629616937501680, 88.66845928578038638, 86.52072916753381548 ) ) ;
#59708 = DIRECTION ( 'NONE',  ( 0.000000000000000000, 0.000000000000000000, 1.000000000000000000 ) ) ;
#59709 = AXIS2_PLACEMENT_3D ( 'NONE', #19533, #59775, #19900 ) ;
#59710 = VECTOR ( 'NONE', #26494, 1000.000000000000227 ) ;
#59711 = FACE_OUTER_BOUND ( 'NONE', #70580, .T. ) ;
#59712 = CIRCLE ( 'NONE', #24872, 37.49900000000000233 ) ;
#59713 = ORIENTED_EDGE ( 'NONE', *, *, #34310, .T. ) ;
#59714 = LINE ( 'NONE', #7465, #7850 ) ;
#59715 = LINE ( 'NONE', #35652, #8367 ) ;
#59716 = CARTESIAN_POINT ( 'NONE',  ( -97.65000000000001990, 90.00000000000004263, 80.47499999999999432 ) ) ;
#59717 = CARTESIAN_POINT ( 'NONE',  ( 92.69370383062501162, -211.3315407142195852, 83.50447916753383026 ) ) ;
#59718 = VECTOR ( 'NONE', #61210, 1000.000000000000114 ) ;
#59719 = ORIENTED_EDGE ( 'NONE', *, *, #72236, .T. ) ;
#59720 = ORIENTED_EDGE ( 'NONE', *, *, #46373, .T. ) ;
#59721 = VECTOR ( 'NONE', #45231, 1000.000000000000114 ) ;
#59722 = EDGE_CURVE ( 'NONE', #26087, #57460, #11443, .T. ) ;
#59723 = FACE_OUTER_BOUND ( 'NONE', #30378, .T. ) ;
#59724 = ORIENTED_EDGE ( 'NONE', *, *, #41117, .T. ) ;
#59725 = DIRECTION ( 'NONE',  ( -1.000000000000000000, 0.000000000000000000, 0.000000000000000000 ) ) ;
#59726 = CYLINDRICAL_SURFACE ( 'NONE', #46021, 2.649999999999985700 ) ;
#59727 = ORIENTED_EDGE ( 'NONE', *, *, #25697, .F. ) ;
#59728 = LINE ( 'NONE', #43191, #20100 ) ;
#59729 = CARTESIAN_POINT ( 'NONE',  ( 97.30629616937498838, -209.9999999999999716, 81.22906250086715829 ) ) ;
#59730 = ORIENTED_EDGE ( 'NONE', *, *, #3528, .F. ) ;
#59731 = LINE ( 'NONE', #8214, #16736 ) ;
#59732 = ORIENTED_EDGE ( 'NONE', *, *, #8913, .F. ) ;
#59733 = VERTEX_POINT ( 'NONE', #5673 ) ;
#59734 = CARTESIAN_POINT ( 'NONE',  ( 7.103376864691351012E-17, -120.0000000000000000, -80.00000000000000000 ) ) ;
#59735 = DIRECTION ( 'NONE',  ( -1.000000000000000000, -0.000000000000000000, -0.000000000000000000 ) ) ;
#59736 = EDGE_CURVE ( 'NONE', #71078, #12401, #59431, .T. ) ;
#59737 = VERTEX_POINT ( 'NONE', #58271 ) ;
#59738 = LINE ( 'NONE', #55202, #54592 ) ;
#59739 = CARTESIAN_POINT ( 'NONE',  ( 97.64999999999997726, -211.5299782133524502, 84.62895833506763665 ) ) ;
#59740 = CARTESIAN_POINT ( 'NONE',  ( 94.99999999999998579, 86.94004357329500010, 86.34874999999999545 ) ) ;
#59741 = EDGE_CURVE ( 'NONE', #59210, #14718, #23428, .T. ) ;
#59742 = ORIENTED_EDGE ( 'NONE', *, *, #43555, .T. ) ;
#59743 = DIRECTION ( 'NONE',  ( 1.427937372958396981E-15, -1.000000000000000000, 1.065814103640131031E-14 ) ) ;
#59744 = FACE_OUTER_BOUND ( 'NONE', #6922, .T. ) ;
#59745 = ORIENTED_EDGE ( 'NONE', *, *, #40263, .F. ) ;
#59746 = ORIENTED_EDGE ( 'NONE', *, *, #67726, .F. ) ;
#59747 = CARTESIAN_POINT ( 'NONE',  ( -97.30629616937501680, 91.33154071421968467, 87.20864583420048177 ) ) ;
#59748 = CIRCLE ( 'NONE', #66919, 42.00000000000000000 ) ;
#59749 = CARTESIAN_POINT ( 'NONE',  ( 97.30629616937498838, 88.66845928578037217, 80.38239583420049428 ) ) ;
#59750 = ORIENTED_EDGE ( 'NONE', *, *, #11483, .F. ) ;
#59752 = CARTESIAN_POINT ( 'NONE',  ( 97.64999999999997726, 91.52997821335252127, 83.46479166840096298 ) ) ;
#59751 = CIRCLE ( 'NONE', #22558, 31.99999999999998579 ) ;
#59753 = EDGE_CURVE ( 'NONE', #20786, #37729, #18051, .T. ) ;
#59754 = ADVANCED_FACE ( 'NONE', ( #5314 ), #45530, .T. ) ;
#59755 = LINE ( 'NONE', #42828, #69681 ) ;
#59756 = ORIENTED_EDGE ( 'NONE', *, *, #50432, .T. ) ;
#59757 = ORIENTED_EDGE ( 'NONE', *, *, #10687, .F. ) ;
#59758 = VERTEX_POINT ( 'NONE', #51141 ) ;
#59759 = VERTEX_POINT ( 'NONE', #11293 ) ;
#59760 = CIRCLE ( 'NONE', #23735, 26.50000000000552092 ) ;
#59761 = DIRECTION ( 'NONE',  ( 0.000000000000000000, 0.8090169943749487835, -0.5877852522924712497 ) ) ;
#59762 = FACE_OUTER_BOUND ( 'NONE', #37182, .T. ) ;
#59763 = CARTESIAN_POINT ( 'NONE',  ( -97.65000000000001990, 91.52997821335253548, 84.23208333333333542 ) ) ;
#59764 = ORIENTED_EDGE ( 'NONE', *, *, #15505, .T. ) ;
#59765 = CARTESIAN_POINT ( 'NONE',  ( 0.000000000000000000, 3.925862922256160736, 41.81611651403863306 ) ) ;
#59766 =( BOUNDED_CURVE ( )  B_SPLINE_CURVE ( 2, ( #50608, #22421, #44620, #55517, #4782, #67166, #4401, #27295, #50228 ),
 .UNSPECIFIED., .F., .F. ) 
 B_SPLINE_CURVE_WITH_KNOTS ( ( 3, 2, 2, 2, 3 ),
 ( 0.6138516023186938453, 0.6209073675976485296, 0.6279631331385309156, 0.6350188986794131907, 0.6350190250571088324 ),
 .UNSPECIFIED. ) 
 CURVE ( )  GEOMETRIC_REPRESENTATION_ITEM ( )  RATIONAL_B_SPLINE_CURVE ( ( 1.000000000000000000, 0.8660254037844387076, 1.000000000000000000, 0.8660254037844387076, 1.000000000000000000, 0.8660254037844387076, 1.000000000000000000, 0.9999976003453283635, 0.9999952007766184092 ) ) 
 REPRESENTATION_ITEM ( '' )  );
#59767 = DIRECTION ( 'NONE',  ( 1.000000000000000000, 0.000000000000000000, 0.000000000000000000 ) ) ;
#59768 = VERTEX_POINT ( 'NONE', #6765 ) ;
#59769 = CARTESIAN_POINT ( 'NONE',  ( 97.64999999999999147, -209.9999999999999716, 85.23749999999999716 ) ) ;
#59770 = CARTESIAN_POINT ( 'NONE',  ( -97.30629616937497417, -208.6684592857803011, 83.23989583420046756 ) ) ;
#59771 = VERTEX_POINT ( 'NONE', #34226 ) ;
#59773 = EDGE_CURVE ( 'NONE', #38512, #40400, #29658, .T. ) ;
#59772 = DIRECTION ( 'NONE',  ( 1.000000000000000000, 0.000000000000000000, 0.000000000000000000 ) ) ;
#59774 = LINE ( 'NONE', #31184, #24811 ) ;
#59775 = DIRECTION ( 'NONE',  ( -1.000000000000000000, -0.000000000000000000, 0.000000000000000000 ) ) ;
#59776 = DIRECTION ( 'NONE',  ( 0.000000000000000000, 0.000000000000000000, 1.000000000000000000 ) ) ;
#59777 = ADVANCED_BREP_SHAPE_REPRESENTATION ( '', ( #36766, #43395 ), #14652 ) ;
#59778 = CARTESIAN_POINT ( 'NONE',  ( -26.41226275915097332, -122.1546173538626761, -2.500000000000000000 ) ) ;
#59779 = CIRCLE ( 'NONE', #24994, 37.49900000000000944 ) ;
#59780 = SURFACE_STYLE_FILL_AREA ( #36831 ) ;
#59781 = CARTESIAN_POINT ( 'NONE',  ( 6.250000000000005329, 0.000000000000000000, -3.250000000000001332 ) ) ;
#59782 = FACE_OUTER_BOUND ( 'NONE', #19307, .T. ) ;
#59783 = VECTOR ( 'NONE', #32882, 1000.000000000000000 ) ;
#59784 = DIRECTION ( 'NONE',  ( 9.814797785686868941E-17, 1.000000000000000000, -0.000000000000000000 ) ) ;
#59785 = AXIS2_PLACEMENT_3D ( 'NONE', #15112, #26022, #20755 ) ;
#59786 = DIRECTION ( 'NONE',  ( -1.000000000000000000, 0.000000000000000000, 0.000000000000000000 ) ) ;
#59787 = ADVANCED_FACE ( 'NONE', ( #54759 ), #3287, .T. ) ;
#59788 = EDGE_CURVE ( 'NONE', #70067, #38969, #54486, .T. ) ;
#59789 = CARTESIAN_POINT ( 'NONE',  ( -93.33922900947484891, 88.39973697852397549, 74.64190534806806454 ) ) ;
#59790 = FACE_OUTER_BOUND ( 'NONE', #13776, .T. ) ;
#59791 = DIRECTION ( 'NONE',  ( 0.000000000000000000, -0.1045284632676429099, -0.9945218953682744001 ) ) ;
#59792 = VECTOR ( 'NONE', #67751, 1000.000000000000000 ) ;
#59793 =( BOUNDED_CURVE ( )  B_SPLINE_CURVE ( 2, ( #12225, #18964, #64477, #35161, #35527, #12952, #58099 ),
 .UNSPECIFIED., .F., .F. ) 
 B_SPLINE_CURVE_WITH_KNOTS ( ( 3, 2, 2, 3 ),
 ( 0.9374999999999995559, 0.9444444444444441977, 0.9513888888888889506, 0.9583333333333337034 ),
 .UNSPECIFIED. ) 
 CURVE ( )  GEOMETRIC_REPRESENTATION_ITEM ( )  RATIONAL_B_SPLINE_CURVE ( ( 1.000000000000008660, 0.8660254037844301589, 1.000000000000000000, 0.8660254037844387076, 1.000000000000000000, 0.8660254037844322683, 1.000000000000006439 ) ) 
 REPRESENTATION_ITEM ( '' )  );
#59794 = EDGE_CURVE ( 'NONE', #54110, #25904, #1879, .T. ) ;
#59795 = DIRECTION ( 'NONE',  ( -7.962523111838990267E-16, -1.065814103640131188E-14, -1.000000000000000000 ) ) ;
#59796 = FACE_OUTER_BOUND ( 'NONE', #57278, .T. ) ;
#59797 = CYLINDRICAL_SURFACE ( 'NONE', #47799, 2.649999999999985700 ) ;
#59798 = CARTESIAN_POINT ( 'NONE',  ( 95.00000000000000000, -213.0599564267049857, 77.45874999999999488 ) ) ;
#59799 = CARTESIAN_POINT ( 'NONE',  ( -35.37301231164799731, -123.0000000000000142, -2.500000000000000000 ) ) ;
#59800 = DIRECTION ( 'NONE',  ( -0.000000000000000000, -0.000000000000000000, 1.000000000000000000 ) ) ;
#59801 = CARTESIAN_POINT ( 'NONE',  ( -93.67499999999998295, -212.2949673200287179, 86.40166666666667084 ) ) ;
#59802 = DIRECTION ( 'NONE',  ( -1.000000000000000000, -0.000000000000000000, -0.000000000000000000 ) ) ;
#59803 = ORIENTED_EDGE ( 'NONE', *, *, #34162, .T. ) ;
#59804 = CIRCLE ( 'NONE', #18940, 26.50000000000000355 ) ;
#59805 = DIRECTION ( 'NONE',  ( 0.000000000000000000, 0.000000000000000000, 1.000000000000000000 ) ) ;
#59806 = CARTESIAN_POINT ( 'NONE',  ( -3.000000000000000000, -22.67460108101774807, -6.353146135318215038 ) ) ;
#59807 = CARTESIAN_POINT ( 'NONE',  ( 97.65000000000000568, -208.4700217866474645, 81.55979166840097605 ) ) ;
#59808 = AXIS2_PLACEMENT_3D ( 'NONE', #17889, #1755, #40840 ) ;
#59809 = AXIS2_PLACEMENT_3D ( 'NONE', #56664, #73926, #39740 ) ;
#59810 = DIRECTION ( 'NONE',  ( 0.9435911131814402886, -0.3311129884571281101, 0.000000000000000000 ) ) ;
#59811 = AXIS2_PLACEMENT_3D ( 'NONE', #32958, #4419, #68310 ) ;
#59812 = ORIENTED_EDGE ( 'NONE', *, *, #59417, .T. ) ;
#59813 = CARTESIAN_POINT ( 'NONE',  ( -7.500000000000011546, -62.04836822995428491, -275.0000000000000000 ) ) ;
#59814 = DIRECTION ( 'NONE',  ( -1.000000000000000000, 0.000000000000000000, 0.000000000000000000 ) ) ;
#59815 = VERTEX_POINT ( 'NONE', #31812 ) ;
#59816 = EDGE_CURVE ( 'NONE', #48167, #40486, #20913, .T. ) ;
#59817 = CARTESIAN_POINT ( 'NONE',  ( 97.30629616937498838, -209.9999999999999716, 81.70531250086713726 ) ) ;
#59818 = CARTESIAN_POINT ( 'NONE',  ( 97.30629616937498838, -209.9999999999999716, 86.94406250086716170 ) ) ;
#59819 = ORIENTED_EDGE ( 'NONE', *, *, #74282, .T. ) ;
#59820 = CARTESIAN_POINT ( 'NONE',  ( 96.15314808468750130, -211.9973110713294489, 88.10822916753382117 ) ) ;
#59821 = EDGE_LOOP ( 'NONE', ( #14871, #20130, #50189, #46148 ) ) ;
#59822 = FACE_BOUND ( 'NONE', #60787, .T. ) ;
#59823 = ORIENTED_EDGE ( 'NONE', *, *, #48628, .F. ) ;
#59824 = CARTESIAN_POINT ( 'NONE',  ( -92.69370383062502583, 91.33154071421968467, 76.20197916753382117 ) ) ;
#59825 = EDGE_CURVE ( 'NONE', #23125, #6148, #47723, .T. ) ;
#59826 = VECTOR ( 'NONE', #27256, 1000.000000000000000 ) ;
#59827 = VERTEX_POINT ( 'NONE', #58634 ) ;
#59828 = VERTEX_POINT ( 'NONE', #37847 ) ;
#59829 = VECTOR ( 'NONE', #71666, 1000.000000000000000 ) ;
#59830 = CARTESIAN_POINT ( 'NONE',  ( -93.67499999999998295, -212.2949673200287179, 87.75104166840095843 ) ) ;
#59831 = EDGE_CURVE ( 'NONE', #13480, #44329, #66425, .T. ) ;
#59832 = AXIS2_PLACEMENT_3D ( 'NONE', #53524, #70805, #25332 ) ;
#59833 = ORIENTED_EDGE ( 'NONE', *, *, #60170, .F. ) ;
#59834 = CARTESIAN_POINT ( 'NONE',  ( 97.65000000000000568, 91.52997821335252127, 87.90979166840097037 ) ) ;
#59835 = CARTESIAN_POINT ( 'NONE',  ( 10.00000000000000000, -12.42422080174614862, -35.38097989696524337 ) ) ;
#59836 = ORIENTED_EDGE ( 'NONE', *, *, #46257, .T. ) ;
#59837 = DIRECTION ( 'NONE',  ( 1.000000000000000000, -0.000000000000000000, 0.000000000000000000 ) ) ;
#59838 = ORIENTED_EDGE ( 'NONE', *, *, #5700, .F. ) ;
#59839 = VECTOR ( 'NONE', #65271, 1000.000000000000114 ) ;
#59840 = CARTESIAN_POINT ( 'NONE',  ( 96.32499999999998863, -212.2949673200287179, 86.40166666666667084 ) ) ;
#59841 = ORIENTED_EDGE ( 'NONE', *, *, #48448, .T. ) ;
#59842 = EDGE_CURVE ( 'NONE', #53064, #5982, #60779, .T. ) ;
#59843 = ORIENTED_EDGE ( 'NONE', *, *, #9609, .F. ) ;
#59844 = ORIENTED_EDGE ( 'NONE', *, *, #58237, .T. ) ;
#59845 = CARTESIAN_POINT ( 'NONE',  ( 92.69370383062501162, -209.9999999999999716, 80.11781250086713158 ) ) ;
#59846 = PLANE ( 'NONE',  #36481 ) ;
#59847 = DIRECTION ( 'NONE',  ( -1.000000000000000000, 0.000000000000000000, 0.000000000000000000 ) ) ;
#59848 = VERTEX_POINT ( 'NONE', #24793 ) ;
#59849 = PLANE ( 'NONE',  #67665 ) ;
#59850 = VERTEX_POINT ( 'NONE', #8895 ) ;
#59851 = CYLINDRICAL_SURFACE ( 'NONE', #71402, 31.99999999999998579 ) ;
#59852 = PLANE ( 'NONE',  #42792 ) ;
#59853 = CARTESIAN_POINT ( 'NONE',  ( -10.00000000000000000, 0.000000000000000000, 0.000000000000000000 ) ) ;
#59854 = LINE ( 'NONE', #15078, #53952 ) ;
#59855 = CARTESIAN_POINT ( 'NONE',  ( -92.69370383062498320, -209.9999999999999716, 80.43531250086714124 ) ) ;
#59856 = CARTESIAN_POINT ( 'NONE',  ( -97.30629616937501680, 91.33154071421968467, 78.31864583420050963 ) ) ;
#59857 = VERTEX_POINT ( 'NONE', #49112 ) ;
#59858 = ADVANCED_FACE ( 'NONE', ( #55125 ), #3650, .T. ) ;
#59859 = CARTESIAN_POINT ( 'NONE',  ( 96.15314808468748708, 88.00268892867053694, 81.59947916753381492 ) ) ;
#59860 = VERTEX_POINT ( 'NONE', #47365 ) ;
#59861 = DIRECTION ( 'NONE',  ( -1.000000000000000000, -0.000000000000000000, -0.000000000000000000 ) ) ;
#59862 = PLANE ( 'NONE',  #57610 ) ;
#59863 = VECTOR ( 'NONE', #20530, 1000.000000000000000 ) ;
#59865 = EDGE_CURVE ( 'NONE', #51720, #45705, #13136, .T. ) ;
#59864 = CARTESIAN_POINT ( 'NONE',  ( 0.000000000000000000, 0.000000000000000000, 0.000000000000000000 ) ) ;
#59866 = CYLINDRICAL_SURFACE ( 'NONE', #49906, 31.99999999999999289 ) ;
#59867 = FACE_OUTER_BOUND ( 'NONE', #61431, .T. ) ;
#59868 = CARTESIAN_POINT ( 'NONE',  ( -93.84685191531248449, -208.0026889286704943, 82.44614583420046472 ) ) ;
#59869 = CIRCLE ( 'NONE', #57500, 3.299999999999983391 ) ;
#59870 = AXIS2_PLACEMENT_3D ( 'NONE', #20498, #4604, #27507 ) ;
#59871 = CARTESIAN_POINT ( 'NONE',  ( 11.99999999999999822, -5.256550761633395297, 77.32052557432841411 ) ) ;
#59872 = FACE_OUTER_BOUND ( 'NONE', #66205, .T. ) ;
#59873 = EDGE_CURVE ( 'NONE', #45145, #70724, #53368, .T. ) ;
#59874 = CARTESIAN_POINT ( 'NONE',  ( 0.000000000000000000, 80.55351364060611274, -15.33399622253396544 ) ) ;
#59875 = EDGE_LOOP ( 'NONE', ( #2623, #29217, #25378, #16914 ) ) ;
#59876 = AXIS2_PLACEMENT_3D ( 'NONE', #32757, #21863, #44807 ) ;
#59877 = ORIENTED_EDGE ( 'NONE', *, *, #26924, .F. ) ;
#59878 = CARTESIAN_POINT ( 'NONE',  ( 0.000000000000000000, -37.16516213103280108, 4.992566952384862589 ) ) ;
#59879 = AXIS2_PLACEMENT_3D ( 'NONE', #65082, #23731, #1589 ) ;
#59880 = CARTESIAN_POINT ( 'NONE',  ( 92.34999999999998010, 91.52997821335250705, 84.86708333333332632 ) ) ;
#59881 = EDGE_CURVE ( 'NONE', #59737, #43856, #72038, .T. ) ;
#59882 = CARTESIAN_POINT ( 'NONE',  ( -97.30629616937501680, 90.00000000000004263, 86.46781250086714010 ) ) ;
#59883 = LINE ( 'NONE', #30178, #26197 ) ;
#59884 = LINE ( 'NONE', #43701, #23002 ) ;
#59885 = DIRECTION ( 'NONE',  ( -1.000000000000000000, 0.000000000000000000, 0.000000000000000000 ) ) ;
#59886 = ORIENTED_EDGE ( 'NONE', *, *, #65347, .F. ) ;
#59887 = EDGE_CURVE ( 'NONE', #62914, #26721, #7141, .T. ) ;
#59888 = DIRECTION ( 'NONE',  ( 2.603472992746261562E-14, 2.546204323184492723E-14, -1.000000000000000000 ) ) ;
#59889 = VECTOR ( 'NONE', #18915, 1000.000000000000000 ) ;
#59890 = LINE ( 'NONE', #53500, #21323 ) ;
#59891 = CIRCLE ( 'NONE', #46672, 37.49900000000000944 ) ;
#59892 = CARTESIAN_POINT ( 'NONE',  ( 0.000000000000000000, 2.543863470249527303, -81.96053171279901051 ) ) ;
#59893 = CARTESIAN_POINT ( 'NONE',  ( -4.088737910769898676, 3.412868758467427988, -1.160540885688320589 ) ) ;
#59894 = CARTESIAN_POINT ( 'NONE',  ( 0.000000000000000000, 0.000000000000000000, 0.000000000000000000 ) ) ;
#59895 = CARTESIAN_POINT ( 'NONE',  ( 10.00000000000000000, 0.000000000000000000, 0.000000000000000000 ) ) ;
#59896 = CARTESIAN_POINT ( 'NONE',  ( -94.99999999999997158, -207.3369185715606307, 81.38781250086715602 ) ) ;
#59897 = PRESENTATION_STYLE_ASSIGNMENT (( #9114 ) ) ;
#59898 = AXIS2_PLACEMENT_3D ( 'NONE', #34661, #40683, #35406 ) ;
#59899 = VECTOR ( 'NONE', #21126, 1000.000000000000000 ) ;
#59900 = CARTESIAN_POINT ( 'NONE',  ( 0.000000000000000000, 0.000000000000000000, 0.000000000000000000 ) ) ;
#59901 = CIRCLE ( 'NONE', #45521, 82.00000000000000000 ) ;
#59902 = CARTESIAN_POINT ( 'NONE',  ( 96.66079198124940319, 88.39975876321993553, 74.80065669543249385 ) ) ;
#59903 = LINE ( 'NONE', #8757, #46605 ) ;
#59904 = LINE ( 'NONE', #31305, #11728 ) ;
#59905 = ORIENTED_EDGE ( 'NONE', *, *, #29692, .T. ) ;
#59906 = CARTESIAN_POINT ( 'NONE',  ( 92.34999999999999432, 90.00000000000002842, 90.00000000000000000 ) ) ;
#59907 = DIRECTION ( 'NONE',  ( -1.000000000000000000, -0.000000000000000000, -0.000000000000000000 ) ) ;
#59908 = CYLINDRICAL_SURFACE ( 'NONE', #1840, 32.00000000000000000 ) ;
#59909 =( BOUNDED_CURVE ( )  B_SPLINE_CURVE ( 2, ( #32491, #56175, #9197, #55058, #44155, #9572, #3589, #72348, #15949 ),
 .UNSPECIFIED., .F., .F. ) 
 B_SPLINE_CURVE_WITH_KNOTS ( ( 3, 2, 2, 2, 3 ),
 ( 0.4445132602971398339, 0.4515689946164713753, 0.4586247601573539279, 0.4656805256982363694, 0.4656806970056960315 ),
 .UNSPECIFIED. ) 
 CURVE ( )  GEOMETRIC_REPRESENTATION_ITEM ( )  RATIONAL_B_SPLINE_CURVE ( ( 0.9999988143381067784, 0.8660259966180086089, 1.000000000000000000, 0.8660254037844387076, 1.000000000000000000, 0.8660254037844387076, 1.000000000000000000, 0.9999967472207509367, 0.9999934945994508606 ) ) 
 REPRESENTATION_ITEM ( '' )  );
#59910 = DIRECTION ( 'NONE',  ( 0.000000000000000000, -6.982962677686266711E-15, 1.000000000000000000 ) ) ;
#59911 = CARTESIAN_POINT ( 'NONE',  ( 97.30629616937498838, -209.9999999999999716, 88.21406250086714351 ) ) ;
#59912 = ORIENTED_EDGE ( 'NONE', *, *, #63001, .F. ) ;
#59913 = AXIS2_PLACEMENT_3D ( 'NONE', #30153, #18501, #58741 ) ;
#59914 = DIRECTION ( 'NONE',  ( 0.000000000000000000, 0.000000000000000000, 1.000000000000000000 ) ) ;
#59915 = FILL_AREA_STYLE_COLOUR ( '', #35513 ) ;
#59916 = ORIENTED_EDGE ( 'NONE', *, *, #10504, .T. ) ;
#59917 = AXIS2_PLACEMENT_3D ( 'NONE', #60314, #48644, #70439 ) ;
#59918 = CARTESIAN_POINT ( 'NONE',  ( 10.00000000000000000, 76.66974797899837313, 11.30684508768368524 ) ) ;
#59919 = ORIENTED_EDGE ( 'NONE', *, *, #31378, .F. ) ;
#59920 = VECTOR ( 'NONE', #65937, 1000.000000000000000 ) ;
#59921 = EDGE_CURVE ( 'NONE', #69710, #55743, #12765, .T. ) ;
#59922 = CARTESIAN_POINT ( 'NONE',  ( 11.99999999999999822, 17.28742895386189460, -75.54627589209927407 ) ) ;
#59923 = CIRCLE ( 'NONE', #61161, 37.49900000000001654 ) ;
#59924 = EDGE_CURVE ( 'NONE', #18572, #26714, #18773, .T. ) ;
#59925 = ORIENTED_EDGE ( 'NONE', *, *, #29444, .F. ) ;
#59926 = ORIENTED_EDGE ( 'NONE', *, *, #20865, .F. ) ;
#59927 = CIRCLE ( 'NONE', #27493, 31.99999999999998579 ) ;
#59929 = VERTEX_POINT ( 'NONE', #72765 ) ;
#59928 = EDGE_CURVE ( 'NONE', #48739, #31708, #73143, .T. ) ;
#59930 = CYLINDRICAL_SURFACE ( 'NONE', #58723, 77.49899999999999523 ) ;
#59931 = ORIENTED_EDGE ( 'NONE', *, *, #28883, .T. ) ;
#59933 = EDGE_CURVE ( 'NONE', #73763, #1655, #54646, .T. ) ;
#59932 = ORIENTED_EDGE ( 'NONE', *, *, #59106, .T. ) ;
#59934 = CARTESIAN_POINT ( 'NONE',  ( 97.30629616937498838, 88.66845928578037217, 81.17614583420048291 ) ) ;
#59935 = DIRECTION ( 'NONE',  ( 1.000000000000000000, 0.000000000000000000, 0.000000000000000000 ) ) ;
#59936 = CARTESIAN_POINT ( 'NONE',  ( -96.32500000000001705, 92.29496732002878900, 88.06854166840095388 ) ) ;
#59937 = CIRCLE ( 'NONE', #67108, 77.49900000000000944 ) ;
#59938 = EDGE_LOOP ( 'NONE', ( #34969, #42370, #23403, #55494 ) ) ;
#59940 = ORIENTED_EDGE ( 'NONE', *, *, #10723, .F. ) ;
#59939 = CIRCLE ( 'NONE', #68312, 77.49899999999999523 ) ;
#59941 = ORIENTED_EDGE ( 'NONE', *, *, #16144, .F. ) ;
#59942 = CARTESIAN_POINT ( 'NONE',  ( 10.00000000000000000, 33.00180498840072829, -17.80606268964504935 ) ) ;
#59943 = VERTEX_POINT ( 'NONE', #33675 ) ;
#59944 = VECTOR ( 'NONE', #53304, 1000.000000000000114 ) ;
#59945 = AXIS2_PLACEMENT_3D ( 'NONE', #11556, #51412, #23232 ) ;
#59946 = DIRECTION ( 'NONE',  ( -3.065994397161057213E-18, 1.942648362116681808E-16, 1.000000000000000000 ) ) ;
#59947 = DIRECTION ( 'NONE',  ( 0.000000000000000000, 0.4539904997395413089, 0.8910065241883705633 ) ) ;
#59948 = DIRECTION ( 'NONE',  ( 1.000000000000000000, 0.000000000000000000, 0.000000000000000000 ) ) ;
#59949 = CYLINDRICAL_SURFACE ( 'NONE', #12483, 82.00000000000000000 ) ;
#59950 = CYLINDRICAL_SURFACE ( 'NONE', #64312, 77.49899999999999523 ) ;
#59951 = DIRECTION ( 'NONE',  ( -1.000000000000000000, -6.951859121168206841E-17, 0.000000000000000000 ) ) ;
#59952 = AXIS2_PLACEMENT_3D ( 'NONE', #70612, #58995, #42075 ) ;
#59953 = CARTESIAN_POINT ( 'NONE',  ( 10.00000000000000000, 74.74816331893428867, 33.71516098798765881 ) ) ;
#59954 = CIRCLE ( 'NONE', #45573, 31.99999999999998579 ) ;
#59955 = CARTESIAN_POINT ( 'NONE',  ( -93.67499999999998295, -207.7050326799711968, 76.53270833506762472 ) ) ;
#59956 = CARTESIAN_POINT ( 'NONE',  ( -92.69370383062502583, 88.66845928578038638, 89.43114583420049257 ) ) ;
#59957 = APPLICATION_CONTEXT ( 'automotive_design' ) ;
#59959 = CARTESIAN_POINT ( 'NONE',  ( -92.35000000000005116, 91.52997821335253548, 77.74979166840097378 ) ) ;
#59958 = CARTESIAN_POINT ( 'NONE',  ( 97.64999999999997726, 91.52997821335252127, 76.47979166840096354 ) ) ;
#59960 = VECTOR ( 'NONE', #68324, 1000.000000000000000 ) ;
#59961 = ORIENTED_EDGE ( 'NONE', *, *, #27260, .F. ) ;
#59962 = CARTESIAN_POINT ( 'NONE',  ( 92.69370383062498320, 91.33154071421968467, 77.68364583420047609 ) ) ;
#59963 = DIRECTION ( 'NONE',  ( 0.000000000000000000, 0.000000000000000000, -1.000000000000000000 ) ) ;
#59964 = DIRECTION ( 'NONE',  ( 1.000000000000000000, 0.000000000000000000, 0.000000000000000000 ) ) ;
#59965 = CARTESIAN_POINT ( 'NONE',  ( 0.000000000000000000, 0.8261519478431255115, 77.49459641780886443 ) ) ;
#59966 = DIRECTION ( 'NONE',  ( 0.000000000000000000, 0.000000000000000000, 1.000000000000000000 ) ) ;
#59967 = CARTESIAN_POINT ( 'NONE',  ( 0.000000000000000000, 37.22597642581150268, 5.202137450157037435 ) ) ;
#59968 = ORIENTED_EDGE ( 'NONE', *, *, #18401, .F. ) ;
#59969 = CARTESIAN_POINT ( 'NONE',  ( -96.32499999999996021, -212.2949673200287179, 87.56583333333333030 ) ) ;
#59970 = EDGE_CURVE ( 'NONE', #31543, #71294, #44972, .T. ) ;
#59971 = EDGE_CURVE ( 'NONE', #50746, #35410, #49639, .T. ) ;
#59972 = CARTESIAN_POINT ( 'NONE',  ( 10.00000000000000000, 0.000000000000000000, 0.000000000000000000 ) ) ;
#59973 = EDGE_LOOP ( 'NONE', ( #17369, #46968, #57096, #43397 ) ) ;
#59974 = ORIENTED_EDGE ( 'NONE', *, *, #73602, .F. ) ;
#59975 = CARTESIAN_POINT ( 'NONE',  ( 11.99999999999999822, -65.58780272294048075, -36.73666225445966660 ) ) ;
#59976 = ADVANCED_FACE ( 'NONE', ( #62649 ), #56631, .T. ) ;
#59977 = DIRECTION ( 'NONE',  ( 0.000000000000000000, 0.8910065241883656784, 0.4539904997395511344 ) ) ;
#59978 = FACE_OUTER_BOUND ( 'NONE', #71086, .T. ) ;
#59979 = CARTESIAN_POINT ( 'NONE',  ( -25.50183398199384754, -112.6408924756582053, 5.500000000000000000 ) ) ;
#59980 = DIRECTION ( 'NONE',  ( 1.000000000000000000, 0.000000000000000000, 0.000000000000000000 ) ) ;
#59981 = DIRECTION ( 'NONE',  ( 1.000000000000000000, 0.000000000000000000, 0.000000000000000000 ) ) ;
#59982 = AXIS2_PLACEMENT_3D ( 'NONE', #24528, #48572, #42939 ) ;
#59983 = ORIENTED_EDGE ( 'NONE', *, *, #44654, .T. ) ;
#59984 = VECTOR ( 'NONE', #22284, 1000.000000000000000 ) ;
#59986 = DIRECTION ( 'NONE',  ( -0.000000000000000000, -0.000000000000000000, 1.000000000000000000 ) ) ;
#59985 = AXIS2_PLACEMENT_3D ( 'NONE', #15658, #21269, #22793 ) ;
#59987 = DIRECTION ( 'NONE',  ( 0.000000000000000000, -0.8526401643540861830, -0.5224985647159590130 ) ) ;
#59988 = CARTESIAN_POINT ( 'NONE',  ( 0.000000000000000000, 44.88180994100466847, -63.18004540532978552 ) ) ;
#59989 = AXIS2_PLACEMENT_3D ( 'NONE', #52651, #15573, #39257 ) ;
#59990 = CARTESIAN_POINT ( 'NONE',  ( -7.469491406282094736, 4.756046723998911929, 42.00000000000001421 ) ) ;
#59991 = CARTESIAN_POINT ( 'NONE',  ( 11.99999999999999822, -39.78640506895559525, -66.50666863322042843 ) ) ;
#59992 = CARTESIAN_POINT ( 'NONE',  ( -7.400000000000003908, -1.056673655988042765E-14, -5.892267102755452808E-15 ) ) ;
#59993 = CARTESIAN_POINT ( 'NONE',  ( 11.99999999999999822, 68.67312586194995561, 35.91791733033500122 ) ) ;
#59994 = CARTESIAN_POINT ( 'NONE',  ( 97.30629616937498838, 88.66845928578035796, 83.71614583420048916 ) ) ;
#59995 = CARTESIAN_POINT ( 'NONE',  ( -97.30629616937497417, -208.6684592857803295, 84.66864583420047552 ) ) ;
#59996 = FACE_OUTER_BOUND ( 'NONE', #45616, .T. ) ;
#59997 = AXIS2_PLACEMENT_3D ( 'NONE', #68749, #17235, #39057 ) ;
#59998 = ORIENTED_EDGE ( 'NONE', *, *, #28612, .F. ) ;
#59999 = DIRECTION ( 'NONE',  ( 1.000000000000000000, -0.000000000000000000, -0.000000000000000000 ) ) ;
#60000 = CARTESIAN_POINT ( 'NONE',  ( -93.67499999999998295, -207.7050326799711968, 78.99333333333332519 ) ) ;
#60001 = DIRECTION ( 'NONE',  ( -1.000000000000000000, 0.000000000000000000, -0.000000000000000000 ) ) ;
#60002 = AXIS2_PLACEMENT_3D ( 'NONE', #43408, #31716, #26080 ) ;
#60003 = CIRCLE ( 'NONE', #21603, 31.99999999999999289 ) ;
#60004 = AXIS2_PLACEMENT_3D ( 'NONE', #11008, #56129, #34300 ) ;
#60005 = VECTOR ( 'NONE', #22831, 1000.000000000000114 ) ;
#60006 = CARTESIAN_POINT ( 'NONE',  ( 92.69370383062501162, -209.9999999999999716, 83.29281250086714294 ) ) ;
#60007 = ORIENTED_EDGE ( 'NONE', *, *, #52791, .T. ) ;
#60008 = DIRECTION ( 'NONE',  ( -1.000000000000000000, -1.427937372958405461E-15, -7.962523111839130290E-16 ) ) ;
#60009 = VERTEX_POINT ( 'NONE', #10375 ) ;
#60010 =( BOUNDED_CURVE ( )  B_SPLINE_CURVE ( 2, ( #14709, #19607, #37660, #42554, #48558, #61605, #55959 ),
 .UNSPECIFIED., .F., .F. ) 
 B_SPLINE_CURVE_WITH_KNOTS ( ( 3, 2, 2, 3 ),
 ( 0.6041666666666670737, 0.6111111111111116045, 0.6180555555555559133, 0.6250000000000003331 ),
 .UNSPECIFIED. ) 
 CURVE ( )  GEOMETRIC_REPRESENTATION_ITEM ( )  RATIONAL_B_SPLINE_CURVE ( ( 0.9999999999999914513, 0.8660254037844472563, 1.000000000000000000, 0.8660254037844387076, 1.000000000000000000, 0.8660254037844322683, 1.000000000000006439 ) ) 
 REPRESENTATION_ITEM ( '' )  );
#60011 = ORIENTED_EDGE ( 'NONE', *, *, #67849, .T. ) ;
#60012 = EDGE_CURVE ( 'NONE', #11199, #25600, #44226, .T. ) ;
#60013 = DIRECTION ( 'NONE',  ( -1.000000000000000000, -0.000000000000000000, 0.000000000000000000 ) ) ;
#60014 = ADVANCED_FACE ( 'NONE', ( #21265 ), #10751, .T. ) ;
#60015 = ORIENTED_EDGE ( 'NONE', *, *, #55327, .T. ) ;
#60016 = FACE_OUTER_BOUND ( 'NONE', #45619, .T. ) ;
#60017 = EDGE_CURVE ( 'NONE', #25521, #71862, #27045, .T. ) ;
#60018 = CARTESIAN_POINT ( 'NONE',  ( 95.00000000000000000, -207.3369185715606307, 78.84781250086714977 ) ) ;
#60019 = CYLINDRICAL_SURFACE ( 'NONE', #27231, 42.00000000000000000 ) ;
#60020 = DIRECTION ( 'NONE',  ( -0.8541291221503265474, 0.5200609990133007177, 0.000000000000000000 ) ) ;
#60021 = CYLINDRICAL_SURFACE ( 'NONE', #42468, 82.00000000000000000 ) ;
#60022 = CARTESIAN_POINT ( 'NONE',  ( 92.34999999999999432, 90.00000000000002842, 76.66499999999999204 ) ) ;
#60023 = EDGE_CURVE ( 'NONE', #57334, #63672, #55892, .T. ) ;
#60024 = AXIS2_PLACEMENT_3D ( 'NONE', #59397, #25543, #53748 ) ;
#60025 = CARTESIAN_POINT ( 'NONE',  ( 0.000000000000000000, 24.73286445877808148, -73.44644590900034586 ) ) ;
#60026 = CARTESIAN_POINT ( 'NONE',  ( 96.32499999999998863, -212.2949673200287179, 80.05166666666666231 ) ) ;
#60027 = AXIS2_PLACEMENT_3D ( 'NONE', #55411, #67057, #15563 ) ;
#60028 = ORIENTED_EDGE ( 'NONE', *, *, #24015, .F. ) ;
#60029 = ORIENTED_EDGE ( 'NONE', *, *, #7418, .F. ) ;
#60030 = AXIS2_PLACEMENT_3D ( 'NONE', #44903, #56560, #39630 ) ;
#60031 = EDGE_CURVE ( 'NONE', #43453, #56886, #50594, .T. ) ;
#60032 = ORIENTED_EDGE ( 'NONE', *, *, #73939, .F. ) ;
#60033 = VERTEX_POINT ( 'NONE', #38957 ) ;
#60034 = DIRECTION ( 'NONE',  ( -0.000000000000000000, -0.000000000000000000, -1.000000000000000000 ) ) ;
#60035 = PRESENTATION_STYLE_ASSIGNMENT (( #37084 ) ) ;
#60036 = CARTESIAN_POINT ( 'NONE',  ( -92.69370383062502583, 88.66845928578038638, 85.62114583420047609 ) ) ;
#60037 = FACE_OUTER_BOUND ( 'NONE', #49267, .T. ) ;
#60038 = AXIS2_PLACEMENT_3D ( 'NONE', #6437, #61447, #44899 ) ;
#60039 = DIRECTION ( 'NONE',  ( 0.000000000000000000, 0.3826834323650907810, -0.9238795325112864054 ) ) ;
#60040 = CARTESIAN_POINT ( 'NONE',  ( 92.34999999999999432, 90.00000000000002842, 75.39499999999999602 ) ) ;
#60041 = EDGE_CURVE ( 'NONE', #42829, #31594, #40274, .T. ) ;
#60042 = DIRECTION ( 'NONE',  ( 1.000000000000000000, 0.000000000000000000, 0.000000000000000000 ) ) ;
#60043 = VERTEX_POINT ( 'NONE', #67151 ) ;
#60044 = CARTESIAN_POINT ( 'NONE',  ( -96.32499999999996021, -212.2949673200287179, 84.47020833506762472 ) ) ;
#60045 = EDGE_LOOP ( 'NONE', ( #33084, #876, #62702, #21113 ) ) ;
#60046 = EDGE_CURVE ( 'NONE', #30489, #8961, #39707, .T. ) ;
#60047 = CARTESIAN_POINT ( 'NONE',  ( 10.00000000000000000, -23.16143007188376757, -73.95703589263997912 ) ) ;
#60048 = EDGE_LOOP ( 'NONE', ( #18473, #68516, #24086, #46270 ) ) ;
#60049 = CARTESIAN_POINT ( 'NONE',  ( -92.35000000000003695, 90.00000000000004263, 85.31687500173428873 ) ) ;
#60050 = VERTEX_POINT ( 'NONE', #61517 ) ;
#60051 = CARTESIAN_POINT ( 'NONE',  ( 97.30629616937498838, 88.66845928578037217, 86.89114583420050053 ) ) ;
#60052 = CARTESIAN_POINT ( 'NONE',  ( 0.000000000000000000, 0.000000000000000000, -5.974599999999999689 ) ) ;
#60053 = DIRECTION ( 'NONE',  ( -1.000000000000000000, 0.000000000000000000, 0.000000000000000000 ) ) ;
#60054 = AXIS2_PLACEMENT_3D ( 'NONE', #3669, #72055, #25824 ) ;
#60055 = CARTESIAN_POINT ( 'NONE',  ( 15.00000000000000000, -13.04903810567675393, -19.60159698893424718 ) ) ;
#60056 = DIRECTION ( 'NONE',  ( -0.000000000000000000, -0.000000000000000000, 1.000000000000000000 ) ) ;
#60057 = ORIENTED_EDGE ( 'NONE', *, *, #41830, .F. ) ;
#60058 = CARTESIAN_POINT ( 'NONE',  ( 0.4079457818577056916, -5.537975084925947478, -5.689399939901065295 ) ) ;
#60059 = CIRCLE ( 'NONE', #24031, 16.00000000000000000 ) ;
#60060 = VECTOR ( 'NONE', #35430, 1000.000000000000000 ) ;
#60061 = EDGE_CURVE ( 'NONE', #24488, #38008, #51334, .T. ) ;
#60062 = EDGE_CURVE ( 'NONE', #18753, #40498, #22788, .T. ) ;
#60064 = CARTESIAN_POINT ( 'NONE',  ( 0.000000000000000000, -56.15606465354916566, -59.75363087400133111 ) ) ;
#60063 = AXIS2_PLACEMENT_3D ( 'NONE', #10662, #17420, #68186 ) ;
#60065 = VERTEX_POINT ( 'NONE', #45729 ) ;
#60066 = ORIENTED_EDGE ( 'NONE', *, *, #13920, .F. ) ;
#60067 = FACE_BOUND ( 'NONE', #72196, .T. ) ;
#60068 = AXIS2_PLACEMENT_3D ( 'NONE', #30870, #65114, #60582 ) ;
#60069 = VECTOR ( 'NONE', #3151, 1000.000000000000000 ) ;
#60070 = FACE_OUTER_BOUND ( 'NONE', #19579, .T. ) ;
#60071 = DIRECTION ( 'NONE',  ( 7.959965316982041921E-16, 1.065814103640131188E-14, 1.000000000000000000 ) ) ;
#60072 = CARTESIAN_POINT ( 'NONE',  ( -97.30629616937495996, -209.9999999999999716, 82.81656250086714977 ) ) ;
#60073 = VERTEX_POINT ( 'NONE', #68651 ) ;
#60074 = CYLINDRICAL_SURFACE ( 'NONE', #58504, 2.649999999999999467 ) ;
#60075 = ORIENTED_EDGE ( 'NONE', *, *, #55163, .T. ) ;
#60076 = ORIENTED_EDGE ( 'NONE', *, *, #33714, .F. ) ;
#60077 = DIRECTION ( 'NONE',  ( 0.000000000000000000, 0.000000000000000000, -1.000000000000000000 ) ) ;
#60078 = CARTESIAN_POINT ( 'NONE',  ( 93.84685191531248449, 88.00268892867053694, 88.63739583420048973 ) ) ;
#60079 = CARTESIAN_POINT ( 'NONE',  ( 92.69370383062498320, 90.00000000000002842, 79.48281250086714067 ) ) ;
#60080 = LINE ( 'NONE', #25475, #38889 ) ;
#60081 = CARTESIAN_POINT ( 'NONE',  ( 11.99999999999999822, -36.72794159290288718, 65.59268652807197952 ) ) ;
#60082 = LINE ( 'NONE', #37875, #32520 ) ;
#60083 = CARTESIAN_POINT ( 'NONE',  ( 94.56602944578222036, 92.35870626171012532, 74.84690984288803861 ) ) ;
#60084 = CARTESIAN_POINT ( 'NONE',  ( -95.00000000000002842, 86.94004357329504273, 76.90312500173429555 ) ) ;
#60085 = CYLINDRICAL_SURFACE ( 'NONE', #58734, 82.00000000000000000 ) ;
#60086 = DIRECTION ( 'NONE',  ( -0.000000000000000000, -0.5000000000000004441, 0.8660254037844383745 ) ) ;
#60087 = CARTESIAN_POINT ( 'NONE',  ( 0.000000000000000000, -75.11725578898466438, -2.956366410621452001 ) ) ;
#60088 = EDGE_LOOP ( 'NONE', ( #11989, #48594, #63928, #64873 ) ) ;
#60089 = AXIS2_PLACEMENT_3D ( 'NONE', #42582, #48943, #8742 ) ;
#60090 = CARTESIAN_POINT ( 'NONE',  ( -96.15314808468752972, 91.99731107132950569, 85.72697916753379843 ) ) ;
#60091 = CIRCLE ( 'NONE', #27649, 15.99999999999999822 ) ;
#60092 = CARTESIAN_POINT ( 'NONE',  ( 0.000000000000000000, 8.830959090342393125, 74.65491531819122883 ) ) ;
#60093 = EDGE_CURVE ( 'NONE', #61657, #65189, #37904, .T. ) ;
#60094 = CARTESIAN_POINT ( 'NONE',  ( -10.00000000000000000, 0.000000000000000000, 0.000000000000000000 ) ) ;
#60095 = EDGE_CURVE ( 'NONE', #26057, #60769, #30700, .T. ) ;
#60096 = VERTEX_POINT ( 'NONE', #12597 ) ;
#60097 = CARTESIAN_POINT ( 'NONE',  ( 93.67500000000001137, -207.7050326799711968, 83.54416666666666913 ) ) ;
#60098 = DIRECTION ( 'NONE',  ( 0.000000000000000000, 0.000000000000000000, -1.000000000000000000 ) ) ;
#60099 = DIRECTION ( 'NONE',  ( 1.000000000000000000, 1.427937372958405461E-15, 7.962523111839130290E-16 ) ) ;
#60100 = ADVANCED_FACE ( 'NONE', ( #29140 ), #265, .F. ) ;
#60101 = AXIS2_PLACEMENT_3D ( 'NONE', #11137, #50227, #68660 ) ;
#60102 = AXIS2_PLACEMENT_3D ( 'NONE', #68404, #73275, #51095 ) ;
#60103 = CIRCLE ( 'NONE', #10886, 16.00000000000000000 ) ;
#60104 = CARTESIAN_POINT ( 'NONE',  ( 96.15314808468750130, -211.9973110713294489, 78.58322916753382970 ) ) ;
#60105 = EDGE_CURVE ( 'NONE', #28069, #8551, #18240, .T. ) ;
#60106 = ORIENTED_EDGE ( 'NONE', *, *, #41085, .T. ) ;
#60107 = CIRCLE ( 'NONE', #32501, 16.00000000000000000 ) ;
#60108 = ORIENTED_EDGE ( 'NONE', *, *, #36307, .F. ) ;
#60109 = DIRECTION ( 'NONE',  ( 0.9730327541852493711, -0.2306669878475637314, 0.000000000000000000 ) ) ;
#60110 = CARTESIAN_POINT ( 'NONE',  ( 10.00000000000000000, -24.73286445877653961, -73.44644590900085745 ) ) ;
#60111 = CARTESIAN_POINT ( 'NONE',  ( -92.34999999999999432, -209.9999999999999716, 86.50750000000000739 ) ) ;
#60112 = ADVANCED_FACE ( 'NONE', ( #11844 ), #1941, .T. ) ;
#60113 = VERTEX_POINT ( 'NONE', #36269 ) ;
#60114 = DIRECTION ( 'NONE',  ( -0.000000000000000000, -0.000000000000000000, -1.000000000000000000 ) ) ;
#60115 = CARTESIAN_POINT ( 'NONE',  ( 92.35000000000002274, -208.4700217866474645, 89.94708333333333883 ) ) ;
#60116 = EDGE_LOOP ( 'NONE', ( #72403, #36926, #69978, #44318 ) ) ;
#60117 = CARTESIAN_POINT ( 'NONE',  ( 92.34999999999999432, 90.00000000000002842, 79.20499999999999829 ) ) ;
#60118 = ORIENTED_EDGE ( 'NONE', *, *, #26535, .F. ) ;
#60119 = ORIENTED_EDGE ( 'NONE', *, *, #21213, .T. ) ;
#60120 = CARTESIAN_POINT ( 'NONE',  ( -93.67500000000003979, 87.70503267997129626, 83.22666666666665947 ) ) ;
#60121 =( NAMED_UNIT ( * ) PLANE_ANGLE_UNIT ( ) SI_UNIT ( $, .RADIAN. ) );
#60122 = CARTESIAN_POINT ( 'NONE',  ( 0.000000000000000000, 41.76937507738875155, -62.50329211542393892 ) ) ;
#60123 = ORIENTED_EDGE ( 'NONE', *, *, #1512, .T. ) ;
#60124 = DIRECTION ( 'NONE',  ( 0.9997280174009349762, -0.02332147558787674158, 0.000000000000000000 ) ) ;
#60125 = CARTESIAN_POINT ( 'NONE',  ( 93.67500000000001137, -207.7050326799711968, 82.35354166840096468 ) ) ;
#60126 = CARTESIAN_POINT ( 'NONE',  ( 92.34999999999999432, 90.00000000000002842, 84.92000000000000171 ) ) ;
#60127 = EDGE_CURVE ( 'NONE', #64091, #20620, #67919, .T. ) ;
#60128 = ORIENTED_EDGE ( 'NONE', *, *, #41665, .F. ) ;
#60129 = DIRECTION ( 'NONE',  ( 0.2306669878475647861, 0.9730327541852491491, 0.000000000000000000 ) ) ;
#60130 = EDGE_CURVE ( 'NONE', #57334, #32561, #58840, .T. ) ;
#60131 = CARTESIAN_POINT ( 'NONE',  ( 10.00000000000000000, 27.13269053701132094, -25.88420570971372570 ) ) ;
#60132 = ORIENTED_EDGE ( 'NONE', *, *, #1808, .T. ) ;
#60133 = VERTEX_POINT ( 'NONE', #64478 ) ;
#60134 = CARTESIAN_POINT ( 'NONE',  ( -97.30629616937501680, 91.33154071421968467, 87.84364583420048689 ) ) ;
#60135 = CARTESIAN_POINT ( 'NONE',  ( 93.84685191531248449, 88.00268892867053694, 82.12864583420046927 ) ) ;
#60136 = ORIENTED_EDGE ( 'NONE', *, *, #73058, .T. ) ;
#60137 = CARTESIAN_POINT ( 'NONE',  ( 93.67499999999999716, 87.70503267997126784, 83.83520833506763381 ) ) ;
#60138 = AXIS2_PLACEMENT_3D ( 'NONE', #54416, #15298, #4414 ) ;
#60139 = CARTESIAN_POINT ( 'NONE',  ( 10.00000000000000000, 0.000000000000000000, 0.000000000000000000 ) ) ;
#60140 = ORIENTED_EDGE ( 'NONE', *, *, #56292, .T. ) ;
#60141 = CARTESIAN_POINT ( 'NONE',  ( 97.65000000000009095, -211.5299782133523649, 78.19958333333332234 ) ) ;
#60142 = VECTOR ( 'NONE', #24189, 1000.000000000000000 ) ;
#60143 = ORIENTED_EDGE ( 'NONE', *, *, #70434, .T. ) ;
#60144 = ORIENTED_EDGE ( 'NONE', *, *, #70410, .F. ) ;
#60145 = VERTEX_POINT ( 'NONE', #622 ) ;
#60146 = DIRECTION ( 'NONE',  ( 0.000000000000000000, -0.7071067811865389130, -0.7071067811865561215 ) ) ;
#60147 = CARTESIAN_POINT ( 'NONE',  ( 4.999999999999999112, -40.98264845739755202, 9.188173127307159405 ) ) ;
#60148 = CARTESIAN_POINT ( 'NONE',  ( -92.35000000000005116, 88.47002178664754979, 84.54958333333333087 ) ) ;
#60149 = ORIENTED_EDGE ( 'NONE', *, *, #65855, .T. ) ;
#60150 = CARTESIAN_POINT ( 'NONE',  ( 0.000000000000000000, -30.41916302227164337, 71.27951684758015460 ) ) ;
#60151 = CARTESIAN_POINT ( 'NONE',  ( 92.34999999999999432, 91.52997821335252127, 89.39145833506763950 ) ) ;
#60152 = ORIENTED_EDGE ( 'NONE', *, *, #21651, .T. ) ;
#60153 = DIRECTION ( 'NONE',  ( -1.000000000000000000, 0.000000000000000000, -0.000000000000000000 ) ) ;
#60154 = CARTESIAN_POINT ( 'NONE',  ( -97.30629616937495996, -209.9999999999999716, 79.48281250086714067 ) ) ;
#60155 = ORIENTED_EDGE ( 'NONE', *, *, #24333, .F. ) ;
#60156 = DIRECTION ( 'NONE',  ( -1.000000000000000000, 0.000000000000000000, -0.000000000000000000 ) ) ;
#60157 = CARTESIAN_POINT ( 'NONE',  ( 0.000000000000000000, -120.0000000000000000, -125.0000000000000000 ) ) ;
#60158 = DIRECTION ( 'NONE',  ( 0.000000000000000000, 0.000000000000000000, -1.000000000000000000 ) ) ;
#60159 = DIRECTION ( 'NONE',  ( 0.000000000000000000, 0.4067366430757887730, 0.9135454576426059736 ) ) ;
#60160 = AXIS2_PLACEMENT_3D ( 'NONE', #63492, #33402, #40928 ) ;
#60161 = CARTESIAN_POINT ( 'NONE',  ( 92.35000000000002274, -210.0000359395330634, 83.72937624475873974 ) ) ;
#60162 = CONICAL_SURFACE ( 'NONE', #55357, 20.64000000000000057, 0.7853981633974482790 ) ;
#60163 = AXIS2_PLACEMENT_3D ( 'NONE', #23693, #17314, #7517 ) ;
#60164 = DIRECTION ( 'NONE',  ( 0.000000000000000000, 0.000000000000000000, 1.000000000000000000 ) ) ;
#60165 = DIRECTION ( 'NONE',  ( 0.000000000000000000, 0.3826834323650904479, -0.9238795325112865164 ) ) ;
#60166 = CYLINDRICAL_SURFACE ( 'NONE', #63962, 16.00000000000000000 ) ;
#60167 = AXIS2_PLACEMENT_3D ( 'NONE', #11981, #63878, #28525 ) ;
#60168 = CARTESIAN_POINT ( 'NONE',  ( -97.64999999954994792, 89.99996890530464100, 88.81037122970319331 ) ) ;
#60169 = CARTESIAN_POINT ( 'NONE',  ( 10.00000000000000000, -0.8828120875898013420, -37.48860685352291711 ) ) ;
#60170 = EDGE_CURVE ( 'NONE', #1606, #28741, #41499, .T. ) ;
#60171 = CARTESIAN_POINT ( 'NONE',  ( -97.30629616937501680, 88.66845928578038638, 75.72572916753381378 ) ) ;
#60172 = DIRECTION ( 'NONE',  ( -1.000000000000000000, -0.000000000000000000, -0.000000000000000000 ) ) ;
#60173 = DIRECTION ( 'NONE',  ( -1.000000000000000000, 0.000000000000000000, 0.000000000000000000 ) ) ;
#60174 = DIRECTION ( 'NONE',  ( 0.000000000000000000, 0.4999999999999995004, -0.8660254037844389297 ) ) ;
#60175 = UNCERTAINTY_MEASURE_WITH_UNIT (LENGTH_MEASURE( 1.000000000000000082E-05 ), #57499, 'distance_accuracy_value', 'NONE');
#60176 = CARTESIAN_POINT ( 'NONE',  ( 5.000000000000002665, -71.87247863392443037, 39.47590169984818687 ) ) ;
#60177 = UNCERTAINTY_MEASURE_WITH_UNIT (LENGTH_MEASURE( 1.000000000000000082E-05 ), #35673, 'distance_accuracy_value', 'NONE');
#60178 = CARTESIAN_POINT ( 'NONE',  ( -92.34999999999999432, -211.5299782133524218, 84.62895833506763665 ) ) ;
#60179 = CARTESIAN_POINT ( 'NONE',  ( -95.00000000000002842, 90.00000000000004263, 90.00000000000000000 ) ) ;
#60180 = CARTESIAN_POINT ( 'NONE',  ( -0.0004442498525516064278, 0.001194404164626844313, -85.59999999999999432 ) ) ;
#60181 = LINE ( 'NONE', #54159, #39428 ) ;
#60182 = DIRECTION ( 'NONE',  ( -1.000000000000000000, 0.000000000000000000, 0.000000000000000000 ) ) ;
#60183 = CARTESIAN_POINT ( 'NONE',  ( -93.67499999999998295, -212.2949673200287179, 87.67166666666666686 ) ) ;
#60184 = ADVANCED_FACE ( 'NONE', ( #29879 ), #24618, .T. ) ;
#60185 = EDGE_CURVE ( 'NONE', #59223, #12564, #42687, .T. ) ;
#60186 = CYLINDRICAL_SURFACE ( 'NONE', #70973, 2.649999999999985700 ) ;
#60187 = ORIENTED_EDGE ( 'NONE', *, *, #45607, .F. ) ;
#60188 = CARTESIAN_POINT ( 'NONE',  ( 0.000000000000000000, 0.000000000000000000, 0.000000000000000000 ) ) ;
#60189 = CARTESIAN_POINT ( 'NONE',  ( 4.999999999999999112, -41.91543099594819921, 2.663952781846001816 ) ) ;
#60190 = EDGE_CURVE ( 'NONE', #54357, #46588, #53194, .T. ) ;
#60191 = CARTESIAN_POINT ( 'NONE',  ( -7.400000000000003908, -1.056673655988042765E-14, -5.892267102755452808E-15 ) ) ;
#60192 =( GEOMETRIC_REPRESENTATION_CONTEXT ( 3 ) GLOBAL_UNCERTAINTY_ASSIGNED_CONTEXT ( ( #49014 ) ) GLOBAL_UNIT_ASSIGNED_CONTEXT ( ( #5073, #45292, #67837 ) ) REPRESENTATION_CONTEXT ( 'NONE', 'WORKASPACE' ) );
#60193 = EDGE_LOOP ( 'NONE', ( #9822, #23728 ) ) ;
#60194 = DIRECTION ( 'NONE',  ( -1.000000000000000000, 0.000000000000000000, 0.000000000000000000 ) ) ;
#60195 = DIRECTION ( 'NONE',  ( 0.000000000000000000, 0.000000000000000000, -1.000000000000000000 ) ) ;
#60196 = VERTEX_POINT ( 'NONE', #70459 ) ;
#60197 = CARTESIAN_POINT ( 'NONE',  ( 97.30629616937498838, -209.9999999999999716, 82.34031250086714238 ) ) ;
#60198 = CARTESIAN_POINT ( 'NONE',  ( 97.30629616937498838, -208.6684592857803295, 88.26697916753381890 ) ) ;
#60199 = EDGE_CURVE ( 'NONE', #70437, #36744, #29462, .T. ) ;
#60200 = ORIENTED_EDGE ( 'NONE', *, *, #3284, .F. ) ;
#60201 = CARTESIAN_POINT ( 'NONE',  ( 97.30629616937498838, -211.3315407142195852, 86.89114583420050053 ) ) ;
#60202 = ORIENTED_EDGE ( 'NONE', *, *, #18935, .F. ) ;
#60203 = CARTESIAN_POINT ( 'NONE',  ( 0.000000000000000000, 0.000000000000000000, 0.000000000000000000 ) ) ;
#60204 = ORIENTED_EDGE ( 'NONE', *, *, #49496, .T. ) ;
#60205 = VECTOR ( 'NONE', #10660, 1000.000000000000000 ) ;
#60206 = CARTESIAN_POINT ( 'NONE',  ( -93.84685191531252713, 88.00268892867056536, 77.94822916753382458 ) ) ;
#60207 = CIRCLE ( 'NONE', #68587, 77.49900000000000944 ) ;
#60208 = EDGE_LOOP ( 'NONE', ( #68239, #30951, #41726, #12920 ) ) ;
#60209 = EDGE_LOOP ( 'NONE', ( #71595, #66845, #22513, #22853 ) ) ;
#60210 = CARTESIAN_POINT ( 'NONE',  ( -18.12185313557659683, -104.9634299478706794, -2.500000000000000000 ) ) ;
#60211 = AXIS2_PLACEMENT_3D ( 'NONE', #69404, #10792, #11883 ) ;
#60212 = EDGE_LOOP ( 'NONE', ( #20835, #39676, #59078, #31145, #73957, #58985, #21145, #3815 ) ) ;
#60213 = CARTESIAN_POINT ( 'NONE',  ( 92.34999999999999432, 90.00000000000002842, 88.17437500173430465 ) ) ;
#60214 = DIRECTION ( 'NONE',  ( 0.000000000000000000, -0.8910065241883722287, 0.4539904997395382558 ) ) ;
#60215 = ADVANCED_FACE ( 'NONE', ( #41915 ), #46446, .T. ) ;
#60216 = ORIENTED_EDGE ( 'NONE', *, *, #49113, .T. ) ;
#60217 = DIRECTION ( 'NONE',  ( -1.000000000000000000, 0.000000000000000000, 0.000000000000000000 ) ) ;
#60218 = EDGE_CURVE ( 'NONE', #18460, #47680, #33057, .T. ) ;
#60219 = ORIENTED_EDGE ( 'NONE', *, *, #41039, .T. ) ;
#60220 =( BOUNDED_CURVE ( )  B_SPLINE_CURVE ( 2, ( #30695, #53642, #64557, #41618, #19050, #1074, #18677 ),
 .UNSPECIFIED., .F., .F. ) 
 B_SPLINE_CURVE_WITH_KNOTS ( ( 3, 2, 2, 3 ),
 ( 0.3125000000000001665, 0.3194444444444445308, 0.3263888888888890061, 0.3333333333333333703 ),
 .UNSPECIFIED. ) 
 CURVE ( )  GEOMETRIC_REPRESENTATION_ITEM ( )  RATIONAL_B_SPLINE_CURVE ( ( 0.9999999999999967804, 0.8660254037844419273, 1.000000000000000000, 0.8660254037844387076, 1.000000000000000000, 0.8660254037844375974, 1.000000000000001110 ) ) 
 REPRESENTATION_ITEM ( '' )  );
#60221 = CARTESIAN_POINT ( 'NONE',  ( -0.9515373497862389396, -96.47140937769621871, -2.500000000000000000 ) ) ;
#60222 = ADVANCED_FACE ( 'NONE', ( #35162 ), #58100, .T. ) ;
#60223 = ORIENTED_EDGE ( 'NONE', *, *, #67484, .F. ) ;
#60224 = ORIENTED_EDGE ( 'NONE', *, *, #67240, .F. ) ;
#60225 = ORIENTED_EDGE ( 'NONE', *, *, #59410, .F. ) ;
#60226 = CARTESIAN_POINT ( 'NONE',  ( 97.30629616937498838, -209.9999999999999716, 79.80031250086713612 ) ) ;
#60227 = CARTESIAN_POINT ( 'NONE',  ( 0.000000000000000000, -12.42422080174663712, 35.38097989696507994 ) ) ;
#60228 = LINE ( 'NONE', #65490, #52183 ) ;
#60229 = ORIENTED_EDGE ( 'NONE', *, *, #30538, .F. ) ;
#60230 = VERTEX_POINT ( 'NONE', #995 ) ;
#60231 = DIRECTION ( 'NONE',  ( 0.000000000000000000, 0.7071067811865439090, 0.7071067811865512365 ) ) ;
#60232 = DIRECTION ( 'NONE',  ( 0.000000000000000000, 0.5000000000000003331, 0.8660254037844383745 ) ) ;
#60233 = ORIENTED_EDGE ( 'NONE', *, *, #25779, .F. ) ;
#60234 = CARTESIAN_POINT ( 'NONE',  ( 5.999999999999999112, 40.65526001592713357, -71.21200624218752750 ) ) ;
#60235 = FACE_OUTER_BOUND ( 'NONE', #39979, .T. ) ;
#60236 = CARTESIAN_POINT ( 'NONE',  ( -93.84685191531247028, -211.9973110713294489, 79.69447916753379957 ) ) ;
#60237 = CARTESIAN_POINT ( 'NONE',  ( -93.84685191531252713, 88.00268892867056536, 78.58322916753382970 ) ) ;
#60238 = ORIENTED_EDGE ( 'NONE', *, *, #10435, .F. ) ;
#60239 = CARTESIAN_POINT ( 'NONE',  ( 97.30629616937498838, 88.66845928578037217, 79.74739583420047495 ) ) ;
#60240 = VERTEX_POINT ( 'NONE', #23890 ) ;
#60241 = PLANE ( 'NONE',  #65989 ) ;
#60242 = CARTESIAN_POINT ( 'NONE',  ( 0.000000000000000000, 0.000000000000000000, 0.000000000000000000 ) ) ;
#60243 = CARTESIAN_POINT ( 'NONE',  ( 11.99999999999999822, 0.000000000000000000, 0.000000000000000000 ) ) ;
#60244 = PLANE ( 'NONE',  #69149 ) ;
#60245 = CARTESIAN_POINT ( 'NONE',  ( -97.65000000000001990, 90.00000000000004263, 90.00000000000000000 ) ) ;
#60246 = CARTESIAN_POINT ( 'NONE',  ( -93.84685191531248449, -208.0026889286704943, 83.71614583420047495 ) ) ;
#60247 = VECTOR ( 'NONE', #40345, 1000.000000000000000 ) ;
#60248 = DIRECTION ( 'NONE',  ( 1.000000000000000000, 0.000000000000000000, 0.000000000000000000 ) ) ;
#60249 = CARTESIAN_POINT ( 'NONE',  ( 10.00000000000000000, 77.32052557432849937, -5.256550761632002633 ) ) ;
#60250 = CARTESIAN_POINT ( 'NONE',  ( -7.670864526094549163, -97.73662565058241114, -5.500000000000000000 ) ) ;
#60251 = VERTEX_POINT ( 'NONE', #46826 ) ;
#60252 = CIRCLE ( 'NONE', #29041, 31.99999999999999289 ) ;
#60253 = ORIENTED_EDGE ( 'NONE', *, *, #10538, .F. ) ;
#60254 = CARTESIAN_POINT ( 'NONE',  ( 0.000000000000000000, 0.000000000000000000, -175.0000000000000000 ) ) ;
#60255 = DIRECTION ( 'NONE',  ( -0.000000000000000000, -0.000000000000000000, 1.000000000000000000 ) ) ;
#60256 = DIRECTION ( 'NONE',  ( 0.000000000000000000, 0.000000000000000000, -1.000000000000000000 ) ) ;
#60257 = CARTESIAN_POINT ( 'NONE',  ( -92.69370383062502583, 91.33154071421968467, 84.93322916753379559 ) ) ;
#60258 = CARTESIAN_POINT ( 'NONE',  ( 2.047646702416564768, -96.54137380445985173, 5.500000000000000000 ) ) ;
#60259 = DIRECTION ( 'NONE',  ( 0.000000000000000000, -0.1564344650402172687, -0.9876883405951399908 ) ) ;
#60260 = DIRECTION ( 'NONE',  ( 0.000000000000000000, 0.000000000000000000, 1.000000000000000000 ) ) ;
#60261 = ORIENTED_EDGE ( 'NONE', *, *, #10709, .T. ) ;
#60262 = DIRECTION ( 'NONE',  ( 1.000000000000000000, 0.000000000000000000, 0.000000000000000000 ) ) ;
#60263 = EDGE_CURVE ( 'NONE', #42705, #7392, #706, .T. ) ;
#60264 = AXIS2_PLACEMENT_3D ( 'NONE', #40261, #28976, #63210 ) ;
#60265 = FACE_OUTER_BOUND ( 'NONE', #8773, .T. ) ;
#60266 = VECTOR ( 'NONE', #12303, 1000.000000000000000 ) ;
#60267 = DIRECTION ( 'NONE',  ( 0.000000000000000000, 0.8090169943749447867, 0.5877852522924769119 ) ) ;
#60268 = LINE ( 'NONE', #13999, #22567 ) ;
#60269 = CARTESIAN_POINT ( 'NONE',  ( -12.00000000000000000, 2.119128821244579932E-15, 17.30399999999999849 ) ) ;
#60270 = CARTESIAN_POINT ( 'NONE',  ( 96.32499999999998863, -212.2949673200287179, 82.59166666666665435 ) ) ;
#60271 = CARTESIAN_POINT ( 'NONE',  ( -92.69370383062498320, -208.6684592857803011, 82.55197916753382970 ) ) ;
#60272 = AXIS2_PLACEMENT_3D ( 'NONE', #59527, #24931, #29447 ) ;
#60273 = EDGE_CURVE ( 'NONE', #27539, #59857, #5519, .T. ) ;
#60274 = EDGE_CURVE ( 'NONE', #47167, #63004, #8065, .T. ) ;
#60275 = CARTESIAN_POINT ( 'NONE',  ( 0.000000000000000000, -30.00120703465189465, -22.64427369931201639 ) ) ;
#60276 = CARTESIAN_POINT ( 'NONE',  ( 12.00000000000000000, -3.948201729842032215, 23.21447184625297666 ) ) ;
#60277 = DIRECTION ( 'NONE',  ( -1.000000000000000000, 0.000000000000000000, 0.000000000000000000 ) ) ;
#60278 = CARTESIAN_POINT ( 'NONE',  ( 10.00000000000000000, -29.81001611431024756, 22.74946021919122785 ) ) ;
#60279 = ORIENTED_EDGE ( 'NONE', *, *, #59590, .T. ) ;
#60280 = EDGE_CURVE ( 'NONE', #49170, #3025, #30986, .T. ) ;
#60281 = DIRECTION ( 'NONE',  ( 0.000000000000000000, 0.000000000000000000, 1.000000000000000000 ) ) ;
#60282 = CARTESIAN_POINT ( 'NONE',  ( -93.67500000000003979, 92.29496732002878900, 78.35833333333333428 ) ) ;
#60283 = CARTESIAN_POINT ( 'NONE',  ( 12.49999999999999645, 1.530808498934191127E-15, 52.00000000000002132 ) ) ;
#60284 = DIRECTION ( 'NONE',  ( -1.000000000000000000, -0.000000000000000000, -0.000000000000000000 ) ) ;
#60285 = ORIENTED_EDGE ( 'NONE', *, *, #39, .F. ) ;
#60286 = LINE ( 'NONE', #11900, #60069 ) ;
#60287 = SURFACE_SIDE_STYLE ('',( #3516 ) ) ;
#60288 = EDGE_CURVE ( 'NONE', #48071, #32115, #65593, .T. ) ;
#60289 = EDGE_LOOP ( 'NONE', ( #46522, #41050, #18612, #3544 ) ) ;
#60290 = CARTESIAN_POINT ( 'NONE',  ( 0.000000000000000000, 21.40280677340421889, -36.13751322684397138 ) ) ;
#60291 = EDGE_CURVE ( 'NONE', #62567, #20422, #9175, .T. ) ;
#60292 = VERTEX_POINT ( 'NONE', #59578 ) ;
#60293 =( GEOMETRIC_REPRESENTATION_CONTEXT ( 3 ) GLOBAL_UNCERTAINTY_ASSIGNED_CONTEXT ( ( #72998 ) ) GLOBAL_UNIT_ASSIGNED_CONTEXT ( ( #4459, #73591, #67966 ) ) REPRESENTATION_CONTEXT ( 'NONE', 'WORKASPACE' ) );
#60294 = VECTOR ( 'NONE', #60156, 1000.000000000000000 ) ;
#60295 = DIRECTION ( 'NONE',  ( 0.000000000000000000, -0.000000000000000000, 1.000000000000000000 ) ) ;
#60296 = VECTOR ( 'NONE', #74252, 1000.000000000000000 ) ;
#60297 = ORIENTED_EDGE ( 'NONE', *, *, #56268, .F. ) ;
#60298 = ORIENTED_EDGE ( 'NONE', *, *, #62579, .F. ) ;
#60299 = ORIENTED_EDGE ( 'NONE', *, *, #3150, .F. ) ;
#60300 = ORIENTED_EDGE ( 'NONE', *, *, #27220, .F. ) ;
#60301 = DIRECTION ( 'NONE',  ( -0.000000000000000000, -0.000000000000000000, 1.000000000000000000 ) ) ;
#60302 = AXIS2_PLACEMENT_3D ( 'NONE', #42120, #54137, #53755 ) ;
#60303 = EDGE_CURVE ( 'NONE', #19443, #6124, #20077, .T. ) ;
#60304 = ORIENTED_EDGE ( 'NONE', *, *, #38543, .F. ) ;
#60305 = ADVANCED_FACE ( 'NONE', ( #59205 ), #3566, .F. ) ;
#60306 = CIRCLE ( 'NONE', #68683, 82.00000000000000000 ) ;
#60307 = ORIENTED_EDGE ( 'NONE', *, *, #35712, .F. ) ;
#60308 = CARTESIAN_POINT ( 'NONE',  ( 93.84685191531248449, 91.99731107132950569, 78.90072916753382515 ) ) ;
#60309 = CARTESIAN_POINT ( 'NONE',  ( 4.999999999999999112, -40.98264845739743123, -9.188173127307734944 ) ) ;
#60310 = DIRECTION ( 'NONE',  ( 1.000000000000000000, 1.427937372958405461E-15, 7.962523111839130290E-16 ) ) ;
#60311 = ORIENTED_EDGE ( 'NONE', *, *, #33439, .T. ) ;
#60312 = ORIENTED_EDGE ( 'NONE', *, *, #35419, .T. ) ;
#60313 = ORIENTED_EDGE ( 'NONE', *, *, #17516, .F. ) ;
#60314 = CARTESIAN_POINT ( 'NONE',  ( 0.000000000000000000, 41.76937507738788469, 62.50329211542452157 ) ) ;
#60315 = ORIENTED_EDGE ( 'NONE', *, *, #58551, .F. ) ;
#60316 = AXIS2_PLACEMENT_3D ( 'NONE', #22780, #69006, #67890 ) ;
#60317 = DIRECTION ( 'NONE',  ( 5.551115123125782702E-17, 2.775557561562891351E-17, 1.000000000000000000 ) ) ;
#60318 = CARTESIAN_POINT ( 'NONE',  ( 12.00000000000000000, 16.83928648764922542, -16.46020748918050458 ) ) ;
#60319 = CARTESIAN_POINT ( 'NONE',  ( -97.19210266091323547, 91.16770611573559790, 74.89296886168685319 ) ) ;
#60320 = CARTESIAN_POINT ( 'NONE',  ( 5.000000000000000000, 39.04073710021344112, 15.48615015657596850 ) ) ;
#60321 = DIRECTION ( 'NONE',  ( -0.000000000000000000, -0.000000000000000000, -1.000000000000000000 ) ) ;
#60322 = CARTESIAN_POINT ( 'NONE',  ( -8.000000000000012434, 2.391149348467643667E-13, 22.89999999999999503 ) ) ;
#60323 = DIRECTION ( 'NONE',  ( -1.000000000000000000, 0.000000000000000000, 0.000000000000000000 ) ) ;
#60324 = CARTESIAN_POINT ( 'NONE',  ( -97.30629616937497417, -208.6684592857803011, 89.58989583420047609 ) ) ;
#60325 = CARTESIAN_POINT ( 'NONE',  ( -97.30629616937501680, 91.33154071421968467, 87.84364583420048689 ) ) ;
#60326 = ORIENTED_EDGE ( 'NONE', *, *, #59435, .F. ) ;
#60328 = CARTESIAN_POINT ( 'NONE',  ( -95.00000000000002842, 87.33691857156074434, 88.53156250086713897 ) ) ;
#60327 = CARTESIAN_POINT ( 'NONE',  ( 92.34999999999999432, 88.47002178664753558, 74.89229166840097207 ) ) ;
#60329 = ORIENTED_EDGE ( 'NONE', *, *, #70616, .F. ) ;
#60330 = CARTESIAN_POINT ( 'NONE',  ( 94.99999999999998579, 92.66308142843935514, 76.30781250086715772 ) ) ;
#60331 = CARTESIAN_POINT ( 'NONE',  ( 10.00000000000000000, -75.54627589209931671, -17.28742895386164591 ) ) ;
#60332 = CARTESIAN_POINT ( 'NONE',  ( 97.64999999999690772, -210.0000040461968638, 77.06187486178042434 ) ) ;
#60333 = PLANE ( 'NONE',  #23060 ) ;
#60334 = DIRECTION ( 'NONE',  ( -1.000000000000000000, 0.000000000000000000, 0.000000000000000000 ) ) ;
#60335 = DIRECTION ( 'NONE',  ( -1.000000000000000000, -0.000000000000000000, -0.000000000000000000 ) ) ;
#60336 = DIRECTION ( 'NONE',  ( 0.000000000000000000, 0.000000000000000000, 1.000000000000000000 ) ) ;
#60337 = VERTEX_POINT ( 'NONE', #2099 ) ;
#60338 = VERTEX_POINT ( 'NONE', #26090 ) ;
#60339 = CARTESIAN_POINT ( 'NONE',  ( 4.999999999999999112, -9.188173127307592836, 40.98264845739746676 ) ) ;
#60340 = DIRECTION ( 'NONE',  ( -0.000000000000000000, 0.9510565162951539753, 0.3090169943749461745 ) ) ;
#60341 = CARTESIAN_POINT ( 'NONE',  ( 10.00000000000000000, -68.26794271651286294, 31.47745569255117104 ) ) ;
#60342 = CARTESIAN_POINT ( 'NONE',  ( 0.000000000000000000, 0.000000000000000000, -44.99999999999998579 ) ) ;
#60343 = DIRECTION ( 'NONE',  ( 0.000000000000000000, 0.000000000000000000, 1.000000000000000000 ) ) ;
#60344 = CARTESIAN_POINT ( 'NONE',  ( -92.69370383062498320, -209.9999999999999716, 74.87906250086714977 ) ) ;
#60345 = ORIENTED_EDGE ( 'NONE', *, *, #50593, .T. ) ;
#60346 = ADVANCED_FACE ( 'NONE', ( #49020 ), #71202, .T. ) ;
#60347 = DIRECTION ( 'NONE',  ( 0.000000000000000000, 0.7604059656000277112, 0.6494480483301875440 ) ) ;
#60348 = B_SPLINE_CURVE_WITH_KNOTS ( 'NONE', 3,
 ( #11859, #41931, #23900, #23526 ),
 .UNSPECIFIED., .F., .F.,
 ( 4, 4 ),
 ( 2.446487931514598506E-06, 1.000000000000000000 ),
 .UNSPECIFIED. ) ;
#60349 = CARTESIAN_POINT ( 'NONE',  ( 95.00000000000000000, -209.9999999999999716, 90.00000000000000000 ) ) ;
#60350 = EDGE_CURVE ( 'NONE', #1809, #71558, #65973, .T. ) ;
#60351 = AXIS2_PLACEMENT_3D ( 'NONE', #14431, #8795, #30600 ) ;
#60352 = CARTESIAN_POINT ( 'NONE',  ( 10.00000000000000000, 21.32104025579114648, 30.84782396557224970 ) ) ;
#60353 = DIRECTION ( 'NONE',  ( 0.000000000000000000, 0.000000000000000000, 1.000000000000000000 ) ) ;
#60354 = ADVANCED_FACE ( 'NONE', ( #25366 ), #55037, .F. ) ;
#60355 = PLANE ( 'NONE',  #11289 ) ;
#60356 = CARTESIAN_POINT ( 'NONE',  ( -3.000000000000000000, -25.60904388321925396, 6.976881207771172377 ) ) ;
#60357 = EDGE_CURVE ( 'NONE', #41327, #35941, #42297, .T. ) ;
#60358 = DIRECTION ( 'NONE',  ( 0.000000000000000000, -0.8660254037844427044, 0.4999999999999929501 ) ) ;
#60359 = DIRECTION ( 'NONE',  ( -1.000000000000000000, 0.000000000000000000, -0.000000000000000000 ) ) ;
#60360 = AXIS2_PLACEMENT_3D ( 'NONE', #65605, #55050, #65238 ) ;
#60361 = CIRCLE ( 'NONE', #14664, 11.59999999999999787 ) ;
#60362 = CARTESIAN_POINT ( 'NONE',  ( 93.84685191531248449, 88.00268892867053694, 82.92239583420048632 ) ) ;
#60363 = CARTESIAN_POINT ( 'NONE',  ( -94.99999999999997158, -212.6630814284392557, 84.88031250086713442 ) ) ;
#60364 = PLANE ( 'NONE',  #47003 ) ;
#60365 = VERTEX_POINT ( 'NONE', #42656 ) ;
#60366 = ADVANCED_FACE ( 'NONE', ( #14061 ), #43031, .F. ) ;
#60367 = CYLINDRICAL_SURFACE ( 'NONE', #61685, 31.99999999999999289 ) ;
#60368 = CARTESIAN_POINT ( 'NONE',  ( -92.34999999999999432, -209.9999999999999716, 78.25249999999999773 ) ) ;
#60369 = DIRECTION ( 'NONE',  ( -0.000000000000000000, -0.000000000000000000, 1.000000000000000000 ) ) ;
#60370 = AXIS2_PLACEMENT_3D ( 'NONE', #65607, #71216, #59594 ) ;
#60371 = VECTOR ( 'NONE', #15854, 1000.000000000000000 ) ;
#60372 = CARTESIAN_POINT ( 'NONE',  ( 97.30629616937498838, -209.9999999999999716, 84.24531250086714351 ) ) ;
#60373 = VERTEX_POINT ( 'NONE', #8448 ) ;
#60374 = LINE ( 'NONE', #9959, #64716 ) ;
#60375 = EDGE_CURVE ( 'NONE', #7056, #64121, #14814, .T. ) ;
#60376 = VERTEX_POINT ( 'NONE', #54311 ) ;
#60377 = EDGE_CURVE ( 'NONE', #18834, #33464, #31874, .T. ) ;
#60378 = ORIENTED_EDGE ( 'NONE', *, *, #73929, .T. ) ;
#60379 = CARTESIAN_POINT ( 'NONE',  ( 10.00000000000000000, -21.53537804866058991, -30.80686688397033635 ) ) ;
#60380 = EDGE_CURVE ( 'NONE', #49000, #60113, #45110, .T. ) ;
#60381 = EDGE_CURVE ( 'NONE', #42834, #7474, #62188, .T. ) ;
#60382 = ORIENTED_EDGE ( 'NONE', *, *, #68495, .T. ) ;
#60383 = CARTESIAN_POINT ( 'NONE',  ( 97.30629616937498838, -209.9999999999999716, 77.41906250086715602 ) ) ;
#60384 = CYLINDRICAL_SURFACE ( 'NONE', #39282, 82.00000000000000000 ) ;
#60385 = EDGE_CURVE ( 'NONE', #13857, #21232, #67056, .T. ) ;
#60386 = APPLICATION_CONTEXT ( 'automotive_design' ) ;
#60387 = DIRECTION ( 'NONE',  ( -0.000000000000000000, -0.000000000000000000, -1.000000000000000000 ) ) ;
#60388 = CYLINDRICAL_SURFACE ( 'NONE', #48467, 16.00000000000000000 ) ;
#60389 = CARTESIAN_POINT ( 'NONE',  ( 0.000000000000000000, 0.000000000000000000, 0.000000000000000000 ) ) ;
#60390 = DIRECTION ( 'NONE',  ( 0.000000000000000000, 0.000000000000000000, 1.000000000000000000 ) ) ;
#60391 = CARTESIAN_POINT ( 'NONE',  ( 92.35000000000002274, -211.5299782133524502, 82.43291666666665662 ) ) ;
#60392 = ORIENTED_EDGE ( 'NONE', *, *, #38173, .F. ) ;
#60393 = EDGE_CURVE ( 'NONE', #14549, #35308, #68177, .T. ) ;
#60394 = PRODUCT_DEFINITION_FORMATION_WITH_SPECIFIED_SOURCE ( 'ANY', '', #31948, .NOT_KNOWN. ) ;
#60395 = ORIENTED_EDGE ( 'NONE', *, *, #74204, .T. ) ;
#60396 = ORIENTED_EDGE ( 'NONE', *, *, #21202, .F. ) ;
#60397 = ORIENTED_EDGE ( 'NONE', *, *, #36314, .T. ) ;
#60398 = CARTESIAN_POINT ( 'NONE',  ( 5.000000000000002665, 40.65526001592612459, 71.21200624218811015 ) ) ;
#60399 = AXIS2_PLACEMENT_3D ( 'NONE', #9502, #55737, #27144 ) ;
#60400 = CARTESIAN_POINT ( 'NONE',  ( -92.69370383062504004, 90.00000000000004263, 82.49906250086715431 ) ) ;
#60401 = CARTESIAN_POINT ( 'NONE',  ( 11.99999999999999822, 0.000000000000000000, 0.000000000000000000 ) ) ;
#60402 = CYLINDRICAL_SURFACE ( 'NONE', #3046, 16.00000000000000000 ) ;
#60403 = DIRECTION ( 'NONE',  ( -0.000000000000000000, -0.000000000000000000, 1.000000000000000000 ) ) ;
#60404 = CARTESIAN_POINT ( 'NONE',  ( -92.34999999999999432, -211.5299782133524218, 83.99395833506763154 ) ) ;
#60405 = ORIENTED_EDGE ( 'NONE', *, *, #29596, .T. ) ;
#60406 = CARTESIAN_POINT ( 'NONE',  ( -92.34999999999999432, -208.4700217866474645, 86.63979166840097434 ) ) ;
#60407 = ORIENTED_EDGE ( 'NONE', *, *, #42139, .T. ) ;
#60408 = LINE ( 'NONE', #49105, #23017 ) ;
#60409 = EDGE_LOOP ( 'NONE', ( #35525, #7048, #40111, #19802 ) ) ;
#60410 = CARTESIAN_POINT ( 'NONE',  ( -92.35000000000005116, 88.47002178664754979, 83.99395833506763154 ) ) ;
#60411 = AXIS2_PLACEMENT_3D ( 'NONE', #44091, #61391, #9873 ) ;
#60412 = ORIENTED_EDGE ( 'NONE', *, *, #20965, .F. ) ;
#60413 = CARTESIAN_POINT ( 'NONE',  ( 94.99999999999998579, 87.33691857156068750, 85.51531250086713953 ) ) ;
#60414 = DIRECTION ( 'NONE',  ( 1.000000000000000000, 0.000000000000000000, -0.000000000000000000 ) ) ;
#60415 = CARTESIAN_POINT ( 'NONE',  ( -17.09243336300205129, -103.8724235629982502, 2.500000000000000000 ) ) ;
#60416 = CARTESIAN_POINT ( 'NONE',  ( -92.69370383062502583, 90.00000000000007105, 74.79348190356851944 ) ) ;
#60417 = CARTESIAN_POINT ( 'NONE',  ( 92.35000000000007958, 88.47002178664749295, 88.78291666666667936 ) ) ;
#60418 = CARTESIAN_POINT ( 'NONE',  ( 12.00000000000000000, 22.07842321921480888, -8.187992925817425771 ) ) ;
#60419 = VERTEX_POINT ( 'NONE', #67433 ) ;
#60420 = CARTESIAN_POINT ( 'NONE',  ( 10.00000000000000000, 0.000000000000000000, 0.000000000000000000 ) ) ;
#60421 = AXIS2_PLACEMENT_3D ( 'NONE', #70570, #42035, #34913 ) ;
#60422 = VECTOR ( 'NONE', #15767, 1000.000000000000114 ) ;
#60423 = DIRECTION ( 'NONE',  ( -1.000000000000000000, 0.000000000000000000, 0.000000000000000000 ) ) ;
#60424 = ORIENTED_EDGE ( 'NONE', *, *, #31246, .F. ) ;
#60425 = ORIENTED_EDGE ( 'NONE', *, *, #2176, .F. ) ;
#60426 = DIRECTION ( 'NONE',  ( -1.000000000000000000, -0.000000000000000000, 0.000000000000000000 ) ) ;
#60427 = FACE_OUTER_BOUND ( 'NONE', #15191, .T. ) ;
#60428 = CYLINDRICAL_SURFACE ( 'NONE', #26930, 2.649999999999985700 ) ;
#60429 = CARTESIAN_POINT ( 'NONE',  ( -96.15314808468745866, -211.9973110713294489, 83.55739583420049144 ) ) ;
#60430 = ORIENTED_EDGE ( 'NONE', *, *, #16810, .F. ) ;
#60431 = CARTESIAN_POINT ( 'NONE',  ( 0.000000000000000000, 5.773502691896262640, -6.000000000000000000 ) ) ;
#60432 = VERTEX_POINT ( 'NONE', #73052 ) ;
#60433 = B_SPLINE_CURVE_WITH_KNOTS ( 'NONE', 1,
 ( #31002, #37026 ),
 .UNSPECIFIED., .F., .F.,
 ( 2, 2 ),
 ( 0.000000000000000000, 1.000000000000000000 ),
 .UNSPECIFIED. ) ;
#60434 = ADVANCED_FACE ( 'NONE', ( #27578 ), #21941, .F. ) ;
#60435 = CARTESIAN_POINT ( 'NONE',  ( 92.69370383062501162, -209.9999999999999716, 89.80156250086714920 ) ) ;
#60436 = LINE ( 'NONE', #25473, #55146 ) ;
#60437 = ADVANCED_FACE ( 'NONE', ( #32834 ), #10288, .T. ) ;
#60438 = DIRECTION ( 'NONE',  ( 0.000000000000000000, -0.9969173337331270757, -0.07845909572785580988 ) ) ;
#60439 = CARTESIAN_POINT ( 'NONE',  ( 97.30629616937498838, 91.33154071421968467, 76.67822916753378593 ) ) ;
#60440 = DIRECTION ( 'NONE',  ( -0.9730327541852491491, 0.2306669878475648139, 0.000000000000000000 ) ) ;
#60441 = CARTESIAN_POINT ( 'NONE',  ( 15.00000000000000000, -25.60904388321925040, -6.976881207771165272 ) ) ;
#60442 = DIRECTION ( 'NONE',  ( -1.000000000000000000, 0.000000000000000000, -0.000000000000000000 ) ) ;
#60443 = CARTESIAN_POINT ( 'NONE',  ( 95.05423112903699234, 92.38875495131965465, 74.83591575723767164 ) ) ;
#60444 = EDGE_CURVE ( 'NONE', #6493, #15073, #42739, .T. ) ;
#60446 = EDGE_CURVE ( 'NONE', #44982, #14031, #31938, .T. ) ;
#60445 = CARTESIAN_POINT ( 'NONE',  ( -93.67500000000003979, 87.70503267997129626, 76.95604166840095672 ) ) ;
#60447 = CARTESIAN_POINT ( 'NONE',  ( 92.35000000000006537, -211.5299782133524786, 84.33791666666667197 ) ) ;
#60448 = CIRCLE ( 'NONE', #18395, 31.99999999999999289 ) ;
#60449 =( BOUNDED_CURVE ( )  B_SPLINE_CURVE ( 2, ( #36900, #48189, #71471, #2737, #47814, #4106, #65856, #30880, #7233, #25265, #25623 ),
 .UNSPECIFIED., .F., .F. ) 
 B_SPLINE_CURVE_WITH_KNOTS ( ( 3, 2, 2, 2, 2, 3 ),
 ( 0.6985206468877303010, 0.6985207885507850323, 0.7055765540917019463, 0.7126323196326189713, 0.7196880851735359963, 0.7196881748069930973 ),
 .UNSPECIFIED. ) 
 CURVE ( )  GEOMETRIC_REPRESENTATION_ITEM ( )  RATIONAL_B_SPLINE_CURVE ( ( 0.9999946203230871689, 0.9999973101075368964, 1.000000000000000000, 0.8660254037844387076, 1.000000000000000000, 0.8660254037844387076, 1.000000000000000000, 0.8660254037844387076, 1.000000000000000000, 0.9999982980434729551, 0.9999965961301877648 ) ) 
 REPRESENTATION_ITEM ( '' )  );
#60450 = DIRECTION ( 'NONE',  ( 1.000000000000000000, 0.000000000000000000, 0.000000000000000000 ) ) ;
#60451 = CARTESIAN_POINT ( 'NONE',  ( 0.000000000000000000, 62.50329211542435104, 41.76937507738811917 ) ) ;
#60452 = ORIENTED_EDGE ( 'NONE', *, *, #65058, .F. ) ;
#60453 = CARTESIAN_POINT ( 'NONE',  ( -92.69370383062504004, 90.00000000000004263, 82.97531250086714749 ) ) ;
#60454 = CARTESIAN_POINT ( 'NONE',  ( 0.000000000000000000, 0.000000000000000000, 0.000000000000000000 ) ) ;
#60455 = CIRCLE ( 'NONE', #40006, 16.00000000000000711 ) ;
#60456 = EDGE_CURVE ( 'NONE', #25971, #33774, #29519, .T. ) ;
#60457 = FACE_OUTER_BOUND ( 'NONE', #33968, .T. ) ;
#60458 = ORIENTED_EDGE ( 'NONE', *, *, #14410, .T. ) ;
#60459 = CIRCLE ( 'NONE', #31610, 82.00000000000000000 ) ;
#60460 = CARTESIAN_POINT ( 'NONE',  ( 0.000000000000000000, 0.000000000000000000, 0.000000000000000000 ) ) ;
#60462 = FACE_OUTER_BOUND ( 'NONE', #51682, .T. ) ;
#60461 = VECTOR ( 'NONE', #63418, 1000.000000000000000 ) ;
#60463 = DIRECTION ( 'NONE',  ( 1.000000000000000000, 1.343011723336883198E-16, -0.000000000000000000 ) ) ;
#60464 = VECTOR ( 'NONE', #33704, 1000.000000000000114 ) ;
#60465 = VECTOR ( 'NONE', #44349, 1000.000000000000000 ) ;
#60466 = CARTESIAN_POINT ( 'NONE',  ( 92.35000000046503033, 89.99996900126896548, 83.09538598081184091 ) ) ;
#60467 = EDGE_CURVE ( 'NONE', #67018, #20918, #34358, .T. ) ;
#60469 = EDGE_CURVE ( 'NONE', #48031, #36613, #45641, .T. ) ;
#60468 = VECTOR ( 'NONE', #39169, 1000.000000000000000 ) ;
#60470 = CARTESIAN_POINT ( 'NONE',  ( 93.84685191531251292, -211.9973110713294489, 78.47739583420049314 ) ) ;
#60471 = ORIENTED_EDGE ( 'NONE', *, *, #26968, .T. ) ;
#60472 = VERTEX_POINT ( 'NONE', #73802 ) ;
#60473 = DIRECTION ( 'NONE',  ( 0.7533909544171998318, 0.6575728627325954090, 0.000000000000000000 ) ) ;
#60474 = DIRECTION ( 'NONE',  ( -1.000000000000000000, -0.000000000000000000, -0.000000000000000000 ) ) ;
#60475 = DIRECTION ( 'NONE',  ( 1.000000000000000000, -0.000000000000000000, -0.000000000000000000 ) ) ;
#60476 = ORIENTED_EDGE ( 'NONE', *, *, #52280, .T. ) ;
#60477 = CARTESIAN_POINT ( 'NONE',  ( 10.00000000000000000, -39.04073710021333454, -15.48615015657624738 ) ) ;
#60478 = CARTESIAN_POINT ( 'NONE',  ( 92.69370383062501162, -211.3315407142195852, 77.78947916753381264 ) ) ;
#60479 = AXIS2_PLACEMENT_3D ( 'NONE', #58933, #30339, #11939 ) ;
#60480 = VERTEX_POINT ( 'NONE', #33961 ) ;
#60481 = DIRECTION ( 'NONE',  ( -1.000000000000000000, -0.000000000000000000, -0.000000000000000000 ) ) ;
#60482 = ORIENTED_EDGE ( 'NONE', *, *, #22345, .F. ) ;
#60483 = ORIENTED_EDGE ( 'NONE', *, *, #46700, .T. ) ;
#60484 = DIRECTION ( 'NONE',  ( 0.000000000000000000, 0.000000000000000000, 1.000000000000000000 ) ) ;
#60485 = CARTESIAN_POINT ( 'NONE',  ( 97.64999999999999147, -209.9999999999999716, 90.00000000000000000 ) ) ;
#60486 = ORIENTED_EDGE ( 'NONE', *, *, #57967, .T. ) ;
#60487 = DIRECTION ( 'NONE',  ( -1.000000000000000000, -0.000000000000000000, 0.000000000000000000 ) ) ;
#60488 = CARTESIAN_POINT ( 'NONE',  ( 95.00000000000000000, -213.0599564267049857, 80.07812500173432113 ) ) ;
#60489 = CARTESIAN_POINT ( 'NONE',  ( 97.64999999999997726, 91.52997821335252127, 85.92541666666664923 ) ) ;
#60490 = VERTEX_POINT ( 'NONE', #62171 ) ;
#60491 = DIRECTION ( 'NONE',  ( 0.000000000000000000, 0.000000000000000000, -1.000000000000000000 ) ) ;
#60492 = LINE ( 'NONE', #65750, #53701 ) ;
#60493 = AXIS2_PLACEMENT_3D ( 'NONE', #71837, #53453, #1990 ) ;
#60494 = EDGE_LOOP ( 'NONE', ( #38806, #41346, #32886, #69067 ) ) ;
#60495 = ORIENTED_EDGE ( 'NONE', *, *, #16445, .F. ) ;
#60496 = CARTESIAN_POINT ( 'NONE',  ( -92.69370383062504004, 90.00000000000004263, 89.48406250086715374 ) ) ;
#60497 = CARTESIAN_POINT ( 'NONE',  ( 97.30629616937498838, 91.33154071421968467, 80.48822916753383083 ) ) ;
#60498 = VERTEX_POINT ( 'NONE', #10656 ) ;
#60499 = CARTESIAN_POINT ( 'NONE',  ( 96.32499999999997442, 92.29496732002878900, 81.61270833506763722 ) ) ;
#60500 = CIRCLE ( 'NONE', #58071, 15.77977592589476608 ) ;
#60501 = CARTESIAN_POINT ( 'NONE',  ( 0.000000000000000000, 21.60688246758586928, 79.10210256391376049 ) ) ;
#60502 = VERTEX_POINT ( 'NONE', #45258 ) ;
#60503 = DIRECTION ( 'NONE',  ( 0.000000000000000000, 0.9510565162951503115, -0.3090169943749573878 ) ) ;
#60504 = EDGE_LOOP ( 'NONE', ( #32058, #55479, #63815, #63566 ) ) ;
#60505 = AXIS2_PLACEMENT_3D ( 'NONE', #35951, #6295, #58902 ) ;
#60506 = ORIENTED_EDGE ( 'NONE', *, *, #21384, .T. ) ;
#60507 = VERTEX_POINT ( 'NONE', #9552 ) ;
#60508 = DIRECTION ( 'NONE',  ( 0.000000000000000000, 0.000000000000000000, 1.000000000000000000 ) ) ;
#60509 = VERTEX_POINT ( 'NONE', #4671 ) ;
#60510 = DIRECTION ( 'NONE',  ( -1.000000000000000000, -0.000000000000000000, -0.000000000000000000 ) ) ;
#60511 = AXIS2_PLACEMENT_3D ( 'NONE', #72559, #44015, #66930 ) ;
#60512 = CARTESIAN_POINT ( 'NONE',  ( 92.34999999999999432, 88.47002178664753558, 88.22729166840096582 ) ) ;
#60513 = ORIENTED_EDGE ( 'NONE', *, *, #66, .T. ) ;
#60514 = DIRECTION ( 'NONE',  ( -1.000000000000000000, -0.000000000000000000, -0.000000000000000000 ) ) ;
#60515 = CARTESIAN_POINT ( 'NONE',  ( -97.30629616937497417, -211.3315407142195852, 80.80572916753382628 ) ) ;
#60516 = VERTEX_POINT ( 'NONE', #39613 ) ;
#60517 = CIRCLE ( 'NONE', #68944, 22.90000000000041780 ) ;
#60518 = DIRECTION ( 'NONE',  ( 0.000000000000000000, 0.000000000000000000, 1.000000000000000000 ) ) ;
#60519 = CYLINDRICAL_SURFACE ( 'NONE', #10418, 31.99999999999998579 ) ;
#60520 = DIRECTION ( 'NONE',  ( -1.000000000000000000, 0.000000000000000000, 0.000000000000000000 ) ) ;
#60521 = CARTESIAN_POINT ( 'NONE',  ( -2.977765906491215642, 1.932465207890948911E-15, 15.77977592589476608 ) ) ;
#60522 = EDGE_CURVE ( 'NONE', #58263, #27808, #21560, .T. ) ;
#60523 = DIRECTION ( 'NONE',  ( 0.000000000000000000, 0.000000000000000000, 1.000000000000000000 ) ) ;
#60524 = VECTOR ( 'NONE', #32864, 1000.000000000000000 ) ;
#60525 = AXIS2_PLACEMENT_3D ( 'NONE', #28613, #29349, #51554 ) ;
#60526 = EDGE_CURVE ( 'NONE', #41089, #32222, #49757, .T. ) ;
#60527 = CARTESIAN_POINT ( 'NONE',  ( 10.00000000000000178, 0.000000000000000000, 0.000000000000000000 ) ) ;
#60528 = CARTESIAN_POINT ( 'NONE',  ( 92.69370383062498320, 91.33154071421968467, 88.95489583420048518 ) ) ;
#60529 = CARTESIAN_POINT ( 'NONE',  ( -3.308722450212110699E-21, 16.95692799528845640, -2.500000000000000000 ) ) ;
#60530 = CARTESIAN_POINT ( 'NONE',  ( 99.99999999999998579, 95.00000000000002842, -90.00000000000000000 ) ) ;
#60532 = ADVANCED_FACE ( 'NONE', ( #55410 ), #50877, .F. ) ;
#60531 = CARTESIAN_POINT ( 'NONE',  ( -96.32499999999996021, -207.7050326799711968, 86.79854166840097207 ) ) ;
#60533 = CARTESIAN_POINT ( 'NONE',  ( 10.00000000000000000, 5.202137450156389953, 37.22597642581160216 ) ) ;
#60534 = CARTESIAN_POINT ( 'NONE',  ( 10.00000000000000000, 0.000000000000000000, 0.000000000000000000 ) ) ;
#60535 = DIRECTION ( 'NONE',  ( -1.000000000000000000, 0.000000000000000000, 0.000000000000000000 ) ) ;
#60536 = EDGE_CURVE ( 'NONE', #70328, #13032, #55931, .T. ) ;
#60537 = CYLINDRICAL_SURFACE ( 'NONE', #70052, 2.649999999999985700 ) ;
#60538 = VECTOR ( 'NONE', #15167, 1000.000000000000000 ) ;
#60539 = CARTESIAN_POINT ( 'NONE',  ( 10.00000000000000000, -16.45098606841149902, 33.79645857604508308 ) ) ;
#60540 = CARTESIAN_POINT ( 'NONE',  ( -3.000000000000000000, -10.45096189432344147, 21.10159698893426494 ) ) ;
#60541 = CARTESIAN_POINT ( 'NONE',  ( 0.000000000000000000, 56.15606465354958488, 59.75363087400094741 ) ) ;
#60542 = DIRECTION ( 'NONE',  ( -1.000000000000000000, 0.000000000000000000, -0.000000000000000000 ) ) ;
#60543 = CARTESIAN_POINT ( 'NONE',  ( -94.99999999999997158, -213.0599564267049857, 89.52375000000000682 ) ) ;
#60544 = EDGE_CURVE ( 'NONE', #19238, #26842, #53577, .T. ) ;
#60545 = CARTESIAN_POINT ( 'NONE',  ( -92.35000000000003695, 90.00000000000004263, 90.00000000000000000 ) ) ;
#60546 = ADVANCED_FACE ( 'NONE', ( #15929 ), #15562, .F. ) ;
#60547 = AXIS2_PLACEMENT_3D ( 'NONE', #6694, #35620, #70194 ) ;
#60548 = VERTEX_POINT ( 'NONE', #58006 ) ;
#60549 = DIRECTION ( 'NONE',  ( -1.000000000000000000, 0.000000000000000000, 0.000000000000000000 ) ) ;
#60550 = DIRECTION ( 'NONE',  ( -1.000000000000000000, -0.000000000000000000, 0.000000000000000000 ) ) ;
#60551 = DIRECTION ( 'NONE',  ( 0.000000000000000000, 0.000000000000000000, 1.000000000000000000 ) ) ;
#60552 = LINE ( 'NONE', #65455, #14938 ) ;
#60553 = EDGE_CURVE ( 'NONE', #45, #37858, #6726, .T. ) ;
#60554 = EDGE_CURVE ( 'NONE', #71157, #32752, #5778, .T. ) ;
#60555 = AXIS2_PLACEMENT_3D ( 'NONE', #67313, #32347, #43657 ) ;
#60556 = VERTEX_POINT ( 'NONE', #64029 ) ;
#60557 = VERTEX_POINT ( 'NONE', #23791 ) ;
#60558 = DIRECTION ( 'NONE',  ( -1.000000000000000000, -0.000000000000000000, 0.000000000000000000 ) ) ;
#60559 = DIRECTION ( 'NONE',  ( -1.000000000000000000, 0.000000000000000000, 0.000000000000000000 ) ) ;
#60560 = ORIENTED_EDGE ( 'NONE', *, *, #49247, .F. ) ;
#60561 = CIRCLE ( 'NONE', #17296, 0.5000000000000004441 ) ;
#60562 = CARTESIAN_POINT ( 'NONE',  ( 97.30629616937498838, -209.9999999999999716, 81.07031250086714635 ) ) ;
#60563 = CARTESIAN_POINT ( 'NONE',  ( 96.15314808468748708, -208.0026889286704943, 84.50989583420049200 ) ) ;
#60564 = CIRCLE ( 'NONE', #53360, 16.00000000000000000 ) ;
#60565 = VERTEX_POINT ( 'NONE', #17774 ) ;
#60566 = CARTESIAN_POINT ( 'NONE',  ( 96.15314808468748708, -208.0026889286704943, 85.14489583420048291 ) ) ;
#60567 = ORIENTED_EDGE ( 'NONE', *, *, #12659, .T. ) ;
#60568 = AXIS2_PLACEMENT_3D ( 'NONE', #64792, #24560, #36947 ) ;
#60569 = DIRECTION ( 'NONE',  ( 0.000000000000000000, 0.9510565162951544194, -0.3090169943749447867 ) ) ;
#60570 = ORIENTED_EDGE ( 'NONE', *, *, #46582, .T. ) ;
#60571 = CARTESIAN_POINT ( 'NONE',  ( -95.00000000000002842, 87.33691857156074434, 76.62531250086715318 ) ) ;
#60572 = ORIENTED_EDGE ( 'NONE', *, *, #57235, .F. ) ;
#60573 = VERTEX_POINT ( 'NONE', #176 ) ;
#60574 = FACE_OUTER_BOUND ( 'NONE', #59286, .T. ) ;
#60575 = AXIS2_PLACEMENT_3D ( 'NONE', #68488, #16976, #28609 ) ;
#60576 = VERTEX_POINT ( 'NONE', #51985 ) ;
#60577 = DIRECTION ( 'NONE',  ( 0.000000000000000000, 0.000000000000000000, 1.000000000000000000 ) ) ;
#60578 = ORIENTED_EDGE ( 'NONE', *, *, #72990, .F. ) ;
#60579 = CARTESIAN_POINT ( 'NONE',  ( 11.99999999999999822, 29.01471420065563933, 76.69515212746024702 ) ) ;
#60580 = VECTOR ( 'NONE', #47332, 1000.000000000000000 ) ;
#60581 = ORIENTED_EDGE ( 'NONE', *, *, #21923, .T. ) ;
#60582 = DIRECTION ( 'NONE',  ( -8.332732854036912157E-16, -1.065814103640131031E-14, -1.000000000000000000 ) ) ;
#60583 = ORIENTED_EDGE ( 'NONE', *, *, #57673, .T. ) ;
#60584 = EDGE_CURVE ( 'NONE', #25904, #14031, #28683, .T. ) ;
#60585 = AXIS2_PLACEMENT_3D ( 'NONE', #2739, #36528, #71101 ) ;
#60586 = ORIENTED_EDGE ( 'NONE', *, *, #51096, .T. ) ;
#60587 = VERTEX_POINT ( 'NONE', #12866 ) ;
#60588 = CARTESIAN_POINT ( 'NONE',  ( 96.15314808468748708, -208.0026889286704943, 78.63614583420047666 ) ) ;
#60589 = FACE_OUTER_BOUND ( 'NONE', #55432, .T. ) ;
#60590 = ITEM_DEFINED_TRANSFORMATION ( 'NONE', 'NONE', #48412,  #43395 ) ;
#60591 = DIRECTION ( 'NONE',  ( 1.000000000000000000, 0.000000000000000000, -0.000000000000000000 ) ) ;
#60592 = ORIENTED_EDGE ( 'NONE', *, *, #21996, .T. ) ;
#60593 = ORIENTED_EDGE ( 'NONE', *, *, #718, .T. ) ;
#60595 = EDGE_CURVE ( 'NONE', #26934, #9345, #43980, .T. ) ;
#60594 = ORIENTED_EDGE ( 'NONE', *, *, #71898, .T. ) ;
#60596 = CARTESIAN_POINT ( 'NONE',  ( -96.32499999999996021, -212.2949673200287179, 84.39083333333333314 ) ) ;
#60597 = DIRECTION ( 'NONE',  ( 0.6862798483830533369, 0.7273375899149812085, 0.000000000000000000 ) ) ;
#60598 = ADVANCED_FACE ( 'NONE', ( #62938 ), #29058, .F. ) ;
#60599 = CARTESIAN_POINT ( 'NONE',  ( -96.15314808468751551, 88.00268892867056536, 78.47739583420049314 ) ) ;
#60600 = VERTEX_POINT ( 'NONE', #35796 ) ;
#60601 = CARTESIAN_POINT ( 'NONE',  ( 93.84685191531248449, 91.99731107132950569, 76.20197916753380696 ) ) ;
#60602 = VERTEX_POINT ( 'NONE', #57651 ) ;
#60603 = CARTESIAN_POINT ( 'NONE',  ( 10.00000000000000000, 0.000000000000000000, 0.000000000000000000 ) ) ;
#60604 = DIRECTION ( 'NONE',  ( -0.000000000000000000, 0.8090169943749426773, -0.5877852522924796874 ) ) ;
#60605 = DIRECTION ( 'NONE',  ( -1.000000000000000000, 0.000000000000000000, 0.000000000000000000 ) ) ;
#60606 = DIRECTION ( 'NONE',  ( -1.000000000000000000, -0.000000000000000000, 0.000000000000000000 ) ) ;
#60607 = DIRECTION ( 'NONE',  ( 1.000000000000000000, 0.000000000000000000, 0.000000000000000000 ) ) ;
#60608 = CARTESIAN_POINT ( 'NONE',  ( -92.69370383062498320, -208.6684592857803295, 82.39322916753381776 ) ) ;
#60609 = EDGE_CURVE ( 'NONE', #68659, #67909, #33115, .T. ) ;
#60610 = CARTESIAN_POINT ( 'NONE',  ( -92.34999999999999432, -209.9999999999999716, 89.68250000000000455 ) ) ;
#60611 = CARTESIAN_POINT ( 'NONE',  ( -92.69370383062502583, 90.00000000000007105, 74.79348190356851944 ) ) ;
#60612 = DIRECTION ( 'NONE',  ( -0.3853207896976533764, 0.9227826878668546895, 0.000000000000000000 ) ) ;
#60613 = ORIENTED_EDGE ( 'NONE', *, *, #49247, .T. ) ;
#60614 = AXIS2_PLACEMENT_3D ( 'NONE', #61966, #16465, #49921 ) ;
#60615 = ORIENTED_EDGE ( 'NONE', *, *, #38130, .T. ) ;
#60616 = CARTESIAN_POINT ( 'NONE',  ( 10.00000000000000000, 40.68715046381944234, -10.41901085202036192 ) ) ;
#60617 = CARTESIAN_POINT ( 'NONE',  ( 11.99999999999999822, -77.49459641780886443, -0.8261519478439277586 ) ) ;
#60618 = CARTESIAN_POINT ( 'NONE',  ( 0.000000000000000000, -39.78640506895559525, -66.50666863322042843 ) ) ;
#60619 = CARTESIAN_POINT ( 'NONE',  ( -93.84685191531252713, 88.00268892867056536, 86.04447916753380809 ) ) ;
#60620 = CARTESIAN_POINT ( 'NONE',  ( -92.34999999999999432, -209.9999999999999716, 90.00000000000000000 ) ) ;
#60621 = LINE ( 'NONE', #70768, #49382 ) ;
#60622 = AXIS2_PLACEMENT_3D ( 'NONE', #51851, #396, #18008 ) ;
#60623 = EDGE_CURVE ( 'NONE', #16652, #70598, #58751, .T. ) ;
#60624 = ORIENTED_EDGE ( 'NONE', *, *, #24284, .T. ) ;
#60625 = AXIS2_PLACEMENT_3D ( 'NONE', #57992, #29766, #161 ) ;
#60626 = LINE ( 'NONE', #67358, #41643 ) ;
#60628 = DIRECTION ( 'NONE',  ( 1.000000000000000000, -0.000000000000000000, -0.000000000000000000 ) ) ;
#60627 = CIRCLE ( 'NONE', #54654, 82.00000000000000000 ) ;
#60629 = DIRECTION ( 'NONE',  ( 1.000000000000000000, -3.061616997868382648E-16, -0.000000000000000000 ) ) ;
#60630 = CARTESIAN_POINT ( 'NONE',  ( 10.00000000000000000, 0.000000000000000000, 0.000000000000000000 ) ) ;
#60631 = CARTESIAN_POINT ( 'NONE',  ( 10.00000000000000000, 0.000000000000000000, 0.000000000000000000 ) ) ;
#60632 = CARTESIAN_POINT ( 'NONE',  ( 92.35000000000000853, -211.5299782133524218, 82.43291666666665662 ) ) ;
#60633 = CARTESIAN_POINT ( 'NONE',  ( -97.30629616937497417, -211.3315407142195852, 84.13947916753383538 ) ) ;
#60634 = FILL_AREA_STYLE ('',( #48603 ) ) ;
#60635 = EDGE_CURVE ( 'NONE', #54914, #27087, #30162, .T. ) ;
#60636 = CARTESIAN_POINT ( 'NONE',  ( -96.32499999999996021, -212.2949673200287179, 87.01020833506763097 ) ) ;
#60637 = ADVANCED_FACE ( 'NONE', ( #533 ), #47105, .T. ) ;
#60638 = EDGE_CURVE ( 'NONE', #8157, #40486, #6152, .T. ) ;
#60639 = CARTESIAN_POINT ( 'NONE',  ( -10.00000000000000000, 0.000000000000000000, 0.000000000000000000 ) ) ;
#60640 = CARTESIAN_POINT ( 'NONE',  ( 0.000000000000000000, -40.98264845739755202, 9.188173127307159405 ) ) ;
#60641 = CARTESIAN_POINT ( 'NONE',  ( 15.00000000000000000, -19.89357724625003598, -12.59942793731059041 ) ) ;
#60642 = EDGE_LOOP ( 'NONE', ( #4634, #22887, #22008, #18665 ) ) ;
#60643 = DIRECTION ( 'NONE',  ( 0.000000000000000000, -0.8090169943749401238, -0.5877852522924831291 ) ) ;
#60644 = DIRECTION ( 'NONE',  ( 0.000000000000000000, 0.000000000000000000, -1.000000000000000000 ) ) ;
#60645 = DIRECTION ( 'NONE',  ( 0.000000000000000000, 0.000000000000000000, -1.000000000000000000 ) ) ;
#60646 = VECTOR ( 'NONE', #67082, 999.9999999999998863 ) ;
#60647 = CARTESIAN_POINT ( 'NONE',  ( -10.00000000000000000, 0.000000000000000000, 0.000000000000000000 ) ) ;
#60648 = ORIENTED_EDGE ( 'NONE', *, *, #43578, .T. ) ;
#60649 = CARTESIAN_POINT ( 'NONE',  ( 92.34999999999990905, 91.52997821335249284, 78.51708333333334622 ) ) ;
#60650 = CARTESIAN_POINT ( 'NONE',  ( -10.90076147243505211, 0.000000000000000000, 0.000000000000000000 ) ) ;
#60651 = ORIENTED_EDGE ( 'NONE', *, *, #60046, .T. ) ;
#60652 =( BOUNDED_CURVE ( )  B_SPLINE_CURVE ( 2, ( #46869, #30941, #65923, #18285, #42250, #37353, #57777, #42613, #13656, #8767, #31685 ),
 .UNSPECIFIED., .F., .F. ) 
 B_SPLINE_CURVE_WITH_KNOTS ( ( 3, 2, 2, 2, 2, 3 ),
 ( 0.1481709449575277227, 0.1481710763585297463, 0.1552268418994118271, 0.1622826074402939078, 0.1693383729811760163, 0.1693384224419981210 ),
 .UNSPECIFIED. ) 
 CURVE ( )  GEOMETRIC_REPRESENTATION_ITEM ( )  RATIONAL_B_SPLINE_CURVE ( ( 0.9999950100189032298, 0.9999975049629860058, 1.000000000000000000, 0.8660254037844387076, 1.000000000000000000, 0.8660254037844387076, 1.000000000000000000, 0.8660254037844387076, 1.000000000000000000, 0.9999990608398716674, 0.9999981216929102468 ) ) 
 REPRESENTATION_ITEM ( '' )  );
#60653 = DIRECTION ( 'NONE',  ( 0.000000000000000000, -0.6494480483301904306, 0.7604059656000251577 ) ) ;
#60654 = DIRECTION ( 'NONE',  ( 1.000000000000000000, 0.000000000000000000, 0.000000000000000000 ) ) ;
#60655 = ORIENTED_EDGE ( 'NONE', *, *, #71785, .F. ) ;
#60656 = ORIENTED_EDGE ( 'NONE', *, *, #63822, .T. ) ;
#60657 = CARTESIAN_POINT ( 'NONE',  ( -2.500000000000000000, 16.00000000000000000, -19.01812422950394676 ) ) ;
#60658 = AXIS2_PLACEMENT_3D ( 'NONE', #73505, #10359, #50957 ) ;
#60659 = EDGE_LOOP ( 'NONE', ( #49104, #64821, #67773, #52642, #1108, #68541 ) ) ;
#60660 = ORIENTED_EDGE ( 'NONE', *, *, #26535, .T. ) ;
#60661 = ORIENTED_EDGE ( 'NONE', *, *, #56089, .T. ) ;
#60662 = ORIENTED_EDGE ( 'NONE', *, *, #62602, .F. ) ;
#60663 = DIRECTION ( 'NONE',  ( -1.000000000000000000, 5.236901059551556403E-15, 2.618450529775778123E-14 ) ) ;
#60664 = ORIENTED_EDGE ( 'NONE', *, *, #57358, .T. ) ;
#60665 = ORIENTED_EDGE ( 'NONE', *, *, #51590, .T. ) ;
#60666 = CARTESIAN_POINT ( 'NONE',  ( 94.99999999999998579, 92.66308142843935514, 78.21281250086717307 ) ) ;
#60667 = AXIS2_PLACEMENT_3D ( 'NONE', #9875, #61011, #15889 ) ;
#60668 = DIRECTION ( 'NONE',  ( -1.000000000000000000, -0.000000000000000000, 0.000000000000000000 ) ) ;
#60669 = CARTESIAN_POINT ( 'NONE',  ( -97.65000000000001990, 90.00000000000004263, 88.17437500173430465 ) ) ;
#60670 = ORIENTED_EDGE ( 'NONE', *, *, #20696, .F. ) ;
#60671 = ORIENTED_EDGE ( 'NONE', *, *, #16193, .F. ) ;
#60672 = ORIENTED_EDGE ( 'NONE', *, *, #35393, .F. ) ;
#60673 = CARTESIAN_POINT ( 'NONE',  ( 97.30629616937498838, 88.66845928578037217, 89.27239583420048064 ) ) ;
#60674 = ORIENTED_EDGE ( 'NONE', *, *, #65355, .F. ) ;
#60675 = CIRCLE ( 'NONE', #33061, 31.99999999999998224 ) ;
#60676 = CARTESIAN_POINT ( 'NONE',  ( 96.15314808468750130, -211.9973110713294489, 89.21947916753380525 ) ) ;
#60677 = DIRECTION ( 'NONE',  ( -5.551115123125782702E-17, 0.000000000000000000, -1.000000000000000000 ) ) ;
#60678 = CARTESIAN_POINT ( 'NONE',  ( -3.000000000000000000, 8.688484142253939169, 21.88630264137371029 ) ) ;
#60679 = CARTESIAN_POINT ( 'NONE',  ( -95.31113939543074309, 92.37342585364828551, 74.84415580543368662 ) ) ;
#60680 = CARTESIAN_POINT ( 'NONE',  ( 5.000000000000000000, 27.75498641678742473, 31.52238457039609187 ) ) ;
#60681 = CARTESIAN_POINT ( 'NONE',  ( 0.000000000000000000, 0.000000000000000000, 0.000000000000000000 ) ) ;
#60682 = EDGE_CURVE ( 'NONE', #14108, #66145, #12722, .T. ) ;
#60683 = AXIS2_PLACEMENT_3D ( 'NONE', #12335, #24002, #41288 ) ;
#60684 = CARTESIAN_POINT ( 'NONE',  ( -94.99999999999997158, -206.9400435732949575, 82.85625000000000284 ) ) ;
#60685 = CARTESIAN_POINT ( 'NONE',  ( 0.000000000000000000, -60.67117009219175827, 55.16347631943019536 ) ) ;
#60686 = CARTESIAN_POINT ( 'NONE',  ( -97.64999999999996305, -209.9999999999999716, 76.10937500173430692 ) ) ;
#60687 = EDGE_CURVE ( 'NONE', #59117, #46890, #47467, .T. ) ;
#60688 = CARTESIAN_POINT ( 'NONE',  ( -92.69370383062502583, 91.33154071421968467, 87.63197916753382799 ) ) ;
#60689 = ORIENTED_EDGE ( 'NONE', *, *, #41662, .F. ) ;
#60691 = CARTESIAN_POINT ( 'NONE',  ( -92.69370383062502583, 88.66845928578038638, 88.63739583420047552 ) ) ;
#60690 = CARTESIAN_POINT ( 'NONE',  ( 93.84685191531248449, 91.99731107132950569, 88.90197916753380980 ) ) ;
#60692 = ORIENTED_EDGE ( 'NONE', *, *, #11388, .F. ) ;
#60693 = CARTESIAN_POINT ( 'NONE',  ( 97.30629616937498838, 90.00000000000002842, 76.78406250086715090 ) ) ;
#60694 = CARTESIAN_POINT ( 'NONE',  ( -92.35000000000003695, 90.00000000000004263, 83.33250000000001023 ) ) ;
#60695 = CARTESIAN_POINT ( 'NONE',  ( -3.000000000000000000, 9.615535125378775305, 24.73947219025917121 ) ) ;
#60696 = DIRECTION ( 'NONE',  ( 0.000000000000000000, -0.5224985647159559043, 0.8526401643540879594 ) ) ;
#60697 = CIRCLE ( 'NONE', #24665, 12.50000000000000000 ) ;
#60698 = CYLINDRICAL_SURFACE ( 'NONE', #72244, 82.00000000000000000 ) ;
#60699 = CARTESIAN_POINT ( 'NONE',  ( 5.000000000000000000, -74.74816331893454446, 33.71516098798714722 ) ) ;
#60700 = EDGE_CURVE ( 'NONE', #50672, #769, #24531, .T. ) ;
#60701 = EDGE_CURVE ( 'NONE', #45793, #41715, #52358, .T. ) ;
#60702 = DIRECTION ( 'NONE',  ( 0.000000000000000000, 0.000000000000000000, 1.000000000000000000 ) ) ;
#60703 = CARTESIAN_POINT ( 'NONE',  ( 4.999999999999999112, -21.40280677340345505, -36.13751322684441192 ) ) ;
#60704 = ORIENTED_EDGE ( 'NONE', *, *, #50731, .F. ) ;
#60705 = CIRCLE ( 'NONE', #7826, 32.50000000000000000 ) ;
#60706 = ORIENTED_EDGE ( 'NONE', *, *, #48798, .T. ) ;
#60707 = CARTESIAN_POINT ( 'NONE',  ( -93.67500000000003979, 92.29496732002878900, 82.16833333333332234 ) ) ;
#60708 = CARTESIAN_POINT ( 'NONE',  ( 1.560000000000000053, -0.8660254037844384856, 1.500000000000000000 ) ) ;
#60709 = DIRECTION ( 'NONE',  ( 0.000000000000000000, 0.000000000000000000, 1.000000000000000000 ) ) ;
#60710 = CARTESIAN_POINT ( 'NONE',  ( 11.99999999999999822, -73.95703589263958122, -23.16143007188505010 ) ) ;
#60711 = CARTESIAN_POINT ( 'NONE',  ( 5.000000000000000000, 22.48208911017500355, 35.47612816024530957 ) ) ;
#60712 = DIRECTION ( 'NONE',  ( -1.000000000000000000, 0.000000000000000000, 0.000000000000000000 ) ) ;
#60713 = FACE_OUTER_BOUND ( 'NONE', #57519, .T. ) ;
#60714 = ADVANCED_FACE ( 'NONE', ( #17413 ), #34697, .F. ) ;
#60715 = ORIENTED_EDGE ( 'NONE', *, *, #59753, .F. ) ;
#60716 = CARTESIAN_POINT ( 'NONE',  ( -96.15314808468751551, 88.00268892867056536, 80.85864583420047325 ) ) ;
#60717 = PLANE ( 'NONE',  #27111 ) ;
#60718 = FACE_OUTER_BOUND ( 'NONE', #32064, .T. ) ;
#60719 =( LENGTH_UNIT ( ) NAMED_UNIT ( * ) SI_UNIT ( .MILLI., .METRE. ) );
#60720 = CARTESIAN_POINT ( 'NONE',  ( 11.99999999999999822, 0.000000000000000000, 0.000000000000000000 ) ) ;
#60721 = CYLINDRICAL_SURFACE ( 'NONE', #55728, 2.649999999999985700 ) ;
#60722 = DIRECTION ( 'NONE',  ( 0.000000000000000000, 0.8526401643540897357, 0.5224985647159531288 ) ) ;
#60723 = CARTESIAN_POINT ( 'NONE',  ( -3.702536634196121224, 8.043911037661892749, -64.01812422950395387 ) ) ;
#60724 = CARTESIAN_POINT ( 'NONE',  ( 0.000000000000000000, -76.66974797899828786, -11.30684508768420393 ) ) ;
#60725 = DIRECTION ( 'NONE',  ( 0.000000000000000000, 0.9969173337331281859, -0.07845909572784182107 ) ) ;
#60726 = EDGE_CURVE ( 'NONE', #50776, #42720, #63664, .T. ) ;
#60727 = EDGE_CURVE ( 'NONE', #62260, #29988, #54757, .T. ) ;
#60728 = AXIS2_PLACEMENT_3D ( 'NONE', #23156, #7339, #41542 ) ;
#60729 = CARTESIAN_POINT ( 'NONE',  ( 97.30629616937498838, 91.33154071421968467, 81.28197916753381946 ) ) ;
#60730 = CARTESIAN_POINT ( 'NONE',  ( -97.30629616937495996, -209.9999999999999716, 84.72156250086715090 ) ) ;
#60731 = CARTESIAN_POINT ( 'NONE',  ( 10.00000000000000000, 0.000000000000000000, 0.000000000000000000 ) ) ;
#60732 = ORIENTED_EDGE ( 'NONE', *, *, #41254, .T. ) ;
#60733 = DIRECTION ( 'NONE',  ( 0.000000000000000000, 0.000000000000000000, 1.000000000000000000 ) ) ;
#60734 = CARTESIAN_POINT ( 'NONE',  ( -97.64999999999994884, -211.5299782133524502, 76.71791666666666742 ) ) ;
#60735 = DIRECTION ( 'NONE',  ( 0.000000000000000000, 0.5224985647159441360, 0.8526401643540952868 ) ) ;
#60736 = VECTOR ( 'NONE', #65953, 1000.000000000000114 ) ;
#60737 = CIRCLE ( 'NONE', #70306, 77.49899999999998101 ) ;
#60738 = CIRCLE ( 'NONE', #24661, 31.99999999999999289 ) ;
#60739 = CARTESIAN_POINT ( 'NONE',  ( 97.30629616937498838, -208.6684592857803011, 82.39322916753381776 ) ) ;
#60740 = ORIENTED_EDGE ( 'NONE', *, *, #22089, .F. ) ;
#60741 = AXIS2_PLACEMENT_3D ( 'NONE', #12145, #35452, #51637 ) ;
#60742 = ORIENTED_EDGE ( 'NONE', *, *, #58317, .F. ) ;
#60743 = VECTOR ( 'NONE', #53846, 1000.000000000000000 ) ;
#60744 = CARTESIAN_POINT ( 'NONE',  ( -93.67499999999998295, -207.7050326799711968, 75.89770833506763381 ) ) ;
#60745 = VERTEX_POINT ( 'NONE', #71853 ) ;
#60746 = CARTESIAN_POINT ( 'NONE',  ( -97.65000000000001990, 90.00000000000004263, 79.28437500173430408 ) ) ;
#60747 = AXIS2_PLACEMENT_3D ( 'NONE', #33159, #39189, #6104 ) ;
#60748 = CARTESIAN_POINT ( 'NONE',  ( 97.30629616937498838, -211.3315407142195852, 79.90614583420048689 ) ) ;
#60749 = DIRECTION ( 'NONE',  ( -0.5687579148473743684, 0.8225049752423791993, 0.000000000000000000 ) ) ;
#60750 = LINE ( 'NONE', #66395, #32787 ) ;
#60751 = EDGE_CURVE ( 'NONE', #36331, #70989, #7979, .T. ) ;
#60752 = CARTESIAN_POINT ( 'NONE',  ( -97.28022634951636860, 88.83725486022233042, 74.94226573542110259 ) ) ;
#60753 = CARTESIAN_POINT ( 'NONE',  ( 92.69370383062498320, 91.33154071421968467, 86.57364583420047666 ) ) ;
#60754 = CARTESIAN_POINT ( 'NONE',  ( 0.000000000000000000, 78.73519480814985627, -22.90783923731548199 ) ) ;
#60755 = CARTESIAN_POINT ( 'NONE',  ( 95.00000000000000000, -206.9400435732949575, 80.95125000000000171 ) ) ;
#60756 = EDGE_CURVE ( 'NONE', #63983, #25489, #64763, .T. ) ;
#60757 = VERTEX_POINT ( 'NONE', #37672 ) ;
#60758 = ORIENTED_EDGE ( 'NONE', *, *, #70659, .F. ) ;
#60759 = ORIENTED_EDGE ( 'NONE', *, *, #67293, .T. ) ;
#60760 = EDGE_LOOP ( 'NONE', ( #35975, #32461, #22886, #3813 ) ) ;
#60761 = CYLINDRICAL_SURFACE ( 'NONE', #1024, 26.50000000000000355 ) ;
#60762 = EDGE_CURVE ( 'NONE', #34299, #14636, #19621, .T. ) ;
#60763 = CARTESIAN_POINT ( 'NONE',  ( -96.15314808468752972, 91.99731107132950569, 85.25072916753381946 ) ) ;
#60764 = DIRECTION ( 'NONE',  ( -1.000000000000000000, -0.000000000000000000, 0.000000000000000000 ) ) ;
#60765 = FACE_OUTER_BOUND ( 'NONE', #23390, .T. ) ;
#60766 = ADVANCED_FACE ( 'NONE', ( #66246 ), #14722, .T. ) ;
#60767 = CARTESIAN_POINT ( 'NONE',  ( 92.34999999999999432, 88.47002178664753558, 76.08291666666666231 ) ) ;
#60768 = DIRECTION ( 'NONE',  ( 1.000000000000000000, 0.000000000000000000, 0.000000000000000000 ) ) ;
#60769 = VERTEX_POINT ( 'NONE', #13249 ) ;
#60770 = CARTESIAN_POINT ( 'NONE',  ( -97.64999999999996305, -209.9999999999999716, 86.90437500173429441 ) ) ;
#60771 = ORIENTED_EDGE ( 'NONE', *, *, #40556, .T. ) ;
#60772 = LINE ( 'NONE', #54383, #31416 ) ;
#60773 = ORIENTED_EDGE ( 'NONE', *, *, #35205, .T. ) ;
#60774 = CARTESIAN_POINT ( 'NONE',  ( -92.35000000000005116, 91.52997821335253548, 82.19479166840095274 ) ) ;
#60775 = VERTEX_POINT ( 'NONE', #70373 ) ;
#60776 = CARTESIAN_POINT ( 'NONE',  ( 96.15314808468748708, 88.00268892867053694, 85.56822916753381492 ) ) ;
#60777 = AXIS2_PLACEMENT_3D ( 'NONE', #6870, #11751, #18149 ) ;
#60778 = DIRECTION ( 'NONE',  ( -1.000000000000000000, -0.000000000000000000, 0.000000000000000000 ) ) ;
#60779 = LINE ( 'NONE', #26551, #30647 ) ;
#60780 = CARTESIAN_POINT ( 'NONE',  ( 0.000000000000000000, 0.000000000000000000, 0.000000000000000000 ) ) ;
#60781 = CARTESIAN_POINT ( 'NONE',  ( 94.99999999999998579, 86.94004357329502852, 88.88875000000000171 ) ) ;
#60782 = EDGE_CURVE ( 'NONE', #51687, #3457, #3110, .T. ) ;
#60783 = CARTESIAN_POINT ( 'NONE',  ( 50.00005079999999680, 0.000000000000000000, 21.00000000000000000 ) ) ;
#60784 = ORIENTED_EDGE ( 'NONE', *, *, #5359, .T. ) ;
#60785 = LINE ( 'NONE', #72770, #8719 ) ;
#60786 = FACE_OUTER_BOUND ( 'NONE', #73232, .T. ) ;
#60787 = EDGE_LOOP ( 'NONE', ( #32975, #21143, #5268, #2145 ) ) ;
#60788 = ORIENTED_EDGE ( 'NONE', *, *, #5397, .T. ) ;
#60790 = DIRECTION ( 'NONE',  ( 0.000000000000000000, -6.938893903907228378E-15, 1.000000000000000000 ) ) ;
#60789 = VECTOR ( 'NONE', #62962, 1000.000000000000114 ) ;
#60791 = CARTESIAN_POINT ( 'NONE',  ( -3.000000000000000000, 16.83928648764923253, 16.46020748918050458 ) ) ;
#60792 = VECTOR ( 'NONE', #20748, 1000.000000000000000 ) ;
#60793 = EDGE_CURVE ( 'NONE', #66201, #23719, #2387, .T. ) ;
#60794 = FACE_OUTER_BOUND ( 'NONE', #59361, .T. ) ;
#60795 = CARTESIAN_POINT ( 'NONE',  ( -94.99999999999997158, -207.3369185715606307, 83.29281250086717137 ) ) ;
#60796 = ORIENTED_EDGE ( 'NONE', *, *, #30377, .T. ) ;
#60797 = DIRECTION ( 'NONE',  ( -1.000000000000000000, 0.000000000000000000, 0.000000000000000000 ) ) ;
#60798 = EDGE_CURVE ( 'NONE', #47938, #65417, #28343, .T. ) ;
#60799 = ORIENTED_EDGE ( 'NONE', *, *, #70095, .F. ) ;
#60800 = DIRECTION ( 'NONE',  ( -1.000000000000000000, -0.000000000000000000, 0.000000000000000000 ) ) ;
#60801 = ADVANCED_FACE ( 'NONE', ( #19987, #48929 ), #25280, .T. ) ;
#60802 = LINE ( 'NONE', #43885, #15482 ) ;
#60803 = AXIS2_PLACEMENT_3D ( 'NONE', #25230, #6465, #60195 ) ;
#60804 = CARTESIAN_POINT ( 'NONE',  ( 93.84685191531248449, 88.00268892867053694, 77.04864583420047097 ) ) ;
#60805 = DIRECTION ( 'NONE',  ( 0.000000000000000000, 0.000000000000000000, -1.000000000000000000 ) ) ;
#60806 = LINE ( 'NONE', #4413, #56487 ) ;
#60807 = DIRECTION ( 'NONE',  ( 0.8541291221503261033, -0.5200609990133016058, 0.000000000000000000 ) ) ;
#60808 = CARTESIAN_POINT ( 'NONE',  ( -2.500000000000003997, -4.330127018922192761, -6.000000000000000000 ) ) ;
#60809 = CARTESIAN_POINT ( 'NONE',  ( 10.00000000000000000, -37.01155633439053361, -6.555932627142825986 ) ) ;
#60810 = DIRECTION ( 'NONE',  ( 1.000000000000000000, 0.000000000000000000, 0.000000000000000000 ) ) ;
#60811 = ADVANCED_FACE ( 'NONE', ( #8724 ), #59866, .T. ) ;
#60812 = DIRECTION ( 'NONE',  ( 0.000000000000000000, -0.7071067811865389130, -0.7071067811865563435 ) ) ;
#60813 = EDGE_CURVE ( 'NONE', #61214, #20114, #17517, .T. ) ;
#60814 = CARTESIAN_POINT ( 'NONE',  ( -97.64998927314377397, 88.47001559349419608, 78.06729209680058545 ) ) ;
#60815 = ORIENTED_EDGE ( 'NONE', *, *, #69033, .F. ) ;
#60816 = CARTESIAN_POINT ( 'NONE',  ( -97.30629616937501680, 91.33154071421968467, 82.60489583420049087 ) ) ;
#60817 = CARTESIAN_POINT ( 'NONE',  ( 0.000000000000000000, -16.65972982744991171, 80.28980883073752750 ) ) ;
#60818 = VECTOR ( 'NONE', #73233, 1000.000000000000000 ) ;
#60819 = CARTESIAN_POINT ( 'NONE',  ( 0.000000000000000000, -63.97538442413390669, -51.29473840253292849 ) ) ;
#60820 = ORIENTED_EDGE ( 'NONE', *, *, #634, .T. ) ;
#60821 = CARTESIAN_POINT ( 'NONE',  ( 11.99999999999999822, 0.000000000000000000, 0.000000000000000000 ) ) ;
#60822 = LINE ( 'NONE', #66828, #16800 ) ;
#60823 = CIRCLE ( 'NONE', #8010, 37.49900000000000233 ) ;
#60824 = CARTESIAN_POINT ( 'NONE',  ( -92.34999999999999432, -209.9999999999999716, 89.68250000000000455 ) ) ;
#60825 = CARTESIAN_POINT ( 'NONE',  ( 10.00000000000000000, 0.000000000000000000, 0.000000000000000000 ) ) ;
#60826 = CARTESIAN_POINT ( 'NONE',  ( 95.00000000000000000, -212.6630814284392557, 77.89531250086714920 ) ) ;
#60827 = AXIS2_PLACEMENT_3D ( 'NONE', #9219, #61105, #37812 ) ;
#60828 = VERTEX_POINT ( 'NONE', #48204 ) ;
#60829 = AXIS2_PLACEMENT_3D ( 'NONE', #29129, #17489, #23145 ) ;
#60830 = ORIENTED_EDGE ( 'NONE', *, *, #12478, .T. ) ;
#60831 = DIRECTION ( 'NONE',  ( 0.000000000000000000, 0.000000000000000000, -1.000000000000000000 ) ) ;
#60832 = CIRCLE ( 'NONE', #64490, 42.00000000000000000 ) ;
#60833 = CARTESIAN_POINT ( 'NONE',  ( -92.34999999999999432, -209.9999999999999716, 81.42749999999999488 ) ) ;
#60834 = CYLINDRICAL_SURFACE ( 'NONE', #66408, 77.49899999999999523 ) ;
#60835 = DIRECTION ( 'NONE',  ( 0.000000000000000000, 0.5877852522924797984, -0.8090169943749426773 ) ) ;
#60836 = CARTESIAN_POINT ( 'NONE',  ( 97.30629616937498838, -211.3315407142195852, 76.73114583420048973 ) ) ;
#60837 = ORIENTED_EDGE ( 'NONE', *, *, #26712, .F. ) ;
#60838 = EDGE_CURVE ( 'NONE', #70907, #69466, #42942, .T. ) ;
#60839 = DIRECTION ( 'NONE',  ( -1.000000000000000000, 0.000000000000000000, 0.000000000000000000 ) ) ;
#60840 = ORIENTED_EDGE ( 'NONE', *, *, #13977, .T. ) ;
#60841 = ORIENTED_EDGE ( 'NONE', *, *, #56857, .F. ) ;
#60842 = DIRECTION ( 'NONE',  ( -1.000000000000000000, 0.000000000000000000, -0.000000000000000000 ) ) ;
#60843 = ADVANCED_FACE ( 'NONE', ( #8353 ), #30526, .T. ) ;
#60844 = AXIS2_PLACEMENT_3D ( 'NONE', #51117, #74041, #67672 ) ;
#60845 = LINE ( 'NONE', #3721, #53314 ) ;
#60846 = VERTEX_POINT ( 'NONE', #31640 ) ;
#60847 = DIRECTION ( 'NONE',  ( -1.000000000000000000, 0.000000000000000000, -0.000000000000000000 ) ) ;
#60848 = CARTESIAN_POINT ( 'NONE',  ( 93.67500000000001137, -212.2949673200287179, 78.75520833506763552 ) ) ;
#60849 = ADVANCED_FACE ( 'NONE', ( #2012 ), #60244, .F. ) ;
#60850 = CARTESIAN_POINT ( 'NONE',  ( 92.34999999999999432, 91.52997821335252127, 85.50208333333331723 ) ) ;
#60851 = EDGE_CURVE ( 'NONE', #71294, #29955, #36768, .T. ) ;
#60852 = AXIS2_PLACEMENT_3D ( 'NONE', #46317, #68884, #62130 ) ;
#60853 = ORIENTED_EDGE ( 'NONE', *, *, #42274, .T. ) ;
#60854 = DIRECTION ( 'NONE',  ( -1.000000000000000000, 0.000000000000000000, 0.000000000000000000 ) ) ;
#60855 = CARTESIAN_POINT ( 'NONE',  ( -93.33864827736697123, -211.6008015735577033, 74.79754476654878204 ) ) ;
#60856 = VERTEX_POINT ( 'NONE', #13614 ) ;
#60857 = DIRECTION ( 'NONE',  ( -1.000000000000000000, -0.000000000000000000, 0.000000000000000000 ) ) ;
#60858 = CARTESIAN_POINT ( 'NONE',  ( -92.69370383062504004, 90.00000000000004263, 85.03906250086714635 ) ) ;
#60859 = CARTESIAN_POINT ( 'NONE',  ( 92.69370383062498320, 91.33154071421968467, 81.96989583420048575 ) ) ;
#60860 = ORIENTED_EDGE ( 'NONE', *, *, #55346, .F. ) ;
#60861 = DIRECTION ( 'NONE',  ( -1.000000000000000000, 0.000000000000000000, 0.000000000000000000 ) ) ;
#60862 = EDGE_LOOP ( 'NONE', ( #46960, #46322, #61802, #65654 ) ) ;
#60863 = CARTESIAN_POINT ( 'NONE',  ( -97.64999999999996305, -209.9999999999999716, 86.18999999999999773 ) ) ;
#60864 = EDGE_LOOP ( 'NONE', ( #59727, #5387, #30801, #23654 ) ) ;
#60865 = TOROIDAL_SURFACE ( 'NONE', #13997, 12.80000000000000071, 0.2999999999999999334 ) ;
#60866 = ORIENTED_EDGE ( 'NONE', *, *, #12496, .F. ) ;
#60867 = EDGE_CURVE ( 'NONE', #25146, #56950, #30804, .T. ) ;
#60868 = ORIENTED_EDGE ( 'NONE', *, *, #44237, .F. ) ;
#60869 = CYLINDRICAL_SURFACE ( 'NONE', #30082, 82.00000000000000000 ) ;
#60870 = ADVANCED_FACE ( 'NONE', ( #43687 ), #61709, .T. ) ;
#60871 = ORIENTED_EDGE ( 'NONE', *, *, #19373, .T. ) ;
#60872 = DIRECTION ( 'NONE',  ( 1.000000000000000000, 0.000000000000000000, 0.000000000000000000 ) ) ;
#60873 = CARTESIAN_POINT ( 'NONE',  ( 0.000000000000000000, -71.21200624218768382, -40.65526001592688488 ) ) ;
#60874 = ORIENTED_EDGE ( 'NONE', *, *, #69362, .T. ) ;
#60875 =( BOUNDED_CURVE ( )  B_SPLINE_CURVE ( 2, ( #3123, #30907, #7621, #49314, #71870, #19998, #54597 ),
 .UNSPECIFIED., .F., .F. ) 
 B_SPLINE_CURVE_WITH_KNOTS ( ( 3, 2, 2, 3 ),
 ( 0.3175094496506953856, 0.3245652148805889259, 0.3316209804214713119, 0.3386766260338262002 ),
 .UNSPECIFIED. ) 
 CURVE ( )  GEOMETRIC_REPRESENTATION_ITEM ( )  RATIONAL_B_SPLINE_CURVE ( ( 1.000000000000000000, 0.8660254037844387076, 1.000000000000000000, 0.8660254037844387076, 1.000000000000000000, 0.8660276809825613320, 0.9999954456811669390 ) ) 
 REPRESENTATION_ITEM ( '' )  );
#60876 = CARTESIAN_POINT ( 'NONE',  ( -93.84685191531247028, -211.9973110713294489, 79.05947916753380866 ) ) ;
#60877 = ORIENTED_EDGE ( 'NONE', *, *, #6438, .T. ) ;
#60878 = CARTESIAN_POINT ( 'NONE',  ( -97.65000000000001990, 90.00000000000004263, 90.00000000000000000 ) ) ;
#60879 = AXIS2_PLACEMENT_3D ( 'NONE', #29242, #62383, #34904 ) ;
#60880 = DIRECTION ( 'NONE',  ( -1.000000000000000000, 0.000000000000000000, 0.000000000000000000 ) ) ;
#60881 = DIRECTION ( 'NONE',  ( -0.5000000000000051070, 0.000000000000000000, 0.8660254037844355990 ) ) ;
#60882 = DIRECTION ( 'NONE',  ( 1.000000000000000000, 0.000000000000000000, 0.000000000000000000 ) ) ;
#60883 = AXIS2_PLACEMENT_3D ( 'NONE', #74146, #69627, #29386 ) ;
#60884 = CARTESIAN_POINT ( 'NONE',  ( 92.35000000000000853, -208.4700217866474645, 83.67645833506763609 ) ) ;
#60885 = EDGE_CURVE ( 'NONE', #63017, #57622, #11596, .T. ) ;
#60886 = EDGE_CURVE ( 'NONE', #38196, #63089, #16388, .T. ) ;
#60887 = CIRCLE ( 'NONE', #34467, 1.000000000000000000 ) ;
#60888 = CYLINDRICAL_SURFACE ( 'NONE', #32490, 16.00000000000000000 ) ;
#60889 = CARTESIAN_POINT ( 'NONE',  ( 92.69370383062498320, 91.33154071421968467, 87.04989583420046984 ) ) ;
#60890 = CARTESIAN_POINT ( 'NONE',  ( 11.99999999999999822, 72.35160999960817207, 20.41045688087850607 ) ) ;
#60891 = CYLINDRICAL_SURFACE ( 'NONE', #13374, 3.299999999999983391 ) ;
#60892 = CARTESIAN_POINT ( 'NONE',  ( -92.35000000000003695, 90.00000000000004263, 88.49187500173430010 ) ) ;
#60893 = CARTESIAN_POINT ( 'NONE',  ( 0.000000000000000000, -2.946379043146863719, 75.11764819372146462 ) ) ;
#60894 = CARTESIAN_POINT ( 'NONE',  ( 92.69370383062498320, 90.00000000000002842, 89.64281250086713726 ) ) ;
#60895 = CARTESIAN_POINT ( 'NONE',  ( 0.000000000000000000, 58.39081064771822582, -50.95692526931267707 ) ) ;
#60896 = CIRCLE ( 'NONE', #11661, 31.99999999999998224 ) ;
#60897 = LINE ( 'NONE', #19548, #29529 ) ;
#60898 = CARTESIAN_POINT ( 'NONE',  ( -95.00000000000002842, 90.00000000000004263, 90.00000000000000000 ) ) ;
#60899 = FACE_OUTER_BOUND ( 'NONE', #70429, .T. ) ;
#60900 = DIRECTION ( 'NONE',  ( -1.000000000000000000, 0.000000000000000000, -0.000000000000000000 ) ) ;
#60901 = CIRCLE ( 'NONE', #64500, 11.59999999999999787 ) ;
#60902 = DIRECTION ( 'NONE',  ( 0.000000000000000000, 0.000000000000000000, 1.000000000000000000 ) ) ;
#60903 = CARTESIAN_POINT ( 'NONE',  ( -94.99999999999997158, -206.9400435732949575, 87.30124999999999602 ) ) ;
#60904 = CIRCLE ( 'NONE', #10503, 37.49900000000000233 ) ;
#60905 = CARTESIAN_POINT ( 'NONE',  ( 10.00000000000000000, -17.67226234102801286, -33.17418723428327354 ) ) ;
#60906 = FACE_OUTER_BOUND ( 'NONE', #11302, .T. ) ;
#60907 = DIRECTION ( 'NONE',  ( 0.000000000000000000, 0.000000000000000000, 1.000000000000000000 ) ) ;
#60908 = CARTESIAN_POINT ( 'NONE',  ( 10.00000000000000000, 0.000000000000000000, 0.000000000000000000 ) ) ;
#60909 = DIRECTION ( 'NONE',  ( 0.000000000000000000, 0.000000000000000000, 1.000000000000000000 ) ) ;
#60910 = ORIENTED_EDGE ( 'NONE', *, *, #10206, .T. ) ;
#60911 = ORIENTED_EDGE ( 'NONE', *, *, #6028, .F. ) ;
#60912 = DIRECTION ( 'NONE',  ( 0.000000000000000000, -0.4539904997395541875, 0.8910065241883641241 ) ) ;
#60913 = CARTESIAN_POINT ( 'NONE',  ( 92.52185191531248165, 90.00000000000002842, 89.90078125043358170 ) ) ;
#60914 = EDGE_LOOP ( 'NONE', ( #11000, #28769, #41883, #29305 ) ) ;
#60915 =( REPRESENTATION_RELATIONSHIP ('NONE','NONE', #31117, #23018 ) REPRESENTATION_RELATIONSHIP_WITH_TRANSFORMATION ( #35346 )SHAPE_REPRESENTATION_RELATIONSHIP( ) );
#60916 = CARTESIAN_POINT ( 'NONE',  ( 97.30629616937498838, -209.9999999999999716, 80.43531250086714124 ) ) ;
#60917 = CARTESIAN_POINT ( 'NONE',  ( 93.84685191531249870, -208.0026889286704943, 85.88572916753381037 ) ) ;
#60918 = EDGE_LOOP ( 'NONE', ( #12094, #16252, #361, #2277 ) ) ;
#60919 = CARTESIAN_POINT ( 'NONE',  ( 95.00000000000000000, -207.3369185715606307, 85.83281250086714920 ) ) ;
#60920 = CIRCLE ( 'NONE', #41708, 77.49900000000000944 ) ;
#60921 = VERTEX_POINT ( 'NONE', #66607 ) ;
#60922 = EDGE_CURVE ( 'NONE', #20976, #65590, #40429, .T. ) ;
#60923 = CARTESIAN_POINT ( 'NONE',  ( 11.99999999999999822, 24.73286445877705475, 73.44644590900068692 ) ) ;
#60924 = ORIENTED_EDGE ( 'NONE', *, *, #28697, .T. ) ;
#60925 = CARTESIAN_POINT ( 'NONE',  ( -96.15314808468752972, 91.99731107132950569, 77.63072916753381492 ) ) ;
#60926 = VERTEX_POINT ( 'NONE', #10193 ) ;
#60927 = AXIS2_PLACEMENT_3D ( 'NONE', #73256, #55607, #48847 ) ;
#60928 = EDGE_CURVE ( 'NONE', #43117, #23577, #53618, .T. ) ;
#60929 = ORIENTED_EDGE ( 'NONE', *, *, #69530, .F. ) ;
#60930 = DIRECTION ( 'NONE',  ( 1.000000000000000000, 0.000000000000000000, 0.000000000000000000 ) ) ;
#60931 = ORIENTED_EDGE ( 'NONE', *, *, #23113, .F. ) ;
#60932 = DIRECTION ( 'NONE',  ( -1.000000000000000000, 0.000000000000000000, 0.000000000000000000 ) ) ;
#60933 = CYLINDRICAL_SURFACE ( 'NONE', #12828, 31.99999999999998579 ) ;
#60934 = EDGE_CURVE ( 'NONE', #31764, #27635, #4209, .T. ) ;
#60935 = ORIENTED_EDGE ( 'NONE', *, *, #39683, .F. ) ;
#60936 = FACE_OUTER_BOUND ( 'NONE', #43901, .T. ) ;
#60937 = ORIENTED_EDGE ( 'NONE', *, *, #51102, .F. ) ;
#60938 = CARTESIAN_POINT ( 'NONE',  ( 0.000000000000000000, 56.15606465354959198, 59.75363087400094741 ) ) ;
#60939 = EDGE_CURVE ( 'NONE', #26439, #11277, #10373, .T. ) ;
#60940 = ORIENTED_EDGE ( 'NONE', *, *, #35828, .T. ) ;
#60941 = ORIENTED_EDGE ( 'NONE', *, *, #2231, .T. ) ;
#60942 = ORIENTED_EDGE ( 'NONE', *, *, #14862, .F. ) ;
#60943 = CARTESIAN_POINT ( 'NONE',  ( -3.346878500200759277, -3.841181488860386573, -5.948595712916170619 ) ) ;
#60944 = CARTESIAN_POINT ( 'NONE',  ( -90.00000000000002842, 85.00000000000002842, 90.00000000000000000 ) ) ;
#60945 = ORIENTED_EDGE ( 'NONE', *, *, #66407, .T. ) ;
#60946 = AXIS2_PLACEMENT_3D ( 'NONE', #4354, #46323, #23033 ) ;
#60947 = ORIENTED_EDGE ( 'NONE', *, *, #28423, .F. ) ;
#60948 = ORIENTED_EDGE ( 'NONE', *, *, #4083, .T. ) ;
#60949 = CARTESIAN_POINT ( 'NONE',  ( -94.99999999999997158, -209.9999999999999716, 90.00000000000000000 ) ) ;
#60950 = CARTESIAN_POINT ( 'NONE',  ( 0.000000000000000000, -46.54456581323847786, 59.03342792756247093 ) ) ;
#60951 = EDGE_CURVE ( 'NONE', #16018, #8967, #3837, .T. ) ;
#60952 = CARTESIAN_POINT ( 'NONE',  ( -96.15314808468752972, 91.99731107132950569, 79.53572916753381605 ) ) ;
#60953 = ADVANCED_FACE ( 'NONE', ( #27856, #49303 ), #21461, .T. ) ;
#60954 = ORIENTED_EDGE ( 'NONE', *, *, #43068, .F. ) ;
#60955 = CARTESIAN_POINT ( 'NONE',  ( 97.30629616937498838, 88.66845928578037217, 79.11239583420046984 ) ) ;
#60956 = ORIENTED_EDGE ( 'NONE', *, *, #11023, .F. ) ;
#60957 = CARTESIAN_POINT ( 'NONE',  ( 10.00000000000000000, 54.21277698773752718, -55.38113227695725271 ) ) ;
#60958 = CARTESIAN_POINT ( 'NONE',  ( 0.000000000000000000, 79.10210256391398786, -21.60688246758503084 ) ) ;
#60959 = CARTESIAN_POINT ( 'NONE',  ( 2.744988726042924210, -4.188682711992893992, -0.5083873451168847701 ) ) ;
#60960 = DIRECTION ( 'NONE',  ( 0.000000000000000000, 0.9876883405951372152, 0.1564344650402346160 ) ) ;
#60961 = DIRECTION ( 'NONE',  ( -1.000000000000000000, 0.000000000000000000, -0.000000000000000000 ) ) ;
#60962 = CARTESIAN_POINT ( 'NONE',  ( -97.30629616937497417, -211.3315407142195852, 80.17072916753380696 ) ) ;
#60963 = CARTESIAN_POINT ( 'NONE',  ( 11.41210121379328335, -99.40233154247455616, -5.500000000000000000 ) ) ;
#60964 = DIRECTION ( 'NONE',  ( -1.000000000000000000, -0.000000000000000000, 0.000000000000000000 ) ) ;
#60965 = DIRECTION ( 'NONE',  ( 1.000000000000000000, -1.047380211910311281E-14, -2.618450529775778123E-14 ) ) ;
#60966 = ORIENTED_EDGE ( 'NONE', *, *, #36313, .T. ) ;
#60967 = EDGE_CURVE ( 'NONE', #8405, #24336, #46388, .T. ) ;
#60968 = EDGE_CURVE ( 'NONE', #23196, #53520, #62467, .T. ) ;
#60969 = ORIENTED_EDGE ( 'NONE', *, *, #48957, .T. ) ;
#60970 = CARTESIAN_POINT ( 'NONE',  ( -2.499999999999992895, 7.589415207398510330E-16, 0.000000000000000000 ) ) ;
#60971 = CARTESIAN_POINT ( 'NONE',  ( -20.63750000000000284, -2.946905753441389499E-14, -1.643265707204933640E-14 ) ) ;
#60972 = CARTESIAN_POINT ( 'NONE',  ( 92.57708711457300410, -209.3980460039466891, 74.90604073465182466 ) ) ;
#60973 = CARTESIAN_POINT ( 'NONE',  ( -96.15314808468751551, 88.00268892867056536, 84.66864583420047552 ) ) ;
#60974 = DIRECTION ( 'NONE',  ( 0.000000000000000000, 0.8910065241883690090, -0.4539904997395446395 ) ) ;
#60975 = DIRECTION ( 'NONE',  ( -1.000000000000000000, 0.000000000000000000, 0.000000000000000000 ) ) ;
#60976 = AXIS2_PLACEMENT_3D ( 'NONE', #63174, #40596, #51873 ) ;
#60977 = ORIENTED_EDGE ( 'NONE', *, *, #20410, .F. ) ;
#60978 = CARTESIAN_POINT ( 'NONE',  ( 10.00000000000000000, -30.84782396557201878, -21.32104025579148399 ) ) ;
#60979 = AXIS2_PLACEMENT_3D ( 'NONE', #72789, #26198, #31839 ) ;
#60980 = AXIS2_PLACEMENT_3D ( 'NONE', #35923, #59239, #13729 ) ;
#60981 = CARTESIAN_POINT ( 'NONE',  ( 92.35000000003284981, 90.00000839192529156, 86.90410584365271518 ) ) ;
#60982 = CYLINDRICAL_SURFACE ( 'NONE', #59785, 16.00000000000000000 ) ;
#60983 = CIRCLE ( 'NONE', #28555, 37.49900000000000944 ) ;
#60984 = DIRECTION ( 'NONE',  ( 1.000000000000000000, 0.000000000000000000, 0.000000000000000000 ) ) ;
#60985 = CARTESIAN_POINT ( 'NONE',  ( -97.30629616937497417, -208.6684592857803011, 82.12864583420048348 ) ) ;
#60986 = VECTOR ( 'NONE', #32030, 1000.000000000000000 ) ;
#60987 = CARTESIAN_POINT ( 'NONE',  ( 92.34999999999999432, 90.00001272927832474, 76.10937456147250657 ) ) ;
#60988 = DIRECTION ( 'NONE',  ( -1.000000000000000000, 0.000000000000000000, 0.000000000000000000 ) ) ;
#60989 = CARTESIAN_POINT ( 'NONE',  ( 10.00000000000000000, 39.78640506895700213, -66.50666863321957578 ) ) ;
#60990 = FACE_OUTER_BOUND ( 'NONE', #9861, .T. ) ;
#60991 = ORIENTED_EDGE ( 'NONE', *, *, #21907, .T. ) ;
#60992 = FACE_OUTER_BOUND ( 'NONE', #1539, .T. ) ;
#60993 = LINE ( 'NONE', #42606, #37126 ) ;
#60994 = DIRECTION ( 'NONE',  ( -0.7950889364178796992, 0.6064928550163510845, 0.000000000000000000 ) ) ;
#60995 = AXIS2_PLACEMENT_3D ( 'NONE', #64915, #25050, #69433 ) ;
#60996 = VECTOR ( 'NONE', #73561, 1000.000000000000000 ) ;
#60997 = EDGE_CURVE ( 'NONE', #69599, #2465, #816, .T. ) ;
#60999 = DIRECTION ( 'NONE',  ( -1.000000000000000000, -0.000000000000000000, -0.000000000000000000 ) ) ;
#60998 = VECTOR ( 'NONE', #5377, 1000.000000000000114 ) ;
#61000 = ORIENTED_EDGE ( 'NONE', *, *, #14572, .T. ) ;
#61002 = EDGE_CURVE ( 'NONE', #21836, #49121, #44422, .T. ) ;
#61001 = AXIS2_PLACEMENT_3D ( 'NONE', #21118, #4230, #67363 ) ;
#61003 = LINE ( 'NONE', #38815, #50428 ) ;
#61004 = DIRECTION ( 'NONE',  ( 0.000000000000000000, 0.000000000000000000, 1.000000000000000000 ) ) ;
#61005 = EDGE_LOOP ( 'NONE', ( #15042, #6564, #48250, #57600 ) ) ;
#61006 = ADVANCED_FACE ( 'NONE', ( #9452 ), #72229, .T. ) ;
#61007 = CYLINDRICAL_SURFACE ( 'NONE', #60399, 82.00000000000000000 ) ;
#61008 = CARTESIAN_POINT ( 'NONE',  ( 93.67500000000001137, -207.7050326799711968, 86.08416666666666117 ) ) ;
#61009 = ORIENTED_EDGE ( 'NONE', *, *, #21629, .T. ) ;
#61010 = EDGE_CURVE ( 'NONE', #24964, #64024, #60823, .T. ) ;
#61011 = DIRECTION ( 'NONE',  ( -1.000000000000000000, 0.000000000000000000, 0.000000000000000000 ) ) ;
#61012 = ORIENTED_EDGE ( 'NONE', *, *, #29973, .F. ) ;
#61013 = DIRECTION ( 'NONE',  ( 0.000000000000000000, 0.4539904997395413089, 0.8910065241883705633 ) ) ;
#61014 = ORIENTED_EDGE ( 'NONE', *, *, #43079, .F. ) ;
#61015 = ADVANCED_FACE ( 'NONE', ( #50414 ), #38404, .T. ) ;
#61016 = ORIENTED_EDGE ( 'NONE', *, *, #17229, .T. ) ;
#61017 = ORIENTED_EDGE ( 'NONE', *, *, #4721, .F. ) ;
#61018 = EDGE_LOOP ( 'NONE', ( #1702, #1424, #43676, #39878 ) ) ;
#61019 = DIRECTION ( 'NONE',  ( 0.000000000000000000, 0.000000000000000000, 1.000000000000000000 ) ) ;
#61020 = ORIENTED_EDGE ( 'NONE', *, *, #69762, .F. ) ;
#61021 = ORIENTED_EDGE ( 'NONE', *, *, #18442, .T. ) ;
#61022 = CARTESIAN_POINT ( 'NONE',  ( 94.99999999999998579, 87.33691857156068750, 75.99031250086716227 ) ) ;
#61023 = CARTESIAN_POINT ( 'NONE',  ( 10.00000000000000000, 33.80338159004283938, 16.23288003029508886 ) ) ;
#61024 = EDGE_CURVE ( 'NONE', #27107, #24755, #18788, .T. ) ;
#61025 = CIRCLE ( 'NONE', #45435, 26.50000000000000355 ) ;
#61026 = DIRECTION ( 'NONE',  ( 0.000000000000000000, -0.07845909572783053842, -0.9969173337331290741 ) ) ;
#61027 = STYLED_ITEM ( 'NONE', ( #9940 ), #12651 ) ;
#61028 = EDGE_LOOP ( 'NONE', ( #8595, #25255, #71715, #34671, #74047, #45692, #67784, #15368 ) ) ;
#61029 = CIRCLE ( 'NONE', #2251, 77.49899999999998101 ) ;
#61030 = ORIENTED_EDGE ( 'NONE', *, *, #54147, .F. ) ;
#61031 = EDGE_LOOP ( 'NONE', ( #20409, #38902, #50701, #20995 ) ) ;
#61032 = CARTESIAN_POINT ( 'NONE',  ( 93.84685191531248449, 88.00268892867053694, 87.20864583420046756 ) ) ;
#61033 = VERTEX_POINT ( 'NONE', #44795 ) ;
#61034 = CARTESIAN_POINT ( 'NONE',  ( 95.00000000000000000, -213.0599564267049857, 74.99812500173430863 ) ) ;
#61035 = CARTESIAN_POINT ( 'NONE',  ( -94.99999999999968736, 89.99999999999876366, 102.7499999999999716 ) ) ;
#61036 = FACE_OUTER_BOUND ( 'NONE', #73323, .T. ) ;
#61037 = AXIS2_PLACEMENT_3D ( 'NONE', #48941, #49316, #15104 ) ;
#61038 = CARTESIAN_POINT ( 'NONE',  ( 1.560000000000000053, -0.8660254037844384856, 1.500000000000000000 ) ) ;
#61039 = DIRECTION ( 'NONE',  ( 1.000000000000000000, -0.000000000000000000, 0.000000000000000000 ) ) ;
#61040 = CIRCLE ( 'NONE', #4609, 15.70000000000326956 ) ;
#61041 = DIRECTION ( 'NONE',  ( -0.000000000000000000, 1.000000000000000000, 0.000000000000000000 ) ) ;
#61042 = CARTESIAN_POINT ( 'NONE',  ( 0.000000000000000000, 22.64427369931212297, -30.00120703465181293 ) ) ;
#61043 = LINE ( 'NONE', #42647, #2304 ) ;
#61044 = CARTESIAN_POINT ( 'NONE',  ( -96.32499999999996021, -207.7050326799711968, 77.27354166840096639 ) ) ;
#61045 = EDGE_CURVE ( 'NONE', #52606, #36080, #72811, .T. ) ;
#61046 = DIRECTION ( 'NONE',  ( 0.000000000000000000, 0.000000000000000000, 1.000000000000000000 ) ) ;
#61047 = ADVANCED_FACE ( 'NONE', ( #23703 ), #69567, .T. ) ;
#61048 = EDGE_LOOP ( 'NONE', ( #6212, #45495, #25657, #28869 ) ) ;
#61049 = UNCERTAINTY_MEASURE_WITH_UNIT (LENGTH_MEASURE( 1.000000000000000082E-05 ), #33615, 'distance_accuracy_value', 'NONE');
#61051 = CARTESIAN_POINT ( 'NONE',  ( -93.84685191531254134, 91.99731107132950569, 88.16114583420046813 ) ) ;
#61050 = CARTESIAN_POINT ( 'NONE',  ( 92.69370383062498320, 88.66845928578037217, 87.15572916753380639 ) ) ;
#61052 = ORIENTED_EDGE ( 'NONE', *, *, #55658, .F. ) ;
#61053 = CARTESIAN_POINT ( 'NONE',  ( 0.000000000000000000, -74.18225833017864090, -34.94270380257719211 ) ) ;
#61054 = LINE ( 'NONE', #39239, #9774 ) ;
#61055 = DIRECTION ( 'NONE',  ( 1.000000000000000000, -7.331661483372147883E-15, -2.618450529775767079E-14 ) ) ;
#61056 = CARTESIAN_POINT ( 'NONE',  ( 11.99999999999999822, -80.55351364060578589, -15.33399622253569383 ) ) ;
#61057 = CARTESIAN_POINT ( 'NONE',  ( -94.99999999999997158, -212.6630814284392557, 88.53156250086716739 ) ) ;
#61058 = DIRECTION ( 'NONE',  ( 0.000000000000000000, -0.7604059656000227152, -0.6494480483301933171 ) ) ;
#61059 = AXIS2_PLACEMENT_3D ( 'NONE', #50545, #4714, #50918 ) ;
#61060 = DIRECTION ( 'NONE',  ( 1.000000000000000000, -0.000000000000000000, 0.000000000000000000 ) ) ;
#61061 = FACE_OUTER_BOUND ( 'NONE', #61688, .T. ) ;
#61062 = ORIENTED_EDGE ( 'NONE', *, *, #55153, .F. ) ;
#61063 = VECTOR ( 'NONE', #43661, 1000.000000000000000 ) ;
#61064 = ORIENTED_EDGE ( 'NONE', *, *, #44994, .F. ) ;
#61065 = CIRCLE ( 'NONE', #40668, 16.00000000000000355 ) ;
#61066 = VECTOR ( 'NONE', #16599, 1000.000000000000000 ) ;
#61067 = CARTESIAN_POINT ( 'NONE',  ( -97.65000000000001990, 91.52997821335253548, 79.78708333333332803 ) ) ;
#61068 = DIRECTION ( 'NONE',  ( -1.000000000000000000, 0.000000000000000000, 0.000000000000000000 ) ) ;
#61069 = CARTESIAN_POINT ( 'NONE',  ( 96.32499999999998863, -212.2949673200287179, 75.68604166840097491 ) ) ;
#61070 = DIRECTION ( 'NONE',  ( -1.000000000000000000, 0.000000000000000000, 0.000000000000000000 ) ) ;
#61071 = CARTESIAN_POINT ( 'NONE',  ( 97.64999999999999147, 90.00000000000002842, 75.07749999999998636 ) ) ;
#61072 = CYLINDRICAL_SURFACE ( 'NONE', #25132, 82.00000000000000000 ) ;
#61073 = AXIS2_PLACEMENT_3D ( 'NONE', #72899, #50729, #61654 ) ;
#61074 = EDGE_LOOP ( 'NONE', ( #67785, #9628, #1438, #401 ) ) ;
#61075 = CARTESIAN_POINT ( 'NONE',  ( -96.15314808468752972, 91.99731107132950569, 81.28197916753380525 ) ) ;
#61076 = DIRECTION ( 'NONE',  ( 2.603472992746261562E-14, 2.546204323184492723E-14, -1.000000000000000000 ) ) ;
#61077 = PLANE ( 'NONE',  #25851 ) ;
#61078 = DIRECTION ( 'NONE',  ( -1.000000000000000000, 0.000000000000000000, 0.000000000000000000 ) ) ;
#61079 = CARTESIAN_POINT ( 'NONE',  ( 5.000000000000002665, -76.69515212746036070, 29.01471420065537643 ) ) ;
#61080 = CARTESIAN_POINT ( 'NONE',  ( 11.99999999999999822, 65.64334221924909230, 41.19522573413756561 ) ) ;
#61081 = DIRECTION ( 'NONE',  ( -1.000000000000000000, 0.000000000000000000, -0.000000000000000000 ) ) ;
#61082 = DIRECTION ( 'NONE',  ( -0.000000000000000000, 0.2079116908177543743, 0.9781476007338066880 ) ) ;
#61083 = CYLINDRICAL_SURFACE ( 'NONE', #50871, 31.99999999999999289 ) ;
#61084 = EDGE_CURVE ( 'NONE', #19565, #53812, #18066, .T. ) ;
#61085 =( BOUNDED_SURFACE ( )  B_SPLINE_SURFACE ( 1, 2, ( 
 ( #1447, #24332, #64555, #52154, #699, #58171, #19418, #23590, #41256, #17949, #6669, #29575, #64937, #70172, #24696, #58923, #70918, #59285, #46521, #69446, #40891, #63828, #64195, #1072, #69811, #65304, #1810, #12668, #13033, #35600, #58535, #7413, #53272, #71279, #43116, #3276, #20904, #66048, #14521, #49475, #8141, #37839, #37475, #43855, #26542, #20155, #14896, #32171, #60770, #32547, #15265, #26167, #66770, #60406, #8887, #9629, #66415, #42732, #55493, #2913, #61139, #21256, #48733, #49103, #3642, #65666, #72399, #71657, #38197, #31804, #9250, #4008, #26908, #55115, #72029, #49838, #72756, #31065, #54748, #25803, #44217, #38577, #67140, #15643, #54021, #20542, #2559, #25439, #48367, #43495, #54381, #19783, #14144, #37094, #60044, #8528, #31440, #68264, #33283, #44962, #67888, #39321, #46070, #73884, #45719, #56986, #5493, #45340, #34037, #17124, #5859, #50584, #38946, #73509, #28389, #5121, #61509, #27659, #50203, #33666, #51324, #34404, #51708, #69003, #16759, #74261, #17491, #40055, #28768, #44596, #255, #50962, #57347, #68642, #67514, #16379, #63016, #10364, #16002, #11474, #9991, #22392, #61884, #22018, #73137, #56621, #62256, #22778, #10742, #56238, #23147, #32911, #55863, #4374, #27272, #21643, #4753, #39698, #28019, #62637, #11113, #58445, #29868, #41906, #69361, #58830, #18593, #6232, #2091, #30606, #52068, #7328, #41170, #1362, #12944, #63740, #63368, #17859, #70450, #64107, #47913, #40418, #35519, #1721, #41532, #29131, #24977, #53554, #611, #30246, #12586, #24253, #35881, #12216, #11834, #40805, #18958, #6943, #70831, #34785, #52818, #24609, #47177, #23503, #64846, #35153, #13326, #57726, #6590, #70089, #53185, #46435, #47547, #29494, #36258, #52430, #64470, #59198, #7689, #58088, #985, #23877, #46815, #69730, #18230, #37003, #20457, #49746, #55028, #38108, #61044, #14053, #37751, #49390, #65215, #25718, #65586, #59571, #3558, #71943, #43768, #65964, #2472, #26082, #59955, #2827, #48655, #71572, #3924, #31718, #26456, #14804, #60686, #3190, #66331, #72318, #9544, #8440, #71193, #31352, #9165, #37389, #19332, #54303, #8057, #14436, #32087, #66688, #32459, #26820, #49011, #20816, #42289, #15172, #55401, #25357, #13689, #8800, #36626, #30978, #48285, #20067, #53933, #42648, #19698 ),
 ( #43023, #60324, #54663, #43410, #10648, #27181, #5768, #21933, #68551, #28675, #73043, #67424, #39605, #11385, #61425, #17037, #44875, #44506, #15921, #16666, #72670, #56530, #33574, #50109, #21172, #67798, #39973, #44121, #21550, #38853, #62547, #34320, #9905, #62928, #16291, #61797, #10278, #56144, #67047, #4292, #5407, #50498, #22305, #32825, #45250, #33199, #57263, #15552, #38487, #4663, #28301, #27569, #55775, #27937, #11026, #51238, #73423, #39232, #62161, #5033, #50868, #73792, #68166, #74170, #33952, #56898, #22684, #45632, #29402, #45988, #1637, #896, #1277, #41442, #29773, #52348, #64019, #46723, #29047, #35066, #23058, #23782, #69647, #12494, #7604, #51615, #34689, #41808, #167, #63656, #40335, #57643, #6142, #64385, #18141, #47096, #6861, #70361, #58742, #68914, #17402, #59115, #63282, #12125, #11742, #51979, #24521, #24164, #70001, #41087, #525, #30154, #57998, #35432, #23419, #6502, #58361, #12857, #52725, #18502, #35786, #46351, #7240, #53098, #47456, #18869, #64754, #13240, #36167, #69278, #17766, #40712, #48563, #15743, #65498, #31267, #33018, #44316, #61987, #36908, #42197, #54215, #25271, #42558, #27006, #55963, #49939, #4480, #21750, #39051, #14349, #67248, #16110, #10096, #73244, #13606, #44703, #19978, #27376, #38679, #36532, #13964, #61609, #53829, #59479, #50313, #30517, #42933, #7968, #19611, #19246, #2744, #8343, #67616, #59855, #2379, #53465, #2000, #24889, #47819, #70740, #65129, #30885, #65865, #71478, #72855, #48195, #37299, #60236, #71106, #25630, #21356, #8713, #31631, #55592, #4110, #22125, #51810, #11215, #45821, #57453, #33773, #33385, #39424, #40525, #34144, #17965, #10468, #5596, #46174, #68744, #45067, #34892, #5228, #63472, #23608, #51064, #28491, #5971, #67991, #28877, #73988, #357, #22503, #11572, #23246, #6334, #17227, #51430, #34507, #57828, #56347, #45444, #28127, #69110, #40907, #17595, #29230, #52169, #68377, #11945, #716, #4862, #16866, #56729, #50691, #46538, #63117, #69465, #57091, #16485, #40162, #39796, #62750, #17246, #22885, #27764, #73614, #62369, #10849, #7790, #47645, #36358, #19433, #8155, #52921, #41271, #1461, #30709, #7431, #63845, #29976, #52535, #35989, #24712, #59298, #12683, #12319, #18330, #42383, #64568, #71296, #35257, #58939, #25081 ) ),
 .UNSPECIFIED., .F., .F., .T. ) 
 B_SPLINE_SURFACE_WITH_KNOTS ( ( 2, 2 ),
 ( 3, 2, 2, 2, 2, 2, 2, 2, 2, 2, 2, 2, 2, 2, 2, 2, 2, 2, 2, 2, 2, 2, 2, 2, 2, 2, 2, 2, 2, 2, 2, 2, 2, 2, 2, 2, 2, 2, 2, 2, 2, 2, 2, 2, 2, 2, 2, 2, 2, 2, 2, 2, 2, 2, 2, 2, 2, 2, 2, 2, 2, 2, 2, 2, 2, 2, 2, 2, 2, 2, 2, 2, 2, 2, 2, 2, 2, 2, 2, 2, 2, 2, 2, 2, 2, 2, 2, 2, 2, 2, 2, 2, 2, 2, 2, 2, 2, 2, 2, 2, 2, 2, 2, 2, 2, 2, 2, 2, 2, 2, 2, 2, 2, 2, 2, 2, 2, 2, 2, 2, 2, 2, 2, 2, 2, 2, 2, 2, 2, 2, 2, 2, 2, 2, 2, 2, 2, 2, 2, 2, 2, 2, 3 ),
 ( 0.000000000000000000, 1.000000000000000000 ),
 ( 0.000000000000000000, 0.006944444444444444059, 0.01388888888888888812, 0.02083333333333333218, 0.02777777777777777624, 0.03472222222222222376, 0.04166666666666666435, 0.04861111111111111188, 0.05555555555555555247, 0.06250000000000000000, 0.06944444444444444753, 0.07638888888888889506, 0.08333333333333332871, 0.09027777777777777624, 0.09722222222222222376, 0.1041666666666666713, 0.1111111111111111049, 0.1180555555555555525, 0.1250000000000000000, 0.1319444444444444475, 0.1388888888888888951, 0.1458333333333333426, 0.1527777777777777901, 0.1597222222222222099, 0.1666666666666666574, 0.1736111111111111049, 0.1805555555555555525, 0.1875000000000000000, 0.1944444444444444475, 0.2013888888888888951, 0.2083333333333333426, 0.2152777777777777901, 0.2222222222222222099, 0.2291666666666666574, 0.2361111111111111049, 0.2430555555555555525, 0.2500000000000000000, 0.2569444444444444198, 0.2638888888888888951, 0.2708333333333333148, 0.2777777777777777901, 0.2847222222222222099, 0.2916666666666666852, 0.2986111111111111049, 0.3055555555555555802, 0.3125000000000000000, 0.3194444444444444198, 0.3263888888888888951, 0.3333333333333333148, 0.3402777777777777901, 0.3472222222222222099, 0.3541666666666666852, 0.3611111111111111049, 0.3680555555555555802, 0.3750000000000000000, 0.3819444444444444198, 0.3888888888888888951, 0.3958333333333333148, 0.4027777777777777901, 0.4097222222222222099, 0.4166666666666666852, 0.4236111111111111049, 0.4305555555555555802, 0.4375000000000000000, 0.4444444444444444198, 0.4513888888888888951, 0.4583333333333333148, 0.4652777777777777901, 0.4722222222222222099, 0.4791666666666666852, 0.4861111111111111049, 0.4930555555555555802, 0.5000000000000000000, 0.5069444444444444198, 0.5138888888888888395, 0.5208333333333333703, 0.5277777777777777901, 0.5347222222222222099, 0.5416666666666666297, 0.5486111111111111605, 0.5555555555555555802, 0.5625000000000000000, 0.5694444444444444198, 0.5763888888888888395, 0.5833333333333333703, 0.5902777777777777901, 0.5972222222222222099, 0.6041666666666666297, 0.6111111111111111605, 0.6180555555555555802, 0.6250000000000000000, 0.6319444444444444198, 0.6388888888888888395, 0.6458333333333333703, 0.6527777777777777901, 0.6597222222222222099, 0.6666666666666666297, 0.6736111111111111605, 0.6805555555555555802, 0.6875000000000000000, 0.6944444444444444198, 0.7013888888888888395, 0.7083333333333333703, 0.7152777777777777901, 0.7222222222222222099, 0.7291666666666666297, 0.7361111111111111605, 0.7430555555555555802, 0.7500000000000000000, 0.7569444444444444198, 0.7638888888888888395, 0.7708333333333333703, 0.7777777777777777901, 0.7847222222222222099, 0.7916666666666666297, 0.7986111111111111605, 0.8055555555555555802, 0.8125000000000000000, 0.8194444444444444198, 0.8263888888888888395, 0.8333333333333333703, 0.8402777777777777901, 0.8472222222222222099, 0.8541666666666666297, 0.8611111111111111605, 0.8680555555555555802, 0.8750000000000000000, 0.8819444444444444198, 0.8888888888888888395, 0.8958333333333333703, 0.9027777777777777901, 0.9097222222222222099, 0.9166666666666666297, 0.9236111111111111605, 0.9305555555555555802, 0.9375000000000000000, 0.9444444444444444198, 0.9513888888888888395, 0.9583333333333333703, 0.9652777777777777901, 0.9722222222222222099, 0.9791666666666666297, 0.9842226981114290396 ),
 .UNSPECIFIED. ) 
 GEOMETRIC_REPRESENTATION_ITEM ( )  RATIONAL_B_SPLINE_SURFACE ( (
 ( 1.000000000000000000, 0.8660254037844387076, 1.000000000000000000, 0.8660254037844387076, 1.000000000000000000, 0.8660254037844387076, 1.000000000000000000, 0.8660254037844387076, 1.000000000000000000, 0.8660254037844387076, 1.000000000000000000, 0.8660254037844387076, 1.000000000000000000, 0.8660254037844387076, 1.000000000000000000, 0.8660254037844387076, 1.000000000000000000, 0.8660254037844387076, 1.000000000000000000, 0.8660254037844387076, 1.000000000000000000, 0.8660254037844387076, 1.000000000000000000, 0.8660254037844387076, 1.000000000000000000, 0.8660254037844387076, 1.000000000000000000, 0.8660254037844387076, 1.000000000000000000, 0.8660254037844387076, 1.000000000000000000, 0.8660254037844387076, 1.000000000000000000, 0.8660254037844387076, 1.000000000000000000, 0.8660254037844387076, 1.000000000000000000, 0.8660254037844387076, 1.000000000000000000, 0.8660254037844387076, 1.000000000000000000, 0.8660254037844387076, 1.000000000000000000, 0.8660254037844387076, 1.000000000000000000, 0.8660254037844387076, 1.000000000000000000, 0.8660254037844387076, 1.000000000000000000, 0.8660254037844387076, 1.000000000000000000, 0.8660254037844387076, 1.000000000000000000, 0.8660254037844387076, 1.000000000000000000, 0.8660254037844387076, 1.000000000000000000, 0.8660254037844387076, 1.000000000000000000, 0.8660254037844387076, 1.000000000000000000, 0.8660254037844387076, 1.000000000000000000, 0.8660254037844387076, 1.000000000000000000, 0.8660254037844387076, 1.000000000000000000, 0.8660254037844387076, 1.000000000000000000, 0.8660254037844387076, 1.000000000000000000, 0.8660254037844387076, 1.000000000000000000, 0.8660254037844387076, 1.000000000000000000, 0.8660254037844387076, 1.000000000000000000, 0.8660254037844387076, 1.000000000000000000, 0.8660254037844387076, 1.000000000000000000, 0.8660254037844387076, 1.000000000000000000, 0.8660254037844387076, 1.000000000000000000, 0.8660254037844387076, 1.000000000000000000, 0.8660254037844387076, 1.000000000000000000, 0.8660254037844387076, 1.000000000000000000, 0.8660254037844387076, 1.000000000000000000, 0.8660254037844387076, 1.000000000000000000, 0.8660254037844387076, 1.000000000000000000, 0.8660254037844387076, 1.000000000000000000, 0.8660254037844387076, 1.000000000000000000, 0.8660254037844387076, 1.000000000000000000, 0.8660254037844387076, 1.000000000000000000, 0.8660254037844387076, 1.000000000000000000, 0.8660254037844387076, 1.000000000000000000, 0.8660254037844387076, 1.000000000000000000, 0.8660254037844387076, 1.000000000000000000, 0.8660254037844387076, 1.000000000000000000, 0.8660254037844387076, 1.000000000000000000, 0.8660254037844387076, 1.000000000000000000, 0.8660254037844387076, 1.000000000000000000, 0.8660254037844387076, 1.000000000000000000, 0.8660254037844387076, 1.000000000000000000, 0.8660254037844387076, 1.000000000000000000, 0.8660254037844387076, 1.000000000000000000, 0.8660254037844387076, 1.000000000000000000, 0.8660254037844387076, 1.000000000000000000, 0.8660254037844387076, 1.000000000000000000, 0.8660254037844387076, 1.000000000000000000, 0.8660254037844387076, 1.000000000000000000, 0.8660254037844387076, 1.000000000000000000, 0.8660254037844387076, 1.000000000000000000, 0.8660254037844387076, 1.000000000000000000, 0.8660254037844387076, 1.000000000000000000, 0.8660254037844387076, 1.000000000000000000, 0.8660254037844387076, 1.000000000000000000, 0.8660254037844387076, 1.000000000000000000, 0.8660254037844387076, 1.000000000000000000, 0.8660254037844387076, 1.000000000000000000, 0.8660254037844387076, 1.000000000000000000, 0.8660254037844387076, 1.000000000000000000, 0.8660254037844387076, 1.000000000000000000, 0.8660254037844387076, 1.000000000000000000, 0.8660254037844387076, 1.000000000000000000, 0.8660254037844387076, 1.000000000000000000, 0.8660254037844387076, 1.000000000000000000, 0.8660254037844387076, 1.000000000000000000, 0.8660254037844387076, 1.000000000000000000, 0.8660254037844387076, 1.000000000000000000, 0.8660254037844387076, 1.000000000000000000, 0.8660254037844387076, 1.000000000000000000, 0.8660254037844387076, 1.000000000000000000, 0.8660254037844387076, 1.000000000000000000, 0.8660254037844387076, 1.000000000000000000, 0.8660254037844387076, 1.000000000000000000, 0.8660254037844387076, 1.000000000000000000, 0.8660254037844387076, 1.000000000000000000, 0.8660254037844387076, 1.000000000000000000, 0.8660254037844387076, 1.000000000000000000, 0.8660254037844387076, 1.000000000000000000, 0.8660254037844387076, 1.000000000000000000, 0.8660254037844387076, 1.000000000000000000, 0.8660254037844387076, 1.000000000000000000, 0.8660254037844387076, 1.000000000000000000, 0.8660254037844387076, 1.000000000000000000, 0.8660254037844387076, 1.000000000000000000, 0.8660254037844387076, 1.000000000000000000, 0.8660254037844387076, 1.000000000000000000, 0.8660254037844387076, 1.000000000000000000, 0.8660254037844387076, 1.000000000000000000, 0.8660254037844387076, 1.000000000000000000, 0.8660254037844387076, 1.000000000000000000, 0.8660254037844387076, 1.000000000000000000, 0.8660254037844387076, 1.000000000000000000, 0.8660254037844387076, 1.000000000000000000, 0.8660254037844387076, 1.000000000000000000, 0.8660254037844387076, 1.000000000000000000, 0.8660254037844387076, 1.000000000000000000, 0.8660254037844387076, 1.000000000000000000, 0.8660254037844387076, 1.000000000000000000, 0.8660254037844387076, 1.000000000000000000, 0.8660254037844387076, 1.000000000000000000, 0.8660254037844387076, 1.000000000000000000, 0.8660254037844387076, 1.000000000000000000, 0.8660254037844387076, 1.000000000000000000, 0.8660254037844387076, 1.000000000000000000, 0.8660254037844387076, 1.000000000000000000, 0.8660254037844387076, 1.000000000000000000, 0.8660254037844387076, 1.000000000000000000, 0.8660254037844387076, 1.000000000000000000, 0.8660254037844387076, 1.000000000000000000, 0.8660254037844387076, 1.000000000000000000, 0.8660254037844387076, 1.000000000000000000, 0.8660254037844387076, 1.000000000000000000, 0.8660254037844387076, 1.000000000000000000, 0.8660254037844387076, 1.000000000000000000, 0.8660254037844387076, 1.000000000000000000, 0.8660254037844387076, 1.000000000000000000, 0.8660254037844387076, 1.000000000000000000, 0.8660254037844387076, 1.000000000000000000, 0.8660254037844387076, 1.000000000000000000, 0.8660254037844387076, 1.000000000000000000, 0.9024573129378088421, 0.9469501470576167090),
 ( 1.000000000000000000, 0.8660254037844387076, 1.000000000000000000, 0.8660254037844387076, 1.000000000000000000, 0.8660254037844387076, 1.000000000000000000, 0.8660254037844387076, 1.000000000000000000, 0.8660254037844387076, 1.000000000000000000, 0.8660254037844387076, 1.000000000000000000, 0.8660254037844387076, 1.000000000000000000, 0.8660254037844387076, 1.000000000000000000, 0.8660254037844387076, 1.000000000000000000, 0.8660254037844387076, 1.000000000000000000, 0.8660254037844387076, 1.000000000000000000, 0.8660254037844387076, 1.000000000000000000, 0.8660254037844387076, 1.000000000000000000, 0.8660254037844387076, 1.000000000000000000, 0.8660254037844387076, 1.000000000000000000, 0.8660254037844387076, 1.000000000000000000, 0.8660254037844387076, 1.000000000000000000, 0.8660254037844387076, 1.000000000000000000, 0.8660254037844387076, 1.000000000000000000, 0.8660254037844387076, 1.000000000000000000, 0.8660254037844387076, 1.000000000000000000, 0.8660254037844387076, 1.000000000000000000, 0.8660254037844387076, 1.000000000000000000, 0.8660254037844387076, 1.000000000000000000, 0.8660254037844387076, 1.000000000000000000, 0.8660254037844387076, 1.000000000000000000, 0.8660254037844387076, 1.000000000000000000, 0.8660254037844387076, 1.000000000000000000, 0.8660254037844387076, 1.000000000000000000, 0.8660254037844387076, 1.000000000000000000, 0.8660254037844387076, 1.000000000000000000, 0.8660254037844387076, 1.000000000000000000, 0.8660254037844387076, 1.000000000000000000, 0.8660254037844387076, 1.000000000000000000, 0.8660254037844387076, 1.000000000000000000, 0.8660254037844387076, 1.000000000000000000, 0.8660254037844387076, 1.000000000000000000, 0.8660254037844387076, 1.000000000000000000, 0.8660254037844387076, 1.000000000000000000, 0.8660254037844387076, 1.000000000000000000, 0.8660254037844387076, 1.000000000000000000, 0.8660254037844387076, 1.000000000000000000, 0.8660254037844387076, 1.000000000000000000, 0.8660254037844387076, 1.000000000000000000, 0.8660254037844387076, 1.000000000000000000, 0.8660254037844387076, 1.000000000000000000, 0.8660254037844387076, 1.000000000000000000, 0.8660254037844387076, 1.000000000000000000, 0.8660254037844387076, 1.000000000000000000, 0.8660254037844387076, 1.000000000000000000, 0.8660254037844387076, 1.000000000000000000, 0.8660254037844387076, 1.000000000000000000, 0.8660254037844387076, 1.000000000000000000, 0.8660254037844387076, 1.000000000000000000, 0.8660254037844387076, 1.000000000000000000, 0.8660254037844387076, 1.000000000000000000, 0.8660254037844387076, 1.000000000000000000, 0.8660254037844387076, 1.000000000000000000, 0.8660254037844387076, 1.000000000000000000, 0.8660254037844387076, 1.000000000000000000, 0.8660254037844387076, 1.000000000000000000, 0.8660254037844387076, 1.000000000000000000, 0.8660254037844387076, 1.000000000000000000, 0.8660254037844387076, 1.000000000000000000, 0.8660254037844387076, 1.000000000000000000, 0.8660254037844387076, 1.000000000000000000, 0.8660254037844387076, 1.000000000000000000, 0.8660254037844387076, 1.000000000000000000, 0.8660254037844387076, 1.000000000000000000, 0.8660254037844387076, 1.000000000000000000, 0.8660254037844387076, 1.000000000000000000, 0.8660254037844387076, 1.000000000000000000, 0.8660254037844387076, 1.000000000000000000, 0.8660254037844387076, 1.000000000000000000, 0.8660254037844387076, 1.000000000000000000, 0.8660254037844387076, 1.000000000000000000, 0.8660254037844387076, 1.000000000000000000, 0.8660254037844387076, 1.000000000000000000, 0.8660254037844387076, 1.000000000000000000, 0.8660254037844387076, 1.000000000000000000, 0.8660254037844387076, 1.000000000000000000, 0.8660254037844387076, 1.000000000000000000, 0.8660254037844387076, 1.000000000000000000, 0.8660254037844387076, 1.000000000000000000, 0.8660254037844387076, 1.000000000000000000, 0.8660254037844387076, 1.000000000000000000, 0.8660254037844387076, 1.000000000000000000, 0.8660254037844387076, 1.000000000000000000, 0.8660254037844387076, 1.000000000000000000, 0.8660254037844387076, 1.000000000000000000, 0.8660254037844387076, 1.000000000000000000, 0.8660254037844387076, 1.000000000000000000, 0.8660254037844387076, 1.000000000000000000, 0.8660254037844387076, 1.000000000000000000, 0.8660254037844387076, 1.000000000000000000, 0.8660254037844387076, 1.000000000000000000, 0.8660254037844387076, 1.000000000000000000, 0.8660254037844387076, 1.000000000000000000, 0.8660254037844387076, 1.000000000000000000, 0.8660254037844387076, 1.000000000000000000, 0.8660254037844387076, 1.000000000000000000, 0.8660254037844387076, 1.000000000000000000, 0.8660254037844387076, 1.000000000000000000, 0.8660254037844387076, 1.000000000000000000, 0.8660254037844387076, 1.000000000000000000, 0.8660254037844387076, 1.000000000000000000, 0.8660254037844387076, 1.000000000000000000, 0.8660254037844387076, 1.000000000000000000, 0.8660254037844387076, 1.000000000000000000, 0.8660254037844387076, 1.000000000000000000, 0.8660254037844387076, 1.000000000000000000, 0.8660254037844387076, 1.000000000000000000, 0.8660254037844387076, 1.000000000000000000, 0.8660254037844387076, 1.000000000000000000, 0.8660254037844387076, 1.000000000000000000, 0.8660254037844387076, 1.000000000000000000, 0.8660254037844387076, 1.000000000000000000, 0.8660254037844387076, 1.000000000000000000, 0.8660254037844387076, 1.000000000000000000, 0.8660254037844387076, 1.000000000000000000, 0.8660254037844387076, 1.000000000000000000, 0.8660254037844387076, 1.000000000000000000, 0.8660254037844387076, 1.000000000000000000, 0.8660254037844387076, 1.000000000000000000, 0.8660254037844387076, 1.000000000000000000, 0.8660254037844387076, 1.000000000000000000, 0.8660254037844387076, 1.000000000000000000, 0.8660254037844387076, 1.000000000000000000, 0.8660254037844387076, 1.000000000000000000, 0.8660254037844387076, 1.000000000000000000, 0.8660254037844387076, 1.000000000000000000, 0.8660254037844387076, 1.000000000000000000, 0.8660254037844387076, 1.000000000000000000, 0.8660254037844387076, 1.000000000000000000, 0.8660254037844387076, 1.000000000000000000, 0.8660254037844387076, 1.000000000000000000, 0.8660254037844387076, 1.000000000000000000, 0.8660254037844387076, 1.000000000000000000, 0.8660254037844387076, 1.000000000000000000, 0.8660254037844387076, 1.000000000000000000, 0.8660254037844387076, 1.000000000000000000, 0.9024573129378088421, 0.9469501470576167090) ) ) 
 REPRESENTATION_ITEM ( '' )  SURFACE ( )  );
#61086 = VECTOR ( 'NONE', #44514, 1000.000000000000000 ) ;
#61087 = CARTESIAN_POINT ( 'NONE',  ( 97.30629616937498838, 90.00000000000002842, 80.59406250086715318 ) ) ;
#61088 = AXIS2_PLACEMENT_3D ( 'NONE', #63690, #64790, #13272 ) ;
#61089 = VECTOR ( 'NONE', #12349, 1000.000000000000000 ) ;
#61090 = CARTESIAN_POINT ( 'NONE',  ( -94.99999999999997158, -207.3369185715606307, 82.65781250086715204 ) ) ;
#61091 = DIRECTION ( 'NONE',  ( 1.000000000000000000, 0.000000000000000000, -0.000000000000000000 ) ) ;
#61092 = ORIENTED_EDGE ( 'NONE', *, *, #24514, .F. ) ;
#61093 = CARTESIAN_POINT ( 'NONE',  ( -94.99999999999997158, -213.0599564267049857, 81.26874999999999716 ) ) ;
#61094 = CARTESIAN_POINT ( 'NONE',  ( -92.34999999999999432, -208.4700217866474645, 78.30541666666668732 ) ) ;
#61095 = DIRECTION ( 'NONE',  ( 0.000000000000000000, 0.000000000000000000, 1.000000000000000000 ) ) ;
#61096 = VECTOR ( 'NONE', #19545, 1000.000000000000000 ) ;
#61097 = VECTOR ( 'NONE', #11697, 1000.000000000000000 ) ;
#61098 = ADVANCED_FACE ( 'NONE', ( #34608 ), #69925, .T. ) ;
#61099 = CARTESIAN_POINT ( 'NONE',  ( -93.84685191531254134, 91.99731107132950569, 76.88989583420048746 ) ) ;
#61100 = CARTESIAN_POINT ( 'NONE',  ( 93.84685191531251292, -211.9973110713294489, 84.66864583420047552 ) ) ;
#61101 = ORIENTED_EDGE ( 'NONE', *, *, #28341, .F. ) ;
#61102 = EDGE_CURVE ( 'NONE', #40399, #40236, #42789, .T. ) ;
#61103 = CARTESIAN_POINT ( 'NONE',  ( 11.99999999999999822, 0.000000000000000000, 0.000000000000000000 ) ) ;
#61104 = ORIENTED_EDGE ( 'NONE', *, *, #29756, .F. ) ;
#61105 = DIRECTION ( 'NONE',  ( -1.000000000000000000, -0.000000000000000000, -0.000000000000000000 ) ) ;
#61106 = ORIENTED_EDGE ( 'NONE', *, *, #66380, .T. ) ;
#61107 = VECTOR ( 'NONE', #17521, 1000.000000000000227 ) ;
#61108 = ADVANCED_FACE ( 'NONE', ( #40632 ), #12781, .T. ) ;
#61109 = AXIS2_PLACEMENT_3D ( 'NONE', #8252, #31177, #47009 ) ;
#61110 = EDGE_CURVE ( 'NONE', #42810, #30067, #55515, .T. ) ;
#61111 = LINE ( 'NONE', #42706, #72946 ) ;
#61112 = VECTOR ( 'NONE', #47058, 1000.000000000000000 ) ;
#61113 = CIRCLE ( 'NONE', #26265, 82.00000000000000000 ) ;
#61114 = ORIENTED_EDGE ( 'NONE', *, *, #36891, .T. ) ;
#61115 = ORIENTED_EDGE ( 'NONE', *, *, #1604, .F. ) ;
#61116 = CIRCLE ( 'NONE', #43158, 31.99999999999999645 ) ;
#61117 = AXIS2_PLACEMENT_3D ( 'NONE', #37707, #8756, #26030 ) ;
#61118 = CARTESIAN_POINT ( 'NONE',  ( 96.15314808468748708, -208.0026889286704943, 78.15989583420049769 ) ) ;
#61119 = CYLINDRICAL_SURFACE ( 'NONE', #21275, 16.00000000000000000 ) ;
#61120 = CARTESIAN_POINT ( 'NONE',  ( -92.35000000000003695, 90.00000000000004263, 90.00000000000000000 ) ) ;
#61121 = CIRCLE ( 'NONE', #43098, 11.59999999999999787 ) ;
#61122 = CARTESIAN_POINT ( 'NONE',  ( 0.000000000000000000, 39.78640506895604290, 66.50666863322015843 ) ) ;
#61123 = CARTESIAN_POINT ( 'NONE',  ( 97.30629616937498838, 91.33154071421968467, 87.63197916753382799 ) ) ;
#61124 = ADVANCED_FACE ( 'NONE', ( #34242 ), #28225, .F. ) ;
#61125 = CARTESIAN_POINT ( 'NONE',  ( 11.99999999999999822, -12.93880638057369659, 76.41127070299266677 ) ) ;
#61126 = CARTESIAN_POINT ( 'NONE',  ( 92.35000000000000853, -209.9999999999999716, 81.74500000000000455 ) ) ;
#61127 = ORIENTED_EDGE ( 'NONE', *, *, #35924, .T. ) ;
#61128 = ORIENTED_EDGE ( 'NONE', *, *, #6940, .T. ) ;
#61129 = ORIENTED_EDGE ( 'NONE', *, *, #36379, .T. ) ;
#61130 = ORIENTED_EDGE ( 'NONE', *, *, #10256, .T. ) ;
#61131 = SURFACE_STYLE_USAGE ( .BOTH. , #62627 ) ;
#61132 = LINE ( 'NONE', #62630, #66738 ) ;
#61133 = DIRECTION ( 'NONE',  ( -0.000000000000000000, -0.000000000000000000, 1.000000000000000000 ) ) ;
#61134 = CARTESIAN_POINT ( 'NONE',  ( -10.00000000000000000, 0.000000000000000000, 0.000000000000000000 ) ) ;
#61135 = DIRECTION ( 'NONE',  ( 0.000000000000000000, -0.07845909572783056618, -0.9969173337331290741 ) ) ;
#61136 = DIRECTION ( 'NONE',  ( -1.000000000000000000, 0.000000000000000000, -0.000000000000000000 ) ) ;
#61137 = ORIENTED_EDGE ( 'NONE', *, *, #4426, .F. ) ;
#61138 = AXIS2_PLACEMENT_3D ( 'NONE', #43317, #48194, #53828 ) ;
#61139 = CARTESIAN_POINT ( 'NONE',  ( -97.64999999999996305, -209.9999999999999716, 86.26937500173430351 ) ) ;
#61141 = ORIENTED_EDGE ( 'NONE', *, *, #69258, .T. ) ;
#61140 = EDGE_CURVE ( 'NONE', #45315, #57888, #13947, .T. ) ;
#61142 = CARTESIAN_POINT ( 'NONE',  ( -3.000000000000000000, -1.278221433540502217, 26.51162292216071847 ) ) ;
#61143 = ORIENTED_EDGE ( 'NONE', *, *, #32418, .F. ) ;
#61144 = CARTESIAN_POINT ( 'NONE',  ( -93.67500000000003979, 92.29496732002878900, 81.61270833506763722 ) ) ;
#61145 = VECTOR ( 'NONE', #41005, 1000.000000000000000 ) ;
#61147 = EDGE_CURVE ( 'NONE', #73431, #17494, #58657, .T. ) ;
#61146 = ORIENTED_EDGE ( 'NONE', *, *, #70153, .F. ) ;
#61148 = CARTESIAN_POINT ( 'NONE',  ( 93.84685191531248449, 88.00268892867053694, 82.28739583420048120 ) ) ;
#61149 = DIRECTION ( 'NONE',  ( 0.000000000000000000, 0.000000000000000000, 1.000000000000000000 ) ) ;
#61150 = VECTOR ( 'NONE', #17469, 1000.000000000000114 ) ;
#61151 = CARTESIAN_POINT ( 'NONE',  ( 10.00000000000000000, -75.16055320797016748, -18.89407956138335365 ) ) ;
#61152 = VECTOR ( 'NONE', #55911, 1000.000000000000000 ) ;
#61153 = LINE ( 'NONE', #55126, #27810 ) ;
#61154 = CARTESIAN_POINT ( 'NONE',  ( 96.32499999999998863, 87.70503267997126784, 88.94166666666666288 ) ) ;
#61155 = CIRCLE ( 'NONE', #68507, 42.00000000000000000 ) ;
#61156 = LINE ( 'NONE', #2924, #49272 ) ;
#61157 = ORIENTED_EDGE ( 'NONE', *, *, #4803, .T. ) ;
#61158 = FACE_OUTER_BOUND ( 'NONE', #20341, .T. ) ;
#61159 = DIRECTION ( 'NONE',  ( -1.000000000000000000, -0.000000000000000000, 0.000000000000000000 ) ) ;
#61160 = ORIENTED_EDGE ( 'NONE', *, *, #61748, .F. ) ;
#61161 = AXIS2_PLACEMENT_3D ( 'NONE', #42776, #47309, #70212 ) ;
#61162 = EDGE_LOOP ( 'NONE', ( #64284, #35460, #48903, #41707 ) ) ;
#61163 = AXIS2_PLACEMENT_3D ( 'NONE', #14579, #42058, #67948 ) ;
#61164 = DIRECTION ( 'NONE',  ( 0.000000000000000000, -0.6691306063588654540, -0.7431448254773878048 ) ) ;
#61165 = CARTESIAN_POINT ( 'NONE',  ( 92.34999999999999432, 90.00000000000002842, 90.00000000000000000 ) ) ;
#61166 = LINE ( 'NONE', #9653, #61725 ) ;
#61167 = CARTESIAN_POINT ( 'NONE',  ( -92.69370383062498320, -209.9999999999999716, 84.40406250086715545 ) ) ;
#61168 = ORIENTED_EDGE ( 'NONE', *, *, #63875, .F. ) ;
#61169 = CARTESIAN_POINT ( 'NONE',  ( 97.64999999999999147, -209.9999999999999716, 81.42749999999999488 ) ) ;
#61170 = ORIENTED_EDGE ( 'NONE', *, *, #13581, .F. ) ;
#61171 = CIRCLE ( 'NONE', #23978, 82.00000000000000000 ) ;
#61172 = CARTESIAN_POINT ( 'NONE',  ( 0.000000000000000000, -13.04903810567647682, -19.60159698893442126 ) ) ;
#61173 = VECTOR ( 'NONE', #19696, 1000.000000000000114 ) ;
#61174 = FACE_BOUND ( 'NONE', #42074, .T. ) ;
#61175 = CARTESIAN_POINT ( 'NONE',  ( 92.35000000046504454, -210.0000309987310061, 83.09538598081256566 ) ) ;
#61176 = CARTESIAN_POINT ( 'NONE',  ( 96.15314808468748708, 91.99731107132950569, 76.73114583420047552 ) ) ;
#61177 = CARTESIAN_POINT ( 'NONE',  ( 10.00000000000000000, 37.16516213103285082, -4.992566952384588141 ) ) ;
#61178 = CARTESIAN_POINT ( 'NONE',  ( 93.67499999999998295, 92.29496732002878900, 86.79854166840097207 ) ) ;
#61179 = CARTESIAN_POINT ( 'NONE',  ( 5.000000000000002665, 80.55351364060611274, -15.33399622253396544 ) ) ;
#61180 = DIRECTION ( 'NONE',  ( -1.000000000000000000, -0.000000000000000000, -0.000000000000000000 ) ) ;
#61181 = CYLINDRICAL_SURFACE ( 'NONE', #49617, 77.49899999999999523 ) ;
#61182 = DIRECTION ( 'NONE',  ( 0.000000000000000000, 0.000000000000000000, 1.000000000000000000 ) ) ;
#61183 = LINE ( 'NONE', #67187, #63644 ) ;
#61184 = CARTESIAN_POINT ( 'NONE',  ( 100.0010000000000900, 64.99999999999997158, -290.0000000000000568 ) ) ;
#61185 = ORIENTED_EDGE ( 'NONE', *, *, #57836, .T. ) ;
#61186 = CARTESIAN_POINT ( 'NONE',  ( -96.15314808468751551, 88.00268892867056536, 83.39864583420047950 ) ) ;
#61187 = LINE ( 'NONE', #43542, #61152 ) ;
#61188 = EDGE_CURVE ( 'NONE', #1192, #57624, #62017, .T. ) ;
#61189 = LINE ( 'NONE', #15312, #59463 ) ;
#61190 = EDGE_CURVE ( 'NONE', #50412, #38492, #71594, .T. ) ;
#61191 = ORIENTED_EDGE ( 'NONE', *, *, #15148, .T. ) ;
#61193 = CARTESIAN_POINT ( 'NONE',  ( -97.64999999993850111, -209.9999881782113675, 76.10900611559516449 ) ) ;
#61192 = CIRCLE ( 'NONE', #3583, 82.00000000000000000 ) ;
#61194 = DIRECTION ( 'NONE',  ( -1.000000000000000000, -0.000000000000000000, 0.000000000000000000 ) ) ;
#61195 = DIRECTION ( 'NONE',  ( 0.000000000000000000, 0.9969173337331281859, -0.07845909572784182107 ) ) ;
#61196 = CIRCLE ( 'NONE', #10803, 2.699999999999999734 ) ;
#61197 = EDGE_CURVE ( 'NONE', #65205, #26530, #28397, .T. ) ;
#61198 = AXIS2_PLACEMENT_3D ( 'NONE', #4577, #26002, #38402 ) ;
#61199 = CARTESIAN_POINT ( 'NONE',  ( 97.64999999999999147, 90.00000000000002842, 83.41187500173430180 ) ) ;
#61200 = CARTESIAN_POINT ( 'NONE',  ( 97.30629616937498838, -208.6684592857803011, 80.01197916753380923 ) ) ;
#61201 = CIRCLE ( 'NONE', #38393, 42.00000000000000000 ) ;
#61202 = VERTEX_POINT ( 'NONE', #23345 ) ;
#61203 = ORIENTED_EDGE ( 'NONE', *, *, #44547, .T. ) ;
#61204 = CYLINDRICAL_SURFACE ( 'NONE', #33244, 2.649999999999999467 ) ;
#61205 = ADVANCED_FACE ( 'NONE', ( #34991 ), #64670, .T. ) ;
#61206 = CARTESIAN_POINT ( 'NONE',  ( 10.00000000000000000, 37.22597642581158084, 10.79786254984347593 ) ) ;
#61207 = CYLINDRICAL_SURFACE ( 'NONE', #18458, 31.99999999999998579 ) ;
#61208 = CARTESIAN_POINT ( 'NONE',  ( 6.000000000000000000, 10.30890764327501152, -81.34940948281325745 ) ) ;
#61209 = EDGE_CURVE ( 'NONE', #15320, #36881, #15201, .T. ) ;
#61210 = DIRECTION ( 'NONE',  ( 0.000000000000000000, -0.8090169943749497827, -0.5877852522924698064 ) ) ;
#61211 = EDGE_CURVE ( 'NONE', #21621, #4375, #59774, .T. ) ;
#61212 = CARTESIAN_POINT ( 'NONE',  ( 95.00000000000000000, -212.6630814284392557, 77.26031250086714408 ) ) ;
#61213 = AXIS2_PLACEMENT_3D ( 'NONE', #37119, #55138, #26929 ) ;
#61214 = VERTEX_POINT ( 'NONE', #31548 ) ;
#61215 = CARTESIAN_POINT ( 'NONE',  ( 10.00000000000000000, 15.33399622253481276, 80.55351364060595643 ) ) ;
#61216 = ORIENTED_EDGE ( 'NONE', *, *, #12961, .F. ) ;
#61217 = ADVANCED_FACE ( 'NONE', ( #66163 ), #31983, .T. ) ;
#61218 = CIRCLE ( 'NONE', #27619, 77.49899999999999523 ) ;
#61219 = ORIENTED_EDGE ( 'NONE', *, *, #971, .F. ) ;
#61220 = DIRECTION ( 'NONE',  ( 0.8774505977381971134, 0.4796670183876317051, -0.000000000000000000 ) ) ;
#61221 = VECTOR ( 'NONE', #23780, 1000.000000000000000 ) ;
#61222 = AXIS2_PLACEMENT_3D ( 'NONE', #14454, #71585, #55042 ) ;
#61223 = FILL_AREA_STYLE_COLOUR ( '', #3888 ) ;
#61224 = CARTESIAN_POINT ( 'NONE',  ( -92.35000000035638834, 89.99995654222792041, 89.12687334326074051 ) ) ;
#61225 = VECTOR ( 'NONE', #73688, 1000.000000000000114 ) ;
#61226 = ORIENTED_EDGE ( 'NONE', *, *, #33427, .F. ) ;
#61227 = LINE ( 'NONE', #8968, #29351 ) ;
#61228 = CARTESIAN_POINT ( 'NONE',  ( 92.35000000000002274, -208.4700217866474645, 81.77145833506763495 ) ) ;
#61230 = AXIS2_PLACEMENT_3D ( 'NONE', #38635, #31493, #48787 ) ;
#61229 = CARTESIAN_POINT ( 'NONE',  ( 94.99999999999998579, 93.05995642670504253, 82.85625000000000284 ) ) ;
#61231 = ORIENTED_EDGE ( 'NONE', *, *, #20175, .F. ) ;
#61232 = DIRECTION ( 'NONE',  ( -1.000000000000000000, -0.000000000000000000, -0.000000000000000000 ) ) ;
#61233 = ORIENTED_EDGE ( 'NONE', *, *, #69082, .T. ) ;
#61234 = EDGE_CURVE ( 'NONE', #44223, #9893, #7158, .T. ) ;
#61235 = CARTESIAN_POINT ( 'NONE',  ( 94.99999999999998579, 93.05995642670504253, 81.03062500173430749 ) ) ;
#61236 = ORIENTED_EDGE ( 'NONE', *, *, #32765, .T. ) ;
#61237 = CARTESIAN_POINT ( 'NONE',  ( 97.64999999999999147, 89.99999997442942856, 84.04687500080852658 ) ) ;
#61238 = CARTESIAN_POINT ( 'NONE',  ( -97.30629616937501680, 91.33154071421968467, 83.39864583420049371 ) ) ;
#61239 = CARTESIAN_POINT ( 'NONE',  ( 92.69370383062498320, 90.00000000000002842, 83.29281250086714294 ) ) ;
#61240 = ORIENTED_EDGE ( 'NONE', *, *, #24107, .T. ) ;
#61241 = DIRECTION ( 'NONE',  ( -1.000000000000000000, -0.000000000000000000, -0.000000000000000000 ) ) ;
#61242 = DIRECTION ( 'NONE',  ( -0.000000000000000000, -0.000000000000000000, 1.000000000000000000 ) ) ;
#61243 = ORIENTED_EDGE ( 'NONE', *, *, #11230, .F. ) ;
#61244 = FACE_OUTER_BOUND ( 'NONE', #50202, .T. ) ;
#61245 = VERTEX_POINT ( 'NONE', #42118 ) ;
#61246 = VERTEX_POINT ( 'NONE', #70286 ) ;
#61247 = DIRECTION ( 'NONE',  ( -1.000000000000000000, -0.000000000000000000, -0.000000000000000000 ) ) ;
#61248 = ORIENTED_EDGE ( 'NONE', *, *, #7576, .T. ) ;
#61249 = DIRECTION ( 'NONE',  ( -0.000000000000000000, -0.000000000000000000, 1.000000000000000000 ) ) ;
#61250 = CARTESIAN_POINT ( 'NONE',  ( 97.64999999999997726, 91.52997821335252127, 89.17979166840096639 ) ) ;
#61251 = VERTEX_POINT ( 'NONE', #13885 ) ;
#61252 = CARTESIAN_POINT ( 'NONE',  ( 0.000000000000000000, 0.8828120875900632436, 37.48860685352291000 ) ) ;
#61253 = CARTESIAN_POINT ( 'NONE',  ( -94.99999999999997158, -212.6630814284392557, 80.91156250086714863 ) ) ;
#61254 = ORIENTED_EDGE ( 'NONE', *, *, #61197, .F. ) ;
#61255 = VECTOR ( 'NONE', #70513, 1000.000000000000000 ) ;
#61256 = CARTESIAN_POINT ( 'NONE',  ( 0.000000000000000000, -21.53537804866103045, 30.80686688397002371 ) ) ;
#61257 = CARTESIAN_POINT ( 'NONE',  ( 7.103376864691351012E-17, -120.0000000000000000, -64.00000000000000000 ) ) ;
#61258 = CARTESIAN_POINT ( 'NONE',  ( 3.000000000000000000, 0.000000000000000000, 2.541999999999999815 ) ) ;
#61259 = CARTESIAN_POINT ( 'NONE',  ( -92.35000000035631729, -210.0000434577671911, 89.12687334326093946 ) ) ;
#61260 = AXIS2_PLACEMENT_3D ( 'NONE', #6171, #33042, #38702 ) ;
#61261 = LINE ( 'NONE', #44717, #54660 ) ;
#61262 = CARTESIAN_POINT ( 'NONE',  ( -92.35000000000000853, 88.47002178664756400, 89.62958333333334338 ) ) ;
#61263 = AXIS2_PLACEMENT_3D ( 'NONE', #33220, #27200, #50135 ) ;
#61264 = FACE_OUTER_BOUND ( 'NONE', #35845, .T. ) ;
#61265 = DIRECTION ( 'NONE',  ( -1.000000000000000000, -0.000000000000000000, -0.000000000000000000 ) ) ;
#61266 = CARTESIAN_POINT ( 'NONE',  ( -96.32500000000001705, 87.70503267997129626, 86.93083333333332519 ) ) ;
#61267 = CARTESIAN_POINT ( 'NONE',  ( -18.12185313557660038, -104.9634299478706794, 2.500000000000000000 ) ) ;
#61268 = DIRECTION ( 'NONE',  ( -1.000000000000000000, 0.000000000000000000, 0.000000000000000000 ) ) ;
#61269 = CARTESIAN_POINT ( 'NONE',  ( 92.34999999999996589, 88.47002178664753558, 77.35291666666665833 ) ) ;
#61270 = CARTESIAN_POINT ( 'NONE',  ( -95.00000000000002842, 90.00000000000004263, 90.00000000000000000 ) ) ;
#61271 = CARTESIAN_POINT ( 'NONE',  ( 93.67499999999998295, 92.29496732002878900, 76.00354166840097037 ) ) ;
#61272 = EDGE_CURVE ( 'NONE', #18300, #51981, #66829, .T. ) ;
#61273 = AXIS2_PLACEMENT_3D ( 'NONE', #62476, #63949, #29700 ) ;
#61274 = DIRECTION ( 'NONE',  ( 0.000000000000000000, -0.4067366430758009299, -0.9135454576426005335 ) ) ;
#61275 = AXIS2_PLACEMENT_3D ( 'NONE', #43678, #38018, #38762 ) ;
#61276 = DIRECTION ( 'NONE',  ( -1.000000000000000000, -0.000000000000000000, 0.000000000000000000 ) ) ;
#61277 = EDGE_CURVE ( 'NONE', #4157, #9311, #24444, .T. ) ;
#61278 = CARTESIAN_POINT ( 'NONE',  ( -96.32499999999996021, -212.2949673200287179, 83.12083333333332291 ) ) ;
#61279 = ADVANCED_FACE ( 'NONE', ( #18789 ), #53388, .F. ) ;
#61280 = EDGE_CURVE ( 'NONE', #61428, #71727, #41728, .T. ) ;
#61281 = AXIS2_PLACEMENT_3D ( 'NONE', #43370, #66291, #38447 ) ;
#61282 = DIRECTION ( 'NONE',  ( 0.000000000000000000, 0.000000000000000000, 1.000000000000000000 ) ) ;
#61283 = EDGE_CURVE ( 'NONE', #16098, #28286, #72866, .T. ) ;
#61284 = LINE ( 'NONE', #3782, #21492 ) ;
#61285 = CARTESIAN_POINT ( 'NONE',  ( -23.50000000000271427, -119.9999999999998153, -48.99999999999936051 ) ) ;
#61286 =( NAMED_UNIT ( * ) PLANE_ANGLE_UNIT ( ) SI_UNIT ( $, .RADIAN. ) );
#61287 = DIRECTION ( 'NONE',  ( 0.000000000000000000, -0.5224985647159379187, -0.8526401643540989506 ) ) ;
#61288 = EDGE_CURVE ( 'NONE', #59443, #38652, #42847, .T. ) ;
#61289 = AXIS2_PLACEMENT_3D ( 'NONE', #7827, #24381, #36761 ) ;
#61290 = CARTESIAN_POINT ( 'NONE',  ( 92.69370383062501162, -208.6684592857803011, 89.74864583420048803 ) ) ;
#61291 = VERTEX_POINT ( 'NONE', #36093 ) ;
#61292 = ORIENTED_EDGE ( 'NONE', *, *, #24304, .T. ) ;
#61293 = CARTESIAN_POINT ( 'NONE',  ( 0.000000000000000000, -120.0000000000000000, 2.500000000000000000 ) ) ;
#61294 = CYLINDRICAL_SURFACE ( 'NONE', #16353, 77.49899999999999523 ) ;
#61295 = ORIENTED_EDGE ( 'NONE', *, *, #34105, .F. ) ;
#61296 = CARTESIAN_POINT ( 'NONE',  ( 96.15314808468748708, -208.0026889286704943, 81.17614583420048291 ) ) ;
#61297 = CARTESIAN_POINT ( 'NONE',  ( 97.30629616937498838, -211.3315407142195852, 84.98614583420047097 ) ) ;
#61299 = ORIENTED_EDGE ( 'NONE', *, *, #32759, .T. ) ;
#61298 = ADVANCED_FACE ( 'NONE', ( #59040 ), #71765, .T. ) ;
#61300 = CARTESIAN_POINT ( 'NONE',  ( 93.84685191531249870, -208.0026889286704943, 87.79072916753381151 ) ) ;
#61301 = AXIS2_PLACEMENT_3D ( 'NONE', #28152, #23631, #57853 ) ;
#61302 = VERTEX_POINT ( 'NONE', #43239 ) ;
#61303 = CARTESIAN_POINT ( 'NONE',  ( 0.000000000000000000, 28.89263327155746097, 71.91182617369197771 ) ) ;
#61304 = EDGE_LOOP ( 'NONE', ( #56047, #46691 ) ) ;
#61305 = AXIS2_PLACEMENT_3D ( 'NONE', #6619, #53224, #64882 ) ;
#61306 = EDGE_CURVE ( 'NONE', #68814, #61974, #36825, .T. ) ;
#61307 = ADVANCED_FACE ( 'NONE', ( #13529 ), #71399, .T. ) ;
#61308 = CARTESIAN_POINT ( 'NONE',  ( -92.69370383062502583, 88.66845928578038638, 76.73114583420048973 ) ) ;
#61309 = ORIENTED_EDGE ( 'NONE', *, *, #23084, .T. ) ;
#61310 = ORIENTED_EDGE ( 'NONE', *, *, #53646, .T. ) ;
#61311 = VECTOR ( 'NONE', #51338, 1000.000000000000000 ) ;
#61312 = CARTESIAN_POINT ( 'NONE',  ( 0.000000000000000000, -8.966570791700167575, -81.50828551894237251 ) ) ;
#61313 = EDGE_LOOP ( 'NONE', ( #20172, #61498, #41518, #16494 ) ) ;
#61314 = CARTESIAN_POINT ( 'NONE',  ( 0.000000000000000000, 12.24744871391589207, -2.500000000000000000 ) ) ;
#61315 = DIRECTION ( 'NONE',  ( 0.000000000000000000, -0.8526401643540860720, -0.5224985647159589019 ) ) ;
#61316 = EDGE_LOOP ( 'NONE', ( #15146, #2601, #21444, #6701 ) ) ;
#61317 = DIRECTION ( 'NONE',  ( 1.000000000000000000, 0.000000000000000000, 0.000000000000000000 ) ) ;
#61318 = ADVANCED_FACE ( 'NONE', ( #59401 ), #7889, .F. ) ;
#61319 = ORIENTED_EDGE ( 'NONE', *, *, #10003, .F. ) ;
#61320 =( BOUNDED_CURVE ( )  B_SPLINE_CURVE ( 2, ( #29798, #70384, #18888, #47120, #11763, #13260, #52370 ),
 .UNSPECIFIED., .F., .F. ) 
 B_SPLINE_CURVE_WITH_KNOTS ( ( 3, 2, 2, 3 ),
 ( 0.7291666666666665186, 0.7361111111111109384, 0.7430555555555553582, 0.7499999999999996669 ),
 .UNSPECIFIED. ) 
 CURVE ( )  GEOMETRIC_REPRESENTATION_ITEM ( )  RATIONAL_B_SPLINE_CURVE ( ( 1.000000000000002220, 0.8660254037844365982, 1.000000000000000000, 0.8660254037844387076, 1.000000000000000000, 0.8660254037844451469, 0.9999999999999935607 ) ) 
 REPRESENTATION_ITEM ( '' )  );
#61321 = CARTESIAN_POINT ( 'NONE',  ( 11.99999999999999822, 26.02418014898310261, 70.52718814184268581 ) ) ;
#61322 = ORIENTED_EDGE ( 'NONE', *, *, #55064, .T. ) ;
#61323 = AXIS2_PLACEMENT_3D ( 'NONE', #40637, #39530, #18075 ) ;
#61324 = VERTEX_POINT ( 'NONE', #48115 ) ;
#61325 = ORIENTED_EDGE ( 'NONE', *, *, #48225, .F. ) ;
#61326 = CARTESIAN_POINT ( 'NONE',  ( 0.000000000000000000, -51.29473840253269401, 63.97538442413407012 ) ) ;
#61327 = CIRCLE ( 'NONE', #68584, 37.49900000000000233 ) ;
#61328 = CONTEXT_DEPENDENT_SHAPE_REPRESENTATION ( #28748, #11607 ) ;
#61329 = FACE_OUTER_BOUND ( 'NONE', #44847, .T. ) ;
#61330 = ORIENTED_EDGE ( 'NONE', *, *, #41126, .F. ) ;
#61331 = CIRCLE ( 'NONE', #140, 13.10000000000023590 ) ;
#61332 = ORIENTED_EDGE ( 'NONE', *, *, #36221, .T. ) ;
#61333 = ORIENTED_EDGE ( 'NONE', *, *, #34550, .T. ) ;
#61334 = DIRECTION ( 'NONE',  ( 0.000000000000000000, 0.000000000000000000, 1.000000000000000000 ) ) ;
#61335 = AXIS2_PLACEMENT_3D ( 'NONE', #52247, #789, #29666 ) ;
#61336 = DIRECTION ( 'NONE',  ( -1.000000000000000000, 3.061616997868382648E-16, 0.000000000000000000 ) ) ;
#61337 = CARTESIAN_POINT ( 'NONE',  ( -93.84685191531252713, 88.00268892867056536, 75.40822916753381833 ) ) ;
#61338 = ORIENTED_EDGE ( 'NONE', *, *, #40380, .F. ) ;
#61339 = CARTESIAN_POINT ( 'NONE',  ( 92.69370383062498320, 88.66845928578037217, 78.90072916753381094 ) ) ;
#61340 = ORIENTED_EDGE ( 'NONE', *, *, #23372, .T. ) ;
#61341 = CARTESIAN_POINT ( 'NONE',  ( 12.00000000000000000, -25.60904388321915803, 6.976881207771517879 ) ) ;
#61342 = CARTESIAN_POINT ( 'NONE',  ( 12.00000000000000000, -19.89357724624986545, 12.59942793731086219 ) ) ;
#61343 = ORIENTED_EDGE ( 'NONE', *, *, #26971, .F. ) ;
#61344 = CARTESIAN_POINT ( 'NONE',  ( 10.00000000000000000, -27.05870788708250885, 26.08949754953014022 ) ) ;
#61345 = DIRECTION ( 'NONE',  ( -1.000000000000000000, -0.000000000000000000, 0.000000000000000000 ) ) ;
#61346 = DIRECTION ( 'NONE',  ( 0.000000000000000000, 0.000000000000000000, 1.000000000000000000 ) ) ;
#61347 = CARTESIAN_POINT ( 'NONE',  ( -94.99999999999997158, -207.3369185715606307, 81.22906250086714408 ) ) ;
#61348 = LINE ( 'NONE', #10565, #31412 ) ;
#61349 = CYLINDRICAL_SURFACE ( 'NONE', #64336, 42.00000000000000000 ) ;
#61350 = DIRECTION ( 'NONE',  ( 2.603472992746261562E-14, 2.546204323184492723E-14, -1.000000000000000000 ) ) ;
#61351 = ORIENTED_EDGE ( 'NONE', *, *, #7544, .T. ) ;
#61352 = EDGE_LOOP ( 'NONE', ( #47796, #46353, #31091, #58836, #508, #73289, #71506, #42046, #4263, #20807, #61771, #35159, #34040, #15826, #59940, #42537, #40860, #38113, #55288, #44300, #70349, #48275, #56295, #20242, #41057, #39508, #60238, #29469, #40592, #32189, #6762, #8115, #17679, #31411, #51551, #39111, #18210, #52536, #42055, #35571, #46422, #56418, #54910, #3372, #25700, #16672, #35848, #59446, #13970, #56605, #17362, #13659 ) ) ;
#61353 = CARTESIAN_POINT ( 'NONE',  ( 0.000000000000000000, -33.71516098798792171, 74.74816331893418919 ) ) ;
#61354 = DIRECTION ( 'NONE',  ( -1.000000000000000000, -0.000000000000000000, -0.000000000000000000 ) ) ;
#61355 = DIRECTION ( 'NONE',  ( 1.000000000000000000, -0.000000000000000000, -0.000000000000000000 ) ) ;
#61356 = CARTESIAN_POINT ( 'NONE',  ( -95.00000000000002842, 87.33691857156074434, 80.91156250086714863 ) ) ;
#61357 = DIRECTION ( 'NONE',  ( 0.000000000000000000, 1.000000000000000000, 3.491481338843133750E-15 ) ) ;
#61358 = CYLINDRICAL_SURFACE ( 'NONE', #49536, 16.00000000000000000 ) ;
#61359 = VERTEX_POINT ( 'NONE', #71033 ) ;
#61360 = CARTESIAN_POINT ( 'NONE',  ( 4.348517481000897078, -143.0941636721797465, 2.500000000000000000 ) ) ;
#61361 = VECTOR ( 'NONE', #16044, 1000.000000000000000 ) ;
#61362 = CIRCLE ( 'NONE', #28933, 2.541999999999999815 ) ;
#61363 = VECTOR ( 'NONE', #74199, 1000.000000000000000 ) ;
#61364 = CARTESIAN_POINT ( 'NONE',  ( 0.000000000000000000, -10.74501242461258244, -35.92658777277521409 ) ) ;
#61365 = CARTESIAN_POINT ( 'NONE',  ( 10.00000000000000000, -69.42325613327466272, 34.44570377933573724 ) ) ;
#61366 = EDGE_CURVE ( 'NONE', #54442, #25438, #59701, .T. ) ;
#61367 = CARTESIAN_POINT ( 'NONE',  ( 0.000000000000000000, -79.10210256391383155, 21.60688246758557796 ) ) ;
#61368 = CARTESIAN_POINT ( 'NONE',  ( -92.35000000053402403, -209.9999467984910382, 78.96687695417375608 ) ) ;
#61369 = CARTESIAN_POINT ( 'NONE',  ( -92.69370383062498320, -209.9999999999999716, 79.95906250086714806 ) ) ;
#61370 = ADVANCED_FACE ( 'NONE', ( #4876 ), #50703, .F. ) ;
#61371 = EDGE_CURVE ( 'NONE', #33591, #15290, #20018, .T. ) ;
#61372 = CARTESIAN_POINT ( 'NONE',  ( 97.65000000000000568, 88.47002178664752137, 76.37395833506761278 ) ) ;
#61373 = APPLICATION_CONTEXT ( 'automotive_design' ) ;
#61374 = VERTEX_POINT ( 'NONE', #9000 ) ;
#61375 = DIRECTION ( 'NONE',  ( 0.000000000000000000, 0.000000000000000000, 1.000000000000000000 ) ) ;
#61376 = DIRECTION ( 'NONE',  ( 0.000000000000000000, -0.9510565162951565288, 0.3090169943749382364 ) ) ;
#61377 = CARTESIAN_POINT ( 'NONE',  ( 0.7195005275814480017, -121.3161758966073052, -2.500000000000000000 ) ) ;
#61378 = STYLED_ITEM ( 'NONE', ( #63136 ), #12047 ) ;
#61379 = ORIENTED_EDGE ( 'NONE', *, *, #20573, .F. ) ;
#61380 = CARTESIAN_POINT ( 'NONE',  ( 0.000000000000000000, -89.50000000000000000, 2.500000000000000000 ) ) ;
#61381 = CARTESIAN_POINT ( 'NONE',  ( 10.00000000000000000, -80.55351364060578589, -15.33399622253569028 ) ) ;
#61382 = CIRCLE ( 'NONE', #20531, 13.10000000000023590 ) ;
#61383 = VECTOR ( 'NONE', #71323, 1000.000000000000000 ) ;
#61384 = CARTESIAN_POINT ( 'NONE',  ( -3.961125083139900749, -143.2122702051246677, -2.500000000000000000 ) ) ;
#61385 = EDGE_CURVE ( 'NONE', #43844, #55291, #65650, .T. ) ;
#61386 = ORIENTED_EDGE ( 'NONE', *, *, #60190, .T. ) ;
#61387 = EDGE_CURVE ( 'NONE', #19308, #4312, #21241, .T. ) ;
#61388 = DIRECTION ( 'NONE',  ( -1.000000000000000000, 0.000000000000000000, -0.000000000000000000 ) ) ;
#61389 = ORIENTED_EDGE ( 'NONE', *, *, #33113, .F. ) ;
#61390 = CARTESIAN_POINT ( 'NONE',  ( 92.35000000000000853, -209.9999999999999716, 90.00000000000000000 ) ) ;
#61391 = DIRECTION ( 'NONE',  ( -1.000000000000000000, -0.000000000000000000, -0.000000000000000000 ) ) ;
#61392 = ORIENTED_EDGE ( 'NONE', *, *, #2194, .T. ) ;
#61393 = CYLINDRICAL_SURFACE ( 'NONE', #34254, 82.00000000000000000 ) ;
#61394 = ORIENTED_EDGE ( 'NONE', *, *, #11228, .T. ) ;
#61395 = FACE_OUTER_BOUND ( 'NONE', #58302, .T. ) ;
#61396 = EDGE_CURVE ( 'NONE', #35405, #34710, #66524, .T. ) ;
#61397 = EDGE_CURVE ( 'NONE', #68902, #31369, #27776, .T. ) ;
#61398 = DIRECTION ( 'NONE',  ( 0.6516173805718078471, -0.7585478161175706058, 0.000000000000000000 ) ) ;
#61399 = VERTEX_POINT ( 'NONE', #21011 ) ;
#61400 = ORIENTED_EDGE ( 'NONE', *, *, #11520, .F. ) ;
#61401 = ORIENTED_EDGE ( 'NONE', *, *, #11691, .T. ) ;
#61402 = LINE ( 'NONE', #4266, #56380 ) ;
#61403 = ORIENTED_EDGE ( 'NONE', *, *, #64050, .F. ) ;
#61404 = EDGE_LOOP ( 'NONE', ( #57555, #43036, #19597, #51037 ) ) ;
#61405 = CARTESIAN_POINT ( 'NONE',  ( 97.30629616937498838, 90.00000000000002842, 76.78406250086715090 ) ) ;
#61406 = LINE ( 'NONE', #11369, #42021 ) ;
#61407 = CARTESIAN_POINT ( 'NONE',  ( 12.00000000000000000, 8.688484142253932063, -21.88630264137371029 ) ) ;
#61408 = ORIENTED_EDGE ( 'NONE', *, *, #28366, .T. ) ;
#61409 = VERTEX_POINT ( 'NONE', #4492 ) ;
#61410 = VECTOR ( 'NONE', #3597, 1000.000000000000000 ) ;
#61411 = AXIS2_PLACEMENT_3D ( 'NONE', #52357, #68923, #6869 ) ;
#61412 = ORIENTED_EDGE ( 'NONE', *, *, #16462, .F. ) ;
#61413 = CARTESIAN_POINT ( 'NONE',  ( 92.69370383062498320, 88.66845928578037217, 87.79072916753381151 ) ) ;
#61414 = AXIS2_PLACEMENT_3D ( 'NONE', #10873, #33798, #63495 ) ;
#61415 = VERTEX_POINT ( 'NONE', #73255 ) ;
#61416 = CARTESIAN_POINT ( 'NONE',  ( 95.00000000000000000, -212.6630814284392557, 84.08656250086713158 ) ) ;
#61417 = SHAPE_DEFINITION_REPRESENTATION ( #33814, #50888 ) ;
#61418 = CARTESIAN_POINT ( 'NONE',  ( 0.000000000000000000, 6.903761155838878061, -77.19088730480517313 ) ) ;
#61420 = CARTESIAN_POINT ( 'NONE',  ( -92.34999999999999432, -209.9999999999999716, 80.15749999999999886 ) ) ;
#61419 = AXIS2_PLACEMENT_3D ( 'NONE', #70387, #12882, #63303 ) ;
#61421 = CARTESIAN_POINT ( 'NONE',  ( 10.00000000000000000, -75.11764819372149304, 2.946379043146075905 ) ) ;
#61422 = DIRECTION ( 'NONE',  ( 1.000000000000000000, 0.000000000000000000, 0.000000000000000000 ) ) ;
#61423 = DIRECTION ( 'NONE',  ( -1.000000000000000000, -0.000000000000000000, -0.000000000000000000 ) ) ;
#61424 = DIRECTION ( 'NONE',  ( -1.000000000000000000, 3.061616997868382648E-16, 0.000000000000000000 ) ) ;
#61425 = CARTESIAN_POINT ( 'NONE',  ( -96.15314808468747287, -208.0026889286704943, 88.90197916753380980 ) ) ;
#61426 = CARTESIAN_POINT ( 'NONE',  ( -97.30629616937501680, 90.00000000000004263, 85.35656250086715602 ) ) ;
#61427 = AXIS2_PLACEMENT_3D ( 'NONE', #66058, #14532, #2188 ) ;
#61428 = VERTEX_POINT ( 'NONE', #31923 ) ;
#61430 = CARTESIAN_POINT ( 'NONE',  ( -97.30629616937501680, 90.00000000000004263, 89.64281250086713726 ) ) ;
#61429 = CARTESIAN_POINT ( 'NONE',  ( 92.69370383062498320, 91.33154071421968467, 87.04989583420048405 ) ) ;
#61431 = EDGE_LOOP ( 'NONE', ( #6303, #55482, #47929, #9964 ) ) ;
#61432 = DIRECTION ( 'NONE',  ( 0.000000000000000000, 0.000000000000000000, 1.000000000000000000 ) ) ;
#61433 = CARTESIAN_POINT ( 'NONE',  ( 0.000000000000000000, -59.46389618801928378, -49.70050353004953791 ) ) ;
#61434 = DIRECTION ( 'NONE',  ( -1.000000000000000000, 0.000000000000000000, 0.000000000000000000 ) ) ;
#61435 = LINE ( 'NONE', #73053, #6002 ) ;
#61436 = CARTESIAN_POINT ( 'NONE',  ( -92.35000000000013642, 91.52997821335257811, 86.56041666666668277 ) ) ;
#61437 = CARTESIAN_POINT ( 'NONE',  ( 25.81725066941077529, -113.8380548628854854, 5.500000000000000000 ) ) ;
#61438 = DIRECTION ( 'NONE',  ( 0.000000000000000000, 0.4539904997395478592, -0.8910065241883673437 ) ) ;
#61439 = FACE_OUTER_BOUND ( 'NONE', #12657, .T. ) ;
#61440 = ORIENTED_EDGE ( 'NONE', *, *, #65183, .T. ) ;
#61441 = AXIS2_PLACEMENT_3D ( 'NONE', #40894, #59659, #65308 ) ;
#61442 = EDGE_LOOP ( 'NONE', ( #9655, #7574, #58381, #47441 ) ) ;
#61443 = VECTOR ( 'NONE', #68311, 1000.000000000000000 ) ;
#61444 = CARTESIAN_POINT ( 'NONE',  ( -95.00000000000002842, 93.05995642670501411, 80.95125000000000171 ) ) ;
#61445 = DIRECTION ( 'NONE',  ( -0.6516173805718079581, 0.7585478161175706058, 0.000000000000000000 ) ) ;
#61446 = CARTESIAN_POINT ( 'NONE',  ( 0.000000000000000000, 0.000000000000000000, 0.000000000000000000 ) ) ;
#61447 = DIRECTION ( 'NONE',  ( -1.000000000000000000, 0.000000000000000000, 0.000000000000000000 ) ) ;
#61448 = CARTESIAN_POINT ( 'NONE',  ( 11.99999999999999822, 28.89263327155849126, -71.91182617369157981 ) ) ;
#61449 = DIRECTION ( 'NONE',  ( -1.000000000000000000, 0.000000000000000000, -0.000000000000000000 ) ) ;
#61450 = DIRECTION ( 'NONE',  ( 0.000000000000000000, 0.000000000000000000, 1.000000000000000000 ) ) ;
#61451 = DIRECTION ( 'NONE',  ( 0.000000000000000000, 0.07845909572784512398, -0.9969173337331279638 ) ) ;
#61452 = ORIENTED_EDGE ( 'NONE', *, *, #68781, .F. ) ;
#61453 = CARTESIAN_POINT ( 'NONE',  ( -95.00000000000002842, 87.33691857156074434, 80.27656250086714351 ) ) ;
#61454 = EDGE_CURVE ( 'NONE', #19565, #9220, #37947, .T. ) ;
#61455 = DIRECTION ( 'NONE',  ( -0.000000000000000000, -0.000000000000000000, 1.000000000000000000 ) ) ;
#61456 = CARTESIAN_POINT ( 'NONE',  ( 6.000000000000000000, -39.47590169984898267, 71.87247863392400404 ) ) ;
#61457 = LINE ( 'NONE', #25391, #40588 ) ;
#61458 = EDGE_CURVE ( 'NONE', #61374, #53067, #22140, .T. ) ;
#61459 = CARTESIAN_POINT ( 'NONE',  ( -6.938893903907228378E-15, -80.00000000000000000, -110.0000000000000000 ) ) ;
#61460 = DIRECTION ( 'NONE',  ( 1.000000000000000000, 0.000000000000000000, 0.000000000000000000 ) ) ;
#61461 = CARTESIAN_POINT ( 'NONE',  ( 0.000000000000000000, 0.000000000000000000, 0.000000000000000000 ) ) ;
#61462 = SHAPE_REPRESENTATION_RELATIONSHIP ( 'NONE' , 'NONE' ,  #8524, #7701 ) ;
#61463 = LINE ( 'NONE', #55066, #42453 ) ;
#61464 = ADVANCED_FACE ( 'NONE', ( #45082 ), #43963, .T. ) ;
#61465 = ADVANCED_FACE ( 'NONE', ( #16498 ), #60519, .T. ) ;
#61466 = CARTESIAN_POINT ( 'NONE',  ( 92.69370383062498320, 91.33154071421968467, 81.49364583420049257 ) ) ;
#61467 = CARTESIAN_POINT ( 'NONE',  ( -96.15314808468745866, -211.9973110713294489, 82.92239583420048632 ) ) ;
#61468 = DIRECTION ( 'NONE',  ( 0.000000000000000000, 0.000000000000000000, 1.000000000000000000 ) ) ;
#61469 = ORIENTED_EDGE ( 'NONE', *, *, #55536, .F. ) ;
#61470 = COLOUR_RGB ( '', 0.40784314, 0.44705882, 0.49803922) ;
#61471 = CYLINDRICAL_SURFACE ( 'NONE', #28080, 77.49899999999999523 ) ;
#61472 = AXIS2_PLACEMENT_3D ( 'NONE', #27387, #15753, #21761 ) ;
#61473 = CARTESIAN_POINT ( 'NONE',  ( -97.64999999999996305, -209.9999999999999716, 77.93499999999998806 ) ) ;
#61474 = CARTESIAN_POINT ( 'NONE',  ( 97.64999999999987779, -208.4700217866473793, 78.30541666666667311 ) ) ;
#61475 = CARTESIAN_POINT ( 'NONE',  ( -92.69370383062505425, 91.33154071421968467, 76.83697916753382628 ) ) ;
#61477 = EDGE_CURVE ( 'NONE', #15522, #31227, #68063, .T. ) ;
#61476 = CARTESIAN_POINT ( 'NONE',  ( 97.30629616937498838, -209.9999999999999716, 81.07031250086714635 ) ) ;
#61478 = ORIENTED_EDGE ( 'NONE', *, *, #19446, .T. ) ;
#61479 = VECTOR ( 'NONE', #9915, 1000.000000000000114 ) ;
#61480 = EDGE_CURVE ( 'NONE', #33774, #44570, #17669, .T. ) ;
#61481 = DIRECTION ( 'NONE',  ( 1.000000000000000000, 0.000000000000000000, 0.000000000000000000 ) ) ;
#61482 = ORIENTED_EDGE ( 'NONE', *, *, #49814, .F. ) ;
#61483 = CIRCLE ( 'NONE', #57882, 77.49899999999999523 ) ;
#61484 = DIRECTION ( 'NONE',  ( 0.000000000000000000, -0.5000000000000028866, -0.8660254037844369313 ) ) ;
#61485 = EDGE_LOOP ( 'NONE', ( #41891, #50762, #22450 ) ) ;
#61486 = CIRCLE ( 'NONE', #63862, 23.50000000000489919 ) ;
#61487 = DIRECTION ( 'NONE',  ( -0.000000000000000000, -0.000000000000000000, 1.000000000000000000 ) ) ;
#61488 = CIRCLE ( 'NONE', #51875, 42.00000000000000000 ) ;
#61489 = ORIENTED_EDGE ( 'NONE', *, *, #43047, .F. ) ;
#61490 = ORIENTED_EDGE ( 'NONE', *, *, #25299, .T. ) ;
#61491 = DIRECTION ( 'NONE',  ( 0.000000000000000000, 0.000000000000000000, 1.000000000000000000 ) ) ;
#61492 = DIRECTION ( 'NONE',  ( 0.000000000000000000, -0.4999999999999998335, 0.8660254037844387076 ) ) ;
#61493 = DIRECTION ( 'NONE',  ( -1.000000000000000000, -0.000000000000000000, -0.000000000000000000 ) ) ;
#61494 = CARTESIAN_POINT ( 'NONE',  ( -96.67299840332304939, 88.01659165168840104, 74.96344747200083702 ) ) ;
#61495 = CARTESIAN_POINT ( 'NONE',  ( 94.99999999999998579, 92.66308142843935514, 88.37281250086715545 ) ) ;
#61496 = LINE ( 'NONE', #4358, #59826 ) ;
#61497 = CARTESIAN_POINT ( 'NONE',  ( 97.64999999999997726, -208.4700217866474645, 77.03541666666666288 ) ) ;
#61498 = ORIENTED_EDGE ( 'NONE', *, *, #59261, .T. ) ;
#61499 = ORIENTED_EDGE ( 'NONE', *, *, #57493, .T. ) ;
#61500 = EDGE_LOOP ( 'NONE', ( #68200, #44304, #68805, #43823, #223 ) ) ;
#61501 = VERTEX_POINT ( 'NONE', #26281 ) ;
#61502 = CYLINDRICAL_SURFACE ( 'NONE', #20180, 77.49899999999999523 ) ;
#61503 = CARTESIAN_POINT ( 'NONE',  ( 0.000000000000000000, 72.35432306680485226, -20.40083707022909110 ) ) ;
#61504 = DIRECTION ( 'NONE',  ( 1.000000000000000000, 1.427937372958405461E-15, 7.962523111839130290E-16 ) ) ;
#61505 = DIRECTION ( 'NONE',  ( 1.000000000000000000, 0.000000000000000000, 0.000000000000000000 ) ) ;
#61506 = FACE_OUTER_BOUND ( 'NONE', #2079, .T. ) ;
#61507 = CARTESIAN_POINT ( 'NONE',  ( -7.469491406282116941, 4.756046723998916370, -55.00000000000000000 ) ) ;
#61508 = ORIENTED_EDGE ( 'NONE', *, *, #70797, .F. ) ;
#61509 = CARTESIAN_POINT ( 'NONE',  ( -93.67499999999998295, -212.2949673200287179, 83.30604166840096525 ) ) ;
#61510 = ORIENTED_EDGE ( 'NONE', *, *, #6229, .T. ) ;
#61511 = CARTESIAN_POINT ( 'NONE',  ( 97.64999999999999147, -209.9999999999999716, 90.00000000000000000 ) ) ;
#61512 = ORIENTED_EDGE ( 'NONE', *, *, #56169, .F. ) ;
#61513 = CARTESIAN_POINT ( 'NONE',  ( -92.35000000000005116, 91.52997821335253548, 82.82979166840095786 ) ) ;
#61514 = ORIENTED_EDGE ( 'NONE', *, *, #18518, .F. ) ;
#61515 = CARTESIAN_POINT ( 'NONE',  ( 97.30629616937498838, 88.66845928578037217, 81.81114583420048803 ) ) ;
#61516 = DIRECTION ( 'NONE',  ( -1.000000000000000000, -0.000000000000000000, 0.000000000000000000 ) ) ;
#61518 = EDGE_CURVE ( 'NONE', #31113, #47563, #35639, .T. ) ;
#61517 = CARTESIAN_POINT ( 'NONE',  ( -92.34999999999999432, -209.9999999999999716, 82.69749999999999091 ) ) ;
#61519 = CYLINDRICAL_SURFACE ( 'NONE', #16987, 77.49899999999999523 ) ;
#61520 = CARTESIAN_POINT ( 'NONE',  ( 5.999999999999999112, -68.55367621811110723, -44.99326035066126650 ) ) ;
#61521 =( GEOMETRIC_REPRESENTATION_CONTEXT ( 3 ) GLOBAL_UNCERTAINTY_ASSIGNED_CONTEXT ( ( #71990 ) ) GLOBAL_UNIT_ASSIGNED_CONTEXT ( ( #31516, #14223, #65742 ) ) REPRESENTATION_CONTEXT ( 'NONE', 'WORKASPACE' ) );
#61522 = CARTESIAN_POINT ( 'NONE',  ( 92.35000000000003695, 91.52997821335253548, 88.04208333333330927 ) ) ;
#61523 = ORIENTED_EDGE ( 'NONE', *, *, #9221, .T. ) ;
#61524 = DIRECTION ( 'NONE',  ( -1.000000000000000000, -0.000000000000000000, -0.000000000000000000 ) ) ;
#61525 = CARTESIAN_POINT ( 'NONE',  ( 10.00000000000000000, 0.000000000000000000, 0.000000000000000000 ) ) ;
#61526 = CARTESIAN_POINT ( 'NONE',  ( 11.99999999999999822, 0.000000000000000000, 0.000000000000000000 ) ) ;
#61527 = EDGE_LOOP ( 'NONE', ( #52620, #13850, #10639, #41797 ) ) ;
#61528 = AXIS2_PLACEMENT_3D ( 'NONE', #52423, #63734, #23497 ) ;
#61529 = ORIENTED_EDGE ( 'NONE', *, *, #60263, .T. ) ;
#61530 = ADVANCED_FACE ( 'NONE', ( #33033 ), #49951, .T. ) ;
#61531 = ADVANCED_FACE ( 'NONE', ( #21372 ), #49582, .T. ) ;
#61532 = AXIS2_PLACEMENT_3D ( 'NONE', #57468, #28891, #45461 ) ;
#61533 = CYLINDRICAL_SURFACE ( 'NONE', #22809, 31.99999999999998579 ) ;
#61534 = DIRECTION ( 'NONE',  ( 1.000000000000000000, -0.000000000000000000, -0.000000000000000000 ) ) ;
#61535 = CARTESIAN_POINT ( 'NONE',  ( -21.67772167707813935, -110.8034581014852762, 5.500000000000000000 ) ) ;
#61536 = VECTOR ( 'NONE', #28875, 1000.000000000000000 ) ;
#61537 =( BOUNDED_CURVE ( )  B_SPLINE_CURVE ( 2, ( #8389, #20408, #65915, #8758, #71522, #25674, #14755 ),
 .UNSPECIFIED., .F., .F. ) 
 B_SPLINE_CURVE_WITH_KNOTS ( ( 3, 2, 2, 3 ),
 ( 0.06249999999999966693, 0.06944444444444407283, 0.07638888888888849260, 0.08333333333333288462 ),
 .UNSPECIFIED. ) 
 CURVE ( )  GEOMETRIC_REPRESENTATION_ITEM ( )  RATIONAL_B_SPLINE_CURVE ( ( 1.000000000000006439, 0.8660254037844322683, 1.000000000000000000, 0.8660254037844387076, 1.000000000000000000, 0.8660254037844472563, 0.9999999999999914513 ) ) 
 REPRESENTATION_ITEM ( '' )  );
#61538 = CARTESIAN_POINT ( 'NONE',  ( -94.99999999999997158, -212.6630814284392557, 79.80031250086715033 ) ) ;
#61539 = ORIENTED_EDGE ( 'NONE', *, *, #40338, .T. ) ;
#61540 = DIRECTION ( 'NONE',  ( 0.000000000000000000, -6.938893903907229955E-15, 1.000000000000000000 ) ) ;
#61541 = ORIENTED_EDGE ( 'NONE', *, *, #52512, .F. ) ;
#61542 = EDGE_CURVE ( 'NONE', #55710, #10397, #15754, .T. ) ;
#61543 = CARTESIAN_POINT ( 'NONE',  ( -10.00000000000000000, 0.000000000000000000, 0.000000000000000000 ) ) ;
#61544 = AXIS2_PLACEMENT_3D ( 'NONE', #31785, #70518, #7763 ) ;
#61545 = CIRCLE ( 'NONE', #71125, 15.99999999999999822 ) ;
#61546 = CARTESIAN_POINT ( 'NONE',  ( -10.00000000000000000, 0.000000000000000000, 0.000000000000000000 ) ) ;
#61547 = CARTESIAN_POINT ( 'NONE',  ( -97.64999999999996305, -211.5299782133524218, 76.16229166840095388 ) ) ;
#61548 = CARTESIAN_POINT ( 'NONE',  ( 96.15314808468748708, 91.99731107132950569, 78.63614583420047666 ) ) ;
#61549 = DIRECTION ( 'NONE',  ( 1.000000000000000000, 0.000000000000000000, -0.000000000000000000 ) ) ;
#61550 = DIRECTION ( 'NONE',  ( 1.000000000000000000, 0.000000000000000000, 0.000000000000000000 ) ) ;
#61551 = DIRECTION ( 'NONE',  ( -1.000000000000000000, 0.000000000000000000, 0.000000000000000000 ) ) ;
#61552 = CYLINDRICAL_SURFACE ( 'NONE', #70053, 2.649999999999999467 ) ;
#61553 = CARTESIAN_POINT ( 'NONE',  ( 5.999999999999999112, -46.11716303203136391, -67.80270845531939017 ) ) ;
#61554 = CARTESIAN_POINT ( 'NONE',  ( 95.00000000000000000, -213.0599564267049857, 84.44374999999999432 ) ) ;
#61555 = ADVANCED_FACE ( 'NONE', ( #40537 ), #6345, .F. ) ;
#61556 = CARTESIAN_POINT ( 'NONE',  ( 0.000000000000000000, 6.555932627142418312, 37.01155633439060466 ) ) ;
#61557 = DIRECTION ( 'NONE',  ( 0.000000000000000000, 0.1564344650402242909, 0.9876883405951387696 ) ) ;
#61558 = DIRECTION ( 'NONE',  ( 0.000000000000000000, 0.8526401643540935105, -0.5224985647159468005 ) ) ;
#61559 = ORIENTED_EDGE ( 'NONE', *, *, #33346, .T. ) ;
#61560 = CARTESIAN_POINT ( 'NONE',  ( -97.30629616937501680, 90.00000000000004263, 83.29281250086714294 ) ) ;
#61561 = DIRECTION ( 'NONE',  ( 0.000000000000000000, 0.000000000000000000, 1.000000000000000000 ) ) ;
#61563 = EDGE_CURVE ( 'NONE', #8860, #16018, #2097, .T. ) ;
#61562 = CARTESIAN_POINT ( 'NONE',  ( -10.00000000000000000, 0.000000000000000000, 0.000000000000000000 ) ) ;
#61564 = EDGE_CURVE ( 'NONE', #9521, #38802, #14006, .T. ) ;
#61565 = ORIENTED_EDGE ( 'NONE', *, *, #36227, .F. ) ;
#61566 = CARTESIAN_POINT ( 'NONE',  ( 0.3000000000000016542, 0.000000000000000000, 0.000000000000000000 ) ) ;
#61567 = EDGE_CURVE ( 'NONE', #50834, #1543, #45278, .T. ) ;
#61568 = CARTESIAN_POINT ( 'NONE',  ( 0.000000000000000000, -40.68715046381921496, -10.41901085202121280 ) ) ;
#61569 = DIRECTION ( 'NONE',  ( 0.000000000000000000, 0.000000000000000000, 1.000000000000000000 ) ) ;
#61570 = DIRECTION ( 'NONE',  ( -0.000000000000000000, -0.000000000000000000, -1.000000000000000000 ) ) ;
#61571 = CARTESIAN_POINT ( 'NONE',  ( 92.69370383062501162, -209.9999999999999716, 77.73656250086715147 ) ) ;
#61572 = VECTOR ( 'NONE', #18952, 1000.000000000000000 ) ;
#61573 = ORIENTED_EDGE ( 'NONE', *, *, #12276, .F. ) ;
#61574 = VERTEX_POINT ( 'NONE', #51077 ) ;
#61575 = DIRECTION ( 'NONE',  ( 1.000000000000000000, -0.000000000000000000, -0.000000000000000000 ) ) ;
#61576 = CARTESIAN_POINT ( 'NONE',  ( 97.64999999999999147, -210.0000001167898631, 84.68187499741277691 ) ) ;
#61577 = AXIS2_PLACEMENT_3D ( 'NONE', #28037, #67905, #74277 ) ;
#61578 = CARTESIAN_POINT ( 'NONE',  ( 96.66135172262724495, 88.39919842643632819, 74.79754476654878204 ) ) ;
#61579 = DIRECTION ( 'NONE',  ( -1.000000000000000000, 0.000000000000000000, -0.000000000000000000 ) ) ;
#61580 = LINE ( 'NONE', #23217, #45359 ) ;
#61581 = CARTESIAN_POINT ( 'NONE',  ( 92.35000000000002274, -211.5299782133524502, 88.14791666666666003 ) ) ;
#61582 = VERTEX_POINT ( 'NONE', #29605 ) ;
#61583 = DIRECTION ( 'NONE',  ( -0.000000000000000000, -0.000000000000000000, -1.000000000000000000 ) ) ;
#61584 = VERTEX_POINT ( 'NONE', #63858 ) ;
#61585 = AXIS2_PLACEMENT_3D ( 'NONE', #67449, #44530, #9564 ) ;
#61586 = ORIENTED_EDGE ( 'NONE', *, *, #32016, .F. ) ;
#61587 = DIRECTION ( 'NONE',  ( 0.000000000000000000, 0.000000000000000000, 1.000000000000000000 ) ) ;
#61588 = AXIS2_PLACEMENT_3D ( 'NONE', #24736, #13809, #48039 ) ;
#61589 = CARTESIAN_POINT ( 'NONE',  ( 0.000000000000000000, -73.95703589263990807, 23.16143007188399139 ) ) ;
#61590 = ORIENTED_EDGE ( 'NONE', *, *, #59430, .T. ) ;
#61591 = CARTESIAN_POINT ( 'NONE',  ( 97.64999999999324132, -209.9999940177821713, 82.14187520865721126 ) ) ;
#61592 = CARTESIAN_POINT ( 'NONE',  ( 96.32499999999998863, -207.7050326799711968, 79.07270833506763097 ) ) ;
#61593 = CARTESIAN_POINT ( 'NONE',  ( 97.64999999999999147, 90.00000000000002842, 80.15749999999999886 ) ) ;
#61594 = ORIENTED_EDGE ( 'NONE', *, *, #68679, .F. ) ;
#61595 = DIRECTION ( 'NONE',  ( -1.000000000000000000, 0.000000000000000000, 0.000000000000000000 ) ) ;
#61596 = VERTEX_POINT ( 'NONE', #52182 ) ;
#61597 = CARTESIAN_POINT ( 'NONE',  ( -92.35002509397452286, -211.5299927013654155, 89.07395733288689144 ) ) ;
#61598 = ORIENTED_EDGE ( 'NONE', *, *, #8050, .T. ) ;
#61599 = EDGE_LOOP ( 'NONE', ( #39156, #62355, #39061, #6799 ) ) ;
#61600 = CARTESIAN_POINT ( 'NONE',  ( -92.69370383062505425, 88.66845928578038638, 83.08114583420048405 ) ) ;
#61601 = CARTESIAN_POINT ( 'NONE',  ( 92.69370383062498320, 91.33154071421968467, 79.42989583420046529 ) ) ;
#61602 = ORIENTED_EDGE ( 'NONE', *, *, #37550, .F. ) ;
#61603 = CARTESIAN_POINT ( 'NONE',  ( 0.000000000000000000, 10.30890764327501152, -81.34940948281325745 ) ) ;
#61604 = EDGE_CURVE ( 'NONE', #9618, #37989, #12825, .T. ) ;
#61605 = CARTESIAN_POINT ( 'NONE',  ( -97.65000000000009095, 88.47002178664760663, 80.52791666666665549 ) ) ;
#61606 = DIRECTION ( 'NONE',  ( -1.000000000000000000, 1.047380211910311281E-14, 2.618450529775778123E-14 ) ) ;
#61607 = ORIENTED_EDGE ( 'NONE', *, *, #38215, .F. ) ;
#61608 = LINE ( 'NONE', #15741, #2102 ) ;
#61609 = CARTESIAN_POINT ( 'NONE',  ( -92.69370383062498320, -209.9999999999999716, 81.07031250086714635 ) ) ;
#61610 = VERTEX_POINT ( 'NONE', #731 ) ;
#61611 = ORIENTED_EDGE ( 'NONE', *, *, #67572, .T. ) ;
#61612 = EDGE_CURVE ( 'NONE', #9787, #62521, #63130, .T. ) ;
#61613 = CARTESIAN_POINT ( 'NONE',  ( 92.34999999999999432, 90.00000000000002842, 79.20499999999999829 ) ) ;
#61614 = EDGE_CURVE ( 'NONE', #16267, #39310, #57286, .T. ) ;
#61615 = ORIENTED_EDGE ( 'NONE', *, *, #18570, .F. ) ;
#61616 = CARTESIAN_POINT ( 'NONE',  ( 11.99999999999999822, -77.49459641780886443, 0.8261519478428549501 ) ) ;
#61617 = TOROIDAL_SURFACE ( 'NONE', #44993, 22.90000000000000213, 0.5999999999999937605 ) ;
#61618 = DIRECTION ( 'NONE',  ( 0.000000000000000000, 0.000000000000000000, 1.000000000000000000 ) ) ;
#61619 = ORIENTED_EDGE ( 'NONE', *, *, #20287, .T. ) ;
#61620 = CARTESIAN_POINT ( 'NONE',  ( -96.15314808468747287, -208.0026889286704943, 80.64697916753381435 ) ) ;
#61621 = VERTEX_POINT ( 'NONE', #22896 ) ;
#61622 = CARTESIAN_POINT ( 'NONE',  ( 92.34999999999999432, 89.99996562134467126, 88.80937619077334944 ) ) ;
#61623 = CARTESIAN_POINT ( 'NONE',  ( 11.99999999999999822, 73.73191006444572793, -14.66109333815486515 ) ) ;
#61624 = DIRECTION ( 'NONE',  ( 1.000000000000000000, 0.000000000000000000, 0.000000000000000000 ) ) ;
#61625 = DIRECTION ( 'NONE',  ( -1.000000000000000000, 0.000000000000000000, -0.000000000000000000 ) ) ;
#61626 = ADVANCED_FACE ( 'NONE', ( #12332 ), #56740, .T. ) ;
#61627 = CARTESIAN_POINT ( 'NONE',  ( 96.92442009029373651, 88.17815826261617929, 75.00000000000000000 ) ) ;
#61628 = VECTOR ( 'NONE', #3519, 1000.000000000000000 ) ;
#61629 = CARTESIAN_POINT ( 'NONE',  ( 15.00000000000000000, 9.615535125379096826, 24.73947219025905042 ) ) ;
#61630 = CARTESIAN_POINT ( 'NONE',  ( 92.69370383062498320, 90.00000000000002842, 89.00781250086714635 ) ) ;
#61631 = DIRECTION ( 'NONE',  ( -0.000000000000000000, -0.000000000000000000, -1.000000000000000000 ) ) ;
#61632 = CARTESIAN_POINT ( 'NONE',  ( 0.000000000000000000, -71.27951684758005513, -30.41916302227188851 ) ) ;
#61633 = CARTESIAN_POINT ( 'NONE',  ( 11.99999999999999822, 75.54627589209944460, 17.28742895386110945 ) ) ;
#61634 = CARTESIAN_POINT ( 'NONE',  ( -92.35000000000005116, 91.52997821335253548, 88.54479166840097548 ) ) ;
#61635 = LINE ( 'NONE', #15768, #45227 ) ;
#61636 = CARTESIAN_POINT ( 'NONE',  ( 0.000000000000000000, 46.53671651293948486, 59.03961581697416250 ) ) ;
#61637 = CARTESIAN_POINT ( 'NONE',  ( -13.05994868825747446, -139.5943292883446532, 5.500000000000000000 ) ) ;
#61638 = AXIS2_PLACEMENT_3D ( 'NONE', #19953, #14322, #53804 ) ;
#61639 = DIRECTION ( 'NONE',  ( -1.000000000000000000, -0.000000000000000000, 0.000000000000000000 ) ) ;
#61640 = EDGE_CURVE ( 'NONE', #45606, #58096, #63484, .T. ) ;
#61641 = CARTESIAN_POINT ( 'NONE',  ( 96.32499999999997442, 92.29496732002878900, 75.89770833506763381 ) ) ;
#61642 = CARTESIAN_POINT ( 'NONE',  ( 0.000000000000000000, 55.16347631943131802, -60.67117009219075641 ) ) ;
#61643 = CIRCLE ( 'NONE', #67653, 77.49899999999999523 ) ;
#61644 = DIRECTION ( 'NONE',  ( 0.000000000000000000, 1.000000000000000000, 3.469446951953614189E-15 ) ) ;
#61645 = CIRCLE ( 'NONE', #2857, 4.749999999999999112 ) ;
#61646 = AXIS2_PLACEMENT_3D ( 'NONE', #30642, #52858, #63780 ) ;
#61647 = CARTESIAN_POINT ( 'NONE',  ( 1.459549131277868561, -120.3460004817713411, -2.500000000000000000 ) ) ;
#61648 = CARTESIAN_POINT ( 'NONE',  ( -96.32499999999996021, -207.7050326799711968, 84.17916666666666003 ) ) ;
#61649 = DIRECTION ( 'NONE',  ( -1.000000000000000000, 0.000000000000000000, 0.000000000000000000 ) ) ;
#61650 = EDGE_CURVE ( 'NONE', #39929, #52914, #11583, .T. ) ;
#61651 = ADVANCED_FACE ( 'NONE', ( #58197 ), #1105, .T. ) ;
#61652 = DIRECTION ( 'NONE',  ( 0.000000000000000000, 0.000000000000000000, 1.000000000000000000 ) ) ;
#61653 = LINE ( 'NONE', #21788, #33436 ) ;
#61654 = DIRECTION ( 'NONE',  ( -8.332732854036912157E-16, -1.065814103640131031E-14, -1.000000000000000000 ) ) ;
#61655 = FACE_OUTER_BOUND ( 'NONE', #4534, .T. ) ;
#61656 = CARTESIAN_POINT ( 'NONE',  ( 97.30629616937498838, -208.6684592857803011, 87.63197916753382799 ) ) ;
#61657 = VERTEX_POINT ( 'NONE', #74001 ) ;
#61658 = ORIENTED_EDGE ( 'NONE', *, *, #28562, .T. ) ;
#61659 = DIRECTION ( 'NONE',  ( 1.000000000000000000, 0.000000000000000000, 0.000000000000000000 ) ) ;
#61660 = CARTESIAN_POINT ( 'NONE',  ( -8.637688417678527131, 13.69818742750669394, 32.98187577049606745 ) ) ;
#61661 = ORIENTED_EDGE ( 'NONE', *, *, #72144, .T. ) ;
#61662 = TOROIDAL_SURFACE ( 'NONE', #40101, 18.00000000000000000, 3.300000000000000266 ) ;
#61663 = CARTESIAN_POINT ( 'NONE',  ( 93.84685191531251292, -211.9973110713294489, 78.31864583420048120 ) ) ;
#61664 = CARTESIAN_POINT ( 'NONE',  ( 95.00000000000000000, -212.6630814284392557, 86.78531250086713555 ) ) ;
#61665 = ORIENTED_EDGE ( 'NONE', *, *, #11687, .F. ) ;
#61666 = CARTESIAN_POINT ( 'NONE',  ( 92.69370383062501162, -208.6684592857803011, 87.84364583420048689 ) ) ;
#61667 = AXIS2_PLACEMENT_3D ( 'NONE', #59148, #65535, #54256 ) ;
#61668 = ADVANCED_FACE ( 'NONE', ( #66365 ), #66001, .T. ) ;
#61669 = VERTEX_POINT ( 'NONE', #57843 ) ;
#61670 = CARTESIAN_POINT ( 'NONE',  ( -1.433254160131044044E-14, -1.896421744167617418E-13, -18.00000000000031974 ) ) ;
#61671 = VERTEX_POINT ( 'NONE', #68390 ) ;
#61672 = DIRECTION ( 'NONE',  ( 0.000000000000000000, 0.8090169943749488946, -0.5877852522924712497 ) ) ;
#61673 = AXIS2_PLACEMENT_3D ( 'NONE', #72740, #22000, #44195 ) ;
#61674 = ORIENTED_EDGE ( 'NONE', *, *, #64526, .F. ) ;
#61675 = PLANE ( 'NONE',  #17259 ) ;
#61676 = ORIENTED_EDGE ( 'NONE', *, *, #25190, .T. ) ;
#61677 = CARTESIAN_POINT ( 'NONE',  ( -92.35000000000009379, 88.47002178664750716, 77.56458333333333144 ) ) ;
#61678 = CARTESIAN_POINT ( 'NONE',  ( 92.35000000000000853, -209.9999999999999716, 88.80937500173430976 ) ) ;
#61679 = ORIENTED_EDGE ( 'NONE', *, *, #43474, .F. ) ;
#61680 = DIRECTION ( 'NONE',  ( -0.000000000000000000, -0.000000000000000000, 1.000000000000000000 ) ) ;
#61681 = EDGE_CURVE ( 'NONE', #24224, #29448, #16877, .T. ) ;
#61682 = AXIS2_PLACEMENT_3D ( 'NONE', #15058, #67687, #27071 ) ;
#61683 = ORIENTED_EDGE ( 'NONE', *, *, #73560, .F. ) ;
#61684 = CARTESIAN_POINT ( 'NONE',  ( 22.63442173698368620, -133.7816164738524378, 2.500000000000000000 ) ) ;
#61685 = AXIS2_PLACEMENT_3D ( 'NONE', #8851, #67096, #50544 ) ;
#61686 = ORIENTED_EDGE ( 'NONE', *, *, #68155, .F. ) ;
#61687 = EDGE_CURVE ( 'NONE', #50461, #42081, #62764, .T. ) ;
#61688 = EDGE_LOOP ( 'NONE', ( #58908, #55567, #58087, #14392 ) ) ;
#61689 = CIRCLE ( 'NONE', #73645, 37.49900000000000233 ) ;
#61690 = EDGE_LOOP ( 'NONE', ( #18017, #32407 ) ) ;
#61691 = CARTESIAN_POINT ( 'NONE',  ( 97.30629616937497417, -210.9303163890423605, 74.68334086212732359 ) ) ;
#61692 = AXIS2_PLACEMENT_3D ( 'NONE', #44353, #16148, #4515 ) ;
#61693 = CONTEXT_DEPENDENT_SHAPE_REPRESENTATION ( #49394, #53689 ) ;
#61694 = PLANE ( 'NONE',  #19811 ) ;
#61696 = EDGE_CURVE ( 'NONE', #14729, #53011, #44076, .T. ) ;
#61695 = VERTEX_POINT ( 'NONE', #51822 ) ;
#61697 = ORIENTED_EDGE ( 'NONE', *, *, #7295, .F. ) ;
#61698 = VERTEX_POINT ( 'NONE', #28504 ) ;
#61699 = CARTESIAN_POINT ( 'NONE',  ( 11.99999999999999822, -81.96053171279901051, -2.543863470249249747 ) ) ;
#61700 = ADVANCED_FACE ( 'NONE', ( #5985 ), #28890, .T. ) ;
#61701 = CARTESIAN_POINT ( 'NONE',  ( 92.35000000000000853, -209.9999999999999716, 86.82500000000000284 ) ) ;
#61702 = CARTESIAN_POINT ( 'NONE',  ( -96.15314808468751551, 88.00268892867056536, 77.20739583420048291 ) ) ;
#61703 = ORIENTED_EDGE ( 'NONE', *, *, #30146, .F. ) ;
#61704 = CARTESIAN_POINT ( 'NONE',  ( 93.84685191531248449, 91.99731107132950569, 76.83697916753381207 ) ) ;
#61705 = VERTEX_POINT ( 'NONE', #59307 ) ;
#61706 = CARTESIAN_POINT ( 'NONE',  ( -92.69370383062498320, -211.3315407142195852, 89.27239583420048064 ) ) ;
#61707 = ORIENTED_EDGE ( 'NONE', *, *, #5174, .T. ) ;
#61708 = PLANE ( 'NONE',  #12183 ) ;
#61709 = CYLINDRICAL_SURFACE ( 'NONE', #41598, 42.00000000000000000 ) ;
#61710 = DIRECTION ( 'NONE',  ( 0.000000000000000000, 0.000000000000000000, 1.000000000000000000 ) ) ;
#61711 = CARTESIAN_POINT ( 'NONE',  ( -92.69370383062498320, -211.3315407142195852, 79.74739583420047495 ) ) ;
#61712 = AXIS2_PLACEMENT_3D ( 'NONE', #28486, #67242, #33380 ) ;
#61713 = EDGE_CURVE ( 'NONE', #63983, #34836, #2579, .T. ) ;
#61714 = CYLINDRICAL_SURFACE ( 'NONE', #32646, 2.649999999999999467 ) ;
#61715 = LINE ( 'NONE', #50036, #73928 ) ;
#61716 = CARTESIAN_POINT ( 'NONE',  ( -92.34999999999999432, -211.5299782133524218, 79.46958333333331836 ) ) ;
#61717 = ORIENTED_EDGE ( 'NONE', *, *, #18535, .T. ) ;
#61718 = ORIENTED_EDGE ( 'NONE', *, *, #37358, .T. ) ;
#61719 = LINE ( 'NONE', #50041, #33678 ) ;
#61720 = CARTESIAN_POINT ( 'NONE',  ( 0.000000000000000000, 0.000000000000000000, 0.000000000000000000 ) ) ;
#61721 = CARTESIAN_POINT ( 'NONE',  ( 94.32747394040364952, -207.6887180216937452, 74.85222950654851104 ) ) ;
#61722 = CARTESIAN_POINT ( 'NONE',  ( -96.15314808468752972, 91.99731107132950569, 81.28197916753380525 ) ) ;
#61723 = CARTESIAN_POINT ( 'NONE',  ( -12.49999999999999645, 1.530808498934191127E-15, -175.0000000000000000 ) ) ;
#61724 = DIRECTION ( 'NONE',  ( 1.000000000000000000, 0.000000000000000000, -0.000000000000000000 ) ) ;
#61725 = VECTOR ( 'NONE', #44239, 1000.000000000000000 ) ;
#61726 = EDGE_CURVE ( 'NONE', #48459, #56518, #14059, .T. ) ;
#61727 = ORIENTED_EDGE ( 'NONE', *, *, #57877, .T. ) ;
#61728 = EDGE_CURVE ( 'NONE', #13032, #50832, #59684, .T. ) ;
#61729 = DIRECTION ( 'NONE',  ( 0.000000000000000000, 0.6691306063588676745, -0.7431448254773856954 ) ) ;
#61730 = EDGE_CURVE ( 'NONE', #68378, #45315, #41283, .T. ) ;
#61731 = EDGE_CURVE ( 'NONE', #423, #26840, #42392, .T. ) ;
#61733 = ADVANCED_FACE ( 'NONE', ( #30353 ), #12695, .F. ) ;
#61732 = CARTESIAN_POINT ( 'NONE',  ( 0.000000000000000000, -24.73286445877654671, -73.44644590900084324 ) ) ;
#61734 = DIRECTION ( 'NONE',  ( 1.000000000000000000, -0.000000000000000000, -0.000000000000000000 ) ) ;
#61735 = CIRCLE ( 'NONE', #542, 31.99999999999998934 ) ;
#61736 = DIRECTION ( 'NONE',  ( 0.000000000000000000, 0.000000000000000000, 1.000000000000000000 ) ) ;
#61737 = DIRECTION ( 'NONE',  ( -0.000000000000000000, -0.000000000000000000, 1.000000000000000000 ) ) ;
#61738 = CARTESIAN_POINT ( 'NONE',  ( -96.15314808468745866, -211.9973110713294489, 78.47739583420049314 ) ) ;
#61739 = DIRECTION ( 'NONE',  ( -1.000000000000000000, -0.000000000000000000, 0.000000000000000000 ) ) ;
#61740 = ADVANCED_FACE ( 'NONE', ( #42760 ), #60074, .F. ) ;
#61741 =( BOUNDED_CURVE ( )  B_SPLINE_CURVE ( 2, ( #54857, #51346, #71761, #32657, #45362 ),
 .UNSPECIFIED., .F., .F. ) 
 B_SPLINE_CURVE_WITH_KNOTS ( ( 3, 2, 3 ),
 ( 0.9525283480368235134, 0.9595841135647146247, 0.9629953541097220349 ),
 .UNSPECIFIED. ) 
 CURVE ( )  GEOMETRIC_REPRESENTATION_ITEM ( )  RATIONAL_B_SPLINE_CURVE ( ( 1.000000000000000000, 0.8660254037844387076, 1.000000000000000000, 0.9352274998423326657, 0.9330859296547711068 ) ) 
 REPRESENTATION_ITEM ( '' )  );
#61742 = EDGE_LOOP ( 'NONE', ( #33549, #16183, #71174, #12514 ) ) ;
#61743 = VECTOR ( 'NONE', #39557, 1000.000000000000000 ) ;
#61744 = CARTESIAN_POINT ( 'NONE',  ( -10.90093335751250692, 0.000000000000000000, 0.000000000000000000 ) ) ;
#61745 = CARTESIAN_POINT ( 'NONE',  ( 97.64999999999601243, 89.99999541993086893, 76.42687486206342840 ) ) ;
#61746 = DIRECTION ( 'NONE',  ( -0.000000000000000000, -0.000000000000000000, 1.000000000000000000 ) ) ;
#61747 = ORIENTED_EDGE ( 'NONE', *, *, #11523, .T. ) ;
#61748 = EDGE_CURVE ( 'NONE', #21151, #71560, #24725, .T. ) ;
#61749 = DIRECTION ( 'NONE',  ( 0.000000000000000000, 0.8090169943749445647, 0.5877852522924771339 ) ) ;
#61750 = DIRECTION ( 'NONE',  ( -1.000000000000000000, 0.000000000000000000, -0.000000000000000000 ) ) ;
#61751 = CIRCLE ( 'NONE', #17304, 12.49999999999999645 ) ;
#61752 = AXIS2_PLACEMENT_3D ( 'NONE', #44174, #61095, #32511 ) ;
#61753 = CARTESIAN_POINT ( 'NONE',  ( -92.35000000035631729, -210.0000434577671911, 89.12687334326093946 ) ) ;
#61754 = ORIENTED_EDGE ( 'NONE', *, *, #56827, .T. ) ;
#61755 = DIRECTION ( 'NONE',  ( -1.000000000000000000, -0.000000000000000000, -0.000000000000000000 ) ) ;
#61756 = DIRECTION ( 'NONE',  ( -1.000000000000000000, -0.000000000000000000, -0.000000000000000000 ) ) ;
#61757 = ORIENTED_EDGE ( 'NONE', *, *, #70589, .T. ) ;
#61758 =( BOUNDED_CURVE ( )  B_SPLINE_CURVE ( 2, ( #39062, #61622, #21371, #67260, #56360, #4875, #50702, #52545, #45832, #6344, #730 ),
 .UNSPECIFIED., .F., .F. ) 
 B_SPLINE_CURVE_WITH_KNOTS ( ( 3, 2, 2, 2, 2, 3 ),
 ( 0.04233441017594429673, 0.04233459324529424694, 0.04939035878617636238, 0.05644612432705847088, 0.06350188986794058632, 0.06350193517735322479 ),
 .UNSPECIFIED. ) 
 CURVE ( )  GEOMETRIC_REPRESENTATION_ITEM ( )  RATIONAL_B_SPLINE_CURVE ( ( 0.9999930479532725958, 0.9999965238864447770, 1.000000000000000000, 0.8660254037844387076, 1.000000000000000000, 0.8660254037844387076, 1.000000000000000000, 0.8660254037844387076, 1.000000000000000000, 0.9999991396666700894, 0.9999982793443895623 ) ) 
 REPRESENTATION_ITEM ( '' )  );
#61759 = CARTESIAN_POINT ( 'NONE',  ( 96.15314808468750130, -211.9973110713294489, 87.31447916753380412 ) ) ;
#61760 = DIRECTION ( 'NONE',  ( 0.000000000000000000, 0.3090169943749482839, -0.9510565162951533091 ) ) ;
#61761 = MANIFOLD_SOLID_BREP ( 'Boss-Extrude1', #62005 ) ;
#61762 = VERTEX_POINT ( 'NONE', #52930 ) ;
#61763 = AXIS2_PLACEMENT_3D ( 'NONE', #49384, #59567, #2822 ) ;
#61764 = DIRECTION ( 'NONE',  ( 0.000000000000000000, 0.000000000000000000, 1.000000000000000000 ) ) ;
#61765 = VERTEX_POINT ( 'NONE', #24360 ) ;
#61766 = FACE_BOUND ( 'NONE', #6845, .T. ) ;
#61767 = ORIENTED_EDGE ( 'NONE', *, *, #25380, .F. ) ;
#61768 = PLANE ( 'NONE',  #9613 ) ;
#61769 = ORIENTED_EDGE ( 'NONE', *, *, #60756, .F. ) ;
#61770 = ORIENTED_EDGE ( 'NONE', *, *, #42945, .T. ) ;
#61771 = ORIENTED_EDGE ( 'NONE', *, *, #48863, .F. ) ;
#61772 = CARTESIAN_POINT ( 'NONE',  ( 11.99999999999999822, -36.73666225445940370, 65.58780272294062286 ) ) ;
#61773 = ORIENTED_EDGE ( 'NONE', *, *, #71180, .F. ) ;
#61774 = VECTOR ( 'NONE', #12240, 1000.000000000000000 ) ;
#61775 = ORIENTED_EDGE ( 'NONE', *, *, #14783, .F. ) ;
#61776 = CARTESIAN_POINT ( 'NONE',  ( 96.15314808468748708, 91.99731107132950569, 77.52489583420047836 ) ) ;
#61777 = CARTESIAN_POINT ( 'NONE',  ( 15.00000000000000000, 14.60985201121729737, 18.46759930825687235 ) ) ;
#61778 = DIRECTION ( 'NONE',  ( 0.000000000000000000, 0.000000000000000000, 1.000000000000000000 ) ) ;
#61779 = ORIENTED_EDGE ( 'NONE', *, *, #29001, .T. ) ;
#61780 = ORIENTED_EDGE ( 'NONE', *, *, #45023, .F. ) ;
#61781 = EDGE_CURVE ( 'NONE', #39383, #74142, #47295, .T. ) ;
#61782 = ORIENTED_EDGE ( 'NONE', *, *, #7201, .T. ) ;
#61783 = CARTESIAN_POINT ( 'NONE',  ( 92.69370383062498320, 90.00000000000002842, 89.00781250086714635 ) ) ;
#61784 = ORIENTED_EDGE ( 'NONE', *, *, #16579, .T. ) ;
#61785 = CARTESIAN_POINT ( 'NONE',  ( 92.69370383062501162, -208.6684592857803011, 85.77989583420048803 ) ) ;
#61786 = AXIS2_PLACEMENT_3D ( 'NONE', #25158, #69175, #63543 ) ;
#61787 = SHAPE_DEFINITION_REPRESENTATION ( #26562, #33525 ) ;
#61788 = CARTESIAN_POINT ( 'NONE',  ( 62.50000000000000000, 0.000000000000000000, -270.0000000000000000 ) ) ;
#61789 = EDGE_CURVE ( 'NONE', #60050, #35038, #69856, .T. ) ;
#61790 = DIRECTION ( 'NONE',  ( -1.000000000000000000, 0.000000000000000000, 0.000000000000000000 ) ) ;
#61791 = DIRECTION ( 'NONE',  ( 0.000000000000000000, -0.3826834323650969427, 0.9238795325112838519 ) ) ;
#61792 = FACE_OUTER_BOUND ( 'NONE', #66601, .T. ) ;
#61793 = CARTESIAN_POINT ( 'NONE',  ( 0.000000000000000000, 0.000000000000000000, 0.000000000000000000 ) ) ;
#61794 = EDGE_CURVE ( 'NONE', #56516, #12353, #30913, .T. ) ;
#61795 = CARTESIAN_POINT ( 'NONE',  ( 93.67499999999999716, 87.70503267997126784, 85.10520833506762983 ) ) ;
#61796 = ADVANCED_FACE ( 'NONE', ( #4787, #55891 ), #54779, .T. ) ;
#61797 = CARTESIAN_POINT ( 'NONE',  ( -97.30629616937497417, -211.3315407142195852, 87.79072916753381151 ) ) ;
#61798 = CARTESIAN_POINT ( 'NONE',  ( -97.30629616937501680, 91.33154071421968467, 86.57364583420047666 ) ) ;
#61799 = VERTEX_POINT ( 'NONE', #27688 ) ;
#61801 = CARTESIAN_POINT ( 'NONE',  ( -97.30629616937501680, 91.33154071421968467, 88.31989583420046586 ) ) ;
#61800 = CARTESIAN_POINT ( 'NONE',  ( 96.15314808468748708, 88.00268892867053694, 87.94947916753380923 ) ) ;
#61802 = ORIENTED_EDGE ( 'NONE', *, *, #24273, .F. ) ;
#61803 = CARTESIAN_POINT ( 'NONE',  ( 12.50000000000000000, -132.5000000000000000, 40.00000000000000000 ) ) ;
#61804 = CIRCLE ( 'NONE', #29358, 37.49900000000001654 ) ;
#61805 = CARTESIAN_POINT ( 'NONE',  ( 11.99999999999999822, 0.000000000000000000, 0.000000000000000000 ) ) ;
#61806 = CIRCLE ( 'NONE', #38993, 16.00000000000000000 ) ;
#61807 = DIRECTION ( 'NONE',  ( -0.000000000000000000, -0.000000000000000000, 1.000000000000000000 ) ) ;
#61808 = PLANE ( 'NONE',  #69613 ) ;
#61809 = DIRECTION ( 'NONE',  ( -1.000000000000000000, -0.000000000000000000, 0.000000000000000000 ) ) ;
#61810 = DIRECTION ( 'NONE',  ( 1.000000000000000000, 0.000000000000000000, 0.000000000000000000 ) ) ;
#61811 = CARTESIAN_POINT ( 'NONE',  ( -3.000000000000000000, -3.948201729842038432, -23.21447184625298021 ) ) ;
#61812 = CARTESIAN_POINT ( 'NONE',  ( 10.00000000000000000, -40.65526001592664329, 71.21200624218782593 ) ) ;
#61813 = ORIENTED_EDGE ( 'NONE', *, *, #15121, .T. ) ;
#61814 = ORIENTED_EDGE ( 'NONE', *, *, #24892, .F. ) ;
#61815 = ADVANCED_FACE ( 'NONE', ( #26190 ), #10396, .F. ) ;
#61816 = CARTESIAN_POINT ( 'NONE',  ( -96.32500000000001705, 92.29496732002878900, 81.63916666666666799 ) ) ;
#61817 = CYLINDRICAL_SURFACE ( 'NONE', #73927, 77.49899999999999523 ) ;
#61818 = CYLINDRICAL_SURFACE ( 'NONE', #15357, 23.50000000000041922 ) ;
#61819 = DIRECTION ( 'NONE',  ( 0.000000000000000000, 1.000000000000000000, 1.224646799147353454E-16 ) ) ;
#61820 = PLANE ( 'NONE',  #44738 ) ;
#61821 = DIRECTION ( 'NONE',  ( -1.000000000000000000, -0.000000000000000000, 0.000000000000000000 ) ) ;
#61822 = CARTESIAN_POINT ( 'NONE',  ( 11.99999999999999822, 0.000000000000000000, 0.000000000000000000 ) ) ;
#61823 = DIRECTION ( 'NONE',  ( 0.000000000000000000, 0.000000000000000000, 1.000000000000000000 ) ) ;
#61824 = EDGE_LOOP ( 'NONE', ( #55832, #65640 ) ) ;
#61825 = CARTESIAN_POINT ( 'NONE',  ( -95.00000000000002842, 92.66308142843932671, 81.86406250086714920 ) ) ;
#61826 = AXIS2_PLACEMENT_3D ( 'NONE', #7786, #35982, #64564 ) ;
#61827 = DIRECTION ( 'NONE',  ( -0.02332147558787674158, -0.9997280174009349762, 0.000000000000000000 ) ) ;
#61828 = EDGE_CURVE ( 'NONE', #62864, #26970, #14548, .T. ) ;
#61829 = ADVANCED_FACE ( 'NONE', ( #38977, #21673 ), #43525, .F. ) ;
#61830 = CARTESIAN_POINT ( 'NONE',  ( -92.35000000000003695, 90.00000000000004263, 85.87249999999998806 ) ) ;
#61831 = CYLINDRICAL_SURFACE ( 'NONE', #19000, 31.99999999999999289 ) ;
#61832 = DIRECTION ( 'NONE',  ( -1.000000000000000000, -0.000000000000000000, 0.000000000000000000 ) ) ;
#61833 = LINE ( 'NONE', #49784, #43726 ) ;
#61834 = CARTESIAN_POINT ( 'NONE',  ( 11.99999999999999822, -28.89263327155693517, -71.91182617369219088 ) ) ;
#61835 = SURFACE_SIDE_STYLE ('',( #16705 ) ) ;
#61836 = CARTESIAN_POINT ( 'NONE',  ( 92.69370383062498320, 90.00000000000002842, 82.18156250086715886 ) ) ;
#61837 = CARTESIAN_POINT ( 'NONE',  ( -94.99999999999997158, -207.3369185715606307, 79.48281250086715488 ) ) ;
#61838 = CARTESIAN_POINT ( 'NONE',  ( -3.000000000000000000, 0.000000000000000000, -5.974599999999999689 ) ) ;
#61839 = EDGE_LOOP ( 'NONE', ( #41060, #21674 ) ) ;
#61840 = CARTESIAN_POINT ( 'NONE',  ( 92.35004305005914205, -208.4699969316842214, 81.13645661577282908 ) ) ;
#61841 = CARTESIAN_POINT ( 'NONE',  ( -94.99999999999997158, -206.9400435732949575, 75.87125000000000341 ) ) ;
#61842 = CARTESIAN_POINT ( 'NONE',  ( 92.35000000000000853, -209.9999831677331770, 78.64937441956426767 ) ) ;
#61843 = VECTOR ( 'NONE', #71653, 1000.000000000000000 ) ;
#61844 = CARTESIAN_POINT ( 'NONE',  ( -97.30629616937501680, 90.00000000000004263, 78.37156250086715659 ) ) ;
#61845 = CARTESIAN_POINT ( 'NONE',  ( 92.69370383062501162, -208.6684592857803011, 80.06489583420047040 ) ) ;
#61846 = ORIENTED_EDGE ( 'NONE', *, *, #34640, .F. ) ;
#61847 = CARTESIAN_POINT ( 'NONE',  ( -0.0004442498507136653329, 0.001194404164628348752, -70.59999999999999432 ) ) ;
#61848 = EDGE_LOOP ( 'NONE', ( #65698, #30337, #8892, #53578 ) ) ;
#61849 = AXIS2_PLACEMENT_3D ( 'NONE', #11260, #15669, #73534 ) ;
#61850 = FACE_OUTER_BOUND ( 'NONE', #38758, .T. ) ;
#61851 = CIRCLE ( 'NONE', #70239, 16.00000000000000000 ) ;
#61852 = ORIENTED_EDGE ( 'NONE', *, *, #61477, .T. ) ;
#61853 = FACE_OUTER_BOUND ( 'NONE', #21521, .T. ) ;
#61854 = VECTOR ( 'NONE', #37153, 1000.000000000000000 ) ;
#61855 = VERTEX_POINT ( 'NONE', #33308 ) ;
#61856 = VERTEX_POINT ( 'NONE', #4405 ) ;
#61857 = AXIS2_PLACEMENT_3D ( 'NONE', #72873, #51447, #73630 ) ;
#61858 = ORIENTED_EDGE ( 'NONE', *, *, #51088, .T. ) ;
#61859 = CARTESIAN_POINT ( 'NONE',  ( 95.00000000000000000, -212.6630814284392557, 75.35531250086715715 ) ) ;
#61860 = EDGE_LOOP ( 'NONE', ( #44930, #14346, #45427, #71389 ) ) ;
#61861 = CARTESIAN_POINT ( 'NONE',  ( -97.64999999999996305, -209.9999999999999716, 77.93499999999998806 ) ) ;
#61862 = CARTESIAN_POINT ( 'NONE',  ( 92.35000000000010800, -211.5299782133525071, 83.70291666666668107 ) ) ;
#61863 = CARTESIAN_POINT ( 'NONE',  ( 97.30629616937498838, 90.00000000000002842, 86.30906250086715659 ) ) ;
#61864 = CARTESIAN_POINT ( 'NONE',  ( 0.000000000000000000, 0.000000000000000000, -0.3851141460153411078 ) ) ;
#61865 = CARTESIAN_POINT ( 'NONE',  ( 95.00000000000000000, -206.9400435732949575, 79.68124999999999147 ) ) ;
#61866 = AXIS2_PLACEMENT_3D ( 'NONE', #21268, #32184, #2922 ) ;
#61867 = EDGE_CURVE ( 'NONE', #8597, #4038, #63351, .T. ) ;
#61868 = VERTEX_POINT ( 'NONE', #72427 ) ;
#61869 = ORIENTED_EDGE ( 'NONE', *, *, #32981, .F. ) ;
#61870 = EDGE_CURVE ( 'NONE', #73668, #9811, #20181, .T. ) ;
#61871 = ORIENTED_EDGE ( 'NONE', *, *, #41317, .T. ) ;
#61872 = ORIENTED_EDGE ( 'NONE', *, *, #64968, .F. ) ;
#61873 = CARTESIAN_POINT ( 'NONE',  ( -15.44521549751111422, -137.7748507232956001, 5.500000000000000000 ) ) ;
#61874 = SURFACE_STYLE_USAGE ( .BOTH. , #55484 ) ;
#61875 = CARTESIAN_POINT ( 'NONE',  ( 30.50000000000000000, -120.0000000000000000, 2.500000000000000000 ) ) ;
#61876 = EDGE_CURVE ( 'NONE', #63903, #28680, #72912, .T. ) ;
#61877 = VECTOR ( 'NONE', #53964, 1000.000000000000000 ) ;
#61878 = CARTESIAN_POINT ( 'NONE',  ( -93.33864827737279768, 88.39919842643631398, 74.79754476654878204 ) ) ;
#61879 = LINE ( 'NONE', #28385, #13788 ) ;
#61880 = DIRECTION ( 'NONE',  ( -1.000000000000000000, -0.000000000000000000, -0.000000000000000000 ) ) ;
#61881 = CARTESIAN_POINT ( 'NONE',  ( -2.499999999999973355, 65.00000000000000000, -290.0000000000000568 ) ) ;
#61883 = ORIENTED_EDGE ( 'NONE', *, *, #47118, .T. ) ;
#61882 = EDGE_CURVE ( 'NONE', #36423, #55652, #3139, .T. ) ;
#61884 = CARTESIAN_POINT ( 'NONE',  ( -96.32499999999996021, -212.2949673200287179, 81.93020833506763267 ) ) ;
#61885 = EDGE_LOOP ( 'NONE', ( #15579, #62947, #2738, #3302 ) ) ;
#61886 = CARTESIAN_POINT ( 'NONE',  ( -3.000000000000000000, 24.81905959214261514, 9.408202855044825341 ) ) ;
#61887 = ORIENTED_EDGE ( 'NONE', *, *, #72896, .F. ) ;
#61889 = CARTESIAN_POINT ( 'NONE',  ( -97.65000000000001990, 91.52997821335253548, 81.77145833506763495 ) ) ;
#61888 = CARTESIAN_POINT ( 'NONE',  ( 94.99999999999998579, 86.94004357329500010, 83.88812500173429498 ) ) ;
#61890 = EDGE_CURVE ( 'NONE', #61324, #39410, #59748, .T. ) ;
#61891 = ORIENTED_EDGE ( 'NONE', *, *, #15242, .T. ) ;
#61892 = CARTESIAN_POINT ( 'NONE',  ( 93.84685191531248449, 91.99731107132950569, 82.71072916753381321 ) ) ;
#61893 = DIRECTION ( 'NONE',  ( -1.000000000000000000, 0.000000000000000000, -0.000000000000000000 ) ) ;
#61894 = CARTESIAN_POINT ( 'NONE',  ( -97.64999999999996305, -209.9999678301198571, 82.45937388908916432 ) ) ;
#61895 = CARTESIAN_POINT ( 'NONE',  ( 8.700667342345820288, -98.11853780484867116, -5.500000000000000000 ) ) ;
#61896 = DIRECTION ( 'NONE',  ( 0.000000000000000000, 0.000000000000000000, 1.000000000000000000 ) ) ;
#61897 = DIRECTION ( 'NONE',  ( 0.000000000000000000, 0.000000000000000000, 1.000000000000000000 ) ) ;
#61898 = EDGE_LOOP ( 'NONE', ( #23843, #1920, #51495, #14245, #69875 ) ) ;
#61899 = CYLINDRICAL_SURFACE ( 'NONE', #20677, 2.649999999999999467 ) ;
#61900 = CARTESIAN_POINT ( 'NONE',  ( 0.000000000000000000, -15.33399622253540961, 80.55351364060584274 ) ) ;
#61901 = ORIENTED_EDGE ( 'NONE', *, *, #25121, .T. ) ;
#61902 = VERTEX_POINT ( 'NONE', #49131 ) ;
#61903 = ADVANCED_FACE ( 'NONE', ( #72061 ), #26568, .T. ) ;
#61904 = ADVANCED_FACE ( 'NONE', ( #66439 ), #14920, .F. ) ;
#61905 = DIRECTION ( 'NONE',  ( 0.000000000000000000, 0.8910065241883656784, 0.4539904997395511899 ) ) ;
#61906 = CARTESIAN_POINT ( 'NONE',  ( 10.00000000000000000, 0.000000000000000000, 0.000000000000000000 ) ) ;
#61907 = CARTESIAN_POINT ( 'NONE',  ( 15.00000000000000000, 8.688484142253932063, -21.88630264137371029 ) ) ;
#61908 = CARTESIAN_POINT ( 'NONE',  ( -94.99999999999997158, -207.3369185715606307, 80.11781250086714579 ) ) ;
#61909 = EDGE_LOOP ( 'NONE', ( #19036, #71630, #18399, #14239 ) ) ;
#61910 = AXIS2_PLACEMENT_3D ( 'NONE', #56259, #62665, #11139 ) ;
#61911 = DIRECTION ( 'NONE',  ( 0.000000000000000000, 0.000000000000000000, -1.000000000000000000 ) ) ;
#61912 = AXIS2_PLACEMENT_3D ( 'NONE', #4385, #5502, #17133 ) ;
#61913 = EDGE_LOOP ( 'NONE', ( #42109, #988, #16486, #5826, #58129, #1540, #37842, #48895 ) ) ;
#61914 = CARTESIAN_POINT ( 'NONE',  ( 10.00000000000000000, 0.000000000000000000, 0.000000000000000000 ) ) ;
#61915 = ADVANCED_FACE ( 'NONE', ( #66802 ), #32573, .T. ) ;
#61916 = EDGE_CURVE ( 'NONE', #7122, #55565, #34519, .T. ) ;
#61917 = DIRECTION ( 'NONE',  ( 0.000000000000000000, 0.000000000000000000, -1.000000000000000000 ) ) ;
#61918 = FACE_OUTER_BOUND ( 'NONE', #43137, .T. ) ;
#61919 = DIRECTION ( 'NONE',  ( 0.000000000000000000, 0.9723699203976773342, -0.2334453638559025601 ) ) ;
#61920 = LINE ( 'NONE', #72791, #42488 ) ;
#61921 = FACE_OUTER_BOUND ( 'NONE', #27062, .T. ) ;
#61922 = AXIS2_PLACEMENT_3D ( 'NONE', #39351, #56653, #4791 ) ;
#61923 = CARTESIAN_POINT ( 'NONE',  ( 10.00000000000000000, -35.47612816024539484, 22.48208911017487921 ) ) ;
#61924 = CARTESIAN_POINT ( 'NONE',  ( 11.99999999999999822, -46.54456581323847786, 59.03342792756247093 ) ) ;
#61925 = CARTESIAN_POINT ( 'NONE',  ( -97.64999999999996305, -209.9999999999999716, 76.66499999999999204 ) ) ;
#61926 = FACE_OUTER_BOUND ( 'NONE', #43591, .T. ) ;
#61927 = CIRCLE ( 'NONE', #72726, 16.00000000000000355 ) ;
#61928 = CARTESIAN_POINT ( 'NONE',  ( 92.35000000000000853, -209.9999999999999716, 83.01499999999998636 ) ) ;
#61929 = CARTESIAN_POINT ( 'NONE',  ( -89.99999999999998579, -116.0000000000000000, -40.00000000000002132 ) ) ;
#61930 = CARTESIAN_POINT ( 'NONE',  ( 7.103376864691351012E-17, -120.0000000000000000, -64.00000000000000000 ) ) ;
#61931 = CARTESIAN_POINT ( 'NONE',  ( 97.65000000000000568, 88.47002178664752137, 77.00895833506763211 ) ) ;
#61932 = EDGE_LOOP ( 'NONE', ( #65540, #50847, #16185, #54651 ) ) ;
#61933 = CARTESIAN_POINT ( 'NONE',  ( -92.69370383062505425, 88.66845928578038638, 79.74739583420047495 ) ) ;
#61934 = AXIS2_PLACEMENT_3D ( 'NONE', #58418, #42252, #47510 ) ;
#61935 = CARTESIAN_POINT ( 'NONE',  ( 10.00000000000000000, -6.555932627142143865, -37.01155633439065440 ) ) ;
#61936 = VERTEX_POINT ( 'NONE', #28050 ) ;
#61937 = DIRECTION ( 'NONE',  ( 0.000000000000000000, -0.7071067811865535679, 0.7071067811865413555 ) ) ;
#61938 = CARTESIAN_POINT ( 'NONE',  ( -26.49999999999739941, -119.9999999999996021, -65.00000000000069633 ) ) ;
#61939 = CARTESIAN_POINT ( 'NONE',  ( 11.99999999999999822, -55.20638768913797634, 51.02545421589302777 ) ) ;
#61940 = CARTESIAN_POINT ( 'NONE',  ( 92.35000000000000853, -209.9999999999999716, 85.55499999999999261 ) ) ;
#61941 = CARTESIAN_POINT ( 'NONE',  ( 93.84685191531251292, -211.9973110713294489, 76.57239583420049200 ) ) ;
#61942 = EDGE_LOOP ( 'NONE', ( #1982, #25172, #31327, #52368 ) ) ;
#61943 = EDGE_CURVE ( 'NONE', #43028, #46835, #58768, .T. ) ;
#61944 = VERTEX_POINT ( 'NONE', #35811 ) ;
#61945 = ADVANCED_FACE ( 'NONE', ( #56649 ), #52753, .T. ) ;
#61946 = CYLINDRICAL_SURFACE ( 'NONE', #69272, 26.50000000000552092 ) ;
#61947 = CARTESIAN_POINT ( 'NONE',  ( -6.112675177960399608, -145.7853679859090903, -2.500000000000000000 ) ) ;
#61948 = ADVANCED_FACE ( 'NONE', ( #12880 ), #27032, .F. ) ;
#61949 = PLANE ( 'NONE',  #26841 ) ;
#61950 = CARTESIAN_POINT ( 'NONE',  ( 10.00000000000000000, 65.58780272294129077, -36.73666225445822420 ) ) ;
#61951 = VECTOR ( 'NONE', #32468, 1000.000000000000000 ) ;
#61952 = DIRECTION ( 'NONE',  ( -1.000000000000000000, -0.000000000000000000, -0.000000000000000000 ) ) ;
#61953 = CARTESIAN_POINT ( 'NONE',  ( 95.00000000000000000, -206.9400435732949575, 87.93625000000000114 ) ) ;
#61954 = ADVANCED_FACE ( 'NONE', ( #16544 ), #32705, .F. ) ;
#61955 = ORIENTED_EDGE ( 'NONE', *, *, #59523, .F. ) ;
#61956 = DIRECTION ( 'NONE',  ( 0.000000000000000000, -0.9723699203976741146, -0.2334453638559160493 ) ) ;
#61957 = ORIENTED_EDGE ( 'NONE', *, *, #7418, .T. ) ;
#61958 = CIRCLE ( 'NONE', #22185, 82.00000000000000000 ) ;
#61959 = EDGE_LOOP ( 'NONE', ( #59339, #43703, #33333, #48963 ) ) ;
#61960 = PLANE ( 'NONE',  #54962 ) ;
#61961 =( NAMED_UNIT ( * ) SI_UNIT ( $, .STERADIAN. ) SOLID_ANGLE_UNIT ( ) );
#61962 = EDGE_CURVE ( 'NONE', #20422, #67440, #27442, .T. ) ;
#61963 = FACE_OUTER_BOUND ( 'NONE', #48263, .T. ) ;
#61964 = AXIS2_PLACEMENT_3D ( 'NONE', #32857, #38515, #21960 ) ;
#61965 = VERTEX_POINT ( 'NONE', #16173 ) ;
#61966 = CARTESIAN_POINT ( 'NONE',  ( -1.895993822078342774E-14, 1.063390998062931622E-14, -55.00000000000000000 ) ) ;
#61967 = CARTESIAN_POINT ( 'NONE',  ( 92.35000000000002274, -211.5299782133524502, 81.24229166840098060 ) ) ;
#61968 = CARTESIAN_POINT ( 'NONE',  ( 97.64999999999997726, 91.52997821335252127, 81.48041666666665606 ) ) ;
#61969 = ORIENTED_EDGE ( 'NONE', *, *, #33723, .T. ) ;
#61970 = DIRECTION ( 'NONE',  ( 0.000000000000000000, 0.000000000000000000, 1.000000000000000000 ) ) ;
#61971 = ORIENTED_EDGE ( 'NONE', *, *, #3101, .F. ) ;
#61972 = CARTESIAN_POINT ( 'NONE',  ( -92.35000000002592913, -210.0000117261698165, 82.77687459617060028 ) ) ;
#61973 = VECTOR ( 'NONE', #44897, 1000.000000000000227 ) ;
#61974 = VERTEX_POINT ( 'NONE', #44762 ) ;
#61975 = CARTESIAN_POINT ( 'NONE',  ( 0.000000000000000000, -10.30890764327441289, 81.34940948281332851 ) ) ;
#61976 =( BOUNDED_CURVE ( )  B_SPLINE_CURVE ( 2, ( #16712, #6186, #29084, #62207, #22349, #50542, #73465 ),
 .UNSPECIFIED., .F., .F. ) 
 B_SPLINE_CURVE_WITH_KNOTS ( ( 3, 2, 2, 3 ),
 ( 0.2963422021981254040, 0.3033979182579412681, 0.3104536837988239317, 0.3175094496506953856 ),
 .UNSPECIFIED. ) 
 CURVE ( )  GEOMETRIC_REPRESENTATION_ITEM ( )  RATIONAL_B_SPLINE_CURVE ( ( 0.9999981209241102231, 0.8660263433289724366, 1.000000000000000000, 0.8660254037844387076, 1.000000000000000000, 0.8660254037844387076, 1.000000000000000000 ) ) 
 REPRESENTATION_ITEM ( '' )  );
#61977 = CARTESIAN_POINT ( 'NONE',  ( -92.69370383062505425, 88.66845928578038638, 85.62114583420047609 ) ) ;
#61978 = EDGE_CURVE ( 'NONE', #6059, #16594, #28196, .T. ) ;
#61979 = CARTESIAN_POINT ( 'NONE',  ( 92.69370383062498320, 91.33154071421968467, 78.79489583420047438 ) ) ;
#61980 = ORIENTED_EDGE ( 'NONE', *, *, #68003, .F. ) ;
#61981 = CARTESIAN_POINT ( 'NONE',  ( -97.30629616937495996, -209.9999999999999716, 89.80156250086714920 ) ) ;
#61982 = DIRECTION ( 'NONE',  ( -1.000000000000000000, 0.000000000000000000, -0.000000000000000000 ) ) ;
#61983 = CARTESIAN_POINT ( 'NONE',  ( 97.64999999999989200, -211.5299782133525071, 85.81958333333332689 ) ) ;
#61984 = CYLINDRICAL_SURFACE ( 'NONE', #30005, 31.99999999999999289 ) ;
#61985 = VERTEX_POINT ( 'NONE', #72919 ) ;
#61986 = DIRECTION ( 'NONE',  ( 0.000000000000000000, 0.000000000000000000, 1.000000000000000000 ) ) ;
#61987 = CARTESIAN_POINT ( 'NONE',  ( -92.69370383062498320, -209.9999999999999716, 82.34031250086714238 ) ) ;
#61988 = ORIENTED_EDGE ( 'NONE', *, *, #72724, .T. ) ;
#61989 = COLOUR_RGB ( '', 0.09019608, 0.27058824, 0.51372549) ;
#61990 = ORIENTED_EDGE ( 'NONE', *, *, #13660, .F. ) ;
#61991 = CARTESIAN_POINT ( 'NONE',  ( 11.99999999999999822, -80.28980883073769803, 16.65972982744905551 ) ) ;
#61992 = EDGE_CURVE ( 'NONE', #60373, #71222, #36869, .T. ) ;
#61993 = ORIENTED_EDGE ( 'NONE', *, *, #35034, .F. ) ;
#61994 = ADVANCED_FACE ( 'NONE', ( #4922 ), #4174, .F. ) ;
#61995 = CARTESIAN_POINT ( 'NONE',  ( 96.32499999999998863, 87.70503267997126784, 78.14666666666667538 ) ) ;
#61996 = DIRECTION ( 'NONE',  ( -0.000000000000000000, 0.5000000000000031086, -0.8660254037844369313 ) ) ;
#61997 = ORIENTED_EDGE ( 'NONE', *, *, #28923, .F. ) ;
#61998 = CARTESIAN_POINT ( 'NONE',  ( -93.84685191531247028, -211.9973110713294489, 76.51947916753380241 ) ) ;
#61999 = VERTEX_POINT ( 'NONE', #22192 ) ;
#62000 = CARTESIAN_POINT ( 'NONE',  ( -93.67500000000003979, 87.70503267997129626, 86.40166666666667084 ) ) ;
#62001 = DIRECTION ( 'NONE',  ( 0.000000000000000000, 0.000000000000000000, -1.000000000000000000 ) ) ;
#62002 = CARTESIAN_POINT ( 'NONE',  ( 0.000000000000000000, -132.5000000000000000, -40.00000000000000711 ) ) ;
#62003 = CARTESIAN_POINT ( 'NONE',  ( 0.000000000000000000, 37.22597642581158084, -5.202137450156524068 ) ) ;
#62004 = CARTESIAN_POINT ( 'NONE',  ( 15.00000000000000000, 6.762365576493647445, 25.66652317338391498 ) ) ;
#62005 = CLOSED_SHELL ( 'NONE', ( #40922, #28355, #32777, #32136, #68758, #64035, #40748, #57862 ) ) ;
#62006 = CARTESIAN_POINT ( 'NONE',  ( -10.43921258969510824, -98.89258801967538659, -5.500000000000000000 ) ) ;
#62007 = CARTESIAN_POINT ( 'NONE',  ( 10.00000000000000000, -12.93880638057369659, 76.41127070299266677 ) ) ;
#62008 = DIRECTION ( 'NONE',  ( 0.000000000000000000, 0.000000000000000000, -1.000000000000000000 ) ) ;
#62009 = DIRECTION ( 'NONE',  ( -0.000000000000000000, -0.000000000000000000, -1.000000000000000000 ) ) ;
#62010 = CARTESIAN_POINT ( 'NONE',  ( 10.00000000000000000, -68.67312586194971402, -35.91791733033549860 ) ) ;
#62011 = DIRECTION ( 'NONE',  ( 0.000000000000000000, 0.5877852522924743583, -0.8090169943749466741 ) ) ;
#62012 = CARTESIAN_POINT ( 'NONE',  ( 93.67499999999999716, 87.70503267997126784, 86.37520833506764006 ) ) ;
#62013 = FACE_OUTER_BOUND ( 'NONE', #65384, .T. ) ;
#62014 = CARTESIAN_POINT ( 'NONE',  ( 97.64999999999993463, 88.47002178664747873, 77.56458333333333144 ) ) ;
#62015 = DIRECTION ( 'NONE',  ( 0.000000000000000000, -0.3826834323650970537, 0.9238795325112838519 ) ) ;
#62016 = MANIFOLD_SOLID_BREP ( 'Cut-Extrude-Thin1', #3209 ) ;
#62017 = CIRCLE ( 'NONE', #17559, 31.99999999999999289 ) ;
#62018 = DIRECTION ( 'NONE',  ( -1.000000000000000000, 0.000000000000000000, -0.000000000000000000 ) ) ;
#62019 = LINE ( 'NONE', #60269, #32543 ) ;
#62020 = PLANE ( 'NONE',  #41303 ) ;
#62021 = CYLINDRICAL_SURFACE ( 'NONE', #63520, 77.49899999999999523 ) ;
#62022 = CIRCLE ( 'NONE', #23581, 31.99999999999999645 ) ;
#62023 = CARTESIAN_POINT ( 'NONE',  ( -93.67499999999998295, -212.2949673200287179, 85.13166666666666060 ) ) ;
#62024 = CIRCLE ( 'NONE', #71606, 82.00000000000000000 ) ;
#62025 = ADVANCED_FACE ( 'NONE', ( #68807 ), #56023, .T. ) ;
#62026 = CARTESIAN_POINT ( 'NONE',  ( -92.35000000000007958, 88.94459177146599416, 75.04099707143593889 ) ) ;
#62027 = PRODUCT ( 'small gear_ISO - Spur gear 2M 40T 20PA 10FW ---S40A75H50L20.0N', 'small gear_ISO - Spur gear 2M 40T 20PA 10FW ---S40A75H50L20.0N', '', ( #17029 ) ) ;
#62028 = VECTOR ( 'NONE', #7991, 1000.000000000000000 ) ;
#62029 = ORIENTED_EDGE ( 'NONE', *, *, #59020, .T. ) ;
#62030 = DIRECTION ( 'NONE',  ( 0.000000000000000000, -0.4539904997395542430, 0.8910065241883641241 ) ) ;
#62031 = DIRECTION ( 'NONE',  ( 0.000000000000000000, 1.000000000000000000, -9.787530781167596740E-16 ) ) ;
#62032 = CARTESIAN_POINT ( 'NONE',  ( -2.499999999999968914, 79.99999999999998579, -189.9999999999999147 ) ) ;
#62033 = CARTESIAN_POINT ( 'NONE',  ( -18.24502636017238899, -100.7225776329765665, 5.500000000000000000 ) ) ;
#62034 = CARTESIAN_POINT ( 'NONE',  ( 92.69370383062501162, -211.3315407142195852, 88.58447916753382856 ) ) ;
#62035 = ORIENTED_EDGE ( 'NONE', *, *, #10796, .F. ) ;
#62036 = ADVANCED_FACE ( 'NONE', ( #44382 ), #73678, .T. ) ;
#62037 = ORIENTED_EDGE ( 'NONE', *, *, #16061, .F. ) ;
#62038 = EDGE_CURVE ( 'NONE', #25707, #63817, #52984, .T. ) ;
#62039 = DIRECTION ( 'NONE',  ( -1.000000000000000000, 0.000000000000000000, 0.000000000000000000 ) ) ;
#62040 = ORIENTED_EDGE ( 'NONE', *, *, #46683, .F. ) ;
#62041 = CARTESIAN_POINT ( 'NONE',  ( 11.99999999999999822, 11.30684508768339569, 76.66974797899841576 ) ) ;
#62042 = CARTESIAN_POINT ( 'NONE',  ( 95.00000000000000000, -207.3369185715606307, 78.05406250086714692 ) ) ;
#62043 = VERTEX_POINT ( 'NONE', #18754 ) ;
#62044 = CARTESIAN_POINT ( 'NONE',  ( 96.15314808468748708, -208.0026889286704943, 82.60489583420049087 ) ) ;
#62045 = EDGE_CURVE ( 'NONE', #47680, #18460, #24959, .T. ) ;
#62046 = ADVANCED_FACE ( 'NONE', ( #18031, #57893 ), #47703, .T. ) ;
#62047 = EDGE_LOOP ( 'NONE', ( #32644, #17044, #672, #17457 ) ) ;
#62048 = DIRECTION ( 'NONE',  ( 1.000000000000000000, 0.000000000000000000, -0.000000000000000000 ) ) ;
#62049 = EDGE_LOOP ( 'NONE', ( #3941, #53700, #67752, #21331 ) ) ;
#62050 = CARTESIAN_POINT ( 'NONE',  ( -95.00000000000002842, 87.33691857156074434, 75.35531250086715715 ) ) ;
#62051 = CARTESIAN_POINT ( 'NONE',  ( 10.00000000000000000, 63.18004540533029001, 44.88180994100400767 ) ) ;
#62052 = ORIENTED_EDGE ( 'NONE', *, *, #4809, .T. ) ;
#62053 = CARTESIAN_POINT ( 'NONE',  ( 92.34999999999989484, 91.52997821335246442, 86.13708333333332234 ) ) ;
#62054 = DIRECTION ( 'NONE',  ( 0.000000000000000000, 0.000000000000000000, 1.000000000000000000 ) ) ;
#62055 = EDGE_LOOP ( 'NONE', ( #71059, #57247, #30398, #30404 ) ) ;
#62056 = CARTESIAN_POINT ( 'NONE',  ( 10.00000000000000000, -37.58145647212455032, 0.6853352020789044152 ) ) ;
#62057 = EDGE_LOOP ( 'NONE', ( #12016, #37840, #12467, #11966 ) ) ;
#62058 = CARTESIAN_POINT ( 'NONE',  ( 10.00000000000000000, 0.000000000000000000, 0.000000000000000000 ) ) ;
#62059 = EDGE_CURVE ( 'NONE', #55579, #38385, #12927, .T. ) ;
#62060 = AXIS2_PLACEMENT_3D ( 'NONE', #10860, #46925, #33788 ) ;
#62061 = VERTEX_POINT ( 'NONE', #13115 ) ;
#62062 = CIRCLE ( 'NONE', #66831, 77.49899999999999523 ) ;
#62063 = ORIENTED_EDGE ( 'NONE', *, *, #72382, .F. ) ;
#62064 = ORIENTED_EDGE ( 'NONE', *, *, #59169, .T. ) ;
#62065 = CARTESIAN_POINT ( 'NONE',  ( 96.15314808468748708, -208.0026889286704943, 75.46114583420047950 ) ) ;
#62066 = DIRECTION ( 'NONE',  ( -0.000000000000000000, -0.000000000000000000, 1.000000000000000000 ) ) ;
#62067 = VERTEX_POINT ( 'NONE', #36053 ) ;
#62068 = VERTEX_POINT ( 'NONE', #17660 ) ;
#62069 = VECTOR ( 'NONE', #13975, 1000.000000000000000 ) ;
#62070 = ORIENTED_EDGE ( 'NONE', *, *, #15627, .T. ) ;
#62071 = VECTOR ( 'NONE', #6976, 1000.000000000000000 ) ;
#62072 = CARTESIAN_POINT ( 'NONE',  ( 0.000000000000000000, -89.50000000000000000, -2.500000000000000000 ) ) ;
#62073 = CARTESIAN_POINT ( 'NONE',  ( 97.64999999999999147, -209.9999999999999716, 78.88750000000000284 ) ) ;
#62074 = CARTESIAN_POINT ( 'NONE',  ( -95.00000000000002842, 86.94004357329504273, 89.52375000000000682 ) ) ;
#62075 = EDGE_CURVE ( 'NONE', #13574, #67492, #71741, .T. ) ;
#62076 = ORIENTED_EDGE ( 'NONE', *, *, #331, .F. ) ;
#62077 = VECTOR ( 'NONE', #58209, 1000.000000000000000 ) ;
#62078 = CARTESIAN_POINT ( 'NONE',  ( 97.30629616937498838, 91.33154071421968467, 75.40822916753381833 ) ) ;
#62079 = ORIENTED_EDGE ( 'NONE', *, *, #73226, .F. ) ;
#62080 = DIRECTION ( 'NONE',  ( 0.000000000000000000, 0.000000000000000000, 1.000000000000000000 ) ) ;
#62081 = CARTESIAN_POINT ( 'NONE',  ( -92.69370383062498320, -209.9999999999999716, 86.78531250086714977 ) ) ;
#62082 = ORIENTED_EDGE ( 'NONE', *, *, #41022, .F. ) ;
#62083 = EDGE_CURVE ( 'NONE', #14143, #58563, #10799, .T. ) ;
#62084 = CYLINDRICAL_SURFACE ( 'NONE', #38605, 12.49999999999999645 ) ;
#62086 = AXIS2_PLACEMENT_3D ( 'NONE', #11606, #50725, #17632 ) ;
#62085 = DIRECTION ( 'NONE',  ( 1.000000000000000000, 0.000000000000000000, 0.000000000000000000 ) ) ;
#62087 = LINE ( 'NONE', #33117, #24862 ) ;
#62088 = CARTESIAN_POINT ( 'NONE',  ( -93.84685191531247028, -211.9973110713294489, 79.05947916753380866 ) ) ;
#62089 = CARTESIAN_POINT ( 'NONE',  ( -97.64999999999996305, -209.9999999999999716, 89.44437500173430067 ) ) ;
#62090 = DIRECTION ( 'NONE',  ( -1.000000000000000000, 0.000000000000000000, 0.000000000000000000 ) ) ;
#62091 = VECTOR ( 'NONE', #61575, 1000.000000000000000 ) ;
#62092 = VERTEX_POINT ( 'NONE', #58613 ) ;
#62093 = DIRECTION ( 'NONE',  ( -0.08130631524010117905, 0.9966891607226784355, 0.000000000000000000 ) ) ;
#62094 = FACE_OUTER_BOUND ( 'NONE', #70699, .T. ) ;
#62095 = DIRECTION ( 'NONE',  ( -0.6064928550163533050, -0.7950889364178781449, 0.000000000000000000 ) ) ;
#62096 = CARTESIAN_POINT ( 'NONE',  ( -92.69370383062502583, 88.66845928578038638, 82.92239583420045790 ) ) ;
#62097 = CARTESIAN_POINT ( 'NONE',  ( 10.00000000000000000, 0.000000000000000000, 0.000000000000000000 ) ) ;
#62098 = DIRECTION ( 'NONE',  ( 0.000000000000000000, -0.07845909572783058006, -0.9969173337331290741 ) ) ;
#62099 = ORIENTED_EDGE ( 'NONE', *, *, #10580, .F. ) ;
#62100 = CARTESIAN_POINT ( 'NONE',  ( 11.99999999999999822, 0.000000000000000000, 0.000000000000000000 ) ) ;
#62101 = CARTESIAN_POINT ( 'NONE',  ( -2.500000000000012879, -65.00000000000000000, -290.0000000000000568 ) ) ;
#62102 = LINE ( 'NONE', #22247, #4570 ) ;
#62103 = CARTESIAN_POINT ( 'NONE',  ( 10.00000000000000000, -37.22597642581153821, -5.202137450156795850 ) ) ;
#62104 = CARTESIAN_POINT ( 'NONE',  ( 96.92442009029420547, -211.8218417373832096, 75.00000000000001421 ) ) ;
#62105 = DIRECTION ( 'NONE',  ( -1.000000000000000000, -0.000000000000000000, -0.000000000000000000 ) ) ;
#62106 = CARTESIAN_POINT ( 'NONE',  ( -92.69370383062498320, -211.3315407142195852, 78.00114583420049996 ) ) ;
#62107 = CARTESIAN_POINT ( 'NONE',  ( 5.999999999999999112, 46.11716303203283474, -67.80270845531839541 ) ) ;
#62108 = EDGE_CURVE ( 'NONE', #73384, #39400, #69399, .T. ) ;
#62109 = ORIENTED_EDGE ( 'NONE', *, *, #41430, .T. ) ;
#62110 = STYLED_ITEM ( 'NONE', ( #67309 ), #62016 ) ;
#62111 = PLANE ( 'NONE',  #23875 ) ;
#62112 = LINE ( 'NONE', #68870, #8220 ) ;
#62113 = DIRECTION ( 'NONE',  ( -1.000000000000000000, -0.000000000000000000, -0.000000000000000000 ) ) ;
#62114 = CIRCLE ( 'NONE', #28507, 15.99999999999999822 ) ;
#62115 = ORIENTED_EDGE ( 'NONE', *, *, #55617, .F. ) ;
#62116 = DIRECTION ( 'NONE',  ( 0.000000000000000000, -0.9135454576426009776, -0.4067366430758000417 ) ) ;
#62117 = CYLINDRICAL_SURFACE ( 'NONE', #65456, 31.99999999999998579 ) ;
#62118 = EDGE_CURVE ( 'NONE', #64733, #32803, #35737, .T. ) ;
#62119 = CIRCLE ( 'NONE', #9299, 82.00000000000000000 ) ;
#62120 = CIRCLE ( 'NONE', #42910, 77.49900000000002365 ) ;
#62121 = EDGE_CURVE ( 'NONE', #56423, #62654, #35672, .T. ) ;
#62122 = DIRECTION ( 'NONE',  ( -1.000000000000000000, -0.000000000000000000, -0.000000000000000000 ) ) ;
#62123 = ORIENTED_EDGE ( 'NONE', *, *, #35476, .F. ) ;
#62124 = CARTESIAN_POINT ( 'NONE',  ( 10.00000000000000000, -75.16055320797016748, -18.89407956138335365 ) ) ;
#62125 = DIRECTION ( 'NONE',  ( 0.000000000000000000, 0.000000000000000000, 1.000000000000000000 ) ) ;
#62126 = ORIENTED_EDGE ( 'NONE', *, *, #42222, .T. ) ;
#62127 = CARTESIAN_POINT ( 'NONE',  ( 96.15314808468748708, -208.0026889286704943, 89.43114583420047836 ) ) ;
#62128 = CARTESIAN_POINT ( 'NONE',  ( 0.000000000000000000, 32.34446384429971033, 26.79245525562726371 ) ) ;
#62129 = VERTEX_POINT ( 'NONE', #52236 ) ;
#62130 = DIRECTION ( 'NONE',  ( 0.000000000000000000, -0.9238795325112821866, -0.3826834323651006065 ) ) ;
#62131 = ADVANCED_FACE ( 'NONE', ( #6033 ), #19131, .T. ) ;
#62132 = ORIENTED_EDGE ( 'NONE', *, *, #23360, .F. ) ;
#62133 = CARTESIAN_POINT ( 'NONE',  ( 10.00000000000000000, -4.992566952384716927, -37.16516213103282951 ) ) ;
#62134 = EDGE_LOOP ( 'NONE', ( #54347, #61236, #26213, #60118, #9729, #13305 ) ) ;
#62135 = CARTESIAN_POINT ( 'NONE',  ( -97.64999999999994884, -209.9999762675147110, 79.91937418090952860 ) ) ;
#62136 = ORIENTED_EDGE ( 'NONE', *, *, #6807, .F. ) ;
#62137 = VERTEX_POINT ( 'NONE', #415 ) ;
#62138 = ORIENTED_EDGE ( 'NONE', *, *, #47603, .T. ) ;
#62139 = DIRECTION ( 'NONE',  ( -1.000000000000000000, 0.000000000000000000, 0.000000000000000000 ) ) ;
#62140 = VERTEX_POINT ( 'NONE', #23308 ) ;
#62141 = EDGE_CURVE ( 'NONE', #65921, #17019, #780, .T. ) ;
#62142 = ORIENTED_EDGE ( 'NONE', *, *, #4117, .F. ) ;
#62143 = CARTESIAN_POINT ( 'NONE',  ( 97.30629616937498838, 91.33154071421968467, 78.10697916753383652 ) ) ;
#62144 = CARTESIAN_POINT ( 'NONE',  ( 0.000000000000000000, 0.000000000000000000, 0.000000000000000000 ) ) ;
#62145 = EDGE_CURVE ( 'NONE', #17733, #19308, #11749, .T. ) ;
#62146 = DIRECTION ( 'NONE',  ( 0.000000000000000000, 0.000000000000000000, 1.000000000000000000 ) ) ;
#62147 = ORIENTED_EDGE ( 'NONE', *, *, #18442, .F. ) ;
#62148 = ORIENTED_EDGE ( 'NONE', *, *, #2065, .F. ) ;
#62149 = ORIENTED_EDGE ( 'NONE', *, *, #29114, .T. ) ;
#62150 = DIRECTION ( 'NONE',  ( 0.000000000000000000, 0.000000000000000000, 1.000000000000000000 ) ) ;
#62152 = VERTEX_POINT ( 'NONE', #35322 ) ;
#62151 = EDGE_CURVE ( 'NONE', #19511, #68424, #8166, .T. ) ;
#62153 = CARTESIAN_POINT ( 'NONE',  ( 92.69370383062501162, -211.3315407142195852, 83.98072916753380923 ) ) ;
#62154 = CARTESIAN_POINT ( 'NONE',  ( 95.00000000002610534, 89.99999999999901945, 102.7500000000000142 ) ) ;
#62155 = LINE ( 'NONE', #11018, #3003 ) ;
#62156 = CARTESIAN_POINT ( 'NONE',  ( -21.67772167707813935, -110.8034581014852762, -2.500000000000000000 ) ) ;
#62157 = CARTESIAN_POINT ( 'NONE',  ( -97.65000000000001990, 89.99999071025123953, 78.01437532303467037 ) ) ;
#62158 = DIRECTION ( 'NONE',  ( -1.000000000000000000, 0.000000000000000000, -0.000000000000000000 ) ) ;
#62159 = DIRECTION ( 'NONE',  ( 0.000000000000000000, 0.000000000000000000, -1.000000000000000000 ) ) ;
#62160 = CARTESIAN_POINT ( 'NONE',  ( 5.999999999999999112, -33.71516098798685590, -74.74816331893465815 ) ) ;
#62161 = CARTESIAN_POINT ( 'NONE',  ( -96.15314808468745866, -211.9973110713294489, 86.57364583420047666 ) ) ;
#62162 = CARTESIAN_POINT ( 'NONE',  ( -96.15314808468751551, 88.00268892867056536, 84.82739583420048746 ) ) ;
#62163 = ADVANCED_FACE ( 'NONE', ( #6749 ), #24053, .T. ) ;
#62164 = ORIENTED_EDGE ( 'NONE', *, *, #49463, .T. ) ;
#62166 = CARTESIAN_POINT ( 'NONE',  ( -97.30629616937501680, 90.00000000000004263, 85.19781250086714408 ) ) ;
#62165 = CARTESIAN_POINT ( 'NONE',  ( 93.84685191531248449, 88.00268892867053694, 87.20864583420046756 ) ) ;
#62167 = VERTEX_POINT ( 'NONE', #36788 ) ;
#62168 = CYLINDRICAL_SURFACE ( 'NONE', #19053, 82.00000000000000000 ) ;
#62169 = CIRCLE ( 'NONE', #22555, 82.00000000000000000 ) ;
#62170 = CARTESIAN_POINT ( 'NONE',  ( 10.00000000000000000, 0.000000000000000000, 0.000000000000000000 ) ) ;
#62171 = CARTESIAN_POINT ( 'NONE',  ( 10.00000000000000000, 74.18225833017889670, 34.94270380257666631 ) ) ;
#62172 = CARTESIAN_POINT ( 'NONE',  ( 0.000000000000000000, 8.688484142254221609, -21.88630264137359660 ) ) ;
#62173 = CARTESIAN_POINT ( 'NONE',  ( -97.30629616937497417, -208.6684592857803295, 88.31989583420048007 ) ) ;
#62174 = AXIS2_PLACEMENT_3D ( 'NONE', #6262, #67924, #73545 ) ;
#62175 = CARTESIAN_POINT ( 'NONE',  ( 4.999999999999999112, 10.41901085202135491, -40.68715046381917944 ) ) ;
#62176 = DIRECTION ( 'NONE',  ( 1.000000000000000000, 0.000000000000000000, 0.000000000000000000 ) ) ;
#62177 = CARTESIAN_POINT ( 'NONE',  ( 0.000000000000000000, -4.992566952384716927, -37.16516213103282951 ) ) ;
#62178 = DIRECTION ( 'NONE',  ( -1.000000000000000000, 0.000000000000000000, -0.000000000000000000 ) ) ;
#62179 = ORIENTED_EDGE ( 'NONE', *, *, #33106, .F. ) ;
#62180 = ORIENTED_EDGE ( 'NONE', *, *, #51442, .F. ) ;
#62181 = CARTESIAN_POINT ( 'NONE',  ( -97.65000000000001990, 91.52997821335253548, 81.05708333333333826 ) ) ;
#62182 = DIRECTION ( 'NONE',  ( 0.000000000000000000, -1.000000000000000000, -1.040834085586084730E-14 ) ) ;
#62183 = DIRECTION ( 'NONE',  ( -1.000000000000000000, -0.000000000000000000, 0.000000000000000000 ) ) ;
#62184 = DIRECTION ( 'NONE',  ( 0.000000000000000000, 0.000000000000000000, 1.000000000000000000 ) ) ;
#62185 = CARTESIAN_POINT ( 'NONE',  ( -97.64999999978466860, 90.00002100773832581, 79.91868729552945183 ) ) ;
#62186 = DIRECTION ( 'NONE',  ( 1.000000000000000000, 0.000000000000000000, 0.000000000000000000 ) ) ;
#62187 = LINE ( 'NONE', #17067, #58954 ) ;
#62188 =( BOUNDED_CURVE ( )  B_SPLINE_CURVE ( 2, ( #8810, #31729, #54673, #71951, #43419, #37761, #33582 ),
 .UNSPECIFIED., .F., .F. ) 
 B_SPLINE_CURVE_WITH_KNOTS ( ( 3, 2, 2, 3 ),
 ( 0.1458333333333334536, 0.1527777777777778734, 0.1597222222222222654, 0.1666666666666666852 ),
 .UNSPECIFIED. ) 
 CURVE ( )  GEOMETRIC_REPRESENTATION_ITEM ( )  RATIONAL_B_SPLINE_CURVE ( ( 0.9999999999999978906, 0.8660254037844408170, 1.000000000000000000, 0.8660254037844387076, 1.000000000000000000, 0.8660254037844381525, 1.000000000000000444 ) ) 
 REPRESENTATION_ITEM ( '' )  );
#62189 = DIRECTION ( 'NONE',  ( 0.000000000000000000, -0.9876883405951393247, 0.1564344650402207382 ) ) ;
#62190 = VERTEX_POINT ( 'NONE', #25879 ) ;
#62191 = CARTESIAN_POINT ( 'NONE',  ( -97.30629616937501680, 91.33154071421968467, 83.23989583420046756 ) ) ;
#62192 = DIRECTION ( 'NONE',  ( 0.6516173805718058487, -0.7585478161175724932, 0.000000000000000000 ) ) ;
#62193 = DIRECTION ( 'NONE',  ( 1.000000000000000000, -0.000000000000000000, -0.000000000000000000 ) ) ;
#62194 = AXIS2_PLACEMENT_3D ( 'NONE', #59270, #7764, #29939 ) ;
#62195 = CARTESIAN_POINT ( 'NONE',  ( -7.670864526094549163, -97.73662565058241114, 2.500000000000000000 ) ) ;
#62196 = DIRECTION ( 'NONE',  ( 0.000000000000000000, -0.9945218953682742891, 0.1045284632676436315 ) ) ;
#62197 = AXIS2_PLACEMENT_3D ( 'NONE', #28485, #34501, #35272 ) ;
#62198 = LINE ( 'NONE', #43807, #18474 ) ;
#62199 = CARTESIAN_POINT ( 'NONE',  ( 10.00000000000000000, 9.188173127307898369, -40.98264845739739570 ) ) ;
#62200 = VECTOR ( 'NONE', #46873, 1000.000000000000000 ) ;
#62201 = AXIS2_PLACEMENT_3D ( 'NONE', #11326, #62867, #56472 ) ;
#62202 = AXIS2_PLACEMENT_3D ( 'NONE', #30930, #53878, #43720 ) ;
#62203 =( BOUNDED_CURVE ( )  B_SPLINE_CURVE ( 2, ( #26029, #61372, #14751, #26405, #20760, #10222, #66277, #60987, #32770 ),
 .UNSPECIFIED., .F., .F. ) 
 B_SPLINE_CURVE_WITH_KNOTS ( ( 3, 2, 2, 2, 3 ),
 ( 0.8678591737214816915, 0.8749149270694133174, 0.8819706926102951483, 0.8890264581511769792, 0.8890265259358468564 ),
 .UNSPECIFIED. ) 
 CURVE ( )  GEOMETRIC_REPRESENTATION_ITEM ( )  RATIONAL_B_SPLINE_CURVE ( ( 1.000000000000000000, 0.8660254037844387076, 1.000000000000000000, 0.8660254037844387076, 1.000000000000000000, 0.8660254037844387076, 1.000000000000000000, 0.9999987129073762970, 0.9999974258394828119 ) ) 
 REPRESENTATION_ITEM ( '' )  );
#62204 = CARTESIAN_POINT ( 'NONE',  ( 93.84685191531248449, 91.99731107132950569, 80.17072916753382117 ) ) ;
#62205 = ADVANCED_FACE ( 'NONE', ( #14599 ), #13493, .T. ) ;
#62206 = CARTESIAN_POINT ( 'NONE',  ( -92.69370383062498320, -209.9999999999999716, 79.32406250086715715 ) ) ;
#62207 = CARTESIAN_POINT ( 'NONE',  ( -95.00000000000002842, 93.05995642670504253, 84.84062500173429555 ) ) ;
#62208 = ORIENTED_EDGE ( 'NONE', *, *, #51793, .T. ) ;
#62209 = DIRECTION ( 'NONE',  ( -1.000000000000000000, -0.000000000000000000, 0.000000000000000000 ) ) ;
#62210 = LINE ( 'NONE', #68600, #20200 ) ;
#62211 = EDGE_CURVE ( 'NONE', #68341, #13137, #54099, .T. ) ;
#62212 = CARTESIAN_POINT ( 'NONE',  ( 10.00000000000000000, -59.46389618801999433, 49.70050353004867816 ) ) ;
#62213 = EDGE_CURVE ( 'NONE', #71356, #44790, #59804, .T. ) ;
#62214 = EDGE_CURVE ( 'NONE', #26369, #38741, #965, .T. ) ;
#62215 = CARTESIAN_POINT ( 'NONE',  ( -97.30629616937501680, 91.33154071421968467, 79.58864583420049144 ) ) ;
#62216 = CARTESIAN_POINT ( 'NONE',  ( 93.84685191531251292, -211.9973110713294489, 79.58864583420047722 ) ) ;
#62217 = EDGE_LOOP ( 'NONE', ( #38391, #57319, #54123, #55971 ) ) ;
#62218 = CARTESIAN_POINT ( 'NONE',  ( 5.000000000000000000, -63.97538442413390669, -51.29473840253292849 ) ) ;
#62219 = ORIENTED_EDGE ( 'NONE', *, *, #737, .F. ) ;
#62220 = ADVANCED_FACE ( 'NONE', ( #8217 ), #20617, .F. ) ;
#62221 = AXIS2_PLACEMENT_3D ( 'NONE', #23578, #57802, #58913 ) ;
#62222 = LINE ( 'NONE', #10708, #12350 ) ;
#62223 = ORIENTED_EDGE ( 'NONE', *, *, #71700, .F. ) ;
#62224 = AXIS2_PLACEMENT_3D ( 'NONE', #27968, #4698, #68206 ) ;
#62225 = AXIS2_PLACEMENT_3D ( 'NONE', #7077, #1850, #52944 ) ;
#62226 = LINE ( 'NONE', #74230, #59783 ) ;
#62227 = VECTOR ( 'NONE', #58018, 1000.000000000000000 ) ;
#62228 = VERTEX_POINT ( 'NONE', #49181 ) ;
#62229 = ORIENTED_EDGE ( 'NONE', *, *, #63003, .T. ) ;
#62230 = VECTOR ( 'NONE', #55540, 1000.000000000000000 ) ;
#62231 = EDGE_LOOP ( 'NONE', ( #6670, #44378 ) ) ;
#62232 = CARTESIAN_POINT ( 'NONE',  ( 97.30629616937498838, -208.6684592857803295, 75.56697916753383026 ) ) ;
#62233 = ORIENTED_EDGE ( 'NONE', *, *, #4703, .T. ) ;
#62234 = CARTESIAN_POINT ( 'NONE',  ( 0.000000000000000000, -2.956366410621191765, 75.11725578898467859 ) ) ;
#62235 = FACE_OUTER_BOUND ( 'NONE', #51400, .T. ) ;
#62236 = CARTESIAN_POINT ( 'NONE',  ( 93.84685191531248449, 91.99731107132950569, 87.79072916753381151 ) ) ;
#62237 = DIRECTION ( 'NONE',  ( -0.3853207896976523772, 0.9227826878668550226, 0.000000000000000000 ) ) ;
#62238 = CARTESIAN_POINT ( 'NONE',  ( 96.32499999999998863, -207.7050326799711968, 76.45333333333333314 ) ) ;
#62239 = EDGE_LOOP ( 'NONE', ( #71367, #43143, #13575, #14249 ) ) ;
#62241 = ORIENTED_EDGE ( 'NONE', *, *, #38258, .T. ) ;
#62240 = VECTOR ( 'NONE', #56938, 1000.000000000000000 ) ;
#62242 = ORIENTED_EDGE ( 'NONE', *, *, #44509, .F. ) ;
#62243 = ORIENTED_EDGE ( 'NONE', *, *, #72124, .F. ) ;
#62244 = DIRECTION ( 'NONE',  ( -0.000000000000000000, -0.000000000000000000, -1.000000000000000000 ) ) ;
#62245 = EDGE_CURVE ( 'NONE', #72136, #11546, #62169, .T. ) ;
#62246 = EDGE_CURVE ( 'NONE', #23563, #62167, #25511, .T. ) ;
#62247 = CIRCLE ( 'NONE', #53801, 82.00000000000000000 ) ;
#62248 = DIRECTION ( 'NONE',  ( 0.000000000000000000, 0.000000000000000000, 1.000000000000000000 ) ) ;
#62249 = CARTESIAN_POINT ( 'NONE',  ( 0.000000000000000000, 0.000000000000000000, 0.000000000000000000 ) ) ;
#62250 = CIRCLE ( 'NONE', #20204, 16.00000000000000000 ) ;
#62251 = DIRECTION ( 'NONE',  ( -1.000000000000000000, 0.000000000000000000, 0.000000000000000000 ) ) ;
#62252 = DIRECTION ( 'NONE',  ( -1.000000000000000000, 0.000000000000000000, -0.000000000000000000 ) ) ;
#62253 = CARTESIAN_POINT ( 'NONE',  ( 11.99999999999999822, -68.27212725128254078, -31.46837873495049465 ) ) ;
#62254 = AXIS2_PLACEMENT_3D ( 'NONE', #10409, #8279, #56667 ) ;
#62255 = ORIENTED_EDGE ( 'NONE', *, *, #23636, .T. ) ;
#62256 = CARTESIAN_POINT ( 'NONE',  ( -96.32499999999996021, -207.7050326799711968, 81.71854166840095957 ) ) ;
#62257 = ORIENTED_EDGE ( 'NONE', *, *, #60023, .T. ) ;
#62258 = CARTESIAN_POINT ( 'NONE',  ( 32.50000000000000000, -120.0000000000000000, 2.500000000000000000 ) ) ;
#62259 = EDGE_CURVE ( 'NONE', #4552, #961, #48944, .T. ) ;
#62260 = VERTEX_POINT ( 'NONE', #19863 ) ;
#62262 = CARTESIAN_POINT ( 'NONE',  ( -97.65000000000001990, 88.47002178664754979, 78.06729166840096923 ) ) ;
#62261 = CARTESIAN_POINT ( 'NONE',  ( 97.64999999999997726, 91.52997821335252127, 82.19479166840095274 ) ) ;
#62263 = AXIS2_PLACEMENT_3D ( 'NONE', #48151, #32320, #55266 ) ;
#62264 = ORIENTED_EDGE ( 'NONE', *, *, #55322, .F. ) ;
#62265 = CARTESIAN_POINT ( 'NONE',  ( 96.15314808468748708, 88.00268892867053694, 83.66322916753382799 ) ) ;
#62266 = CARTESIAN_POINT ( 'NONE',  ( 93.67499999999998295, 92.29496732002878900, 83.54416666666666913 ) ) ;
#62267 = CARTESIAN_POINT ( 'NONE',  ( -97.64999999960633659, -209.9999706968024782, 82.45844277047601167 ) ) ;
#62268 = FACE_OUTER_BOUND ( 'NONE', #17309, .T. ) ;
#62269 = CYLINDRICAL_SURFACE ( 'NONE', #66640, 16.00000000000000000 ) ;
#62270 = CARTESIAN_POINT ( 'NONE',  ( 0.000000000000000000, 0.000000000000000000, -175.0000000000000000 ) ) ;
#62271 = EDGE_LOOP ( 'NONE', ( #47067, #5874, #33652, #21511 ) ) ;
#62272 = CARTESIAN_POINT ( 'NONE',  ( -96.32500000000001705, 92.29496732002878900, 80.36916666666665776 ) ) ;
#62273 = DIRECTION ( 'NONE',  ( -1.000000000000000000, -0.000000000000000000, -0.000000000000000000 ) ) ;
#62274 = DIRECTION ( 'NONE',  ( -1.000000000000000000, 0.000000000000000000, 0.000000000000000000 ) ) ;
#62275 = ORIENTED_EDGE ( 'NONE', *, *, #15956, .F. ) ;
#62276 = VERTEX_POINT ( 'NONE', #36416 ) ;
#62277 = CARTESIAN_POINT ( 'NONE',  ( -94.99999999999997158, -209.9999999999999716, 90.00000000000000000 ) ) ;
#62278 = FACE_OUTER_BOUND ( 'NONE', #71576, .T. ) ;
#62279 = CARTESIAN_POINT ( 'NONE',  ( 11.99999999999999822, -75.11764819372145041, 29.05362095685286050 ) ) ;
#62280 = CARTESIAN_POINT ( 'NONE',  ( -96.15314808468747287, -208.0026889286704943, 81.44072916753381719 ) ) ;
#62281 = ORIENTED_EDGE ( 'NONE', *, *, #68768, .F. ) ;
#62282 = AXIS2_PLACEMENT_3D ( 'NONE', #4669, #50115, #50875 ) ;
#62283 = CARTESIAN_POINT ( 'NONE',  ( -93.84685191531254134, 91.99731107132950569, 87.52614583420047722 ) ) ;
#62284 = ORIENTED_EDGE ( 'NONE', *, *, #6642, .T. ) ;
#62285 = AXIS2_PLACEMENT_3D ( 'NONE', #3492, #26400, #53864 ) ;
#62286 = AXIS2_PLACEMENT_3D ( 'NONE', #10583, #3230, #5346 ) ;
#62287 = CARTESIAN_POINT ( 'NONE',  ( 48.80839716909466830, -10.37454508288725208, -5.500000000000000000 ) ) ;
#62288 = LINE ( 'NONE', #67176, #69525 ) ;
#62289 = AXIS2_PLACEMENT_3D ( 'NONE', #9101, #50434, #38790 ) ;
#62290 = DIRECTION ( 'NONE',  ( -1.000000000000000000, 0.000000000000000000, -0.000000000000000000 ) ) ;
#62291 = CARTESIAN_POINT ( 'NONE',  ( 92.69370383062498320, 90.00000000000002842, 75.03781250086713328 ) ) ;
#62292 = VECTOR ( 'NONE', #19201, 1000.000000000000000 ) ;
#62293 = FACE_OUTER_BOUND ( 'NONE', #19939, .T. ) ;
#62294 = DIRECTION ( 'NONE',  ( -1.000000000000000000, 0.000000000000000000, -0.000000000000000000 ) ) ;
#62295 = CARTESIAN_POINT ( 'NONE',  ( -12.75044424985254921, 0.001194404164626844313, 127.4927882439603195 ) ) ;
#62296 = LINE ( 'NONE', #21682, #22038 ) ;
#62297 = CYLINDRICAL_SURFACE ( 'NONE', #2830, 82.00000000000000000 ) ;
#62298 = DIRECTION ( 'NONE',  ( -1.000000000000000000, 0.000000000000000000, -0.000000000000000000 ) ) ;
#62299 = CARTESIAN_POINT ( 'NONE',  ( 2.184357737007946383E-12, -120.0000000000000000, -48.99999999999997158 ) ) ;
#62300 = DIRECTION ( 'NONE',  ( -0.000000000000000000, -0.000000000000000000, 1.000000000000000000 ) ) ;
#62301 = AXIS2_PLACEMENT_3D ( 'NONE', #7256, #1652, #52743 ) ;
#62302 = DIRECTION ( 'NONE',  ( 0.000000000000000000, 0.000000000000000000, 1.000000000000000000 ) ) ;
#62303 = CARTESIAN_POINT ( 'NONE',  ( -12.50000000000000000, -132.5000000000000000, -40.00000000000000000 ) ) ;
#62304 = CIRCLE ( 'NONE', #17905, 31.99999999999998934 ) ;
#62305 = ORIENTED_EDGE ( 'NONE', *, *, #47459, .F. ) ;
#62306 = FACE_OUTER_BOUND ( 'NONE', #55961, .T. ) ;
#62307 = CARTESIAN_POINT ( 'NONE',  ( -93.84685191531252713, 88.00268892867056536, 78.42447916753381776 ) ) ;
#62308 = AXIS2_PLACEMENT_3D ( 'NONE', #44301, #61595, #4466 ) ;
#62309 = EDGE_CURVE ( 'NONE', #36390, #46172, #14972, .T. ) ;
#62310 = VECTOR ( 'NONE', #7935, 1000.000000000000227 ) ;
#62311 = VECTOR ( 'NONE', #64800, 1000.000000000000000 ) ;
#62312 = EDGE_CURVE ( 'NONE', #3737, #32728, #18466, .T. ) ;
#62313 = CARTESIAN_POINT ( 'NONE',  ( 92.69370383062501162, -211.3315407142195852, 89.06072916753379332 ) ) ;
#62314 = EDGE_LOOP ( 'NONE', ( #65368, #12178, #72578, #62625 ) ) ;
#62315 = CIRCLE ( 'NONE', #53874, 82.00000000000000000 ) ;
#62316 = EDGE_CURVE ( 'NONE', #33390, #11562, #65012, .T. ) ;
#62317 = CARTESIAN_POINT ( 'NONE',  ( -92.34999999999999432, -210.0000000198591295, 85.95187500101400246 ) ) ;
#62318 = CARTESIAN_POINT ( 'NONE',  ( 92.34999999999999432, 90.00000000000002842, 78.57000000000000739 ) ) ;
#62319 = DIRECTION ( 'NONE',  ( -0.000000000000000000, -0.000000000000000000, 1.000000000000000000 ) ) ;
#62320 = CARTESIAN_POINT ( 'NONE',  ( 0.000000000000000000, -10.45096189432344147, 21.10159698893426494 ) ) ;
#62321 = CARTESIAN_POINT ( 'NONE',  ( 97.30629616937498838, -209.9999999999999716, 76.78406250086715090 ) ) ;
#62322 = VERTEX_POINT ( 'NONE', #3720 ) ;
#62324 = ORIENTED_EDGE ( 'NONE', *, *, #35040, .F. ) ;
#62323 =( BOUNDED_CURVE ( )  B_SPLINE_CURVE ( 2, ( #13906, #31209, #48506, #19919, #49880, #65805, #9672 ),
 .UNSPECIFIED., .F., .F. ) 
 B_SPLINE_CURVE_WITH_KNOTS ( ( 3, 2, 2, 3 ),
 ( 0.7291666666666665186, 0.7361111111111109384, 0.7430555555555553582, 0.7499999999999996669 ),
 .UNSPECIFIED. ) 
 CURVE ( )  GEOMETRIC_REPRESENTATION_ITEM ( )  RATIONAL_B_SPLINE_CURVE ( ( 1.000000000000002220, 0.8660254037844365982, 1.000000000000000000, 0.8660254037844387076, 1.000000000000000000, 0.8660254037844451469, 0.9999999999999935607 ) ) 
 REPRESENTATION_ITEM ( '' )  );
#62325 = EDGE_CURVE ( 'NONE', #35410, #44776, #6422, .T. ) ;
#62326 = AXIS2_PLACEMENT_3D ( 'NONE', #63281, #27180, #62546 ) ;
#62327 = EDGE_CURVE ( 'NONE', #63369, #50488, #16535, .T. ) ;
#62328 = DIRECTION ( 'NONE',  ( -1.000000000000000000, 0.000000000000000000, 0.000000000000000000 ) ) ;
#62329 = DIRECTION ( 'NONE',  ( 0.000000000000000000, 0.000000000000000000, 1.000000000000000000 ) ) ;
#62330 = DIRECTION ( 'NONE',  ( -0.000000000000000000, -0.000000000000000000, 1.000000000000000000 ) ) ;
#62331 = LINE ( 'NONE', #72826, #36305 ) ;
#62332 = VECTOR ( 'NONE', #13245, 1000.000000000000000 ) ;
#62333 = CARTESIAN_POINT ( 'NONE',  ( 12.00000000000000000, 16.83928648764945635, 16.46020748918027010 ) ) ;
#62334 = CARTESIAN_POINT ( 'NONE',  ( 97.64999999999999147, -209.9999999999999716, 89.04749999999999943 ) ) ;
#62335 = AXIS2_PLACEMENT_3D ( 'NONE', #6822, #52689, #6107 ) ;
#62336 = AXIS2_PLACEMENT_3D ( 'NONE', #50353, #4145, #72166 ) ;
#62337 = ORIENTED_EDGE ( 'NONE', *, *, #43333, .F. ) ;
#62338 = DIRECTION ( 'NONE',  ( -1.000000000000000000, 0.000000000000000000, 0.000000000000000000 ) ) ;
#62339 = ORIENTED_EDGE ( 'NONE', *, *, #29082, .T. ) ;
#62340 = EDGE_LOOP ( 'NONE', ( #43300, #16464, #69632, #48545 ) ) ;
#62341 = CARTESIAN_POINT ( 'NONE',  ( 18.80329974962065265, -105.8248132807389084, 2.500000000000000000 ) ) ;
#62342 = ADVANCED_FACE ( 'NONE', ( #70992 ), #19494, .F. ) ;
#62343 = EDGE_CURVE ( 'NONE', #29316, #15874, #58561, .T. ) ;
#62344 = AXIS2_PLACEMENT_3D ( 'NONE', #17991, #57856, #34919 ) ;
#62345 = FACE_OUTER_BOUND ( 'NONE', #36413, .T. ) ;
#62346 = VECTOR ( 'NONE', #54803, 1000.000000000000000 ) ;
#62347 = EDGE_LOOP ( 'NONE', ( #17340, #55301, #55780, #25906 ) ) ;
#62348 = DIRECTION ( 'NONE',  ( 1.000000000000000000, 0.000000000000000000, -0.000000000000000000 ) ) ;
#62349 = CARTESIAN_POINT ( 'NONE',  ( 95.00000000000000000, -213.0599564267049857, 76.90312500173429555 ) ) ;
#62350 = CARTESIAN_POINT ( 'NONE',  ( 92.34999999999999432, 91.52997821335252127, 82.32708333333332007 ) ) ;
#62351 = EDGE_LOOP ( 'NONE', ( #3689, #19705, #50500, #6947 ) ) ;
#62352 = LINE ( 'NONE', #17576, #4729 ) ;
#62353 = ORIENTED_EDGE ( 'NONE', *, *, #22425, .F. ) ;
#62354 = LINE ( 'NONE', #21731, #72894 ) ;
#62355 = ORIENTED_EDGE ( 'NONE', *, *, #52461, .T. ) ;
#62356 = DIRECTION ( 'NONE',  ( 0.000000000000000000, 0.9876883405951371042, 0.1564344650402346437 ) ) ;
#62357 = CARTESIAN_POINT ( 'NONE',  ( -95.00000000000002842, 92.66308142843932671, 83.92781250086716227 ) ) ;
#62358 = CARTESIAN_POINT ( 'NONE',  ( 93.84685191531248449, 88.00268892867053694, 78.31864583420048120 ) ) ;
#62359 = ORIENTED_EDGE ( 'NONE', *, *, #3828, .F. ) ;
#62360 = CARTESIAN_POINT ( 'NONE',  ( -0.9515373497862389396, -96.47140937769621871, -5.500000000000000000 ) ) ;
#62361 = VECTOR ( 'NONE', #60612, 999.9999999999998863 ) ;
#62362 = PLANE ( 'NONE',  #22050 ) ;
#62363 = AXIS2_PLACEMENT_3D ( 'NONE', #43596, #72502, #55969 ) ;
#62364 = CARTESIAN_POINT ( 'NONE',  ( -22.17439115976385366, -112.2188447712574799, 2.500000000000000000 ) ) ;
#62365 = CARTESIAN_POINT ( 'NONE',  ( 10.00000000000000000, -59.03342792756231461, -46.54456581323868392 ) ) ;
#62366 = ORIENTED_EDGE ( 'NONE', *, *, #58858, .T. ) ;
#62367 = CARTESIAN_POINT ( 'NONE',  ( -94.99999999999997158, -213.0599564267049857, 86.34874999999999545 ) ) ;
#62368 = CIRCLE ( 'NONE', #10715, 16.00000000000000355 ) ;
#62369 = CARTESIAN_POINT ( 'NONE',  ( -92.69370383062498320, -209.9999999999999716, 75.99031250086714806 ) ) ;
#62370 = ORIENTED_EDGE ( 'NONE', *, *, #18899, .T. ) ;
#62371 = EDGE_LOOP ( 'NONE', ( #47422, #17480, #54179, #72908 ) ) ;
#62372 = CARTESIAN_POINT ( 'NONE',  ( 94.99999999999998579, 93.05995642670504253, 79.04624999999997215 ) ) ;
#62373 = VECTOR ( 'NONE', #65008, 1000.000000000000000 ) ;
#62374 = AXIS2_PLACEMENT_3D ( 'NONE', #40202, #45487, #67661 ) ;
#62375 = EDGE_LOOP ( 'NONE', ( #36741, #8820, #17831, #13488 ) ) ;
#62376 = FACE_OUTER_BOUND ( 'NONE', #23248, .T. ) ;
#62377 = APPLICATION_CONTEXT ( 'automotive_design' ) ;
#62378 = CARTESIAN_POINT ( 'NONE',  ( 94.99999999999998579, 86.94004357329502852, 80.63375000000000625 ) ) ;
#62379 = EDGE_LOOP ( 'NONE', ( #16542, #27918, #63919, #48837 ) ) ;
#62380 = CARTESIAN_POINT ( 'NONE',  ( -92.69370383062498320, -209.9999999999999716, 74.72031250086713783 ) ) ;
#62381 = ORIENTED_EDGE ( 'NONE', *, *, #9226, .F. ) ;
#62382 = CARTESIAN_POINT ( 'NONE',  ( -95.00000000000002842, 86.94004357329504273, 76.82374999999998977 ) ) ;
#62383 = DIRECTION ( 'NONE',  ( -0.000000000000000000, -0.000000000000000000, -1.000000000000000000 ) ) ;
#62384 = FACE_OUTER_BOUND ( 'NONE', #70551, .T. ) ;
#62385 = DIRECTION ( 'NONE',  ( 0.000000000000000000, 0.000000000000000000, 1.000000000000000000 ) ) ;
#62386 = DIRECTION ( 'NONE',  ( -7.616308197390131428E-15, 1.000000000000000000, -2.546204323184492723E-14 ) ) ;
#62387 = CARTESIAN_POINT ( 'NONE',  ( 97.65000000000000568, -208.4700217866474645, 82.19479166840095274 ) ) ;
#62388 = CARTESIAN_POINT ( 'NONE',  ( 97.30629616937498838, 90.00000000000002842, 84.88031250086713442 ) ) ;
#62389 = CARTESIAN_POINT ( 'NONE',  ( 10.00000000000000000, 0.8828120875905820508, -37.48860685352290290 ) ) ;
#62390 = FACE_OUTER_BOUND ( 'NONE', #40215, .T. ) ;
#62391 = DIRECTION ( 'NONE',  ( 0.000000000000000000, 0.000000000000000000, 1.000000000000000000 ) ) ;
#62392 = CARTESIAN_POINT ( 'NONE',  ( 0.000000000000000000, 0.000000000000000000, 0.000000000000000000 ) ) ;
#62393 = EDGE_CURVE ( 'NONE', #38016, #28475, #53776, .T. ) ;
#62394 = CARTESIAN_POINT ( 'NONE',  ( 0.000000000000000000, 68.26794271651307611, -31.47745569255064169 ) ) ;
#62395 = CARTESIAN_POINT ( 'NONE',  ( -3.000000000000000000, 23.59884966291538078, -12.14883922797231541 ) ) ;
#62396 = DIRECTION ( 'NONE',  ( 0.000000000000000000, 0.000000000000000000, -1.000000000000000000 ) ) ;
#62397 = EDGE_CURVE ( 'NONE', #47439, #65482, #38656, .T. ) ;
#62398 = CARTESIAN_POINT ( 'NONE',  ( 10.00000000000000000, -0.8261519478436571973, 77.49459641780886443 ) ) ;
#62399 = VECTOR ( 'NONE', #53250, 1000.000000000000000 ) ;
#62400 = CARTESIAN_POINT ( 'NONE',  ( 10.00000000000000000, -17.80606268964563554, 33.00180498840040855 ) ) ;
#62401 = AXIS2_PLACEMENT_3D ( 'NONE', #41660, #58970, #64987 ) ;
#62402 = EDGE_CURVE ( 'NONE', #63726, #29541, #5573, .T. ) ;
#62403 = CARTESIAN_POINT ( 'NONE',  ( 4.999999999999999112, -2.663952781845850826, -41.91543099594819921 ) ) ;
#62404 = CIRCLE ( 'NONE', #40763, 77.49900000000000944 ) ;
#62405 = CARTESIAN_POINT ( 'NONE',  ( -97.30629616937501680, 91.33154071421968467, 88.31989583420048007 ) ) ;
#62406 = CARTESIAN_POINT ( 'NONE',  ( -95.00000000000002842, 90.00000000000004263, 90.00000000000000000 ) ) ;
#62407 = ADVANCED_FACE ( 'NONE', ( #44677 ), #38277, .T. ) ;
#62408 = CARTESIAN_POINT ( 'NONE',  ( -92.34999999999999432, -211.5299782133524502, 84.54958333333333087 ) ) ;
#62409 = CIRCLE ( 'NONE', #54017, 16.00000000000000355 ) ;
#62410 = ADVANCED_FACE ( 'NONE', ( #57065 ), #45040, .F. ) ;
#62411 = CARTESIAN_POINT ( 'NONE',  ( 93.67499999999999716, 87.70503267997126784, 85.66083333333332916 ) ) ;
#62412 = ADVANCED_FACE ( 'NONE', ( #28103 ), #55938, .T. ) ;
#62413 = LINE ( 'NONE', #10894, #64824 ) ;
#62414 = DIRECTION ( 'NONE',  ( 0.000000000000000000, 0.1564344650402244852, 0.9876883405951387696 ) ) ;
#62415 = DIRECTION ( 'NONE',  ( 0.000000000000000000, 0.000000000000000000, 1.000000000000000000 ) ) ;
#62416 = DIRECTION ( 'NONE',  ( 1.000000000000000000, 0.000000000000000000, 0.000000000000000000 ) ) ;
#62417 = VECTOR ( 'NONE', #21366, 1000.000000000000000 ) ;
#62418 = CIRCLE ( 'NONE', #29975, 37.49900000000000233 ) ;
#62419 = CARTESIAN_POINT ( 'NONE',  ( 96.15314808468750130, -211.9973110713294489, 86.20322916753382003 ) ) ;
#62420 = ORIENTED_EDGE ( 'NONE', *, *, #62661, .T. ) ;
#62421 = AXIS2_PLACEMENT_3D ( 'NONE', #54645, #31701, #43391 ) ;
#62422 = ORIENTED_EDGE ( 'NONE', *, *, #61882, .F. ) ;
#62423 = EDGE_CURVE ( 'NONE', #72940, #32025, #67594, .T. ) ;
#62424 = EDGE_CURVE ( 'NONE', #27527, #47680, #33360, .T. ) ;
#62425 = CARTESIAN_POINT ( 'NONE',  ( -97.64999999969894873, 90.00002455906438570, 87.53856274002211535 ) ) ;
#62426 = ORIENTED_EDGE ( 'NONE', *, *, #36743, .T. ) ;
#62427 = CARTESIAN_POINT ( 'NONE',  ( -92.34999999999999432, -209.9999998456625860, 79.60187500750915035 ) ) ;
#62428 =( BOUNDED_CURVE ( )  B_SPLINE_CURVE ( 2, ( #50942, #7582, #51305, #58342, #65478, #59092, #41423 ),
 .UNSPECIFIED., .F., .F. ) 
 B_SPLINE_CURVE_WITH_KNOTS ( ( 3, 2, 2, 3 ),
 ( 0.2963422021981251264, 0.3033979182579412126, 0.3104536837988238762, 0.3175094496506952191 ),
 .UNSPECIFIED. ) 
 CURVE ( )  GEOMETRIC_REPRESENTATION_ITEM ( )  RATIONAL_B_SPLINE_CURVE ( ( 0.9999981209241187718, 0.8660263433289682178, 1.000000000000000000, 0.8660254037844387076, 1.000000000000000000, 0.8660254037844387076, 1.000000000000000000 ) ) 
 REPRESENTATION_ITEM ( '' )  );
#62429 = CARTESIAN_POINT ( 'NONE',  ( 92.69370383062501162, -208.6684592857803295, 78.15989583420048348 ) ) ;
#62430 = ORIENTED_EDGE ( 'NONE', *, *, #50226, .T. ) ;
#62431 = CARTESIAN_POINT ( 'NONE',  ( 97.30629616937498838, -208.6684592857803011, 83.18697916753382060 ) ) ;
#62432 = ORIENTED_EDGE ( 'NONE', *, *, #58237, .F. ) ;
#62433 = CARTESIAN_POINT ( 'NONE',  ( 10.00000000000000000, 35.91791733033475253, 68.67312586195009771 ) ) ;
#62434 = VERTEX_POINT ( 'NONE', #16087 ) ;
#62435 = EDGE_LOOP ( 'NONE', ( #31239, #3521, #54111, #28356 ) ) ;
#62436 = CARTESIAN_POINT ( 'NONE',  ( -93.84685191531254134, 91.99731107132950569, 74.98489583420048632 ) ) ;
#62437 = LINE ( 'NONE', #33839, #30431 ) ;
#62438 = VERTEX_POINT ( 'NONE', #4836 ) ;
#62439 = CARTESIAN_POINT ( 'NONE',  ( 0.000000000000000000, 0.000000000000000000, 0.000000000000000000 ) ) ;
#62440 = DIRECTION ( 'NONE',  ( -1.000000000000000000, 0.000000000000000000, -0.000000000000000000 ) ) ;
#62441 = ORIENTED_EDGE ( 'NONE', *, *, #58926, .T. ) ;
#62442 = CYLINDRICAL_SURFACE ( 'NONE', #25098, 16.00000000000000000 ) ;
#62443 = ORIENTED_EDGE ( 'NONE', *, *, #8766, .F. ) ;
#62444 = DIRECTION ( 'NONE',  ( 0.000000000000000000, 0.000000000000000000, 1.000000000000000000 ) ) ;
#62445 = AXIS2_PLACEMENT_3D ( 'NONE', #19025, #41976, #36691 ) ;
#62446 = ORIENTED_EDGE ( 'NONE', *, *, #55018, .T. ) ;
#62447 = AXIS2_PLACEMENT_3D ( 'NONE', #44832, #62122, #72629 ) ;
#62448 = CIRCLE ( 'NONE', #39636, 31.99999999999998579 ) ;
#62449 = ORIENTED_EDGE ( 'NONE', *, *, #46939, .T. ) ;
#62450 = ORIENTED_EDGE ( 'NONE', *, *, #47022, .T. ) ;
#62451 = CARTESIAN_POINT ( 'NONE',  ( 92.69370383062501162, -208.6684592857803011, 75.61989583420047722 ) ) ;
#62452 = CARTESIAN_POINT ( 'NONE',  ( -10.00000000000000000, 0.000000000000000000, 0.000000000000000000 ) ) ;
#62453 = ORIENTED_EDGE ( 'NONE', *, *, #66780, .T. ) ;
#62454 = EDGE_LOOP ( 'NONE', ( #27439, #50060, #73664, #7932 ) ) ;
#62455 = AXIS2_PLACEMENT_3D ( 'NONE', #32643, #55589, #8620 ) ;
#62456 = VERTEX_POINT ( 'NONE', #73217 ) ;
#62457 = CARTESIAN_POINT ( 'NONE',  ( 90.00000000000000000, 95.00000000000002842, -79.99999999999998579 ) ) ;
#62458 = DIRECTION ( 'NONE',  ( 0.000000000000000000, 0.000000000000000000, 1.000000000000000000 ) ) ;
#62459 = CARTESIAN_POINT ( 'NONE',  ( -93.84685191531252713, 88.00268892867056536, 76.67822916753381435 ) ) ;
#62460 = ORIENTED_EDGE ( 'NONE', *, *, #43896, .F. ) ;
#62461 = CARTESIAN_POINT ( 'NONE',  ( 96.32499999999998863, -207.7050326799711968, 89.78833333333332689 ) ) ;
#62462 = ORIENTED_EDGE ( 'NONE', *, *, #29424, .F. ) ;
#62463 = CARTESIAN_POINT ( 'NONE',  ( 97.64999999999999147, 90.00000000000002842, 75.07749999999998636 ) ) ;
#62464 = CARTESIAN_POINT ( 'NONE',  ( -97.30629616937497417, -208.6684592857803011, 86.41489583420047893 ) ) ;
#62465 = VERTEX_POINT ( 'NONE', #62341 ) ;
#62466 = CARTESIAN_POINT ( 'NONE',  ( 92.35000000000000853, -209.9999999999999716, 76.66499999999999204 ) ) ;
#62467 = LINE ( 'NONE', #44048, #48788 ) ;
#62468 = DIRECTION ( 'NONE',  ( 1.000000000000000000, -0.000000000000000000, -0.000000000000000000 ) ) ;
#62469 = CARTESIAN_POINT ( 'NONE',  ( -97.30629616937497417, -208.6684592857803295, 80.06489583420047040 ) ) ;
#62470 = EDGE_CURVE ( 'NONE', #27241, #66920, #22102, .T. ) ;
#62471 = AXIS2_PLACEMENT_3D ( 'NONE', #30349, #64954, #18697 ) ;
#62472 = FACE_OUTER_BOUND ( 'NONE', #12389, .T. ) ;
#62473 = CARTESIAN_POINT ( 'NONE',  ( 92.34999999999999432, 90.00000000000002842, 89.36499999999999488 ) ) ;
#62474 = CIRCLE ( 'NONE', #52849, 77.49900000000002365 ) ;
#62475 = AXIS2_PLACEMENT_3D ( 'NONE', #71123, #43693, #72594 ) ;
#62476 = CARTESIAN_POINT ( 'NONE',  ( -3.000000000000000000, -25.60904388321925396, 6.976881207771172377 ) ) ;
#62477 = ADVANCED_FACE ( 'NONE', ( #56698 ), #39023, .F. ) ;
#62478 = AXIS2_PLACEMENT_3D ( 'NONE', #24874, #15065, #54925 ) ;
#62479 = VECTOR ( 'NONE', #10606, 1000.000000000000000 ) ;
#62480 = CARTESIAN_POINT ( 'NONE',  ( 0.000000000000000000, -76.41127070299262414, -12.93880638057396304 ) ) ;
#62481 = EDGE_CURVE ( 'NONE', #41070, #56046, #72833, .T. ) ;
#62482 = DIRECTION ( 'NONE',  ( -0.000000000000000000, -0.000000000000000000, -1.000000000000000000 ) ) ;
#62483 = CARTESIAN_POINT ( 'NONE',  ( -92.69370383062502583, 88.66845928578038638, 81.65239583420049030 ) ) ;
#62484 = CARTESIAN_POINT ( 'NONE',  ( 0.000000000000000000, -67.80270845531921964, 46.11716303203163392 ) ) ;
#62485 = DIRECTION ( 'NONE',  ( -0.9435911131814402886, 0.3311129884571281101, 0.000000000000000000 ) ) ;
#62486 = ORIENTED_EDGE ( 'NONE', *, *, #13132, .T. ) ;
#62487 = CARTESIAN_POINT ( 'NONE',  ( 97.65000000000000568, 88.47002178664752137, 79.54895833506762415 ) ) ;
#62488 = ADVANCED_FACE ( 'NONE', ( #43930 ), #61960, .F. ) ;
#62489 = CARTESIAN_POINT ( 'NONE',  ( -2.500000000000003997, 4.330127018922192761, -6.000000000000000000 ) ) ;
#62490 = CARTESIAN_POINT ( 'NONE',  ( 2.500000000000034639, 90.00000000000000000, -90.00000000000000000 ) ) ;
#62491 = DIRECTION ( 'NONE',  ( -1.000000000000000000, 0.000000000000000000, 0.000000000000000000 ) ) ;
#62492 = CYLINDRICAL_SURFACE ( 'NONE', #47775, 77.49899999999999523 ) ;
#62493 = PLANE ( 'NONE',  #37602 ) ;
#62494 = CARTESIAN_POINT ( 'NONE',  ( -94.99999999999997158, -207.3369185715606307, 80.11781250086714579 ) ) ;
#62495 = FACE_OUTER_BOUND ( 'NONE', #38951, .T. ) ;
#62496 = ORIENTED_EDGE ( 'NONE', *, *, #64197, .T. ) ;
#62497 = ADVANCED_FACE ( 'NONE', ( #73962 ), #9706, .T. ) ;
#62498 = DIRECTION ( 'NONE',  ( -1.000000000000000000, 0.000000000000000000, 0.000000000000000000 ) ) ;
#62499 = CARTESIAN_POINT ( 'NONE',  ( 11.99999999999999822, 28.89263327155746097, 71.91182617369197771 ) ) ;
#62500 = CARTESIAN_POINT ( 'NONE',  ( 5.999999999999999112, 59.75363087400153006, -56.15606465354896670 ) ) ;
#62501 = CARTESIAN_POINT ( 'NONE',  ( -3.000000000000000000, 24.81905959214261514, 9.408202855044825341 ) ) ;
#62502 = AXIS2_PLACEMENT_3D ( 'NONE', #44722, #2030, #2770 ) ;
#62503 = DIRECTION ( 'NONE',  ( -1.000000000000000000, 0.000000000000000000, 0.000000000000000000 ) ) ;
#62504 = AXIS2_PLACEMENT_3D ( 'NONE', #38985, #45754, #5898 ) ;
#62505 = VECTOR ( 'NONE', #29970, 1000.000000000000000 ) ;
#62506 = DIRECTION ( 'NONE',  ( 1.000000000000000000, 0.000000000000000000, 0.000000000000000000 ) ) ;
#62507 = ORIENTED_EDGE ( 'NONE', *, *, #19229, .F. ) ;
#62508 = EDGE_CURVE ( 'NONE', #8415, #42183, #4088, .T. ) ;
#62509 = CARTESIAN_POINT ( 'NONE',  ( 4.999999999999999112, -38.55633173627022359, 16.65560815589396526 ) ) ;
#62510 = EDGE_CURVE ( 'NONE', #58494, #40236, #38162, .T. ) ;
#62511 = CYLINDRICAL_SURFACE ( 'NONE', #27124, 2.649999999999985700 ) ;
#62512 = VERTEX_POINT ( 'NONE', #1440 ) ;
#62513 = CARTESIAN_POINT ( 'NONE',  ( 92.69370383062501162, -208.6684592857803295, 88.31989583420048007 ) ) ;
#62514 = DIRECTION ( 'NONE',  ( -1.000000000000000000, -0.000000000000000000, 0.000000000000000000 ) ) ;
#62515 = EDGE_CURVE ( 'NONE', #62167, #29219, #29722, .T. ) ;
#62516 = ORIENTED_EDGE ( 'NONE', *, *, #25412, .F. ) ;
#62517 = DIRECTION ( 'NONE',  ( 0.000000000000000000, 0.000000000000000000, 1.000000000000000000 ) ) ;
#62518 = AXIS2_PLACEMENT_3D ( 'NONE', #15099, #49674, #21101 ) ;
#62519 = ORIENTED_EDGE ( 'NONE', *, *, #45267, .F. ) ;
#62520 = DIRECTION ( 'NONE',  ( -1.000000000000000000, 0.000000000000000000, 0.000000000000000000 ) ) ;
#62521 = VERTEX_POINT ( 'NONE', #35590 ) ;
#62522 = AXIS2_PLACEMENT_3D ( 'NONE', #32729, #55310, #61334 ) ;
#62523 = DIRECTION ( 'NONE',  ( -1.000000000000000000, 0.000000000000000000, -0.000000000000000000 ) ) ;
#62524 = CIRCLE ( 'NONE', #54140, 4.700000000000000178 ) ;
#62525 = ORIENTED_EDGE ( 'NONE', *, *, #31116, .T. ) ;
#62526 = ORIENTED_EDGE ( 'NONE', *, *, #3412, .T. ) ;
#62527 = VERTEX_POINT ( 'NONE', #6304 ) ;
#62528 = DIRECTION ( 'NONE',  ( -1.000000000000000000, 0.000000000000000000, -0.000000000000000000 ) ) ;
#62529 = ORIENTED_EDGE ( 'NONE', *, *, #40923, .T. ) ;
#62530 = ORIENTED_EDGE ( 'NONE', *, *, #33712, .F. ) ;
#62531 = CARTESIAN_POINT ( 'NONE',  ( 96.32499999999998863, 87.70503267997126784, 87.03666666666666174 ) ) ;
#62532 = DIRECTION ( 'NONE',  ( -0.000000000000000000, -0.000000000000000000, 1.000000000000000000 ) ) ;
#62533 = CARTESIAN_POINT ( 'NONE',  ( -2.459674775249762302, -3.512261536895417911E-15, -1.958521724548552858E-15 ) ) ;
#62534 = VERTEX_POINT ( 'NONE', #34864 ) ;
#62535 = ORIENTED_EDGE ( 'NONE', *, *, #63586, .F. ) ;
#62536 = ORIENTED_EDGE ( 'NONE', *, *, #20092, .T. ) ;
#62537 = CARTESIAN_POINT ( 'NONE',  ( 97.30629616937498838, 90.00000000000002842, 85.51531250086713953 ) ) ;
#62538 = ORIENTED_EDGE ( 'NONE', *, *, #46421, .F. ) ;
#62539 = CARTESIAN_POINT ( 'NONE',  ( 93.84685191531251292, -211.9973110713294489, 86.57364583420047666 ) ) ;
#62540 = APPLICATION_PROTOCOL_DEFINITION ( 'draft international standard', 'automotive_design', 1998, #40737 ) ;
#62541 = CARTESIAN_POINT ( 'NONE',  ( 2.459674775249774736, -1.861299128798561507E-13, -15.79999999999999538 ) ) ;
#62542 = LINE ( 'NONE', #6855, #43690 ) ;
#62543 = CARTESIAN_POINT ( 'NONE',  ( 15.00000000000000000, 23.59884966291538078, 12.14883922797231008 ) ) ;
#62544 = DIRECTION ( 'NONE',  ( 0.000000000000000000, 0.000000000000000000, -1.000000000000000000 ) ) ;
#62545 = CARTESIAN_POINT ( 'NONE',  ( 1.560000000000000053, -0.8660254037844384856, 1.500000000000000000 ) ) ;
#62546 = DIRECTION ( 'NONE',  ( 0.000000000000000000, 0.000000000000000000, 1.000000000000000000 ) ) ;
#62547 = CARTESIAN_POINT ( 'NONE',  ( -92.69370383062498320, -209.9999999999999716, 88.05531250086713158 ) ) ;
#62548 = CARTESIAN_POINT ( 'NONE',  ( -93.84685191531254134, 91.99731107132950569, 86.41489583420049314 ) ) ;
#62549 = VERTEX_POINT ( 'NONE', #69080 ) ;
#62551 = CARTESIAN_POINT ( 'NONE',  ( -97.30629616937501680, 90.00000000000004263, 84.56281250086713897 ) ) ;
#62550 = CARTESIAN_POINT ( 'NONE',  ( 92.69370383062498320, 90.00000000000002842, 83.29281250086714294 ) ) ;
#62552 = VERTEX_POINT ( 'NONE', #690 ) ;
#62553 = CARTESIAN_POINT ( 'NONE',  ( 15.00000000000000000, 0.000000000000000000, 0.000000000000000000 ) ) ;
#62554 = DIRECTION ( 'NONE',  ( 0.000000000000000000, 0.000000000000000000, 1.000000000000000000 ) ) ;
#62555 = CARTESIAN_POINT ( 'NONE',  ( 10.00000000000000000, 8.840884882376133902, -74.65374052328640175 ) ) ;
#62556 = CARTESIAN_POINT ( 'NONE',  ( 0.000000000000000000, 28.89263327155848415, -71.91182617369156560 ) ) ;
#62557 = CARTESIAN_POINT ( 'NONE',  ( -93.84685191531247028, -211.9973110713294489, 88.58447916753381435 ) ) ;
#62558 = CARTESIAN_POINT ( 'NONE',  ( 0.000000000000000000, 62.50329211542435104, 41.76937507738811917 ) ) ;
#62559 = EDGE_CURVE ( 'NONE', #14320, #25862, #18302, .T. ) ;
#62560 = VECTOR ( 'NONE', #4798, 1000.000000000000000 ) ;
#62561 = AXIS2_PLACEMENT_3D ( 'NONE', #58839, #34794, #18238 ) ;
#62562 = DIRECTION ( 'NONE',  ( -0.000000000000000000, -0.000000000000000000, 1.000000000000000000 ) ) ;
#62563 = DIRECTION ( 'NONE',  ( -1.000000000000000000, 0.000000000000000000, 0.000000000000000000 ) ) ;
#62564 = AXIS2_PLACEMENT_3D ( 'NONE', #14081, #2496, #60343 ) ;
#62565 = CARTESIAN_POINT ( 'NONE',  ( -97.65000000000001990, 90.00000000000004263, 90.00000000000000000 ) ) ;
#62566 = ORIENTED_EDGE ( 'NONE', *, *, #19860, .T. ) ;
#62567 = VERTEX_POINT ( 'NONE', #70163 ) ;
#62568 = EDGE_CURVE ( 'NONE', #27866, #63232, #67027, .T. ) ;
#62569 = CARTESIAN_POINT ( 'NONE',  ( -96.32500000000001705, 87.70503267997129626, 78.67583333333332973 ) ) ;
#62570 = ADVANCED_FACE ( 'NONE', ( #7021 ), #29204, .F. ) ;
#62571 = CARTESIAN_POINT ( 'NONE',  ( 0.000000000000000000, 0.000000000000000000, 0.000000000000000000 ) ) ;
#62572 = CARTESIAN_POINT ( 'NONE',  ( 97.64999999999821512, -209.9999969335172807, 75.79187510780352000 ) ) ;
#62573 = DIRECTION ( 'NONE',  ( 0.000000000000000000, 0.000000000000000000, 1.000000000000000000 ) ) ;
#62574 = DIRECTION ( 'NONE',  ( -1.000000000000000000, 0.000000000000000000, -0.000000000000000000 ) ) ;
#62575 = CARTESIAN_POINT ( 'NONE',  ( -97.64997399525483956, 88.47000677280088610, 86.32229270695526679 ) ) ;
#62576 = DIRECTION ( 'NONE',  ( -1.000000000000000000, 0.000000000000000000, 0.000000000000000000 ) ) ;
#62577 = ORIENTED_EDGE ( 'NONE', *, *, #70434, .F. ) ;
#62578 = CARTESIAN_POINT ( 'NONE',  ( -95.00000000000002842, 92.66308142843932671, 77.41906250086714181 ) ) ;
#62579 = EDGE_CURVE ( 'NONE', #68468, #7579, #44242, .T. ) ;
#62580 = DIRECTION ( 'NONE',  ( 0.000000000000000000, 0.000000000000000000, 1.000000000000000000 ) ) ;
#62581 = VECTOR ( 'NONE', #35897, 1000.000000000000114 ) ;
#62582 = CARTESIAN_POINT ( 'NONE',  ( -3.702536634196119447, 8.043911037661890973, -45.00000000000000000 ) ) ;
#62583 = AXIS2_PLACEMENT_3D ( 'NONE', #31823, #26185, #8908 ) ;
#62584 = DIRECTION ( 'NONE',  ( 1.000000000000000000, 0.000000000000000000, 0.000000000000000000 ) ) ;
#62585 = CARTESIAN_POINT ( 'NONE',  ( 0.000000000000000000, 0.000000000000000000, 0.000000000000000000 ) ) ;
#62586 = FACE_OUTER_BOUND ( 'NONE', #3381, .T. ) ;
#62587 = CARTESIAN_POINT ( 'NONE',  ( -97.30629616937497417, -208.6684592857803011, 89.74864583420048803 ) ) ;
#62588 = VECTOR ( 'NONE', #30002, 1000.000000000000000 ) ;
#62589 = ADVANCED_FACE ( 'NONE', ( #11920 ), #46511, .F. ) ;
#62590 = EDGE_CURVE ( 'NONE', #58552, #35978, #24324, .T. ) ;
#62591 = CARTESIAN_POINT ( 'NONE',  ( 96.15314808468748708, 91.99731107132950569, 75.61989583420049144 ) ) ;
#62592 = CARTESIAN_POINT ( 'NONE',  ( -96.15314808468747287, -208.0026889286704943, 80.80572916753382628 ) ) ;
#62593 = LINE ( 'NONE', #51660, #17059 ) ;
#62594 = ORIENTED_EDGE ( 'NONE', *, *, #52746, .T. ) ;
#62595 = CARTESIAN_POINT ( 'NONE',  ( 97.64999999999999147, -210.0000000207152198, 80.87187500099602744 ) ) ;
#62596 = CARTESIAN_POINT ( 'NONE',  ( 0.000000000000000000, 72.35432306680485226, -20.40083707022909110 ) ) ;
#62597 = LINE ( 'NONE', #33999, #50953 ) ;
#62598 = CARTESIAN_POINT ( 'NONE',  ( -92.69370383062505425, 91.33154071421968467, 79.37697916753381833 ) ) ;
#62599 = CARTESIAN_POINT ( 'NONE',  ( 92.69370383062501162, -208.6684592857803011, 78.79489583420047438 ) ) ;
#62600 = VERTEX_POINT ( 'NONE', #47257 ) ;
#62601 = ADVANCED_FACE ( 'NONE', ( #68720 ), #40883, .T. ) ;
#62602 = EDGE_CURVE ( 'NONE', #47885, #18460, #12291, .T. ) ;
#62603 = CYLINDRICAL_SURFACE ( 'NONE', #2288, 31.99999999999998579 ) ;
#62604 = ORIENTED_EDGE ( 'NONE', *, *, #54725, .F. ) ;
#62605 = CARTESIAN_POINT ( 'NONE',  ( 10.00000000000000000, -10.74501242461308159, 35.92658777277507909 ) ) ;
#62606 = VERTEX_POINT ( 'NONE', #41605 ) ;
#62607 = COLOUR_RGB ( '', 0.72549020, 0.75294118, 0.79215686) ;
#62608 = AXIS2_PLACEMENT_3D ( 'NONE', #61344, #38772, #20735 ) ;
#62610 = VECTOR ( 'NONE', #29252, 1000.000000000000000 ) ;
#62609 = LINE ( 'NONE', #21614, #17742 ) ;
#62611 = AXIS2_PLACEMENT_3D ( 'NONE', #46374, #64044, #12518 ) ;
#62612 = ORIENTED_EDGE ( 'NONE', *, *, #21083, .F. ) ;
#62613 = VERTEX_POINT ( 'NONE', #41245 ) ;
#62614 = EDGE_LOOP ( 'NONE', ( #71546, #62624, #56172, #16102 ) ) ;
#62615 = CARTESIAN_POINT ( 'NONE',  ( 92.69370383062501162, -211.3315407142195852, 76.51947916753381662 ) ) ;
#62616 = AXIS2_PLACEMENT_3D ( 'NONE', #72040, #8898, #72410 ) ;
#62617 = ORIENTED_EDGE ( 'NONE', *, *, #35132, .T. ) ;
#62618 = CARTESIAN_POINT ( 'NONE',  ( 10.00000000000000000, -44.88180994100421373, 63.18004540533011948 ) ) ;
#62619 = CARTESIAN_POINT ( 'NONE',  ( 11.99999999999999822, 46.54456581323805153, 59.03342792756280488 ) ) ;
#62620 = CARTESIAN_POINT ( 'NONE',  ( 92.69370383062498320, 90.00000000000002842, 84.72156250086715090 ) ) ;
#62621 = DIRECTION ( 'NONE',  ( 0.000000000000000000, 0.000000000000000000, -1.000000000000000000 ) ) ;
#62622 = CARTESIAN_POINT ( 'NONE',  ( 93.67500000000001137, -212.2949673200287179, 78.67583333333332973 ) ) ;
#62623 = ORIENTED_EDGE ( 'NONE', *, *, #61084, .F. ) ;
#62624 = ORIENTED_EDGE ( 'NONE', *, *, #41926, .F. ) ;
#62625 = ORIENTED_EDGE ( 'NONE', *, *, #45284, .T. ) ;
#62626 = ORIENTED_EDGE ( 'NONE', *, *, #47392, .T. ) ;
#62627 = SURFACE_SIDE_STYLE ('',( #16750 ) ) ;
#62628 = AXIS2_PLACEMENT_3D ( 'NONE', #9556, #32472, #50511 ) ;
#62629 = CIRCLE ( 'NONE', #18175, 82.00000000000000000 ) ;
#62630 = CARTESIAN_POINT ( 'NONE',  ( -26.50044424985679825, 0.001194404164828994459, -48.99999999999931788 ) ) ;
#62631 = CARTESIAN_POINT ( 'NONE',  ( 95.00000000000000000, -209.9999999999999716, 90.00000000000000000 ) ) ;
#62632 = AXIS2_PLACEMENT_3D ( 'NONE', #1029, #18634, #18275 ) ;
#62633 = DIRECTION ( 'NONE',  ( -1.000000000000000000, -0.000000000000000000, -0.000000000000000000 ) ) ;
#62634 = LINE ( 'NONE', #50198, #55197 ) ;
#62635 = CARTESIAN_POINT ( 'NONE',  ( 10.00000000000000000, 0.6853352020795618893, -37.58145647212453611 ) ) ;
#62636 = VERTEX_POINT ( 'NONE', #35228 ) ;
#62637 = CARTESIAN_POINT ( 'NONE',  ( -94.99999999999997158, -206.9400435732949575, 81.03062500173430749 ) ) ;
#62638 = VERTEX_POINT ( 'NONE', #64546 ) ;
#62639 = CARTESIAN_POINT ( 'NONE',  ( 11.99999999999999822, -31.46837873494930093, -68.27212725128309501 ) ) ;
#62640 = ORIENTED_EDGE ( 'NONE', *, *, #10073, .T. ) ;
#62642 = CARTESIAN_POINT ( 'NONE',  ( -97.65000000000001990, 88.47002178664754979, 81.24229166840098060 ) ) ;
#62641 = CARTESIAN_POINT ( 'NONE',  ( 97.64999999999997726, 88.47002178664753558, 79.54895833506762415 ) ) ;
#62643 =( BOUNDED_CURVE ( )  B_SPLINE_CURVE ( 2, ( #68557, #45994, #17045, #39980, #29056, #62935, #11394 ),
 .UNSPECIFIED., .F., .F. ) 
 B_SPLINE_CURVE_WITH_KNOTS ( ( 3, 2, 2, 3 ),
 ( 0.1250000000000002220, 0.1319444444444446418, 0.1388888888888890338, 0.1458333333333334536 ),
 .UNSPECIFIED. ) 
 CURVE ( )  GEOMETRIC_REPRESENTATION_ITEM ( )  RATIONAL_B_SPLINE_CURVE ( ( 0.9999999999999956701, 0.8660254037844430375, 1.000000000000000000, 0.8660254037844387076, 1.000000000000000000, 0.8660254037844365982, 1.000000000000002220 ) ) 
 REPRESENTATION_ITEM ( '' )  );
#62644 = AXIS2_PLACEMENT_3D ( 'NONE', #43268, #26677, #55261 ) ;
#62645 = ORIENTED_EDGE ( 'NONE', *, *, #8076, .T. ) ;
#62646 = MANIFOLD_SOLID_BREP ( 'OuterRace', #53608 ) ;
#62647 = CARTESIAN_POINT ( 'NONE',  ( 92.69370383062498320, 91.33154071421968467, 83.39864583420050792 ) ) ;
#62648 = CARTESIAN_POINT ( 'NONE',  ( 10.00000000000000000, 21.32104025579114648, 30.84782396557224970 ) ) ;
#62649 = FACE_OUTER_BOUND ( 'NONE', #68153, .T. ) ;
#62650 = EDGE_CURVE ( 'NONE', #29886, #66673, #27419, .T. ) ;
#62651 = DIRECTION ( 'NONE',  ( -1.000000000000000000, 0.000000000000000000, 0.000000000000000000 ) ) ;
#62652 = CARTESIAN_POINT ( 'NONE',  ( 92.35001469785312622, 91.52998669916200924, 81.77145774807789280 ) ) ;
#62653 = FACE_OUTER_BOUND ( 'NONE', #31040, .T. ) ;
#62654 = VERTEX_POINT ( 'NONE', #2550 ) ;
#62655 = DIRECTION ( 'NONE',  ( -0.000000000000000000, -0.000000000000000000, 1.000000000000000000 ) ) ;
#62656 = CARTESIAN_POINT ( 'NONE',  ( -3.000000000000000000, -11.95096189432345390, 23.69967320028757385 ) ) ;
#62657 = DIRECTION ( 'NONE',  ( -1.000000000000000000, 0.000000000000000000, 0.000000000000000000 ) ) ;
#62658 = EDGE_LOOP ( 'NONE', ( #6836, #32091, #49985, #69058 ) ) ;
#62659 = EDGE_CURVE ( 'NONE', #48302, #21733, #8879, .T. ) ;
#62660 = EDGE_LOOP ( 'NONE', ( #19573, #68042, #69523, #67877 ) ) ;
#62661 = EDGE_CURVE ( 'NONE', #65748, #65117, #14082, .T. ) ;
#62662 = DIRECTION ( 'NONE',  ( -1.000000000000000000, 0.000000000000000000, 0.000000000000000000 ) ) ;
#62663 = PRODUCT_DEFINITION_SHAPE ( 'NONE', 'NONE',  #74375 ) ;
#62664 = DIRECTION ( 'NONE',  ( 0.000000000000000000, -0.4539904997395350361, -0.8910065241883738940 ) ) ;
#62665 = DIRECTION ( 'NONE',  ( -1.000000000000000000, -0.000000000000000000, -0.000000000000000000 ) ) ;
#62666 = DIRECTION ( 'NONE',  ( -0.000000000000000000, -0.000000000000000000, 1.000000000000000000 ) ) ;
#62667 = CARTESIAN_POINT ( 'NONE',  ( -92.69370383062498320, -211.3315407142195852, 80.54114583420049200 ) ) ;
#62668 = ORIENTED_EDGE ( 'NONE', *, *, #15776, .T. ) ;
#62669 =( BOUNDED_CURVE ( )  B_SPLINE_CURVE ( 2, ( #12069, #465, #11682, #69221, #17708, #10963, #33891 ),
 .UNSPECIFIED., .F., .F. ) 
 B_SPLINE_CURVE_WITH_KNOTS ( ( 3, 2, 2, 3 ),
 ( 0.5926843883826560244, 0.5997400709779450168, 0.6067958365188629299, 0.6138516023217082118 ),
 .UNSPECIFIED. ) 
 CURVE ( )  GEOMETRIC_REPRESENTATION_ITEM ( )  RATIONAL_B_SPLINE_CURVE ( ( 0.9999968501004118382, 0.8660269787527477003, 1.000000000000000000, 0.8660254037844387076, 1.000000000000000000, 0.8660254037844387076, 1.000000000000000000 ) ) 
 REPRESENTATION_ITEM ( '' )  );
#62670 = CARTESIAN_POINT ( 'NONE',  ( -95.00000000000002842, 92.66308142843932671, 89.48406250086713953 ) ) ;
#62671 = ORIENTED_EDGE ( 'NONE', *, *, #74205, .F. ) ;
#62672 = EDGE_CURVE ( 'NONE', #65467, #29404, #20143, .T. ) ;
#62673 = AXIS2_PLACEMENT_3D ( 'NONE', #1194, #11308, #34241 ) ;
#62674 = DIRECTION ( 'NONE',  ( -0.7533909544171997208, -0.6575728627325955200, 0.000000000000000000 ) ) ;
#62675 = CARTESIAN_POINT ( 'NONE',  ( -95.79297114434442051, -212.5043059285055733, 74.98272308147976162 ) ) ;
#62676 = AXIS2_PLACEMENT_3D ( 'NONE', #27873, #62485, #56079 ) ;
#62677 = CARTESIAN_POINT ( 'NONE',  ( 0.000000000000000000, 21.60688246758697062, -79.10210256391344785 ) ) ;
#62678 = CARTESIAN_POINT ( 'NONE',  ( 93.84685191531248449, 88.00268892867053694, 76.41364583420048007 ) ) ;
#62679 = CARTESIAN_POINT ( 'NONE',  ( 11.99999999999999822, 39.78640506895604290, 66.50666863322015843 ) ) ;
#62680 = CARTESIAN_POINT ( 'NONE',  ( 92.35001072685618340, 88.47001559349421029, 78.06729209680057124 ) ) ;
#62681 = LINE ( 'NONE', #11155, #52933 ) ;
#62682 = DIRECTION ( 'NONE',  ( 0.9435911131814398445, -0.3311129884571295534, 0.000000000000000000 ) ) ;
#62683 = DIRECTION ( 'NONE',  ( 1.000000000000000000, 0.000000000000000000, 0.000000000000000000 ) ) ;
#62684 = CARTESIAN_POINT ( 'NONE',  ( 0.000000000000000000, -33.80338159004296017, 16.23288003029484727 ) ) ;
#62685 = VECTOR ( 'NONE', #14064, 1000.000000000000000 ) ;
#62686 = EDGE_CURVE ( 'NONE', #68784, #14616, #73024, .T. ) ;
#62687 = VECTOR ( 'NONE', #35515, 1000.000000000000114 ) ;
#62688 = EDGE_CURVE ( 'NONE', #28347, #69250, #42724, .T. ) ;
#62689 = CARTESIAN_POINT ( 'NONE',  ( 97.30629616937498838, 91.33154071421968467, 86.99697916753382287 ) ) ;
#62690 = CARTESIAN_POINT ( 'NONE',  ( -93.84685191531248449, -208.0026889286704943, 88.95489583420049939 ) ) ;
#62691 = CARTESIAN_POINT ( 'NONE',  ( -5.420674214417706693, -142.8662697233533265, 2.500000000000000000 ) ) ;
#62692 = ORIENTED_EDGE ( 'NONE', *, *, #39987, .F. ) ;
#62693 = DIRECTION ( 'NONE',  ( 0.000000000000000000, 0.4067366430757887730, 0.9135454576426059736 ) ) ;
#62694 = CARTESIAN_POINT ( 'NONE',  ( -95.00000000000002842, 87.33691857156074434, 80.91156250086714863 ) ) ;
#62695 = AXIS2_PLACEMENT_3D ( 'NONE', #55929, #4827, #66842 ) ;
#62696 = EDGE_CURVE ( 'NONE', #28018, #39348, #15398, .T. ) ;
#62697 = EDGE_CURVE ( 'NONE', #16594, #43494, #65811, .T. ) ;
#62698 = VECTOR ( 'NONE', #68359, 1000.000000000000000 ) ;
#62699 = CIRCLE ( 'NONE', #36254, 82.00000000000000000 ) ;
#62700 = CARTESIAN_POINT ( 'NONE',  ( 95.00000000000000000, -207.3369185715606307, 89.48406250086713953 ) ) ;
#62701 = EDGE_CURVE ( 'NONE', #27539, #50397, #19776, .T. ) ;
#62702 = ORIENTED_EDGE ( 'NONE', *, *, #43376, .T. ) ;
#62703 = CARTESIAN_POINT ( 'NONE',  ( 10.00000000000000000, 0.000000000000000000, 0.000000000000000000 ) ) ;
#62704 = CARTESIAN_POINT ( 'NONE',  ( 92.34999999999999432, 90.00000000000002842, 83.01499999999998636 ) ) ;
#62705 = LINE ( 'NONE', #50641, #28791 ) ;
#62706 = ADVANCED_FACE ( 'NONE', ( #19039 ), #60761, .T. ) ;
#62707 = CARTESIAN_POINT ( 'NONE',  ( 92.35004149090323722, -211.5300021681365763, 85.68729332542764610 ) ) ;
#62708 = CARTESIAN_POINT ( 'NONE',  ( 97.64999999999999147, 90.00000000000002842, 90.00000000000000000 ) ) ;
#62709 = ORIENTED_EDGE ( 'NONE', *, *, #27823, .F. ) ;
#62710 = ORIENTED_EDGE ( 'NONE', *, *, #50751, .F. ) ;
#62711 = CARTESIAN_POINT ( 'NONE',  ( 94.99999999999998579, 90.00000000000002842, 90.00000000000000000 ) ) ;
#62712 = DIRECTION ( 'NONE',  ( -1.000000000000000000, 0.000000000000000000, 0.000000000000000000 ) ) ;
#62713 = FACE_OUTER_BOUND ( 'NONE', #13702, .T. ) ;
#62714 = CARTESIAN_POINT ( 'NONE',  ( 0.000000000000000000, -120.0000000000000000, 125.0000000000000000 ) ) ;
#62715 = CARTESIAN_POINT ( 'NONE',  ( 5.000000000000002665, 10.30890764327382847, 81.34940948281339956 ) ) ;
#62716 = CARTESIAN_POINT ( 'NONE',  ( 97.64999999999997726, -208.4700217866474645, 86.56041666666665435 ) ) ;
#62717 = ORIENTED_EDGE ( 'NONE', *, *, #69410, .F. ) ;
#62718 = STYLED_ITEM ( 'NONE', ( #42813 ), #21132 ) ;
#62719 = AXIS2_PLACEMENT_3D ( 'NONE', #17607, #68754, #11582 ) ;
#62720 = EDGE_LOOP ( 'NONE', ( #14418, #52992, #32253, #13515 ) ) ;
#62721 = CARTESIAN_POINT ( 'NONE',  ( -97.64999999947052345, 90.00003365185393989, 81.18829462297244959 ) ) ;
#62722 = ORIENTED_EDGE ( 'NONE', *, *, #13468, .F. ) ;
#62723 = ORIENTED_EDGE ( 'NONE', *, *, #34555, .F. ) ;
#62724 = DIRECTION ( 'NONE',  ( 2.603472992746261562E-14, 2.546204323184492723E-14, -1.000000000000000000 ) ) ;
#62725 = CIRCLE ( 'NONE', #54331, 16.00000000000000000 ) ;
#62726 = DIRECTION ( 'NONE',  ( 0.000000000000000000, 0.000000000000000000, 1.000000000000000000 ) ) ;
#62727 = CARTESIAN_POINT ( 'NONE',  ( 0.000000000000000000, 75.54627589209970040, -17.28742895386005785 ) ) ;
#62728 = CARTESIAN_POINT ( 'NONE',  ( 93.67500000000001137, -207.7050326799711968, 77.27354166840096639 ) ) ;
#62729 = CARTESIAN_POINT ( 'NONE',  ( 96.32499999999998863, 87.70503267997126784, 80.68666666666665321 ) ) ;
#62730 = ORIENTED_EDGE ( 'NONE', *, *, #74004, .F. ) ;
#62731 = CYLINDRICAL_SURFACE ( 'NONE', #20313, 2.649999999999999467 ) ;
#62732 = AXIS2_PLACEMENT_3D ( 'NONE', #67263, #15756, #56742 ) ;
#62733 = EDGE_LOOP ( 'NONE', ( #57013, #62241 ) ) ;
#62734 = CARTESIAN_POINT ( 'NONE',  ( 92.34999999999999432, 90.00000000000002842, 90.00000000000000000 ) ) ;
#62735 = ORIENTED_EDGE ( 'NONE', *, *, #8857, .T. ) ;
#62736 = DIRECTION ( 'NONE',  ( 0.000000000000000000, -0.000000000000000000, -1.000000000000000000 ) ) ;
#62737 = AXIS2_PLACEMENT_3D ( 'NONE', #50219, #20919, #50599 ) ;
#62738 = CARTESIAN_POINT ( 'NONE',  ( -96.15314808468752972, 91.99731107132950569, 80.80572916753382628 ) ) ;
#62739 = CARTESIAN_POINT ( 'NONE',  ( 92.69370383062498320, 90.00000000000002842, 76.94281250086713442 ) ) ;
#62740 = VERTEX_POINT ( 'NONE', #13768 ) ;
#62741 = CARTESIAN_POINT ( 'NONE',  ( 3.000000000000000000, -2.201436576420044755, -1.270999999999999019 ) ) ;
#62742 = CARTESIAN_POINT ( 'NONE',  ( 11.99999999999999822, 36.72794159290334903, -65.59268652807170952 ) ) ;
#62743 = DIRECTION ( 'NONE',  ( -1.000000000000000000, -0.000000000000000000, 0.000000000000000000 ) ) ;
#62744 = ADVANCED_FACE ( 'NONE', ( #9240 ), #59277, .T. ) ;
#62745 = DIRECTION ( 'NONE',  ( -1.000000000000000000, 0.000000000000000000, 0.000000000000000000 ) ) ;
#62746 = ORIENTED_EDGE ( 'NONE', *, *, #2534, .T. ) ;
#62747 = PLANE ( 'NONE',  #71111 ) ;
#62748 = AXIS2_PLACEMENT_3D ( 'NONE', #25744, #2117, #71591 ) ;
#62749 = AXIS2_PLACEMENT_3D ( 'NONE', #47179, #41533, #64471 ) ;
#62750 = CARTESIAN_POINT ( 'NONE',  ( -97.30629616937497417, -208.6684592857803011, 76.25489583420049655 ) ) ;
#62751 = ORIENTED_EDGE ( 'NONE', *, *, #12660, .T. ) ;
#62752 = EDGE_CURVE ( 'NONE', #69024, #52406, #1187, .T. ) ;
#62753 = ORIENTED_EDGE ( 'NONE', *, *, #60263, .F. ) ;
#62754 = DIRECTION ( 'NONE',  ( 0.000000000000000000, -1.000000000000000000, 0.000000000000000000 ) ) ;
#62755 = EDGE_CURVE ( 'NONE', #40253, #71453, #36704, .T. ) ;
#62756 = EDGE_CURVE ( 'NONE', #56357, #46252, #3266, .T. ) ;
#62757 = ORIENTED_EDGE ( 'NONE', *, *, #17902, .F. ) ;
#62758 = DIRECTION ( 'NONE',  ( -1.000000000000000000, -0.000000000000000000, -0.000000000000000000 ) ) ;
#62759 = DIRECTION ( 'NONE',  ( 0.000000000000000000, -0.000000000000000000, -1.000000000000000000 ) ) ;
#62760 = ORIENTED_EDGE ( 'NONE', *, *, #40011, .T. ) ;
#62761 = CARTESIAN_POINT ( 'NONE',  ( -97.30629616937495996, -209.9999999999999716, 77.57781250086713953 ) ) ;
#62762 = ORIENTED_EDGE ( 'NONE', *, *, #65801, .F. ) ;
#62763 = CYLINDRICAL_SURFACE ( 'NONE', #43508, 16.00000000000000000 ) ;
#62764 = LINE ( 'NONE', #34159, #24852 ) ;
#62765 = CARTESIAN_POINT ( 'NONE',  ( -94.95306897617061281, -212.6495843973424655, 75.00000002508416230 ) ) ;
#62766 = CARTESIAN_POINT ( 'NONE',  ( 96.32499999999998863, -207.7050326799711968, 81.53333333333333144 ) ) ;
#62767 = CARTESIAN_POINT ( 'NONE',  ( 0.000000000000000000, -22.74946021919110706, -29.81001611431033282 ) ) ;
#62769 = ADVANCED_FACE ( 'NONE', ( #71648 ), #66039, .T. ) ;
#62768 = CARTESIAN_POINT ( 'NONE',  ( 92.35000000019411459, -210.0000198427945861, 86.27002759516706476 ) ) ;
#62770 = CARTESIAN_POINT ( 'NONE',  ( 97.30629616937498838, 90.00000000000002842, 85.51531250086713953 ) ) ;
#62771 = CARTESIAN_POINT ( 'NONE',  ( -10.00000000000000000, 0.000000000000000000, 0.000000000000000000 ) ) ;
#62772 = DIRECTION ( 'NONE',  ( 0.000000000000000000, 0.000000000000000000, 1.000000000000000000 ) ) ;
#62773 = DIRECTION ( 'NONE',  ( -1.000000000000000000, -0.000000000000000000, 0.000000000000000000 ) ) ;
#62774 = CARTESIAN_POINT ( 'NONE',  ( -2.500000000000015543, -73.00000000000001421, -255.0000000000000000 ) ) ;
#62775 = EDGE_CURVE ( 'NONE', #31441, #31980, #74226, .T. ) ;
#62776 = DIRECTION ( 'NONE',  ( 0.000000000000000000, 0.3090169943749461745, -0.9510565162951539753 ) ) ;
#62777 = LINE ( 'NONE', #68017, #38338 ) ;
#62778 = DIRECTION ( 'NONE',  ( -1.000000000000000000, -0.000000000000000000, 0.000000000000000000 ) ) ;
#62779 = CARTESIAN_POINT ( 'NONE',  ( -11.59999999999999787, 0.000000000000000000, -56.19999999999998863 ) ) ;
#62780 = CARTESIAN_POINT ( 'NONE',  ( 10.00000000000000000, 0.000000000000000000, 0.000000000000000000 ) ) ;
#62781 = PRESENTATION_LAYER_ASSIGNMENT (  '', '', ( #71150 ) ) ;
#62782 = FACE_OUTER_BOUND ( 'NONE', #47082, .T. ) ;
#62783 = FACE_OUTER_BOUND ( 'NONE', #36171, .T. ) ;
#62784 = EDGE_CURVE ( 'NONE', #41411, #72954, #8827, .T. ) ;
#62785 = EDGE_CURVE ( 'NONE', #52790, #3338, #56609, .T. ) ;
#62786 = FACE_OUTER_BOUND ( 'NONE', #69256, .T. ) ;
#62787 = CIRCLE ( 'NONE', #3957, 31.99999999999998934 ) ;
#62788 = CARTESIAN_POINT ( 'NONE',  ( -93.67499999999998295, -207.7050326799711968, 84.07333333333333769 ) ) ;
#62789 = AXIS2_PLACEMENT_3D ( 'NONE', #23808, #70023, #47483 ) ;
#62790 = CARTESIAN_POINT ( 'NONE',  ( -97.65000000000006253, 88.47002178664756400, 79.89291666666666458 ) ) ;
#62791 = VECTOR ( 'NONE', #53614, 1000.000000000000000 ) ;
#62792 = ORIENTED_EDGE ( 'NONE', *, *, #72144, .F. ) ;
#62793 = CYLINDRICAL_SURFACE ( 'NONE', #68382, 77.49899999999999523 ) ;
#62794 = CARTESIAN_POINT ( 'NONE',  ( 2.500000000000000000, 0.000000000000000000, -0.3501037691048548561 ) ) ;
#62795 = CARTESIAN_POINT ( 'NONE',  ( 14.59956846177685996, -138.4757300459248484, 5.500000000000000000 ) ) ;
#62796 = CARTESIAN_POINT ( 'NONE',  ( 22.75000000000000000, 2.789133085058097101E-16, -2.055000000000000160 ) ) ;
#62797 = VECTOR ( 'NONE', #44149, 1000.000000000000000 ) ;
#62798 = AXIS2_PLACEMENT_3D ( 'NONE', #12061, #39532, #34618 ) ;
#62799 = CARTESIAN_POINT ( 'NONE',  ( 92.69370383062501162, -209.9999999999999716, 84.72156250086715090 ) ) ;
#62800 = EDGE_LOOP ( 'NONE', ( #69784, #17768, #41174, #23295 ) ) ;
#62801 = EDGE_LOOP ( 'NONE', ( #31725, #58632, #46871, #49709 ) ) ;
#62802 = LINE ( 'NONE', #67299, #9214 ) ;
#62803 = ORIENTED_EDGE ( 'NONE', *, *, #35702, .F. ) ;
#62804 = DIRECTION ( 'NONE',  ( 0.9038112904824853189, -0.4279312458752977388, 0.000000000000000000 ) ) ;
#62805 = CARTESIAN_POINT ( 'NONE',  ( 92.69370383062501162, -211.3315407142195852, 78.26572916753380582 ) ) ;
#62806 = ORIENTED_EDGE ( 'NONE', *, *, #6174, .F. ) ;
#62807 = CARTESIAN_POINT ( 'NONE',  ( 97.30629616937498838, -211.3315407142195852, 83.71614583420050337 ) ) ;
#62808 = EDGE_LOOP ( 'NONE', ( #69559, #23690, #10363, #5051 ) ) ;
#62809 = DIRECTION ( 'NONE',  ( 0.000000000000000000, 0.000000000000000000, 1.000000000000000000 ) ) ;
#62810 = ORIENTED_EDGE ( 'NONE', *, *, #24929, .F. ) ;
#62811 = ORIENTED_EDGE ( 'NONE', *, *, #61614, .F. ) ;
#62812 = DIRECTION ( 'NONE',  ( -0.6516173805718067369, 0.7585478161175716050, 0.000000000000000000 ) ) ;
#62813 = DIRECTION ( 'NONE',  ( 1.000000000000000000, 0.000000000000000000, 0.000000000000000000 ) ) ;
#62814 = ORIENTED_EDGE ( 'NONE', *, *, #36743, .F. ) ;
#62815 = DIRECTION ( 'NONE',  ( -0.000000000000000000, -0.5877852522924789103, 0.8090169943749432324 ) ) ;
#62816 = CARTESIAN_POINT ( 'NONE',  ( 92.35000000000002274, -211.5299782133524502, 87.59229166840096070 ) ) ;
#62817 = EDGE_LOOP ( 'NONE', ( #38304, #69975, #58024, #12217 ) ) ;
#62818 = DIRECTION ( 'NONE',  ( 1.000000000000000000, 0.000000000000000000, 0.000000000000000000 ) ) ;
#62819 = ORIENTED_EDGE ( 'NONE', *, *, #31719, .F. ) ;
#62820 = CARTESIAN_POINT ( 'NONE',  ( -96.15314808468752972, 91.99731107132950569, 89.69572916753382685 ) ) ;
#62821 = VERTEX_POINT ( 'NONE', #10355 ) ;
#62822 = EDGE_CURVE ( 'NONE', #35621, #2136, #27648, .T. ) ;
#62823 = AXIS2_PLACEMENT_3D ( 'NONE', #47904, #53544, #55020 ) ;
#62824 = EDGE_CURVE ( 'NONE', #44809, #2269, #61025, .T. ) ;
#62825 = VERTEX_POINT ( 'NONE', #44204 ) ;
#62826 = ORIENTED_EDGE ( 'NONE', *, *, #21821, .T. ) ;
#62827 = DIRECTION ( 'NONE',  ( -1.000000000000000000, 0.000000000000000000, -0.000000000000000000 ) ) ;
#62828 = ITEM_DEFINED_TRANSFORMATION ( 'NONE', 'NONE', #42408,  #43395 ) ;
#62829 = CARTESIAN_POINT ( 'NONE',  ( 1.560000000000000053, -0.8660254037844384856, 1.500000000000000000 ) ) ;
#62830 = ORIENTED_EDGE ( 'NONE', *, *, #53128, .T. ) ;
#62831 = AXIS2_PLACEMENT_3D ( 'NONE', #54272, #38450, #42993 ) ;
#62832 = ORIENTED_EDGE ( 'NONE', *, *, #243, .T. ) ;
#62833 = EDGE_CURVE ( 'NONE', #58096, #51229, #22383, .T. ) ;
#62834 = VERTEX_POINT ( 'NONE', #4746 ) ;
#62835 = DIRECTION ( 'NONE',  ( -1.000000000000000000, -0.000000000000000000, 0.000000000000000000 ) ) ;
#62836 = LINE ( 'NONE', #27465, #5926 ) ;
#62837 = EDGE_CURVE ( 'NONE', #60602, #40539, #50952, .T. ) ;
#62838 = CARTESIAN_POINT ( 'NONE',  ( -97.30629616937501680, 90.00000000000004263, 75.83156250086716454 ) ) ;
#62839 = ORIENTED_EDGE ( 'NONE', *, *, #63673, .F. ) ;
#62840 = CARTESIAN_POINT ( 'NONE',  ( 92.69370383062498320, 91.33154071421968467, 74.98489583420048632 ) ) ;
#62841 = AXIS2_PLACEMENT_3D ( 'NONE', #44575, #5476, #55844 ) ;
#62842 = ORIENTED_EDGE ( 'NONE', *, *, #38555, .F. ) ;
#62843 = DIRECTION ( 'NONE',  ( -1.000000000000000000, 0.000000000000000000, 0.000000000000000000 ) ) ;
#62844 = CARTESIAN_POINT ( 'NONE',  ( -96.15314808468745866, -211.9973110713294489, 84.66864583420047552 ) ) ;
#62846 = ORIENTED_EDGE ( 'NONE', *, *, #29189, .F. ) ;
#62845 = ADVANCED_FACE ( 'NONE', ( #44955 ), #38186, .T. ) ;
#62847 = AXIS2_PLACEMENT_3D ( 'NONE', #33142, #27883, #72613 ) ;
#62848 = DIRECTION ( 'NONE',  ( 1.000000000000000000, 0.000000000000000000, -0.000000000000000000 ) ) ;
#62849 = CARTESIAN_POINT ( 'NONE',  ( 93.08933536981351153, -211.7387787020258259, 74.95660481729454716 ) ) ;
#62850 = CARTESIAN_POINT ( 'NONE',  ( 96.32499999999998863, -207.7050326799711968, 87.88333333333332575 ) ) ;
#62851 = CARTESIAN_POINT ( 'NONE',  ( -94.99999999999997158, -207.3369185715606307, 76.14906250086716000 ) ) ;
#62852 = PLANE ( 'NONE',  #71064 ) ;
#62853 = CARTESIAN_POINT ( 'NONE',  ( 10.00000000000000000, 29.01471420065674423, -76.69515212745983490 ) ) ;
#62854 = AXIS2_PLACEMENT_3D ( 'NONE', #30728, #36010, #19085 ) ;
#62855 = VECTOR ( 'NONE', #39450, 1000.000000000000114 ) ;
#62856 = CARTESIAN_POINT ( 'NONE',  ( -97.64999999996712177, 90.00000839536629371, 84.99910573348492449 ) ) ;
#62857 = FACE_OUTER_BOUND ( 'NONE', #67772, .T. ) ;
#62858 = ADVANCED_FACE ( 'NONE', ( #4364 ), #61502, .T. ) ;
#62859 = CARTESIAN_POINT ( 'NONE',  ( -12.50000000000000000, -132.5000000000000000, 40.00000000000000000 ) ) ;
#62860 = EDGE_CURVE ( 'NONE', #65693, #47656, #26898, .T. ) ;
#62861 = CARTESIAN_POINT ( 'NONE',  ( -93.84685191531254134, 91.99731107132950569, 79.90614583420047268 ) ) ;
#62862 = FACE_BOUND ( 'NONE', #29566, .T. ) ;
#62863 = CARTESIAN_POINT ( 'NONE',  ( 0.000000000000000000, 22.07842321921492612, -8.187992925817130896 ) ) ;
#62864 = VERTEX_POINT ( 'NONE', #68253 ) ;
#62865 = CARTESIAN_POINT ( 'NONE',  ( 92.34999999999999432, 88.47002178664752137, 79.33729166840096525 ) ) ;
#62866 = FACE_OUTER_BOUND ( 'NONE', #25989, .T. ) ;
#62867 = DIRECTION ( 'NONE',  ( -1.000000000000000000, -0.000000000000000000, -0.000000000000000000 ) ) ;
#62868 = ADVANCED_FACE ( 'NONE', ( #21634 ), #73502, .F. ) ;
#62869 = EDGE_CURVE ( 'NONE', #46312, #32997, #40643, .T. ) ;
#62870 = DIRECTION ( 'NONE',  ( 0.000000000000000000, -0.4067366430758010409, 0.9135454576426005335 ) ) ;
#62871 = CARTESIAN_POINT ( 'NONE',  ( 11.99999999999999822, 46.11716303203186840, 67.80270845531904911 ) ) ;
#62872 = CARTESIAN_POINT ( 'NONE',  ( -95.00000000000002842, 93.05995642670504253, 85.47562500173430067 ) ) ;
#62873 = CARTESIAN_POINT ( 'NONE',  ( -96.15314808468747287, -208.0026889286704943, 80.17072916753382117 ) ) ;
#62874 = CARTESIAN_POINT ( 'NONE',  ( -95.00000000000002842, 90.00000000000004263, 90.00000000000000000 ) ) ;
#62875 = AXIS2_PLACEMENT_3D ( 'NONE', #47665, #70211, #52943 ) ;
#62876 =( BOUNDED_CURVE ( )  B_SPLINE_CURVE ( 2, ( #64176, #69071, #69429, #57419, #47246, #5930, #52886 ),
 .UNSPECIFIED., .F., .F. ) 
 B_SPLINE_CURVE_WITH_KNOTS ( ( 3, 2, 2, 3 ),
 ( 0.4583333333333335924, 0.4652777777777780122, 0.4722222222222224319, 0.4791666666666668517 ),
 .UNSPECIFIED. ) 
 CURVE ( )  GEOMETRIC_REPRESENTATION_ITEM ( )  RATIONAL_B_SPLINE_CURVE ( ( 0.9999999999999946709, 0.8660254037844440367, 1.000000000000000000, 0.8660254037844387076, 1.000000000000000000, 0.8660254037844354880, 1.000000000000003109 ) ) 
 REPRESENTATION_ITEM ( '' )  );
#62877 = VERTEX_POINT ( 'NONE', #66763 ) ;
#62878 = CARTESIAN_POINT ( 'NONE',  ( 2.750000000000000000, 0.000000000000000000, 4.750000000000000000 ) ) ;
#62879 = DIRECTION ( 'NONE',  ( -0.000000000000000000, -0.000000000000000000, 1.000000000000000000 ) ) ;
#62880 = CARTESIAN_POINT ( 'NONE',  ( 10.00000000000000000, 0.000000000000000000, 0.000000000000000000 ) ) ;
#62881 = PRODUCT_DEFINITION_FORMATION_WITH_SPECIFIED_SOURCE ( 'ANY', '', #37366, .NOT_KNOWN. ) ;
#62882 = CARTESIAN_POINT ( 'NONE',  ( 0.000000000000000000, 37.58145647212455032, -0.6853352020786441789 ) ) ;
#62883 = CIRCLE ( 'NONE', #36440, 31.99999999999998579 ) ;
#62884 = DIRECTION ( 'NONE',  ( -1.000000000000000000, -0.000000000000000000, 0.000000000000000000 ) ) ;
#62885 = ORIENTED_EDGE ( 'NONE', *, *, #11183, .T. ) ;
#62886 = DIRECTION ( 'NONE',  ( 0.000000000000000000, 0.000000000000000000, 1.000000000000000000 ) ) ;
#62887 = DIRECTION ( 'NONE',  ( -1.000000000000000000, -0.000000000000000000, -0.000000000000000000 ) ) ;
#62888 = ORIENTED_EDGE ( 'NONE', *, *, #51288, .T. ) ;
#62889 = VECTOR ( 'NONE', #28197, 1000.000000000000000 ) ;
#62890 = CARTESIAN_POINT ( 'NONE',  ( 93.84685191531249870, -208.0026889286704943, 86.99697916753380866 ) ) ;
#62891 = CARTESIAN_POINT ( 'NONE',  ( -97.64999999999996305, -209.9999999999999716, 83.72937500173429726 ) ) ;
#62892 = MANIFOLD_SOLID_BREP ( 'Hex', #19950 ) ;
#62893 = AXIS2_PLACEMENT_3D ( 'NONE', #37967, #10794, #28820 ) ;
#62894 = VERTEX_POINT ( 'NONE', #34395 ) ;
#62895 = EDGE_CURVE ( 'NONE', #46530, #8777, #28011, .T. ) ;
#62896 = DIRECTION ( 'NONE',  ( 0.000000000000000000, 0.8910065241883656784, 0.4539904997395510788 ) ) ;
#62897 = ORIENTED_EDGE ( 'NONE', *, *, #66902, .F. ) ;
#62898 = VECTOR ( 'NONE', #34075, 1000.000000000000000 ) ;
#62899 = CARTESIAN_POINT ( 'NONE',  ( 95.00000000000000000, -213.0599564267049857, 85.15812500173429100 ) ) ;
#62900 = VERTEX_POINT ( 'NONE', #17115 ) ;
#62901 = VECTOR ( 'NONE', #32764, 1000.000000000000000 ) ;
#62902 = CARTESIAN_POINT ( 'NONE',  ( -92.34999999999999432, -210.0000000983656605, 80.23687499810813506 ) ) ;
#62903 = EDGE_LOOP ( 'NONE', ( #30995, #4822, #8683, #39935 ) ) ;
#62904 = DIRECTION ( 'NONE',  ( -1.000000000000000000, -0.000000000000000000, -0.000000000000000000 ) ) ;
#62905 = ORIENTED_EDGE ( 'NONE', *, *, #2783, .T. ) ;
#62906 = ADVANCED_FACE ( 'NONE', ( #51695 ), #35141, .T. ) ;
#62907 = ORIENTED_EDGE ( 'NONE', *, *, #61371, .T. ) ;
#62908 = DIRECTION ( 'NONE',  ( 1.000000000000000000, 0.000000000000000000, 0.000000000000000000 ) ) ;
#62909 = EDGE_CURVE ( 'NONE', #7483, #27087, #17482, .T. ) ;
#62910 = ORIENTED_EDGE ( 'NONE', *, *, #59106, .F. ) ;
#62911 = ORIENTED_EDGE ( 'NONE', *, *, #7906, .F. ) ;
#62912 = DIRECTION ( 'NONE',  ( -1.000000000000000000, -0.000000000000000000, -0.000000000000000000 ) ) ;
#62913 = CARTESIAN_POINT ( 'NONE',  ( 10.00000000000000000, 30.00120703465236716, -22.64427369931138756 ) ) ;
#62914 = VERTEX_POINT ( 'NONE', #52809 ) ;
#62915 = CIRCLE ( 'NONE', #47277, 82.00000000000000000 ) ;
#62916 = EDGE_CURVE ( 'NONE', #61359, #70648, #35846, .T. ) ;
#62917 = ORIENTED_EDGE ( 'NONE', *, *, #19242, .F. ) ;
#62918 = CARTESIAN_POINT ( 'NONE',  ( 97.30629616937498838, 88.66845928578037217, 83.55739583420047722 ) ) ;
#62919 = ORIENTED_EDGE ( 'NONE', *, *, #50737, .F. ) ;
#62920 = CARTESIAN_POINT ( 'NONE',  ( 96.15314808468748708, -208.0026889286704943, 85.62114583420046188 ) ) ;
#62921 = PRODUCT_CONTEXT ( 'NONE', #36427, 'mechanical' ) ;
#62922 = CARTESIAN_POINT ( 'NONE',  ( -96.32499999999996021, -207.7050326799711968, 76.55916666666666970 ) ) ;
#62923 = CARTESIAN_POINT ( 'NONE',  ( -97.64999999999996305, -209.9999999999999716, 83.01499999999998636 ) ) ;
#62924 = CARTESIAN_POINT ( 'NONE',  ( -6.782329983125270800, 10.49999999999999467, 20.00000000000000000 ) ) ;
#62925 = DIRECTION ( 'NONE',  ( 0.000000000000000000, -0.7431448254773953543, -0.6691306063588570163 ) ) ;
#62926 = CARTESIAN_POINT ( 'NONE',  ( 10.00000000000000000, -21.60688246758529019, -79.10210256391388839 ) ) ;
#62927 = DIRECTION ( 'NONE',  ( -1.000000000000000000, -0.000000000000000000, 0.000000000000000000 ) ) ;
#62928 = CARTESIAN_POINT ( 'NONE',  ( -94.99999999999997158, -212.6630814284392557, 87.89656250086713385 ) ) ;
#62929 = CARTESIAN_POINT ( 'NONE',  ( -93.84685191531252713, 88.00268892867056536, 86.20322916753382003 ) ) ;
#62930 = ORIENTED_EDGE ( 'NONE', *, *, #51726, .T. ) ;
#62931 = AXIS2_PLACEMENT_3D ( 'NONE', #16493, #28885, #5236 ) ;
#62933 = CARTESIAN_POINT ( 'NONE',  ( -93.84685191531254134, 91.99731107132950569, 83.71614583420047495 ) ) ;
#62932 = CARTESIAN_POINT ( 'NONE',  ( 97.30629616937498838, 91.33154071421968467, 83.66322916753379957 ) ) ;
#62934 = ORIENTED_EDGE ( 'NONE', *, *, #27334, .F. ) ;
#62935 = CARTESIAN_POINT ( 'NONE',  ( -92.35000000000000853, 91.52997821335252127, 87.83041666666669300 ) ) ;
#62936 = EDGE_CURVE ( 'NONE', #52621, #63423, #40795, .T. ) ;
#62937 = CARTESIAN_POINT ( 'NONE',  ( 92.35000000006147047, -209.9999881782113107, 76.10900611559200968 ) ) ;
#62938 = FACE_OUTER_BOUND ( 'NONE', #9320, .T. ) ;
#62939 = DIRECTION ( 'NONE',  ( -0.000000000000000000, -0.000000000000000000, 1.000000000000000000 ) ) ;
#62940 = CARTESIAN_POINT ( 'NONE',  ( -97.30629616937497417, -208.6684592857803295, 87.04989583420046984 ) ) ;
#62941 = AXIS2_PLACEMENT_3D ( 'NONE', #54613, #14005, #7278 ) ;
#62942 = CARTESIAN_POINT ( 'NONE',  ( 93.67500000000001137, -207.7050326799711968, 82.27416666666665890 ) ) ;
#62943 = DIRECTION ( 'NONE',  ( -0.000000000000000000, -0.000000000000000000, 1.000000000000000000 ) ) ;
#62944 = DIRECTION ( 'NONE',  ( -1.000000000000000000, -0.000000000000000000, -0.000000000000000000 ) ) ;
#62945 = DIRECTION ( 'NONE',  ( 1.000000000000000000, -7.571541139944063212E-15, -2.603472992745718826E-14 ) ) ;
#62946 = ORIENTED_EDGE ( 'NONE', *, *, #32434, .F. ) ;
#62947 = ORIENTED_EDGE ( 'NONE', *, *, #6642, .F. ) ;
#62948 = CARTESIAN_POINT ( 'NONE',  ( -97.65000000000001990, 90.00000000000004263, 76.66499999999999204 ) ) ;
#62949 = EDGE_CURVE ( 'NONE', #70635, #70258, #38267, .T. ) ;
#62950 = CARTESIAN_POINT ( 'NONE',  ( 11.99999999999999822, 0.000000000000000000, 0.000000000000000000 ) ) ;
#62951 = EDGE_CURVE ( 'NONE', #71724, #19049, #40046, .T. ) ;
#62952 = CYLINDRICAL_SURFACE ( 'NONE', #28616, 12.49999999999999645 ) ;
#62953 = CARTESIAN_POINT ( 'NONE',  ( -96.32499999999996021, -212.2949673200287179, 76.85020833506763438 ) ) ;
#62954 = LINE ( 'NONE', #7535, #39962 ) ;
#62955 = CARTESIAN_POINT ( 'NONE',  ( 10.00000000000000000, 37.58145647212453611, 16.68533520207917675 ) ) ;
#62956 = VECTOR ( 'NONE', #37915, 1000.000000000000000 ) ;
#62957 = DIRECTION ( 'NONE',  ( 0.000000000000000000, 0.6691306063588563502, 0.7431448254773960205 ) ) ;
#62958 = ADVANCED_FACE ( 'NONE', ( #52058, #601, #17846 ), #23138, .T. ) ;
#62959 = AXIS2_PLACEMENT_3D ( 'NONE', #35838, #24571, #40376 ) ;
#62960 = VERTEX_POINT ( 'NONE', #63007 ) ;
#62961 = CARTESIAN_POINT ( 'NONE',  ( -97.30629616937501680, 91.33154071421968467, 77.52489583420046415 ) ) ;
#62962 = DIRECTION ( 'NONE',  ( 0.8774505977381983346, 0.4796670183876293736, 0.000000000000000000 ) ) ;
#62963 = VECTOR ( 'NONE', #2126, 1000.000000000000000 ) ;
#62964 = CARTESIAN_POINT ( 'NONE',  ( 0.000000000000000000, -41.19522573413689059, -65.64334221924951862 ) ) ;
#62965 = DIRECTION ( 'NONE',  ( -1.000000000000000000, 0.000000000000000000, -0.000000000000000000 ) ) ;
#62966 = CYLINDRICAL_SURFACE ( 'NONE', #40485, 2.649999999999985700 ) ;
#62967 = CARTESIAN_POINT ( 'NONE',  ( -97.64999999994218172, 89.99998877583867340, 75.47473230081648410 ) ) ;
#62968 = LINE ( 'NONE', #22343, #62240 ) ;
#62969 = CARTESIAN_POINT ( 'NONE',  ( 92.69370383062498320, 91.33154071421968467, 78.31864583420050963 ) ) ;
#62970 = AXIS2_PLACEMENT_3D ( 'NONE', #62543, #44502, #44871 ) ;
#62971 = CARTESIAN_POINT ( 'NONE',  ( -97.30629616937497417, -211.3315407142195852, 78.42447916753380355 ) ) ;
#62972 = CARTESIAN_POINT ( 'NONE',  ( 0.000000000000000000, 0.000000000000000000, 0.000000000000000000 ) ) ;
#62973 = ORIENTED_EDGE ( 'NONE', *, *, #49624, .T. ) ;
#62974 = CARTESIAN_POINT ( 'NONE',  ( 96.32499999999998863, -207.7050326799711968, 80.97770833506763211 ) ) ;
#62975 = CARTESIAN_POINT ( 'NONE',  ( 0.000000000000000000, -120.0000000000000000, -40.00000000000000711 ) ) ;
#62976 = FACE_OUTER_BOUND ( 'NONE', #37095, .T. ) ;
#62977 = DIRECTION ( 'NONE',  ( -1.000000000000000000, -0.000000000000000000, -0.000000000000000000 ) ) ;
#62978 = CARTESIAN_POINT ( 'NONE',  ( 92.69370383062501162, -209.9999999999999716, 81.38781250086714181 ) ) ;
#62979 = ORIENTED_EDGE ( 'NONE', *, *, #9579, .F. ) ;
#62980 = EDGE_CURVE ( 'NONE', #49355, #25988, #974, .T. ) ;
#62981 = CIRCLE ( 'NONE', #5339, 31.99999999999999289 ) ;
#62982 = DIRECTION ( 'NONE',  ( 0.000000000000000000, 0.000000000000000000, 1.000000000000000000 ) ) ;
#62983 = ORIENTED_EDGE ( 'NONE', *, *, #63245, .T. ) ;
#62984 = CARTESIAN_POINT ( 'NONE',  ( -3.000000000000000000, -19.89357724624987256, -12.59942793731086041 ) ) ;
#62985 = ORIENTED_EDGE ( 'NONE', *, *, #40937, .T. ) ;
#62986 = CYLINDRICAL_SURFACE ( 'NONE', #44213, 2.649999999999999467 ) ;
#62987 = AXIS2_PLACEMENT_3D ( 'NONE', #14228, #25884, #43575 ) ;
#62988 = ORIENTED_EDGE ( 'NONE', *, *, #50593, .F. ) ;
#62989 = VERTEX_POINT ( 'NONE', #6932 ) ;
#62990 = ADVANCED_FACE ( 'NONE', ( #23864 ), #1352, .T. ) ;
#62991 = ORIENTED_EDGE ( 'NONE', *, *, #56366, .F. ) ;
#62992 = DIRECTION ( 'NONE',  ( -0.000000000000000000, -0.000000000000000000, -1.000000000000000000 ) ) ;
#62993 = EDGE_CURVE ( 'NONE', #34951, #73248, #47169, .T. ) ;
#62994 = ORIENTED_EDGE ( 'NONE', *, *, #47883, .T. ) ;
#62995 = CIRCLE ( 'NONE', #26948, 37.49900000000000944 ) ;
#62996 = ORIENTED_EDGE ( 'NONE', *, *, #19114, .T. ) ;
#62997 = CARTESIAN_POINT ( 'NONE',  ( 94.99999999999998579, 87.33691857156068750, 81.70531250086715147 ) ) ;
#62998 = CIRCLE ( 'NONE', #30547, 17.50000000000000355 ) ;
#62999 = CARTESIAN_POINT ( 'NONE',  ( 95.00000000000000000, -213.0599564267049857, 77.45874999999999488 ) ) ;
#63000 = ORIENTED_EDGE ( 'NONE', *, *, #5012, .T. ) ;
#63001 = EDGE_CURVE ( 'NONE', #19051, #12910, #41521, .T. ) ;
#63002 = VERTEX_POINT ( 'NONE', #22769 ) ;
#63003 = EDGE_CURVE ( 'NONE', #34558, #49532, #68992, .T. ) ;
#63004 = VERTEX_POINT ( 'NONE', #28757 ) ;
#63005 = AXIS2_PLACEMENT_3D ( 'NONE', #15489, #27125, #50805 ) ;
#63006 = ORIENTED_EDGE ( 'NONE', *, *, #69258, .F. ) ;
#63007 = CARTESIAN_POINT ( 'NONE',  ( 7.999999999999974243, -2.326479307499132695E-13, -22.90000000000041069 ) ) ;
#63008 =( NAMED_UNIT ( * ) PLANE_ANGLE_UNIT ( ) SI_UNIT ( $, .RADIAN. ) );
#63009 = DIRECTION ( 'NONE',  ( -2.628368902995164490E-16, -1.000000000000000000, 0.000000000000000000 ) ) ;
#63010 = CARTESIAN_POINT ( 'NONE',  ( -93.25528180581933668, 88.31889241252943634, 74.86350982016035971 ) ) ;
#63011 = CARTESIAN_POINT ( 'NONE',  ( 0.000000000000000000, 71.91182617369230456, -28.89263327155667938 ) ) ;
#63012 = AXIS2_PLACEMENT_3D ( 'NONE', #17341, #4972, #6443 ) ;
#63013 = LINE ( 'NONE', #41530, #33563 ) ;
#63014 = FACE_OUTER_BOUND ( 'NONE', #43394, .T. ) ;
#63015 = VERTEX_POINT ( 'NONE', #34776 ) ;
#63016 = CARTESIAN_POINT ( 'NONE',  ( -93.67499999999998295, -207.7050326799711968, 82.24770833506762813 ) ) ;
#63017 = VERTEX_POINT ( 'NONE', #57714 ) ;
#63018 = DIRECTION ( 'NONE',  ( -1.000000000000000000, -0.000000000000000000, -0.000000000000000000 ) ) ;
#63019 = CIRCLE ( 'NONE', #4183, 37.49900000000000233 ) ;
#63020 = ORIENTED_EDGE ( 'NONE', *, *, #3828, .T. ) ;
#63022 = CARTESIAN_POINT ( 'NONE',  ( -92.35000000000003695, 90.00000000000004263, 78.33187500173430351 ) ) ;
#63021 = CARTESIAN_POINT ( 'NONE',  ( 97.64999999999999147, 90.00000000000002842, 80.23687500173429044 ) ) ;
#63023 = ORIENTED_EDGE ( 'NONE', *, *, #38523, .F. ) ;
#63024 = CARTESIAN_POINT ( 'NONE',  ( 93.84685191531248449, 91.99731107132950569, 79.53572916753381605 ) ) ;
#63025 = EDGE_CURVE ( 'NONE', #8298, #25226, #6220, .T. ) ;
#63026 = DIRECTION ( 'NONE',  ( -1.000000000000000000, -0.000000000000000000, -0.000000000000000000 ) ) ;
#63027 = CIRCLE ( 'NONE', #34179, 82.00000000000000000 ) ;
#63028 = FACE_OUTER_BOUND ( 'NONE', #8915, .T. ) ;
#63029 = ORIENTED_EDGE ( 'NONE', *, *, #25190, .F. ) ;
#63030 = DIRECTION ( 'NONE',  ( 0.000000000000000000, 0.000000000000000000, -1.000000000000000000 ) ) ;
#63031 = CARTESIAN_POINT ( 'NONE',  ( -92.34999999999998010, -209.9999999999999716, 75.00000000000000000 ) ) ;
#63032 = DIRECTION ( 'NONE',  ( 0.000000000000000000, 0.8090169943749486725, -0.5877852522924713607 ) ) ;
#63033 = VERTEX_POINT ( 'NONE', #58821 ) ;
#63034 = EDGE_LOOP ( 'NONE', ( #40590, #16394, #53298, #45077 ) ) ;
#63035 = EDGE_CURVE ( 'NONE', #7392, #3697, #13038, .T. ) ;
#63036 = EDGE_CURVE ( 'NONE', #18829, #54942, #43069, .T. ) ;
#63037 = DIRECTION ( 'NONE',  ( 2.603472992746261562E-14, 2.546204323184492723E-14, -1.000000000000000000 ) ) ;
#63038 = ADVANCED_FACE ( 'NONE', ( #64460 ), #70822, .F. ) ;
#63039 = DIRECTION ( 'NONE',  ( 1.000000000000000000, 0.000000000000000000, 0.000000000000000000 ) ) ;
#63040 = CARTESIAN_POINT ( 'NONE',  ( 92.35000000000000853, -209.9999999999999716, 90.00000000000000000 ) ) ;
#63041 = CARTESIAN_POINT ( 'NONE',  ( -96.15314808468745866, -211.9973110713294489, 82.28739583420048120 ) ) ;
#63042 = VERTEX_POINT ( 'NONE', #36990 ) ;
#63043 = ORIENTED_EDGE ( 'NONE', *, *, #56744, .F. ) ;
#63044 = DIRECTION ( 'NONE',  ( 0.000000000000000000, 0.000000000000000000, 1.000000000000000000 ) ) ;
#63045 = VECTOR ( 'NONE', #40887, 1000.000000000000000 ) ;
#63046 = DIRECTION ( 'NONE',  ( 1.000000000000000000, 0.000000000000000000, 0.000000000000000000 ) ) ;
#63047 = CARTESIAN_POINT ( 'NONE',  ( 0.000000000000000000, -56.15606465355000410, 59.75363087400056372 ) ) ;
#63048 = CARTESIAN_POINT ( 'NONE',  ( 92.69370383062498320, 91.33154071421968467, 75.61989583420047722 ) ) ;
#63049 = DIRECTION ( 'NONE',  ( -1.000000000000000000, 0.000000000000000000, -0.000000000000000000 ) ) ;
#63050 = DIRECTION ( 'NONE',  ( -1.000000000000000000, 0.000000000000000000, -0.000000000000000000 ) ) ;
#63051 = CARTESIAN_POINT ( 'NONE',  ( 0.000000000000000000, 46.53671651293948486, 59.03961581697416250 ) ) ;
#63052 = FACE_OUTER_BOUND ( 'NONE', #53158, .T. ) ;
#63053 = DIRECTION ( 'NONE',  ( -1.000000000000000000, 0.000000000000000000, 0.000000000000000000 ) ) ;
#63054 = CARTESIAN_POINT ( 'NONE',  ( 11.99999999999999822, -75.11764819372145041, -2.946379043147127064 ) ) ;
#63055 = CIRCLE ( 'NONE', #57026, 12.49999999999999645 ) ;
#63056 = AXIS2_PLACEMENT_3D ( 'NONE', #48914, #15443, #33098 ) ;
#63057 = CARTESIAN_POINT ( 'NONE',  ( 97.30629616937498838, 91.33154071421968467, 85.72697916753381264 ) ) ;
#63058 = CARTESIAN_POINT ( 'NONE',  ( -94.99999999999997158, -207.3369185715606307, 88.37281250086715545 ) ) ;
#63059 = CARTESIAN_POINT ( 'NONE',  ( 92.34999999999999432, 88.47002178664752137, 82.43291666666665662 ) ) ;
#63060 = ORIENTED_EDGE ( 'NONE', *, *, #18069, .F. ) ;
#63061 = CYLINDRICAL_SURFACE ( 'NONE', #68882, 82.00000000000000000 ) ;
#63062 = CARTESIAN_POINT ( 'NONE',  ( -95.00000000000002842, 92.66308142843932671, 78.05406250086714692 ) ) ;
#63063 = AXIS2_PLACEMENT_3D ( 'NONE', #52579, #16614, #45203 ) ;
#63064 = VECTOR ( 'NONE', #6348, 1000.000000000000000 ) ;
#63065 = CARTESIAN_POINT ( 'NONE',  ( 11.99999999999999822, -11.30684508768393748, 76.66974797899833050 ) ) ;
#63066 = EDGE_CURVE ( 'NONE', #27978, #39783, #5888, .T. ) ;
#63067 = ORIENTED_EDGE ( 'NONE', *, *, #3163, .T. ) ;
#63068 = DIRECTION ( 'NONE',  ( 0.000000000000000000, 0.000000000000000000, 1.000000000000000000 ) ) ;
#63069 = CARTESIAN_POINT ( 'NONE',  ( 0.000000000000000000, 77.32052557432841411, 5.256550761633121738 ) ) ;
#63070 = CIRCLE ( 'NONE', #6638, 21.00000000000000000 ) ;
#63071 = EDGE_CURVE ( 'NONE', #54637, #28318, #33483, .T. ) ;
#63072 = CARTESIAN_POINT ( 'NONE',  ( -7.499999999999969802, 73.00000000000001421, -204.9999999999999716 ) ) ;
#63073 = CARTESIAN_POINT ( 'NONE',  ( 93.84685191531249870, -208.0026889286704943, 76.99572916753382401 ) ) ;
#63074 = ADVANCED_FACE ( 'NONE', ( #30595 ), #48273, .T. ) ;
#63075 = VERTEX_POINT ( 'NONE', #47535 ) ;
#63076 = EDGE_CURVE ( 'NONE', #73949, #69471, #54652, .T. ) ;
#63077 = ORIENTED_EDGE ( 'NONE', *, *, #13167, .F. ) ;
#63078 = CARTESIAN_POINT ( 'NONE',  ( 96.15314808468748708, -208.0026889286704943, 85.14489583420048291 ) ) ;
#63079 = DIRECTION ( 'NONE',  ( 0.000000000000000000, 0.7071067811865487940, -0.7071067811865462405 ) ) ;
#63080 = DIRECTION ( 'NONE',  ( 0.000000000000000000, 0.5877852522924685852, 0.8090169943749508930 ) ) ;
#63081 =( BOUNDED_CURVE ( )  B_SPLINE_CURVE ( 2, ( #14655, #51008, #68308, #73931, #31941, #22442, #3405, #26306, #33322, #45385, #31206, #49238, #21686, #44642, #2688, #25569, #52113, #57391, #69771, #293, #23548, #58126, #28817, #40851, #52476, #35561, #46477, #69400, #40102, #6627, #11516, #23187, #5905, #63785, #70131, #1025, #58491, #6986, #34448, #29538, #18273, #29909, #39741, #51746, #28437, #45759, #68684, #23917, #34833, #35193, #17900, #52862, #46859, #62689, #11160, #47221, #34082, #46114, #57028, #5538, #12623, #12260, #11880, #51369, #41210, #69049, #64148, #74306, #17533, #57765, #1400, #40463, #63410, #24294, #22821, #17169, #6271, #63057, #29169, #655, #25399, #31761, #8098, #14478, #2867, #24653, #2133, #48690, #41953, #1766, #71613, #3233, #31019, #7368, #59615, #8479, #42688, #70876, #54344, #53594, #64891, #2517, #19375, #26123, #53973, #25761, #14098, #37046, #48326, #65627, #20111, #37430, #7733, #70488, #30648, #59994, #36669, #18632, #59240, #30285, #65259, #25015, #31392, #41571, #71235, #47958, #43070, #66004, #42326, #19740, #60362, #8846, #54704, #49058, #64512, #12988, #13731, #35926, #58876, #53230, #47584, #18999, #13365, #36298, #61836, #21593, #49789, #33236, #32505, #43812, #67841, #56188, #66370, #21971, #44920, #27611, #50540, #61466, #38529, #15959, #72359, #60729, #16333, #44169, #66729, #9584, #55445, #27974, #3602, #4706, #72709, #44548, #9207, #67466, #61087, #39275, #5075, #10690, #15219, #73463, #3964, #67090, #62204, #55817, #32126, #33619, #38150, #56576, #71984, #26862, #15593, #38898, #55068, #10319, #21215, #20499, #9946, #73089, #43450, #14849, #4330, #37796, #26502, #49430, #32867, #27223, #20855, #50157, #22347, #51658, #205, #63323, #6903, #50911, #33993, #41128, #73835, #62969, #39646, #56939, #5447, #23098, #28344, #57681, #22729, #34359, #57303, #23826, #64062, #58403, #34737, #63696, #35472, #29445, #18184, #51280, #12535, #40372, #46766, #35107, #74214, #11425, #46029, #52388, #12169, #45296, #5813, #566, #17081, #23460, #45668, #46389, #936, #68594, #69315, #68215, #6184, #11786, #40016, #16707, #68958, #69687, #29081, #17444, #17807, #28719, #52018, #40755, #62591, #58036, #6542, #11070, #70044, #65913, #20019, #41482, #71146, #30562, #65169, #2421, #53138, #37336, #42975, #24566, #59902, #13278, #12901 ),
 .UNSPECIFIED., .F., .F. ) 
 B_SPLINE_CURVE_WITH_KNOTS ( ( 3, 2, 2, 2, 2, 2, 2, 2, 2, 2, 2, 2, 2, 2, 2, 2, 2, 2, 2, 2, 2, 2, 2, 2, 2, 2, 2, 2, 2, 2, 2, 2, 2, 2, 2, 2, 2, 2, 2, 2, 2, 2, 2, 2, 2, 2, 2, 2, 2, 2, 2, 2, 2, 2, 2, 2, 2, 2, 2, 2, 2, 2, 2, 2, 2, 2, 2, 2, 2, 2, 2, 2, 2, 2, 2, 2, 2, 2, 2, 2, 2, 2, 2, 2, 2, 2, 2, 2, 2, 2, 2, 2, 2, 2, 2, 2, 2, 2, 2, 2, 2, 2, 2, 2, 2, 2, 2, 2, 2, 2, 2, 2, 2, 2, 2, 2, 2, 2, 2, 2, 2, 2, 2, 2, 2, 2, 2, 2, 2, 2, 2, 2, 2, 2, 2, 2, 2, 2, 2, 2, 2, 2, 2, 3 ),
 ( 0.000000000000000000, 0.007055764916269564521, 0.01411152983253912904, 0.02116729474880869530, 0.02822305966507825808, 0.03527882458134782434, 0.04233458949761739060, 0.04939035441388695685, 0.05644611933015651617, 0.06350188424642608243, 0.07055764916269564868, 0.07761341407896522882, 0.08466917899523478119, 0.09172494391150434745, 0.09878070882777391370, 0.1058364737440434800, 0.1128922386603130323, 0.1199480035765825986, 0.1270037684928521649, 0.1340595334091217450, 0.1411152983253912974, 0.1481710632416608775, 0.1552268281579304576, 0.1622825930741999823, 0.1693383579904695624, 0.1763941229067391148, 0.1834498878230086949, 0.1905056527392782473, 0.1975614176555478274, 0.2046171825718174075, 0.2116729474880869599, 0.2187287124043565401, 0.2257844773206260647, 0.2328402422368956448, 0.2398960071531651972, 0.2469517720694347773, 0.2540075369857043297, 0.2610633019019739098, 0.2681190668182434900, 0.2751748317345130146, 0.2822305966507825947, 0.2892863615670521749, 0.2963421264833217550, 0.3033978913995912796, 0.3104536563158609153, 0.3175094212321304399, 0.3245651861483999645, 0.3316209510646695446, 0.3386767159809391248, 0.3457324808972087049, 0.3527882458134782295, 0.3598440107297478652, 0.3668997756460173898, 0.3739555405622869699, 0.3810113054785564946, 0.3880670703948260747, 0.3951228353110956548, 0.4021786002273651794, 0.4092343651436348151, 0.4162901300599043397, 0.4233458949761739198, 0.4304016598924434445, 0.4374574248087130801, 0.4445131897249826047, 0.4515689546412521294, 0.4586247195575217650, 0.4656804844737912896, 0.4727362493900608698, 0.4797920143063303944, 0.4868477792226000300, 0.4939035441388695546, 0.5009593090551391903, 0.5080150739714086594, 0.5150708388876782395, 0.5221266038039478197, 0.5291823687202173998, 0.5362381336364869799, 0.5432938985527564490, 0.5503496634690260292, 0.5574054283852957203, 0.5644611933015651895, 0.5715169582178347696, 0.5785727231341043497, 0.5856284880503738188, 0.5926842529666435100, 0.5997400178829130901, 0.6067957827991825592, 0.6138515477154521394, 0.6209073126317218305, 0.6279630775479912996, 0.6350188424642608798, 0.6420746073805303489, 0.6491303722967999290, 0.6561861372130696202, 0.6632419021293390893, 0.6702976670456086694, 0.6773534319618782495, 0.6844091968781478297, 0.6914649617944174098, 0.6985207267106869899, 0.7055764916269564591, 0.7126322565432260392, 0.7196880214594957303, 0.7267437863757651995, 0.7337995512920347796, 0.7408553162083042487, 0.7479110811245739399, 0.7549668460408435200, 0.7620226109571129891, 0.7690783758733825692, 0.7761341407896521494, 0.7831899057059217295, 0.7902456706221913096, 0.7973014355384608898, 0.8043572004547303589, 0.8114129653710000500, 0.8184687302872696302, 0.8255244952035390993, 0.8325802601198086794, 0.8396360250360781485, 0.8466917899523478397, 0.8537475548686174198, 0.8608033197848868889, 0.8678590847011564691, 0.8749148496174261602, 0.8819706145336956293, 0.8890263794499652095, 0.8960821443662347896, 0.9031379092825042587, 0.9101936741987739499, 0.9172494391150435300, 0.9243052040313129991, 0.9313609689475825792, 0.9384167338638521594, 0.9454724987801217395, 0.9525282636963913196, 0.9595840286126607888, 0.9666397935289303689, 0.9736955584452000600, 0.9807513233614695292, 0.9878070882777391093, 0.9948628531940086894, 0.9999999123559569769, 1.000000000000000000 ),
 .UNSPECIFIED. ) 
 CURVE ( )  GEOMETRIC_REPRESENTATION_ITEM ( )  RATIONAL_B_SPLINE_CURVE ( ( 1.000000000000000000, 0.8660254037844387076, 1.000000000000000000, 0.8660254037844387076, 1.000000000000000000, 0.8660254037844387076, 1.000000000000000000, 0.8660254037844387076, 1.000000000000000000, 0.8660254037844387076, 1.000000000000000000, 0.8660254037844387076, 1.000000000000000000, 0.8660254037844387076, 1.000000000000000000, 0.8660254037844387076, 1.000000000000000000, 0.8660254037844387076, 1.000000000000000000, 0.8660254037844387076, 1.000000000000000000, 0.8660254037844387076, 1.000000000000000000, 0.8660254037844387076, 1.000000000000000000, 0.8660254037844387076, 1.000000000000000000, 0.8660254037844387076, 1.000000000000000000, 0.8660254037844387076, 1.000000000000000000, 0.8660254037844387076, 1.000000000000000000, 0.8660254037844387076, 1.000000000000000000, 0.8660254037844387076, 1.000000000000000000, 0.8660254037844387076, 1.000000000000000000, 0.8660254037844387076, 1.000000000000000000, 0.8660254037844387076, 1.000000000000000000, 0.8660254037844387076, 1.000000000000000000, 0.8660254037844387076, 1.000000000000000000, 0.8660254037844387076, 1.000000000000000000, 0.8660254037844387076, 1.000000000000000000, 0.8660254037844387076, 1.000000000000000000, 0.8660254037844387076, 1.000000000000000000, 0.8660254037844387076, 1.000000000000000000, 0.8660254037844387076, 1.000000000000000000, 0.8660254037844387076, 1.000000000000000000, 0.8660254037844387076, 1.000000000000000000, 0.8660254037844387076, 1.000000000000000000, 0.8660254037844387076, 1.000000000000000000, 0.8660254037844387076, 1.000000000000000000, 0.8660254037844387076, 1.000000000000000000, 0.8660254037844387076, 1.000000000000000000, 0.8660254037844387076, 1.000000000000000000, 0.8660254037844387076, 1.000000000000000000, 0.8660254037844387076, 1.000000000000000000, 0.8660254037844387076, 1.000000000000000000, 0.8660254037844387076, 1.000000000000000000, 0.8660254037844387076, 1.000000000000000000, 0.8660254037844387076, 1.000000000000000000, 0.8660254037844387076, 1.000000000000000000, 0.8660254037844387076, 1.000000000000000000, 0.8660254037844387076, 1.000000000000000000, 0.8660254037844387076, 1.000000000000000000, 0.8660254037844387076, 1.000000000000000000, 0.8660254037844387076, 1.000000000000000000, 0.8660254037844387076, 1.000000000000000000, 0.8660254037844387076, 1.000000000000000000, 0.8660254037844387076, 1.000000000000000000, 0.8660254037844387076, 1.000000000000000000, 0.8660254037844387076, 1.000000000000000000, 0.8660254037844387076, 1.000000000000000000, 0.8660254037844387076, 1.000000000000000000, 0.8660254037844387076, 1.000000000000000000, 0.8660254037844387076, 1.000000000000000000, 0.8660254037844387076, 1.000000000000000000, 0.8660254037844387076, 1.000000000000000000, 0.8660254037844387076, 1.000000000000000000, 0.8660254037844387076, 1.000000000000000000, 0.8660254037844387076, 1.000000000000000000, 0.8660254037844387076, 1.000000000000000000, 0.8660254037844387076, 1.000000000000000000, 0.8660254037844387076, 1.000000000000000000, 0.8660254037844387076, 1.000000000000000000, 0.8660254037844387076, 1.000000000000000000, 0.8660254037844387076, 1.000000000000000000, 0.8660254037844387076, 1.000000000000000000, 0.8660254037844387076, 1.000000000000000000, 0.8660254037844387076, 1.000000000000000000, 0.8660254037844387076, 1.000000000000000000, 0.8660254037844387076, 1.000000000000000000, 0.8660254037844387076, 1.000000000000000000, 0.8660254037844387076, 1.000000000000000000, 0.8660254037844387076, 1.000000000000000000, 0.8660254037844387076, 1.000000000000000000, 0.8660254037844387076, 1.000000000000000000, 0.8660254037844387076, 1.000000000000000000, 0.8660254037844387076, 1.000000000000000000, 0.8660254037844387076, 1.000000000000000000, 0.8660254037844387076, 1.000000000000000000, 0.8660254037844387076, 1.000000000000000000, 0.8660254037844387076, 1.000000000000000000, 0.8660254037844387076, 1.000000000000000000, 0.8660254037844387076, 1.000000000000000000, 0.8660254037844387076, 1.000000000000000000, 0.8660254037844387076, 1.000000000000000000, 0.8660254037844387076, 1.000000000000000000, 0.8660254037844387076, 1.000000000000000000, 0.8660254037844387076, 1.000000000000000000, 0.8660254037844387076, 1.000000000000000000, 0.8660254037844387076, 1.000000000000000000, 0.8660254037844387076, 1.000000000000000000, 0.8660254037844387076, 1.000000000000000000, 0.8660254037844387076, 1.000000000000000000, 0.8660254037844387076, 1.000000000000000000, 0.8660254037844387076, 1.000000000000000000, 0.8660254037844387076, 1.000000000000000000, 0.8660254037844387076, 1.000000000000000000, 0.8660254037844387076, 1.000000000000000000, 0.8660254037844387076, 1.000000000000000000, 0.8660254037844387076, 1.000000000000000000, 0.8660254037844387076, 1.000000000000000000, 0.8660254037844387076, 1.000000000000000000, 0.8660254037844387076, 1.000000000000000000, 0.8660254037844387076, 1.000000000000000000, 0.8660254037844387076, 1.000000000000000000, 0.8660254037844387076, 1.000000000000000000, 0.8660254037844387076, 1.000000000000000000, 0.8660254037844387076, 1.000000000000000000, 0.8660254037844387076, 1.000000000000000000, 0.8660254037844387076, 1.000000000000000000, 0.8660254037844387076, 1.000000000000000000, 0.8660254037844387076, 1.000000000000000000, 0.8660254037844387076, 1.000000000000000000, 0.8660254037844387076, 1.000000000000000000, 0.8660254037844387076, 1.000000000000000000, 0.8660254037844387076, 1.000000000000000000, 0.8660254037844387076, 1.000000000000000000, 0.8660254037844387076, 1.000000000000000000, 0.8660254037844387076, 1.000000000000000000, 0.8660254037844387076, 1.000000000000000000, 0.8660254037844387076, 1.000000000000000000, 0.8660254037844387076, 1.000000000000000000, 0.8660254037844387076, 1.000000000000000000, 0.8660254037844387076, 1.000000000000000000, 0.8660254037844387076, 1.000000000000000000, 0.8660254037844387076, 1.000000000000000000, 0.8660254037844387076, 1.000000000000000000, 0.8660254037844387076, 1.000000000000000000, 0.8660254037844387076, 1.000000000000000000, 0.8660254037844387076, 1.000000000000000000, 0.8660254037844387076, 1.000000000000000000, 0.8660254037844387076, 1.000000000000000000, 0.8660254037844387076, 1.000000000000000000, 0.8660254037844387076, 1.000000000000000000, 0.8660254037844387076, 1.000000000000000000, 0.8660254037844387076, 1.000000000000000000, 0.8660254037844387076, 1.000000000000000000, 0.9024577157650908177, 0.9469497795711379062, 0.9469497795711379062, 0.9469497795711379062 ) ) 
 REPRESENTATION_ITEM ( '' )  );
#63082 = CARTESIAN_POINT ( 'NONE',  ( -3.000000000000000000, 23.50000000000000000, -1.500000000000001332 ) ) ;
#63083 = DIRECTION ( 'NONE',  ( 1.000000000000000000, 0.000000000000000000, 0.000000000000000000 ) ) ;
#63084 = DIRECTION ( 'NONE',  ( 0.000000000000000000, 0.000000000000000000, 1.000000000000000000 ) ) ;
#63085 = CARTESIAN_POINT ( 'NONE',  ( 97.64999999999997726, -211.5299782133524502, 88.99458333333333826 ) ) ;
#63086 = ORIENTED_EDGE ( 'NONE', *, *, #61731, .F. ) ;
#63087 = ADVANCED_FACE ( 'NONE', ( #8791 ), #20444, .F. ) ;
#63088 = ORIENTED_EDGE ( 'NONE', *, *, #8745, .F. ) ;
#63089 = VERTEX_POINT ( 'NONE', #47901 ) ;
#63090 = ORIENTED_EDGE ( 'NONE', *, *, #37887, .T. ) ;
#63091 = CARTESIAN_POINT ( 'NONE',  ( 0.000000000000000000, -33.79645857604501913, -16.45098606841161626 ) ) ;
#63092 = CIRCLE ( 'NONE', #6661, 37.49900000000000944 ) ;
#63093 = FILL_AREA_STYLE ('',( #57067 ) ) ;
#63094 = CARTESIAN_POINT ( 'NONE',  ( -10.00000000000000000, 0.000000000000000000, 0.000000000000000000 ) ) ;
#63095 = CARTESIAN_POINT ( 'NONE',  ( 10.00000000000000000, 29.81001611431009479, 22.74946021919143391 ) ) ;
#63096 = CARTESIAN_POINT ( 'NONE',  ( 97.64999999999997726, -211.5299782133524502, 76.37395833506761278 ) ) ;
#63097 = CARTESIAN_POINT ( 'NONE',  ( 93.67499999999998295, 92.29496732002878900, 79.09916666666666174 ) ) ;
#63098 = EDGE_LOOP ( 'NONE', ( #37014, #19074, #68045, #65823 ) ) ;
#63099 = DIRECTION ( 'NONE',  ( 0.000000000000000000, -0.6494480483301903195, 0.7604059656000252687 ) ) ;
#63100 = ORIENTED_EDGE ( 'NONE', *, *, #55159, .F. ) ;
#63101 = DIRECTION ( 'NONE',  ( 0.000000000000000000, 0.000000000000000000, 1.000000000000000000 ) ) ;
#63102 = EDGE_CURVE ( 'NONE', #71746, #27263, #42637, .T. ) ;
#63103 = VERTEX_POINT ( 'NONE', #7318 ) ;
#63104 = FACE_OUTER_BOUND ( 'NONE', #22382, .T. ) ;
#63105 = CARTESIAN_POINT ( 'NONE',  ( -97.30629616937501680, 91.33154071421968467, 81.49364583420049257 ) ) ;
#63106 = CARTESIAN_POINT ( 'NONE',  ( 92.69370383062498320, 91.33154071421968467, 78.15989583420048348 ) ) ;
#63107 = EDGE_CURVE ( 'NONE', #52404, #12733, #27477, .T. ) ;
#63108 = VECTOR ( 'NONE', #27086, 1000.000000000000000 ) ;
#63109 = ORIENTED_EDGE ( 'NONE', *, *, #58720, .F. ) ;
#63110 = CARTESIAN_POINT ( 'NONE',  ( 11.99999999999999822, 65.58780272294076497, 36.73666225445916211 ) ) ;
#63111 = CARTESIAN_POINT ( 'NONE',  ( 0.000000000000000000, 0.000000000000000000, 0.000000000000000000 ) ) ;
#63112 = CARTESIAN_POINT ( 'NONE',  ( -96.32499999999996021, -207.7050326799711968, 77.82916666666665151 ) ) ;
#63113 = ORIENTED_EDGE ( 'NONE', *, *, #70659, .T. ) ;
#63114 = DIRECTION ( 'NONE',  ( -1.000000000000000000, 0.000000000000000000, 0.000000000000000000 ) ) ;
#63115 = EDGE_CURVE ( 'NONE', #44409, #41316, #15458, .T. ) ;
#63116 = AXIS2_PLACEMENT_3D ( 'NONE', #60460, #44656, #73197 ) ;
#63117 = CARTESIAN_POINT ( 'NONE',  ( -92.69370383062498320, -211.3315407142195852, 76.57239583420046358 ) ) ;
#63118 = ORIENTED_EDGE ( 'NONE', *, *, #60934, .F. ) ;
#63119 = ORIENTED_EDGE ( 'NONE', *, *, #29371, .F. ) ;
#63121 = FACE_BOUND ( 'NONE', #70476, .T. ) ;
#63120 = VECTOR ( 'NONE', #29522, 1000.000000000000000 ) ;
#63122 = VERTEX_POINT ( 'NONE', #65576 ) ;
#63123 = EDGE_CURVE ( 'NONE', #16557, #70771, #7679, .T. ) ;
#63124 = DIRECTION ( 'NONE',  ( 0.7950889364178796992, -0.6064928550163510845, 0.000000000000000000 ) ) ;
#63125 = CARTESIAN_POINT ( 'NONE',  ( 10.00000000000000000, 0.000000000000000000, 0.000000000000000000 ) ) ;
#63126 = ORIENTED_EDGE ( 'NONE', *, *, #813, .T. ) ;
#63127 = CARTESIAN_POINT ( 'NONE',  ( -94.99999999999997158, -212.6630814284392557, 77.10156250086711793 ) ) ;
#63128 = VERTEX_POINT ( 'NONE', #20058 ) ;
#63129 = LINE ( 'NONE', #57466, #13424 ) ;
#63130 = LINE ( 'NONE', #40920, #9231 ) ;
#63131 = CARTESIAN_POINT ( 'NONE',  ( 97.64999999999999147, -209.9999999999999716, 81.42749999999999488 ) ) ;
#63132 = VERTEX_POINT ( 'NONE', #19321 ) ;
#63133 = CIRCLE ( 'NONE', #30663, 77.49899999999999523 ) ;
#63134 = EDGE_CURVE ( 'NONE', #9528, #28379, #22664, .T. ) ;
#63135 = CARTESIAN_POINT ( 'NONE',  ( -95.00000000000002842, 93.05995642670504253, 83.57062500173429953 ) ) ;
#63136 = PRESENTATION_STYLE_ASSIGNMENT (( #74008 ) ) ;
#63137 = CARTESIAN_POINT ( 'NONE',  ( 93.84685191531248449, 88.00268892867053694, 85.30364583420046642 ) ) ;
#63138 = CARTESIAN_POINT ( 'NONE',  ( 11.99999999999999822, 0.000000000000000000, 0.000000000000000000 ) ) ;
#63139 = CARTESIAN_POINT ( 'NONE',  ( -4.999999999999999112, 2.691270400161067666, -1.881368198414903548 ) ) ;
#63140 = CARTESIAN_POINT ( 'NONE',  ( 11.99999999999999822, -68.67312586195022561, 35.91791733033451806 ) ) ;
#63141 = CARTESIAN_POINT ( 'NONE',  ( 2.981146944884248473, 4.052336700773506273, -0.5666985376598466795 ) ) ;
#63142 = FACE_OUTER_BOUND ( 'NONE', #72722, .T. ) ;
#63143 = DIRECTION ( 'NONE',  ( -1.000000000000000000, 0.000000000000000000, 0.000000000000000000 ) ) ;
#63144 = CYLINDRICAL_SURFACE ( 'NONE', #60167, 12.49999999999999822 ) ;
#63145 = CARTESIAN_POINT ( 'NONE',  ( -93.84685191531252713, 88.00268892867056536, 88.58447916753381435 ) ) ;
#63146 = DIRECTION ( 'NONE',  ( -0.000000000000000000, -0.000000000000000000, 1.000000000000000000 ) ) ;
#63147 = CARTESIAN_POINT ( 'NONE',  ( 92.34999999999993747, 88.47002178664756400, 85.60791666666665378 ) ) ;
#63148 = CARTESIAN_POINT ( 'NONE',  ( 15.00000000000000000, -19.89357724624986545, 12.59942793731086219 ) ) ;
#63149 = CARTESIAN_POINT ( 'NONE',  ( 10.00000000000000000, 0.000000000000000000, 0.000000000000000000 ) ) ;
#63150 = DIRECTION ( 'NONE',  ( -1.000000000000000000, 0.000000000000000000, 0.000000000000000000 ) ) ;
#63151 = DIRECTION ( 'NONE',  ( 1.000000000000000000, 0.000000000000000000, 0.000000000000000000 ) ) ;
#63152 = EDGE_CURVE ( 'NONE', #56518, #74246, #30967, .T. ) ;
#63153 = CARTESIAN_POINT ( 'NONE',  ( 10.00000000000000000, 29.81001611431009479, 22.74946021919143391 ) ) ;
#63154 = CIRCLE ( 'NONE', #22295, 77.49900000000000944 ) ;
#63155 = CARTESIAN_POINT ( 'NONE',  ( 95.00000000000000000, -207.3369185715606307, 83.92781250086716227 ) ) ;
#63156 = ADVANCED_FACE ( 'NONE', ( #36615 ), #59561, .F. ) ;
#63157 = CIRCLE ( 'NONE', #37914, 21.00000000000000000 ) ;
#63158 = VERTEX_POINT ( 'NONE', #54292 ) ;
#63159 = AXIS2_PLACEMENT_3D ( 'NONE', #41116, #11061, #64052 ) ;
#63160 = ADVANCED_FACE ( 'NONE', ( #2817 ), #9529, .T. ) ;
#63161 = ORIENTED_EDGE ( 'NONE', *, *, #46415, .F. ) ;
#63162 = DIRECTION ( 'NONE',  ( 0.000000000000000000, 0.000000000000000000, 1.000000000000000000 ) ) ;
#63163 = ORIENTED_EDGE ( 'NONE', *, *, #11347, .T. ) ;
#63164 = VECTOR ( 'NONE', #3211, 1000.000000000000000 ) ;
#63165 = FACE_OUTER_BOUND ( 'NONE', #66573, .T. ) ;
#63166 = VECTOR ( 'NONE', #41459, 1000.000000000000000 ) ;
#63167 = CARTESIAN_POINT ( 'NONE',  ( 93.84685191531251292, -211.9973110713294489, 77.04864583420047097 ) ) ;
#63168 = ORIENTED_EDGE ( 'NONE', *, *, #44815, .T. ) ;
#63169 = CARTESIAN_POINT ( 'NONE',  ( 97.30629616937498838, -209.9999999999999716, 84.40406250086715545 ) ) ;
#63170 = ORIENTED_EDGE ( 'NONE', *, *, #22990, .F. ) ;
#63171 = CARTESIAN_POINT ( 'NONE',  ( 0.000000000000000000, 0.000000000000000000, 0.000000000000000000 ) ) ;
#63172 = ORIENTED_EDGE ( 'NONE', *, *, #4457, .F. ) ;
#63173 = ORIENTED_EDGE ( 'NONE', *, *, #43801, .F. ) ;
#63174 = CARTESIAN_POINT ( 'NONE',  ( -10.00000000000000000, 0.000000000000000000, 0.000000000000000000 ) ) ;
#63175 = VECTOR ( 'NONE', #33825, 1000.000000000000000 ) ;
#63176 = DIRECTION ( 'NONE',  ( -1.000000000000000000, 0.000000000000000000, 0.000000000000000000 ) ) ;
#63177 = ORIENTED_EDGE ( 'NONE', *, *, #25557, .T. ) ;
#63178 = CARTESIAN_POINT ( 'NONE',  ( 0.000000000000000000, 0.000000000000000000, 37.49900000000000233 ) ) ;
#63179 = CARTESIAN_POINT ( 'NONE',  ( 95.00000000000000000, -206.9400435732949575, 88.01562500173429271 ) ) ;
#63180 = EDGE_CURVE ( 'NONE', #14764, #45615, #20221, .T. ) ;
#63181 = ORIENTED_EDGE ( 'NONE', *, *, #68532, .F. ) ;
#63182 = DIRECTION ( 'NONE',  ( 0.000000000000000000, 0.000000000000000000, -1.000000000000000000 ) ) ;
#63183 = ORIENTED_EDGE ( 'NONE', *, *, #1906, .F. ) ;
#63184 = LINE ( 'NONE', #23319, #70869 ) ;
#63185 = VERTEX_POINT ( 'NONE', #73411 ) ;
#63186 = ORIENTED_EDGE ( 'NONE', *, *, #38465, .F. ) ;
#63187 = EDGE_LOOP ( 'NONE', ( #8412, #17604, #33301, #38922 ) ) ;
#63188 = CARTESIAN_POINT ( 'NONE',  ( 10.00000000000000000, 71.27951684758069462, -30.41916302227035729 ) ) ;
#63189 = ADVANCED_FACE ( 'NONE', ( #9154 ), #16511, .F. ) ;
#63190 = EDGE_CURVE ( 'NONE', #38975, #6686, #63514, .T. ) ;
#63191 = DIRECTION ( 'NONE',  ( -1.000000000000000000, -0.000000000000000000, -0.000000000000000000 ) ) ;
#63192 = EDGE_LOOP ( 'NONE', ( #19791, #31500, #50099, #66504 ) ) ;
#63193 = ORIENTED_EDGE ( 'NONE', *, *, #22240, .F. ) ;
#63194 = EDGE_LOOP ( 'NONE', ( #27153, #11959, #59843, #15064 ) ) ;
#63195 = DIRECTION ( 'NONE',  ( -1.000000000000000000, -0.000000000000000000, -0.000000000000000000 ) ) ;
#63196 = CYLINDRICAL_SURFACE ( 'NONE', #50533, 77.49899999999999523 ) ;
#63197 = CARTESIAN_POINT ( 'NONE',  ( -92.35000000000003695, 90.00000000000004263, 86.50750000000000739 ) ) ;
#63198 = ORIENTED_EDGE ( 'NONE', *, *, #62343, .T. ) ;
#63199 = EDGE_CURVE ( 'NONE', #3531, #61698, #33428, .T. ) ;
#63200 = DIRECTION ( 'NONE',  ( 0.000000000000000000, 0.000000000000000000, -1.000000000000000000 ) ) ;
#63201 = ORIENTED_EDGE ( 'NONE', *, *, #52008, .F. ) ;
#63202 = DIRECTION ( 'NONE',  ( 1.000000000000000000, 0.000000000000000000, 0.000000000000000000 ) ) ;
#63203 = CARTESIAN_POINT ( 'NONE',  ( -97.30629616937497417, -211.3315407142195852, 87.79072916753381151 ) ) ;
#63204 = VERTEX_POINT ( 'NONE', #61053 ) ;
#63205 = DIRECTION ( 'NONE',  ( 0.000000000000000000, 0.000000000000000000, 1.000000000000000000 ) ) ;
#63206 = AXIS2_PLACEMENT_3D ( 'NONE', #67806, #61434, #27947 ) ;
#63207 = CARTESIAN_POINT ( 'NONE',  ( 10.00000000000000000, 0.000000000000000000, 0.000000000000000000 ) ) ;
#63208 = CARTESIAN_POINT ( 'NONE',  ( 0.000000000000000000, 0.000000000000000000, -6.000000000000000000 ) ) ;
#63209 = CARTESIAN_POINT ( 'NONE',  ( -93.84685191531248449, -208.0026889286704943, 76.73114583420047552 ) ) ;
#63210 = DIRECTION ( 'NONE',  ( -1.000000000000000000, 1.047380211910311281E-14, 2.618450529775778123E-14 ) ) ;
#63211 = CARTESIAN_POINT ( 'NONE',  ( 0.000000000000000000, 0.000000000000000000, 125.0000000000000000 ) ) ;
#63212 = CIRCLE ( 'NONE', #48792, 3.299999999999983391 ) ;
#63213 = DIRECTION ( 'NONE',  ( -1.000000000000000000, 0.000000000000000000, 0.000000000000000000 ) ) ;
#63214 = CIRCLE ( 'NONE', #46397, 32.00000000000000000 ) ;
#63215 = CARTESIAN_POINT ( 'NONE',  ( 10.00000000000000000, -77.49459641780886443, -0.8261519478439277586 ) ) ;
#63216 = CARTESIAN_POINT ( 'NONE',  ( 96.32499999999998863, 87.70503267997126784, 80.13104166840095388 ) ) ;
#63217 = CARTESIAN_POINT ( 'NONE',  ( -97.30629616937501680, 90.00000000000004263, 77.57781250086713953 ) ) ;
#63218 = PLANE ( 'NONE',  #8218 ) ;
#63219 = CARTESIAN_POINT ( 'NONE',  ( 12.75000000000000000, -120.0000000000000000, 127.5000000000000000 ) ) ;
#63220 = CIRCLE ( 'NONE', #7971, 1.500000000000000000 ) ;
#63221 = AXIS2_PLACEMENT_3D ( 'NONE', #74094, #16966, #69574 ) ;
#63222 = EDGE_LOOP ( 'NONE', ( #33395, #9278, #31328, #48171 ) ) ;
#63223 = DIRECTION ( 'NONE',  ( 1.000000000000000000, 0.000000000000000000, 0.000000000000000000 ) ) ;
#63224 = CYLINDRICAL_SURFACE ( 'NONE', #46089, 42.00000000000000000 ) ;
#63225 = DIRECTION ( 'NONE',  ( -1.000000000000000000, 0.000000000000000000, 0.000000000000000000 ) ) ;
#63226 = LINE ( 'NONE', #28990, #38226 ) ;
#63227 = DIRECTION ( 'NONE',  ( 1.000000000000000000, -7.571539615859142926E-15, -2.618450529775767079E-14 ) ) ;
#63228 = CIRCLE ( 'NONE', #17597, 26.50000000000552092 ) ;
#63229 = CARTESIAN_POINT ( 'NONE',  ( -97.64999999950704535, 89.99996796756893502, 85.63541623677065218 ) ) ;
#63230 = CARTESIAN_POINT ( 'NONE',  ( -97.64999999999996305, -209.9999999999999716, 90.00000000000000000 ) ) ;
#63231 = DIRECTION ( 'NONE',  ( -1.000000000000000000, 0.000000000000000000, -0.000000000000000000 ) ) ;
#63232 = VERTEX_POINT ( 'NONE', #50504 ) ;
#63233 = DIRECTION ( 'NONE',  ( 0.000000000000000000, 0.000000000000000000, 1.000000000000000000 ) ) ;
#63234 = CARTESIAN_POINT ( 'NONE',  ( -93.67500000000003979, 87.70503267997129626, 80.76604166840097321 ) ) ;
#63235 = FACE_OUTER_BOUND ( 'NONE', #17040, .T. ) ;
#63236 = DIRECTION ( 'NONE',  ( 0.000000000000000000, -0.7604059656000369261, 0.6494480483301767748 ) ) ;
#63237 = EDGE_CURVE ( 'NONE', #47001, #49804, #10654, .T. ) ;
#63238 = ADVANCED_FACE ( 'NONE', ( #49398 ), #62168, .T. ) ;
#63239 = CYLINDRICAL_SURFACE ( 'NONE', #64379, 31.99999999999998579 ) ;
#63240 = EDGE_LOOP ( 'NONE', ( #35971, #20271, #62839, #14774 ) ) ;
#63241 = EDGE_CURVE ( 'NONE', #48030, #70758, #56537, .T. ) ;
#63242 = DIRECTION ( 'NONE',  ( 0.000000000000000000, -0.9510565162951565288, 0.3090169943749382364 ) ) ;
#63243 = LINE ( 'NONE', #17728, #36689 ) ;
#63244 = ORIENTED_EDGE ( 'NONE', *, *, #47311, .F. ) ;
#63245 = EDGE_CURVE ( 'NONE', #15433, #10724, #57353, .T. ) ;
#63246 = CARTESIAN_POINT ( 'NONE',  ( 95.00000000000000000, -212.6630814284392557, 89.16656250086712987 ) ) ;
#63247 = DIRECTION ( 'NONE',  ( -0.000000000000000000, 0.4999999999999919509, 0.8660254037844432595 ) ) ;
#63248 = ORIENTED_EDGE ( 'NONE', *, *, #48123, .F. ) ;
#63249 = CARTESIAN_POINT ( 'NONE',  ( -97.64999999980591383, 89.99998015682162134, 84.36502760998403971 ) ) ;
#63250 = VECTOR ( 'NONE', #52704, 1000.000000000000000 ) ;
#63251 = ORIENTED_EDGE ( 'NONE', *, *, #48957, .F. ) ;
#63252 = EDGE_CURVE ( 'NONE', #4121, #9267, #27576, .T. ) ;
#63253 = FACE_OUTER_BOUND ( 'NONE', #49576, .T. ) ;
#63254 = ORIENTED_EDGE ( 'NONE', *, *, #36681, .F. ) ;
#63255 = CYLINDRICAL_SURFACE ( 'NONE', #21625, 77.49899999999999523 ) ;
#63256 = ORIENTED_EDGE ( 'NONE', *, *, #47515, .F. ) ;
#63257 = CARTESIAN_POINT ( 'NONE',  ( 10.00000000000000000, -36.72794159290197769, -65.59268652807249111 ) ) ;
#63258 = ORIENTED_EDGE ( 'NONE', *, *, #55358, .F. ) ;
#63259 = AXIS2_PLACEMENT_3D ( 'NONE', #39732, #27695, #11152 ) ;
#63260 = ORIENTED_EDGE ( 'NONE', *, *, #7663, .T. ) ;
#63261 = DIRECTION ( 'NONE',  ( -1.000000000000000000, 0.000000000000000000, 0.000000000000000000 ) ) ;
#63262 = EDGE_CURVE ( 'NONE', #55165, #15320, #21557, .T. ) ;
#63263 = EDGE_CURVE ( 'NONE', #27990, #16188, #68173, .T. ) ;
#63264 = ORIENTED_EDGE ( 'NONE', *, *, #21387, .T. ) ;
#63265 = ORIENTED_EDGE ( 'NONE', *, *, #45267, .T. ) ;
#63266 = DIRECTION ( 'NONE',  ( 1.000000000000000000, 0.000000000000000000, 0.000000000000000000 ) ) ;
#63267 = AXIS2_PLACEMENT_3D ( 'NONE', #46214, #45106, #40201 ) ;
#63268 = ORIENTED_EDGE ( 'NONE', *, *, #330, .F. ) ;
#63269 = ORIENTED_EDGE ( 'NONE', *, *, #65470, .T. ) ;
#63270 = CARTESIAN_POINT ( 'NONE',  ( 96.15314808468748708, 88.00268892867053694, 84.77447916753381207 ) ) ;
#63271 = ORIENTED_EDGE ( 'NONE', *, *, #12214, .T. ) ;
#63272 = CARTESIAN_POINT ( 'NONE',  ( 92.69370383062501162, -211.3315407142195852, 83.34572916753380412 ) ) ;
#63273 = ADVANCED_FACE ( 'NONE', ( #5040, #27945 ), #26828, .F. ) ;
#63274 = EDGE_CURVE ( 'NONE', #39300, #53012, #10285, .T. ) ;
#63275 = SHAPE_DEFINITION_REPRESENTATION ( #38597, #31559 ) ;
#63276 = DIRECTION ( 'NONE',  ( 1.000000000000000000, 0.000000000000000000, 0.000000000000000000 ) ) ;
#63277 = DIRECTION ( 'NONE',  ( 1.000000000000000000, 0.000000000000000000, -0.000000000000000000 ) ) ;
#63278 = DIRECTION ( 'NONE',  ( -1.000000000000000000, -0.000000000000000000, -0.000000000000000000 ) ) ;
#63279 = CARTESIAN_POINT ( 'NONE',  ( 0.000000000000000000, 62.50884508063427347, 41.76106447765511831 ) ) ;
#63280 = CARTESIAN_POINT ( 'NONE',  ( 0.000000000000000000, -19.89357724625003598, 12.59942793731059574 ) ) ;
#63281 = CARTESIAN_POINT ( 'NONE',  ( 10.00000000000000000, 74.65491531819118620, -8.830959090342659579 ) ) ;
#63282 = CARTESIAN_POINT ( 'NONE',  ( -92.69370383062498320, -209.9999999999999716, 84.24531250086714351 ) ) ;
#63283 = VECTOR ( 'NONE', #26067, 1000.000000000000000 ) ;
#63284 = CARTESIAN_POINT ( 'NONE',  ( -93.84685191531252713, 88.00268892867056536, 81.75822916753382685 ) ) ;
#63285 = VERTEX_POINT ( 'NONE', #72324 ) ;
#63287 = CARTESIAN_POINT ( 'NONE',  ( -93.84685191531254134, 91.99731107132950569, 86.25614583420048120 ) ) ;
#63286 = CARTESIAN_POINT ( 'NONE',  ( 96.15314808468748708, 91.99731107132950569, 85.62114583420046188 ) ) ;
#63288 = ORIENTED_EDGE ( 'NONE', *, *, #65022, .F. ) ;
#63289 = FACE_OUTER_BOUND ( 'NONE', #33096, .T. ) ;
#63290 = CARTESIAN_POINT ( 'NONE',  ( -25.00516449930816876, -111.2255058058861010, 2.500000000000000000 ) ) ;
#63291 = CARTESIAN_POINT ( 'NONE',  ( 26.50000000000770939, -120.0000000000001847, -49.00000000000066080 ) ) ;
#63292 = DIRECTION ( 'NONE',  ( -1.000000000000000000, -0.000000000000000000, -0.000000000000000000 ) ) ;
#63293 = CARTESIAN_POINT ( 'NONE',  ( -94.99999999999997158, -212.6630814284392557, 85.99156250086714692 ) ) ;
#63294 = LINE ( 'NONE', #46734, #37883 ) ;
#63295 = CARTESIAN_POINT ( 'NONE',  ( -97.64999999954994792, 89.99996890530464100, 88.81037122970319331 ) ) ;
#63296 = DIRECTION ( 'NONE',  ( 0.000000000000000000, 0.000000000000000000, 1.000000000000000000 ) ) ;
#63297 = DIRECTION ( 'NONE',  ( -1.000000000000000000, -0.000000000000000000, 0.000000000000000000 ) ) ;
#63298 = ORIENTED_EDGE ( 'NONE', *, *, #46870, .T. ) ;
#63299 = ORIENTED_EDGE ( 'NONE', *, *, #6983, .T. ) ;
#63300 = CARTESIAN_POINT ( 'NONE',  ( -93.67500000000003979, 92.29496732002878900, 78.99333333333332519 ) ) ;
#63301 = CARTESIAN_POINT ( 'NONE',  ( 9.984461079971730157, -95.40710393340120277, 5.500000000000000000 ) ) ;
#63302 = CARTESIAN_POINT ( 'NONE',  ( -94.70223316838999494, -207.6384304500494977, 74.83035915144985495 ) ) ;
#63303 = DIRECTION ( 'NONE',  ( 0.000000000000000000, 0.000000000000000000, 1.000000000000000000 ) ) ;
#63304 = CYLINDRICAL_SURFACE ( 'NONE', #44745, 82.00000000000000000 ) ;
#63305 = FACE_OUTER_BOUND ( 'NONE', #612, .T. ) ;
#63306 = FACE_OUTER_BOUND ( 'NONE', #25510, .T. ) ;
#63307 =( BOUNDED_CURVE ( )  B_SPLINE_CURVE ( 2, ( #4826, #72825, #67955, #55928, #22846, #27728, #50652, #38646, #28093 ),
 .UNSPECIFIED., .F., .F. ) 
 B_SPLINE_CURVE_WITH_KNOTS ( ( 3, 2, 2, 2, 3 ),
 ( 0.2540073681295598185, 0.2540075594730126229, 0.2610633250139296480, 0.2681190905548467285, 0.2751748541917909407 ),
 .UNSPECIFIED. ) 
 CURVE ( )  GEOMETRIC_REPRESENTATION_ITEM ( )  RATIONAL_B_SPLINE_CURVE ( ( 0.9999927337532719118, 0.9999963667781075483, 1.000000000000000000, 0.8660254037844387076, 1.000000000000000000, 0.8660254037844387076, 1.000000000000000000, 0.8660254037844387076, 1.000000000000000000 ) ) 
 REPRESENTATION_ITEM ( '' )  );
#63308 = VECTOR ( 'NONE', #56361, 1000.000000000000000 ) ;
#63309 = ORIENTED_EDGE ( 'NONE', *, *, #36815, .F. ) ;
#63310 = CARTESIAN_POINT ( 'NONE',  ( -93.84685191531254134, 91.99731107132950569, 77.36614583420046642 ) ) ;
#63311 = AXIS2_PLACEMENT_3D ( 'NONE', #1174, #11291, #46617 ) ;
#63312 = CARTESIAN_POINT ( 'NONE',  ( 0.000000000000000000, 0.000000000000000000, 125.0000000000000000 ) ) ;
#63313 = CARTESIAN_POINT ( 'NONE',  ( 5.000000000000002665, -81.50828551894234408, 8.966570791700407383 ) ) ;
#63314 = FACE_OUTER_BOUND ( 'NONE', #3526, .T. ) ;
#63315 = DIRECTION ( 'NONE',  ( 1.000000000000000000, 0.000000000000000000, 0.000000000000000000 ) ) ;
#63316 = DIRECTION ( 'NONE',  ( -1.000000000000000000, -0.000000000000000000, -0.000000000000000000 ) ) ;
#63317 = FACE_OUTER_BOUND ( 'NONE', #40882, .T. ) ;
#63318 = ADVANCED_FACE ( 'NONE', ( #73798 ), #22313, .T. ) ;
#63319 = CIRCLE ( 'NONE', #66931, 37.49900000000000233 ) ;
#63320 = FILL_AREA_STYLE ('',( #12898 ) ) ;
#63321 = ADVANCED_FACE ( 'NONE', ( #73432 ), #33206, .F. ) ;
#63322 = ADVANCED_FACE ( 'NONE', ( #33958 ), #3564, .F. ) ;
#63323 = CARTESIAN_POINT ( 'NONE',  ( 97.30629616937498838, 88.66845928578035796, 78.63614583420046245 ) ) ;
#63324 = EDGE_CURVE ( 'NONE', #60073, #59929, #45486, .T. ) ;
#63325 = CARTESIAN_POINT ( 'NONE',  ( -96.15314808468745866, -211.9973110713294489, 81.01739583420049939 ) ) ;
#63326 = FACE_OUTER_BOUND ( 'NONE', #51345, .T. ) ;
#63327 = ORIENTED_EDGE ( 'NONE', *, *, #36405, .T. ) ;
#63328 = CARTESIAN_POINT ( 'NONE',  ( -92.35000000000003695, 90.00000000000004263, 82.77687500173431090 ) ) ;
#63329 = CARTESIAN_POINT ( 'NONE',  ( 97.64999999954044085, -209.9999506483753180, 87.22187670868780174 ) ) ;
#63330 = CARTESIAN_POINT ( 'NONE',  ( 96.32499999999998863, -212.2949673200287179, 78.86104166840097207 ) ) ;
#63331 = VECTOR ( 'NONE', #46144, 1000.000000000000000 ) ;
#63332 = EDGE_CURVE ( 'NONE', #64894, #36430, #51531, .T. ) ;
#63333 = CARTESIAN_POINT ( 'NONE',  ( -97.30629616937501680, 91.33154071421968467, 75.14364583420049826 ) ) ;
#63334 = CARTESIAN_POINT ( 'NONE',  ( 95.00000000000000000, -207.3369185715606307, 75.51406250086714067 ) ) ;
#63335 = ORIENTED_EDGE ( 'NONE', *, *, #46582, .F. ) ;
#63336 = FACE_OUTER_BOUND ( 'NONE', #58550, .T. ) ;
#63337 = ORIENTED_EDGE ( 'NONE', *, *, #31223, .F. ) ;
#63338 = EDGE_CURVE ( 'NONE', #16918, #39783, #27528, .T. ) ;
#63339 = DIRECTION ( 'NONE',  ( -0.000000000000000000, -0.000000000000000000, 1.000000000000000000 ) ) ;
#63340 = ORIENTED_EDGE ( 'NONE', *, *, #33689, .F. ) ;
#63341 = CYLINDRICAL_SURFACE ( 'NONE', #4622, 13.90444123027096879 ) ;
#63342 = VERTEX_POINT ( 'NONE', #56907 ) ;
#63343 = VERTEX_POINT ( 'NONE', #45639 ) ;
#63344 = ORIENTED_EDGE ( 'NONE', *, *, #4864, .F. ) ;
#63345 = CARTESIAN_POINT ( 'NONE',  ( -96.32499999999996021, -212.2949673200287179, 77.40583333333331950 ) ) ;
#63346 = EDGE_CURVE ( 'NONE', #33464, #66997, #34328, .T. ) ;
#63347 = EDGE_CURVE ( 'NONE', #14951, #60573, #17408, .T. ) ;
#63348 = EDGE_LOOP ( 'NONE', ( #15495, #72755, #23848, #54533 ) ) ;
#63349 = ORIENTED_EDGE ( 'NONE', *, *, #47963, .T. ) ;
#63350 = CARTESIAN_POINT ( 'NONE',  ( 96.15314808468748708, 91.99731107132950569, 83.23989583420049598 ) ) ;
#63351 = CIRCLE ( 'NONE', #44130, 82.00000000000000000 ) ;
#63352 = CARTESIAN_POINT ( 'NONE',  ( 93.67500000000001137, -207.7050326799711968, 75.28916666666665947 ) ) ;
#63353 = AXIS2_PLACEMENT_3D ( 'NONE', #44998, #33312, #33702 ) ;
#63354 = ORIENTED_EDGE ( 'NONE', *, *, #31000, .F. ) ;
#63355 = ORIENTED_EDGE ( 'NONE', *, *, #31212, .T. ) ;
#63356 = ORIENTED_EDGE ( 'NONE', *, *, #59597, .T. ) ;
#63357 = ORIENTED_EDGE ( 'NONE', *, *, #65863, .T. ) ;
#63358 = DIRECTION ( 'NONE',  ( -1.000000000000000000, 0.000000000000000000, 0.000000000000000000 ) ) ;
#63359 = DIRECTION ( 'NONE',  ( 1.000000000000000000, 0.000000000000000000, 0.000000000000000000 ) ) ;
#63360 = CARTESIAN_POINT ( 'NONE',  ( 10.00000000000000000, 0.000000000000000000, 0.000000000000000000 ) ) ;
#63361 = LINE ( 'NONE', #11826, #39947 ) ;
#63362 = LINE ( 'NONE', #34780, #51861 ) ;
#63363 = CIRCLE ( 'NONE', #21309, 31.99999999999999289 ) ;
#63364 = DIRECTION ( 'NONE',  ( 0.000000000000000000, 0.000000000000000000, 1.000000000000000000 ) ) ;
#63365 = FACE_OUTER_BOUND ( 'NONE', #29565, .T. ) ;
#63366 = CARTESIAN_POINT ( 'NONE',  ( 0.000000000000000000, -79.10210256391353312, -21.60688246758670061 ) ) ;
#63367 = ORIENTED_EDGE ( 'NONE', *, *, #14072, .T. ) ;
#63368 = CARTESIAN_POINT ( 'NONE',  ( -93.67499999999998295, -212.2949673200287179, 80.13104166840095388 ) ) ;
#63369 = VERTEX_POINT ( 'NONE', #35437 ) ;
#63370 = FACE_OUTER_BOUND ( 'NONE', #1261, .T. ) ;
#63371 = ORIENTED_EDGE ( 'NONE', *, *, #58805, .F. ) ;
#63373 = CARTESIAN_POINT ( 'NONE',  ( -97.65000000000001990, 90.00000000000004263, 79.91937500173429498 ) ) ;
#63372 = CARTESIAN_POINT ( 'NONE',  ( 97.64999999999999147, 90.00000000000002842, 78.96687500173429441 ) ) ;
#63374 = EDGE_LOOP ( 'NONE', ( #31243, #42761, #38550, #16780 ) ) ;
#63375 = CARTESIAN_POINT ( 'NONE',  ( 92.69370383062498320, 88.66845928578037217, 78.42447916753380355 ) ) ;
#63376 = FACE_OUTER_BOUND ( 'NONE', #10761, .T. ) ;
#63377 = DIRECTION ( 'NONE',  ( 0.000000000000000000, -0.8090169943749402348, -0.5877852522924830181 ) ) ;
#63378 = DIRECTION ( 'NONE',  ( 0.000000000000000000, 0.000000000000000000, 1.000000000000000000 ) ) ;
#63379 = FACE_OUTER_BOUND ( 'NONE', #14673, .T. ) ;
#63380 = ORIENTED_EDGE ( 'NONE', *, *, #66744, .T. ) ;
#63381 = DIRECTION ( 'NONE',  ( -0.000000000000000000, -0.000000000000000000, 1.000000000000000000 ) ) ;
#63382 = CARTESIAN_POINT ( 'NONE',  ( 8.000000000000007105, 1.142349898368116708E-14, 6.370018489481387452E-15 ) ) ;
#63383 = DIRECTION ( 'NONE',  ( -0.000000000000000000, -0.000000000000000000, 1.000000000000000000 ) ) ;
#63384 = EDGE_LOOP ( 'NONE', ( #47433, #26447, #30968, #21730 ) ) ;
#63385 = AXIS2_PLACEMENT_3D ( 'NONE', #71264, #14124, #37075 ) ;
#63386 = EDGE_LOOP ( 'NONE', ( #31984, #12671, #45279, #67779 ) ) ;
#63387 = CIRCLE ( 'NONE', #42985, 16.00000000000000000 ) ;
#63388 = CIRCLE ( 'NONE', #30938, 23.50000000000000355 ) ;
#63389 = AXIS2_PLACEMENT_3D ( 'NONE', #24196, #48229, #47849 ) ;
#63390 = EDGE_CURVE ( 'NONE', #68921, #60376, #69565, .T. ) ;
#63391 = DIRECTION ( 'NONE',  ( 4.476705744456278560E-17, -1.000000000000000000, 8.723836835350694626E-17 ) ) ;
#63392 = CARTESIAN_POINT ( 'NONE',  ( 11.99999999999999822, 17.28742895386189460, -75.54627589209927407 ) ) ;
#63393 = FACE_OUTER_BOUND ( 'NONE', #22187, .T. ) ;
#63394 = CARTESIAN_POINT ( 'NONE',  ( -93.84685191531247028, -211.9973110713294489, 76.67822916753381435 ) ) ;
#63395 = VECTOR ( 'NONE', #117, 1000.000000000000000 ) ;
#63396 = EDGE_LOOP ( 'NONE', ( #44705, #25039, #26764, #1242 ) ) ;
#63397 = CARTESIAN_POINT ( 'NONE',  ( 12.00000000000000000, -10.45096189432344502, -21.10159698893425784 ) ) ;
#63398 = PLANE ( 'NONE',  #43147 ) ;
#63399 = CARTESIAN_POINT ( 'NONE',  ( 0.000000000000000000, -37.58145647212455032, 0.6853352020789044152 ) ) ;
#63400 = CARTESIAN_POINT ( 'NONE',  ( 93.84685191531248449, 88.00268892867053694, 75.77864583420047495 ) ) ;
#63401 = CARTESIAN_POINT ( 'NONE',  ( 95.00000000000000000, -209.9999999999999716, 90.00000000000000000 ) ) ;
#63402 = DIRECTION ( 'NONE',  ( -1.000000000000000000, 0.000000000000000000, 0.000000000000000000 ) ) ;
#63403 = EDGE_CURVE ( 'NONE', #56237, #21161, #41980, .T. ) ;
#63404 = LINE ( 'NONE', #28431, #58951 ) ;
#63405 = CARTESIAN_POINT ( 'NONE',  ( 10.00000000000000000, 75.54627589209943039, 17.28742895386112721 ) ) ;
#63406 = DIRECTION ( 'NONE',  ( 0.000000000000000000, 0.6691306063588672304, -0.7431448254773862505 ) ) ;
#63407 = ADVANCED_FACE ( 'NONE', ( #64393 ), #46728, .T. ) ;
#63408 = DIRECTION ( 'NONE',  ( -1.000000000000000000, 0.000000000000000000, 0.000000000000000000 ) ) ;
#63409 = AXIS2_PLACEMENT_3D ( 'NONE', #73589, #61587, #34120 ) ;
#63410 = CARTESIAN_POINT ( 'NONE',  ( 92.69370383062498320, 90.00000000000002842, 85.99156250086716113 ) ) ;
#63411 = VECTOR ( 'NONE', #38519, 1000.000000000000000 ) ;
#63412 = CIRCLE ( 'NONE', #56207, 10.00000000000000178 ) ;
#63413 = EDGE_CURVE ( 'NONE', #11375, #66589, #40344, .T. ) ;
#63414 = FACE_OUTER_BOUND ( 'NONE', #49629, .T. ) ;
#63415 = CARTESIAN_POINT ( 'NONE',  ( 6.938893903907228378E-15, 0.000000000000000000, 0.000000000000000000 ) ) ;
#63416 = ORIENTED_EDGE ( 'NONE', *, *, #13414, .T. ) ;
#63417 = EDGE_CURVE ( 'NONE', #67162, #63432, #51622, .T. ) ;
#63418 = DIRECTION ( 'NONE',  ( -1.000000000000000000, -0.000000000000000000, -0.000000000000000000 ) ) ;
#63419 = CARTESIAN_POINT ( 'NONE',  ( -95.00000000000002842, 87.33691857156074434, 80.27656250086714351 ) ) ;
#63420 = CIRCLE ( 'NONE', #12998, 31.99999999999998934 ) ;
#63421 = CIRCLE ( 'NONE', #38172, 77.49899999999999523 ) ;
#63422 = DIRECTION ( 'NONE',  ( 0.000000000000000000, 0.7071067811865487940, -0.7071067811865462405 ) ) ;
#63423 = VERTEX_POINT ( 'NONE', #22691 ) ;
#63424 = DIRECTION ( 'NONE',  ( 1.000000000000000000, 0.000000000000000000, 0.000000000000000000 ) ) ;
#63425 = DIRECTION ( 'NONE',  ( -1.000000000000000000, 0.000000000000000000, 0.000000000000000000 ) ) ;
#63426 = ADVANCED_FACE ( 'NONE', ( #63289 ), #69653, .T. ) ;
#63427 = DIRECTION ( 'NONE',  ( 1.000000000000000000, -0.000000000000000000, 0.000000000000000000 ) ) ;
#63428 = CARTESIAN_POINT ( 'NONE',  ( 10.00000000000000000, 22.48208911017551515, -35.47612816024499693 ) ) ;
#63429 = CARTESIAN_POINT ( 'NONE',  ( 0.000000000000000000, 0.000000000000000000, 0.000000000000000000 ) ) ;
#63430 = AXIS2_PLACEMENT_3D ( 'NONE', #74058, #22955, #50758 ) ;
#63431 = AXIS2_PLACEMENT_3D ( 'NONE', #37103, #20164, #60414 ) ;
#63432 = VERTEX_POINT ( 'NONE', #64025 ) ;
#63433 = VERTEX_POINT ( 'NONE', #6149 ) ;
#63434 = AXIS2_PLACEMENT_3D ( 'NONE', #18563, #41502, #53160 ) ;
#63435 = AXIS2_PLACEMENT_3D ( 'NONE', #59419, #41386, #64691 ) ;
#63436 = CARTESIAN_POINT ( 'NONE',  ( 96.15314808468748708, -208.0026889286704943, 80.69989583420047552 ) ) ;
#63437 = EDGE_CURVE ( 'NONE', #59366, #29381, #62643, .T. ) ;
#63438 = DIRECTION ( 'NONE',  ( 0.000000000000000000, -0.8910065241883627918, -0.4539904997395568520 ) ) ;
#63439 = CARTESIAN_POINT ( 'NONE',  ( 4.999999999999999112, -3.925862922255855647, -41.81611651403866858 ) ) ;
#63440 = DIRECTION ( 'NONE',  ( -0.2079116908177431888, 0.000000000000000000, 0.9781476007338091305 ) ) ;
#63441 = CARTESIAN_POINT ( 'NONE',  ( 92.34999999999999432, 90.00000000000002842, 83.72937500173429726 ) ) ;
#63442 = EDGE_CURVE ( 'NONE', #43013, #64475, #531, .T. ) ;
#63443 = DIRECTION ( 'NONE',  ( 0.000000000000000000, 0.000000000000000000, 1.000000000000000000 ) ) ;
#63444 = CARTESIAN_POINT ( 'NONE',  ( 93.67500000000001137, -207.7050326799711968, 86.08416666666666117 ) ) ;
#63445 = ORIENTED_EDGE ( 'NONE', *, *, #60041, .F. ) ;
#63446 = VERTEX_POINT ( 'NONE', #37306 ) ;
#63447 = ORIENTED_EDGE ( 'NONE', *, *, #53392, .T. ) ;
#63448 = ORIENTED_EDGE ( 'NONE', *, *, #63263, .T. ) ;
#63449 = CARTESIAN_POINT ( 'NONE',  ( -92.69370383062502583, 91.33154071421968467, 88.90197916753382401 ) ) ;
#63450 = DIRECTION ( 'NONE',  ( 0.000000000000000000, 0.000000000000000000, 1.000000000000000000 ) ) ;
#63451 = CARTESIAN_POINT ( 'NONE',  ( -96.32500000000001705, 87.70503267997129626, 83.75583333333332803 ) ) ;
#63452 = CARTESIAN_POINT ( 'NONE',  ( 92.35000000000002274, -211.5299782133524502, 77.43229166840096411 ) ) ;
#63453 = CARTESIAN_POINT ( 'NONE',  ( 97.64999999999997726, 91.52997821335252127, 77.67041666666665378 ) ) ;
#63454 = VERTEX_POINT ( 'NONE', #53105 ) ;
#63455 = DIRECTION ( 'NONE',  ( -0.000000000000000000, -0.000000000000000000, 1.000000000000000000 ) ) ;
#63456 = ORIENTED_EDGE ( 'NONE', *, *, #35123, .T. ) ;
#63457 = CARTESIAN_POINT ( 'NONE',  ( -97.64999999999996305, -208.4700217866474645, 83.04145833506764518 ) ) ;
#63458 = ORIENTED_EDGE ( 'NONE', *, *, #36098, .F. ) ;
#63459 = CARTESIAN_POINT ( 'NONE',  ( -92.35000000000005116, 88.47002178664754979, 88.43895833506762472 ) ) ;
#63460 = CARTESIAN_POINT ( 'NONE',  ( -92.69370383062505425, 88.66845928578038638, 81.17614583420049712 ) ) ;
#63461 = AXIS2_PLACEMENT_3D ( 'NONE', #37466, #26156, #72019 ) ;
#63462 = CARTESIAN_POINT ( 'NONE',  ( 94.99999999999998579, 87.33691857156068750, 89.32531250086715602 ) ) ;
#63463 = ORIENTED_EDGE ( 'NONE', *, *, #58767, .F. ) ;
#63464 = CARTESIAN_POINT ( 'NONE',  ( -10.00000000000000000, 0.000000000000000000, 0.000000000000000000 ) ) ;
#63465 = VECTOR ( 'NONE', #17006, 1000.000000000000000 ) ;
#63466 = AXIS2_PLACEMENT_3D ( 'NONE', #31390, #2864, #25760 ) ;
#63467 = CARTESIAN_POINT ( 'NONE',  ( 0.000000000000000000, 0.000000000000000000, 0.000000000000000000 ) ) ;
#63468 = CARTESIAN_POINT ( 'NONE',  ( -97.65000000000001990, 90.00000000000004263, 86.18999999999999773 ) ) ;
#63469 = CARTESIAN_POINT ( 'NONE',  ( -92.93550210798947830, 91.06393496763725182, 74.79348190356850523 ) ) ;
#63470 = EDGE_LOOP ( 'NONE', ( #5087, #53806, #29231 ) ) ;
#63471 = DIRECTION ( 'NONE',  ( 0.000000000000000000, 0.8660254037844432595, -0.4999999999999919509 ) ) ;
#63472 = CARTESIAN_POINT ( 'NONE',  ( -96.15314808468745866, -211.9973110713294489, 78.31864583420048120 ) ) ;
#63473 = ORIENTED_EDGE ( 'NONE', *, *, #19536, .T. ) ;
#63474 = ORIENTED_EDGE ( 'NONE', *, *, #64795, .F. ) ;
#63475 = AXIS2_PLACEMENT_3D ( 'NONE', #54617, #3504, #20020 ) ;
#63476 = FACE_BOUND ( 'NONE', #64428, .T. ) ;
#63477 = ORIENTED_EDGE ( 'NONE', *, *, #45249, .T. ) ;
#63478 = CARTESIAN_POINT ( 'NONE',  ( 92.35000000019411459, -210.0000198431783929, 84.36502760998391182 ) ) ;
#63479 = CARTESIAN_POINT ( 'NONE',  ( 0.000000000000000000, 44.99326035066052043, 68.55367621811159040 ) ) ;
#63480 = ORIENTED_EDGE ( 'NONE', *, *, #10682, .F. ) ;
#63481 = CARTESIAN_POINT ( 'NONE',  ( -93.84685191531248449, -208.0026889286704943, 77.36614583420046642 ) ) ;
#63482 = ORIENTED_EDGE ( 'NONE', *, *, #48063, .F. ) ;
#63483 = CARTESIAN_POINT ( 'NONE',  ( 10.00000000000000000, 72.35432306680485226, -20.40083707022909110 ) ) ;
#63484 = LINE ( 'NONE', #46552, #71640 ) ;
#63485 = CARTESIAN_POINT ( 'NONE',  ( -2.500000000000000000, 16.00000000000000000, 0.000000000000000000 ) ) ;
#63486 = ORIENTED_EDGE ( 'NONE', *, *, #48411, .F. ) ;
#63487 = VECTOR ( 'NONE', #6549, 1000.000000000000000 ) ;
#63488 = EDGE_CURVE ( 'NONE', #49839, #69802, #17930, .T. ) ;
#63489 = VERTEX_POINT ( 'NONE', #41813 ) ;
#63490 = FACE_OUTER_BOUND ( 'NONE', #67303, .T. ) ;
#63491 = VECTOR ( 'NONE', #49191, 1000.000000000000000 ) ;
#63492 = CARTESIAN_POINT ( 'NONE',  ( 10.00000000000000000, 0.000000000000000000, 0.000000000000000000 ) ) ;
#63493 = CARTESIAN_POINT ( 'NONE',  ( 96.15314808468748708, 88.00268892867053694, 85.40947916753380298 ) ) ;
#63494 = DIRECTION ( 'NONE',  ( 0.000000000000000000, 0.000000000000000000, 1.000000000000000000 ) ) ;
#63495 = DIRECTION ( 'NONE',  ( 0.1276937514489679404, 0.9918136447140103451, 0.000000000000000000 ) ) ;
#63496 = ADVANCED_FACE ( 'NONE', ( #14355 ), #63570, .F. ) ;
#63497 = CARTESIAN_POINT ( 'NONE',  ( 11.99999999999999822, 73.72996012237460661, -14.67089635893632504 ) ) ;
#63498 = VECTOR ( 'NONE', #21421, 1000.000000000000000 ) ;
#63499 = FACE_OUTER_BOUND ( 'NONE', #14541, .T. ) ;
#63500 = AXIS2_PLACEMENT_3D ( 'NONE', #46303, #29360, #52305 ) ;
#63501 = LINE ( 'NONE', #24009, #3232 ) ;
#63502 = ADVANCED_FACE ( 'NONE', ( #65871 ), #60241, .F. ) ;
#63503 = CARTESIAN_POINT ( 'NONE',  ( 4.084562121000262280, 3.415279651815005924, -1.156968425231149844 ) ) ;
#63504 = DIRECTION ( 'NONE',  ( -0.000000000000000000, -0.000000000000000000, 1.000000000000000000 ) ) ;
#63505 = LINE ( 'NONE', #67650, #454 ) ;
#63506 = ADVANCED_FACE ( 'NONE', ( #2752 ), #42564, .F. ) ;
#63507 = LINE ( 'NONE', #5628, #204 ) ;
#63508 = CARTESIAN_POINT ( 'NONE',  ( 10.00000000000000000, 0.000000000000000000, 0.000000000000000000 ) ) ;
#63509 = VECTOR ( 'NONE', #25717, 1000.000000000000000 ) ;
#63510 = PLANE ( 'NONE',  #29636 ) ;
#63511 = EDGE_CURVE ( 'NONE', #6829, #70343, #31637, .T. ) ;
#63512 = ORIENTED_EDGE ( 'NONE', *, *, #33105, .T. ) ;
#63513 =( BOUNDED_CURVE ( )  B_SPLINE_CURVE ( 2, ( #56923, #5430, #45654, #53760, #28325, #191, #22714 ),
 .UNSPECIFIED., .F., .F. ) 
 B_SPLINE_CURVE_WITH_KNOTS ( ( 3, 2, 2, 3 ),
 ( 0.000000000000000000, 0.006944444444444406762, 0.01388888888888881352, 0.02083333333333322115 ),
 .UNSPECIFIED. ) 
 CURVE ( )  GEOMETRIC_REPRESENTATION_ITEM ( )  RATIONAL_B_SPLINE_CURVE ( ( 1.000000000000000000, 0.8660254037844387076, 1.000000000000000000, 0.8660254037844387076, 1.000000000000000000, 0.8660254037844408170, 0.9999999999999978906 ) ) 
 REPRESENTATION_ITEM ( '' )  );
#63514 = CIRCLE ( 'NONE', #69506, 37.49900000000000944 ) ;
#63515 = DIRECTION ( 'NONE',  ( 0.000000000000000000, 0.7071067811865439090, 0.7071067811865512365 ) ) ;
#63516 = ADVANCED_FACE ( 'NONE', ( #26001 ), #8350, .F. ) ;
#63517 = DIRECTION ( 'NONE',  ( -1.000000000000000000, 0.000000000000000000, 0.000000000000000000 ) ) ;
#63518 = LINE ( 'NONE', #65639, #8192 ) ;
#63519 = AXIS2_PLACEMENT_3D ( 'NONE', #23127, #69711, #64450 ) ;
#63520 = AXIS2_PLACEMENT_3D ( 'NONE', #10499, #49603, #67282 ) ;
#63521 = CARTESIAN_POINT ( 'NONE',  ( 0.000000000000000000, 31.52238457039637609, -27.75498641678709788 ) ) ;
#63522 = ADVANCED_FACE ( 'NONE', ( #65503 ), #53471, .F. ) ;
#63523 = CARTESIAN_POINT ( 'NONE',  ( 93.84685191531251292, -211.9973110713294489, 84.82739583420048746 ) ) ;
#63524 = ORIENTED_EDGE ( 'NONE', *, *, #67561, .T. ) ;
#63525 = VERTEX_POINT ( 'NONE', #2008 ) ;
#63526 = EDGE_CURVE ( 'NONE', #33020, #47477, #53959, .T. ) ;
#63527 = CARTESIAN_POINT ( 'NONE',  ( -92.34999999999989484, -208.4700217866475214, 85.92541666666664923 ) ) ;
#63528 = ORIENTED_EDGE ( 'NONE', *, *, #48358, .T. ) ;
#63529 = CARTESIAN_POINT ( 'NONE',  ( -92.34999999999999432, -208.4700217866474645, 79.65479166840096070 ) ) ;
#63530 = CARTESIAN_POINT ( 'NONE',  ( 93.84685191531249870, -208.0026889286704943, 74.93197916753379673 ) ) ;
#63531 = ORIENTED_EDGE ( 'NONE', *, *, #34162, .F. ) ;
#63532 = CARTESIAN_POINT ( 'NONE',  ( 96.15314808468748708, -208.0026889286704943, 83.23989583420049598 ) ) ;
#63533 = AXIS2_PLACEMENT_3D ( 'NONE', #37314, #43334, #53847 ) ;
#63534 = ORIENTED_EDGE ( 'NONE', *, *, #69177, .F. ) ;
#63535 = ORIENTED_EDGE ( 'NONE', *, *, #27911, .T. ) ;
#63536 = ORIENTED_EDGE ( 'NONE', *, *, #24856, .T. ) ;
#63537 = CARTESIAN_POINT ( 'NONE',  ( 10.00000000000000000, 0.000000000000000000, 0.000000000000000000 ) ) ;
#63538 = CIRCLE ( 'NONE', #56345, 31.99999999999998934 ) ;
#63539 = CIRCLE ( 'NONE', #11889, 31.99999999999998224 ) ;
#63540 = CARTESIAN_POINT ( 'NONE',  ( -11.70000000000000107, 0.000000000000000000, 0.000000000000000000 ) ) ;
#63541 = AXIS2_PLACEMENT_3D ( 'NONE', #40591, #34205, #68804 ) ;
#63542 = EDGE_LOOP ( 'NONE', ( #40312, #13003, #22564, #52905 ) ) ;
#63543 = DIRECTION ( 'NONE',  ( -1.000000000000000000, 0.000000000000000000, 0.000000000000000000 ) ) ;
#63544 = CARTESIAN_POINT ( 'NONE',  ( 96.32499999999998863, -212.2949673200287179, 85.84604166840097150 ) ) ;
#63545 = AXIS2_PLACEMENT_3D ( 'NONE', #38719, #49249, #37975 ) ;
#63546 = ORIENTED_EDGE ( 'NONE', *, *, #30696, .F. ) ;
#63547 = DIRECTION ( 'NONE',  ( 1.000000000000000000, 0.000000000000000000, 0.000000000000000000 ) ) ;
#63548 = ORIENTED_EDGE ( 'NONE', *, *, #47599, .F. ) ;
#63549 = CIRCLE ( 'NONE', #10552, 16.00000000000000000 ) ;
#63550 = FACE_OUTER_BOUND ( 'NONE', #23137, .T. ) ;
#63551 = VERTEX_POINT ( 'NONE', #1642 ) ;
#63552 = ORIENTED_EDGE ( 'NONE', *, *, #4336, .F. ) ;
#63553 = EDGE_LOOP ( 'NONE', ( #41462, #7743, #4259, #61523 ) ) ;
#63554 = CARTESIAN_POINT ( 'NONE',  ( 0.000000000000000000, 0.000000000000000000, -54.99999999999998579 ) ) ;
#63555 = CONTEXT_DEPENDENT_SHAPE_REPRESENTATION ( #45121, #8078 ) ;
#63556 = DIRECTION ( 'NONE',  ( -1.000000000000000000, -0.000000000000000000, -0.000000000000000000 ) ) ;
#63557 = ORIENTED_EDGE ( 'NONE', *, *, #53137, .F. ) ;
#63558 = VERTEX_POINT ( 'NONE', #30159 ) ;
#63559 = EDGE_LOOP ( 'NONE', ( #73191, #33757, #53604, #69541 ) ) ;
#63560 = DIRECTION ( 'NONE',  ( -1.000000000000000000, 0.000000000000000000, -0.000000000000000000 ) ) ;
#63561 = CARTESIAN_POINT ( 'NONE',  ( 11.99999999999999822, 80.55351364060611274, -15.33399622253397609 ) ) ;
#63563 = CARTESIAN_POINT ( 'NONE',  ( -93.67500000000003979, 87.70503267997129626, 88.30666666666665776 ) ) ;
#63562 = VECTOR ( 'NONE', #8342, 1000.000000000000000 ) ;
#63564 = ORIENTED_EDGE ( 'NONE', *, *, #58490, .F. ) ;
#63565 = CARTESIAN_POINT ( 'NONE',  ( 100.0000000000260343, -214.9999999999999716, 75.00000000000001421 ) ) ;
#63566 = ORIENTED_EDGE ( 'NONE', *, *, #44433, .T. ) ;
#63567 = CARTESIAN_POINT ( 'NONE',  ( 10.00000000000000000, 40.68715046381928602, 10.41901085202092503 ) ) ;
#63568 = CARTESIAN_POINT ( 'NONE',  ( -97.30629616937497417, -208.6684592857803011, 87.68489583420047495 ) ) ;
#63569 = ORIENTED_EDGE ( 'NONE', *, *, #40770, .F. ) ;
#63570 = CONICAL_SURFACE ( 'NONE', #50344, 17.30399999999999849, 0.2094395102393129815 ) ;
#63571 = DIRECTION ( 'NONE',  ( -1.000000000000000000, -0.000000000000000000, 0.000000000000000000 ) ) ;
#63572 = DIRECTION ( 'NONE',  ( -1.000000000000000000, -0.000000000000000000, -0.000000000000000000 ) ) ;
#63573 = CARTESIAN_POINT ( 'NONE',  ( 10.00000000000000000, 16.65560815589411092, 38.55633173627015964 ) ) ;
#63574 = CARTESIAN_POINT ( 'NONE',  ( -93.84685191531247028, -211.9973110713294489, 75.88447916753381151 ) ) ;
#63575 = AXIS2_PLACEMENT_3D ( 'NONE', #15527, #67778, #73399 ) ;
#63576 = AXIS2_PLACEMENT_3D ( 'NONE', #33811, #11251, #28165 ) ;
#63577 = ADVANCED_FACE ( 'NONE', ( #19984 ), #21508, .T. ) ;
#63578 = AXIS2_PLACEMENT_3D ( 'NONE', #65609, #14829, #54690 ) ;
#63579 = DIRECTION ( 'NONE',  ( 1.000000000000000000, 0.000000000000000000, 0.000000000000000000 ) ) ;
#63580 = CARTESIAN_POINT ( 'NONE',  ( 0.000000000000000000, 0.000000000000000000, 0.000000000000000000 ) ) ;
#63581 = EDGE_CURVE ( 'NONE', #6695, #55639, #71849, .T. ) ;
#63582 = CARTESIAN_POINT ( 'NONE',  ( -97.65000000000001990, 88.47002178664754979, 85.05229166840096866 ) ) ;
#63583 = ADVANCED_FACE ( 'NONE', ( #66244 ), #35792, .F. ) ;
#63585 = AXIS2_PLACEMENT_3D ( 'NONE', #1500, #47684, #58977 ) ;
#63584 = PLANE ( 'NONE',  #15587 ) ;
#63586 = EDGE_CURVE ( 'NONE', #36276, #39410, #9501, .T. ) ;
#63587 = CARTESIAN_POINT ( 'NONE',  ( 10.00000000000000000, -74.65491531819111515, -8.830959090343204920 ) ) ;
#63588 = CARTESIAN_POINT ( 'NONE',  ( -10.00000000000000000, 0.000000000000000000, 0.000000000000000000 ) ) ;
#63589 = CARTESIAN_POINT ( 'NONE',  ( -92.69370383062504004, 90.00000000000004263, 77.89531250086714920 ) ) ;
#63590 = CARTESIAN_POINT ( 'NONE',  ( 10.00000000000000000, 68.26794271651307611, -31.47745569255064169 ) ) ;
#63591 = DIRECTION ( 'NONE',  ( -0.000000000000000000, -0.000000000000000000, 1.000000000000000000 ) ) ;
#63592 = EDGE_CURVE ( 'NONE', #6488, #26693, #47462, .T. ) ;
#63593 = VERTEX_POINT ( 'NONE', #24897 ) ;
#63594 = CARTESIAN_POINT ( 'NONE',  ( 92.34999999999999432, 90.00000000000002842, 79.28437500173430408 ) ) ;
#63595 = VECTOR ( 'NONE', #18781, 1000.000000000000114 ) ;
#63596 = EDGE_CURVE ( 'NONE', #11817, #26794, #39273, .T. ) ;
#63597 = CARTESIAN_POINT ( 'NONE',  ( -97.64999999999996305, -209.9999999999999716, 81.10999999999999943 ) ) ;
#63599 = CARTESIAN_POINT ( 'NONE',  ( 15.00000000000000000, -25.60904388321925040, -6.976881207771165272 ) ) ;
#63598 = AXIS2_PLACEMENT_3D ( 'NONE', #49471, #32907, #15262 ) ;
#63600 = CARTESIAN_POINT ( 'NONE',  ( 10.00000000000000000, 36.13751322684449718, -21.40280677340333071 ) ) ;
#63601 = LINE ( 'NONE', #28991, #73038 ) ;
#63602 = CARTESIAN_POINT ( 'NONE',  ( 10.00000000000000000, 0.000000000000000000, 0.000000000000000000 ) ) ;
#63603 = CARTESIAN_POINT ( 'NONE',  ( -93.84685191531248449, -208.0026889286704943, 76.25489583420049655 ) ) ;
#63604 = AXIS2_PLACEMENT_3D ( 'NONE', #57062, #5198, #64093 ) ;
#63605 = VECTOR ( 'NONE', #41671, 1000.000000000000000 ) ;
#63606 = CARTESIAN_POINT ( 'NONE',  ( 10.00000000000000000, 74.65374052328648702, 8.840884882375350529 ) ) ;
#63607 = ORIENTED_EDGE ( 'NONE', *, *, #40080, .F. ) ;
#63608 = FACE_OUTER_BOUND ( 'NONE', #3718, .T. ) ;
#63609 = ADVANCED_FACE ( 'NONE', ( #26732, #15456 ), #37669, .F. ) ;
#63610 = CARTESIAN_POINT ( 'NONE',  ( 0.000000000000000000, 0.000000000000000000, 0.000000000000000000 ) ) ;
#63611 = DIRECTION ( 'NONE',  ( -0.7950889364178798102, 0.6064928550163511956, 0.000000000000000000 ) ) ;
#63612 = CARTESIAN_POINT ( 'NONE',  ( 0.000000000000000000, 2.446882695291915554E-15, 2.500000000000016431 ) ) ;
#63613 = EDGE_CURVE ( 'NONE', #22472, #44000, #56059, .T. ) ;
#63614 = EDGE_CURVE ( 'NONE', #4987, #5465, #46765, .T. ) ;
#63615 = DIRECTION ( 'NONE',  ( 0.000000000000000000, 0.000000000000000000, 1.000000000000000000 ) ) ;
#63616 = ORIENTED_EDGE ( 'NONE', *, *, #70886, .F. ) ;
#63617 = CARTESIAN_POINT ( 'NONE',  ( 97.64999999999999147, 90.00000000000002842, 81.42749999999999488 ) ) ;
#63618 = ADVANCED_FACE ( 'NONE', ( #32738 ), #16203, .T. ) ;
#63619 = DIRECTION ( 'NONE',  ( 0.000000000000000000, 0.000000000000000000, 1.000000000000000000 ) ) ;
#63620 = VERTEX_POINT ( 'NONE', #61341 ) ;
#63621 = AXIS2_PLACEMENT_3D ( 'NONE', #37942, #62662, #55601 ) ;
#63622 = CARTESIAN_POINT ( 'NONE',  ( 95.00000000000000000, -212.6630814284392557, 84.72156250086713669 ) ) ;
#63623 = FACE_OUTER_BOUND ( 'NONE', #47270, .T. ) ;
#63624 = MANIFOLD_SOLID_BREP ( 'Boss-Extrude1', #42783 ) ;
#63625 = EDGE_LOOP ( 'NONE', ( #45437, #38760, #1344, #31083 ) ) ;
#63626 = AXIS2_PLACEMENT_3D ( 'NONE', #54985, #50072, #62506 ) ;
#63627 = FACE_OUTER_BOUND ( 'NONE', #28879, .T. ) ;
#63628 = TOROIDAL_SURFACE ( 'NONE', #40818, 12.80000000000000071, 0.2999999999999999334 ) ;
#63629 = ORIENTED_EDGE ( 'NONE', *, *, #9141, .T. ) ;
#63630 = CARTESIAN_POINT ( 'NONE',  ( 10.00000000000000000, -24.73286445877653961, -73.44644590900085745 ) ) ;
#63631 = ORIENTED_EDGE ( 'NONE', *, *, #66278, .T. ) ;
#63632 = CARTESIAN_POINT ( 'NONE',  ( -97.30629616937501680, 88.66845928578038638, 81.59947916753381492 ) ) ;
#63633 = VERTEX_POINT ( 'NONE', #27852 ) ;
#63634 = VERTEX_POINT ( 'NONE', #72955 ) ;
#63635 = ORIENTED_EDGE ( 'NONE', *, *, #16538, .F. ) ;
#63636 = DIRECTION ( 'NONE',  ( -1.000000000000000000, -0.000000000000000000, 0.000000000000000000 ) ) ;
#63637 = VERTEX_POINT ( 'NONE', #20733 ) ;
#63638 = ORIENTED_EDGE ( 'NONE', *, *, #46042, .T. ) ;
#63639 = CARTESIAN_POINT ( 'NONE',  ( 93.08933536981345469, 88.26122129797421678, 74.95660481729451874 ) ) ;
#63640 = ORIENTED_EDGE ( 'NONE', *, *, #23420, .T. ) ;
#63641 = VERTEX_POINT ( 'NONE', #56442 ) ;
#63642 = CARTESIAN_POINT ( 'NONE',  ( 92.69370383062498320, 90.00000000000002842, 86.46781250086714010 ) ) ;
#63643 = ORIENTED_EDGE ( 'NONE', *, *, #53571, .T. ) ;
#63644 = VECTOR ( 'NONE', #44641, 999.9999999999998863 ) ;
#63645 = CARTESIAN_POINT ( 'NONE',  ( 97.30629616937498838, -209.9999999999999716, 82.34031250086714238 ) ) ;
#63646 = AXIS2_PLACEMENT_3D ( 'NONE', #51977, #47094, #39601 ) ;
#63647 = CIRCLE ( 'NONE', #45622, 16.00000000000000000 ) ;
#63648 = CONTEXT_DEPENDENT_SHAPE_REPRESENTATION ( #45575, #43990 ) ;
#63649 = DIRECTION ( 'NONE',  ( -1.000000000000000000, -0.000000000000000000, -0.000000000000000000 ) ) ;
#63650 = PLANE ( 'NONE',  #2868 ) ;
#63651 = FACE_OUTER_BOUND ( 'NONE', #65569, .T. ) ;
#63652 = PLANE ( 'NONE',  #30749 ) ;
#63653 = CARTESIAN_POINT ( 'NONE',  ( -92.35000000000005116, 88.47002178664754979, 79.46958333333331836 ) ) ;
#63654 = PLANE ( 'NONE',  #26296 ) ;
#63655 = CIRCLE ( 'NONE', #69646, 77.49900000000002365 ) ;
#63656 = CARTESIAN_POINT ( 'NONE',  ( -92.69370383062498320, -208.6684592857803011, 84.93322916753379559 ) ) ;
#63657 = CARTESIAN_POINT ( 'NONE',  ( -95.00000000000002842, 87.33691857156074434, 81.07031250086716057 ) ) ;
#63658 = VERTEX_POINT ( 'NONE', #50780 ) ;
#63659 = CARTESIAN_POINT ( 'NONE',  ( 96.15314808468748708, 88.00268892867053694, 86.04447916753380809 ) ) ;
#63660 = ORIENTED_EDGE ( 'NONE', *, *, #19411, .F. ) ;
#63661 = CARTESIAN_POINT ( 'NONE',  ( 10.00000000000000000, -14.66109333815410487, -73.73191006444587003 ) ) ;
#63662 = B_SPLINE_CURVE_WITH_KNOTS ( 'NONE', 3,
 ( #7347, #46833, #6959, #29884 ),
 .UNSPECIFIED., .F., .F.,
 ( 4, 4 ),
 ( 2.380735200821679637E-07, 0.002921158011986721599 ),
 .UNSPECIFIED. ) ;
#63663 = CARTESIAN_POINT ( 'NONE',  ( 10.00000000000000000, 0.000000000000000000, 0.000000000000000000 ) ) ;
#63664 = LINE ( 'NONE', #12133, #10318 ) ;
#63665 = DIRECTION ( 'NONE',  ( -8.587739980083048116E-16, -1.065814103640131346E-14, -1.000000000000000000 ) ) ;
#63666 = CARTESIAN_POINT ( 'NONE',  ( -97.30629616937497417, -211.3315407142195852, 87.79072916753379729 ) ) ;
#63667 = CARTESIAN_POINT ( 'NONE',  ( 0.000000000000000000, 16.65972982745046238, -80.28980883073738539 ) ) ;
#63668 = ADVANCED_FACE ( 'NONE', ( #43684 ), #66960, .T. ) ;
#63669 = CARTESIAN_POINT ( 'NONE',  ( 2.750000000000000000, 0.000000000000000000, 0.000000000000000000 ) ) ;
#63670 = DIRECTION ( 'NONE',  ( -1.000000000000000000, -0.000000000000000000, 0.000000000000000000 ) ) ;
#63671 = CARTESIAN_POINT ( 'NONE',  ( -92.35000000000553655, 89.99999459739531460, 81.50687481489494246 ) ) ;
#63672 = VERTEX_POINT ( 'NONE', #32005 ) ;
#63673 = EDGE_CURVE ( 'NONE', #26241, #43461, #55120, .T. ) ;
#63674 = ORIENTED_EDGE ( 'NONE', *, *, #19272, .F. ) ;
#63675 = ADVANCED_FACE ( 'NONE', ( #26370 ), #49300, .F. ) ;
#63676 = EDGE_CURVE ( 'NONE', #71724, #68795, #66604, .T. ) ;
#63677 = CARTESIAN_POINT ( 'NONE',  ( -92.35000000000005116, 91.52997821335253548, 78.94041666666666401 ) ) ;
#63678 = CARTESIAN_POINT ( 'NONE',  ( 10.00000000000000000, -30.80686688396994910, -21.53537804866113703 ) ) ;
#63679 = CARTESIAN_POINT ( 'NONE',  ( -95.43397055421739594, -207.6412937382899031, 74.84690984288805282 ) ) ;
#63680 = CARTESIAN_POINT ( 'NONE',  ( -10.00000000000000000, 0.000000000000000000, 0.000000000000000000 ) ) ;
#63681 = DIRECTION ( 'NONE',  ( 2.603472992745699578E-14, -2.546204323184531851E-14, 1.000000000000000000 ) ) ;
#63682 = CARTESIAN_POINT ( 'NONE',  ( 10.00000000000000000, 0.000000000000000000, 0.000000000000000000 ) ) ;
#63683 = CIRCLE ( 'NONE', #49214, 16.00000000000000000 ) ;
#63684 = VERTEX_POINT ( 'NONE', #60957 ) ;
#63685 = CARTESIAN_POINT ( 'NONE',  ( -92.69370383062502583, 91.33154071421968467, 79.85322916753379729 ) ) ;
#63687 = DIRECTION ( 'NONE',  ( 0.000000000000000000, 0.000000000000000000, -1.000000000000000000 ) ) ;
#63686 = VECTOR ( 'NONE', #64590, 1000.000000000000114 ) ;
#63688 = AXIS2_PLACEMENT_3D ( 'NONE', #40844, #13360, #70125 ) ;
#63689 = DIRECTION ( 'NONE',  ( -1.000000000000000000, 0.000000000000000000, 0.000000000000000000 ) ) ;
#63690 = CARTESIAN_POINT ( 'NONE',  ( 0.000000000000000000, 41.76106447765489094, 62.50884508063442269 ) ) ;
#63691 = CARTESIAN_POINT ( 'NONE',  ( 95.00000000000000000, -206.9400435732949575, 84.20562500173429044 ) ) ;
#63692 = DIRECTION ( 'NONE',  ( 0.000000000000000000, -6.938893903907228378E-15, 1.000000000000000000 ) ) ;
#63693 = CARTESIAN_POINT ( 'NONE',  ( -92.69370383062498320, -211.3315407142195852, 84.98614583420047097 ) ) ;
#63694 = EDGE_CURVE ( 'NONE', #7677, #13386, #44348, .T. ) ;
#63695 = DIRECTION ( 'NONE',  ( 0.000000000000000000, 0.000000000000000000, -1.000000000000000000 ) ) ;
#63696 = CARTESIAN_POINT ( 'NONE',  ( 94.99999999999998579, 92.66308142843932671, 77.57781250086715374 ) ) ;
#63697 = CARTESIAN_POINT ( 'NONE',  ( -94.99999999999997158, -207.3369185715606307, 77.57781250086715374 ) ) ;
#63698 = CARTESIAN_POINT ( 'NONE',  ( 4.749999999999999112, 5.817072295949926440E-16, 0.000000000000000000 ) ) ;
#63699 = ORIENTED_EDGE ( 'NONE', *, *, #40826, .T. ) ;
#63700 = CYLINDRICAL_SURFACE ( 'NONE', #44904, 31.99999999999998579 ) ;
#63701 = DIRECTION ( 'NONE',  ( 0.000000000000000000, -0.9945218953682742891, -0.1045284632676436315 ) ) ;
#63702 = CARTESIAN_POINT ( 'NONE',  ( 16.84844760790522855, -103.5491698323862124, -5.500000000000000000 ) ) ;
#63703 = CIRCLE ( 'NONE', #61275, 82.00000000000000000 ) ;
#63704 = EDGE_CURVE ( 'NONE', #66690, #70972, #85, .T. ) ;
#63705 = EDGE_CURVE ( 'NONE', #70313, #62456, #63937, .T. ) ;
#63706 = AXIS2_PLACEMENT_3D ( 'NONE', #64286, #17298, #46990 ) ;
#63707 = FACE_BOUND ( 'NONE', #33466, .T. ) ;
#63708 = CARTESIAN_POINT ( 'NONE',  ( 93.84685191531251292, -211.9973110713294489, 78.31864583420048120 ) ) ;
#63709 = VERTEX_POINT ( 'NONE', #28968 ) ;
#63710 = CARTESIAN_POINT ( 'NONE',  ( 3.429551818649054340, -146.3199197248623875, -5.500000000000000000 ) ) ;
#63711 = ORIENTED_EDGE ( 'NONE', *, *, #18562, .T. ) ;
#63712 = FACE_OUTER_BOUND ( 'NONE', #63240, .T. ) ;
#63713 = ORIENTED_EDGE ( 'NONE', *, *, #72299, .F. ) ;
#63714 = CARTESIAN_POINT ( 'NONE',  ( 92.35000000000000853, -209.9999999999999716, 83.65000000000000568 ) ) ;
#63715 = EDGE_LOOP ( 'NONE', ( #24965, #4123, #8034, #32243 ) ) ;
#63716 = ORIENTED_EDGE ( 'NONE', *, *, #451, .T. ) ;
#63717 = VERTEX_POINT ( 'NONE', #45542 ) ;
#63718 = CARTESIAN_POINT ( 'NONE',  ( 97.64999999999999147, -209.9999998456624155, 79.60187500750917877 ) ) ;
#63719 = VERTEX_POINT ( 'NONE', #23699 ) ;
#63720 = ORIENTED_EDGE ( 'NONE', *, *, #60701, .T. ) ;
#63721 = CARTESIAN_POINT ( 'NONE',  ( 94.99999999999998579, 87.33691857156068750, 83.61031250086716682 ) ) ;
#63722 = CARTESIAN_POINT ( 'NONE',  ( -10.00000000000000000, 0.000000000000000000, 0.000000000000000000 ) ) ;
#63723 = ORIENTED_EDGE ( 'NONE', *, *, #33329, .T. ) ;
#63724 = VERTEX_POINT ( 'NONE', #68466 ) ;
#63725 = AXIS2_PLACEMENT_3D ( 'NONE', #21295, #14185, #42772 ) ;
#63726 = VERTEX_POINT ( 'NONE', #29325 ) ;
#63727 = VERTEX_POINT ( 'NONE', #63567 ) ;
#63728 = CARTESIAN_POINT ( 'NONE',  ( 11.99999999999999822, -14.67089635893764665, 73.72996012237435082 ) ) ;
#63729 = VECTOR ( 'NONE', #73819, 1000.000000000000000 ) ;
#63730 = VERTEX_POINT ( 'NONE', #22978 ) ;
#63731 = B_SPLINE_CURVE_WITH_KNOTS ( 'NONE', 3,
 ( #72010, #20520, #43478, #66396, #37821, #60752, #9229, #32151, #15624, #61494, #26889, #15243, #73120, #3624, #11096, #26523, #38177, #45319 ),
 .UNSPECIFIED., .F., .F.,
 ( 4, 2, 2, 2, 2, 2, 2, 2, 4 ),
 ( -0.004093595874563257103, -0.003575961937392224069, -0.003058328000221191036, -0.002540694063050158436, -0.002023060125879125402, -0.001505426188708092368, -0.0009877922515370597678, -0.0004701583143660267340, 4.747562280500629978E-05 ),
 .UNSPECIFIED. ) ;
#63732 = DIRECTION ( 'NONE',  ( 0.7633350786957842082, 0.6460027535796584175, -4.719448930578168776E-15 ) ) ;
#63733 = CARTESIAN_POINT ( 'NONE',  ( -97.64999999999996305, -208.4700217866474645, 75.42145833506764063 ) ) ;
#63734 = DIRECTION ( 'NONE',  ( -1.000000000000000000, 0.000000000000000000, -0.000000000000000000 ) ) ;
#63735 = DIRECTION ( 'NONE',  ( 0.000000000000000000, -0.9945218953682730678, -0.1045284632676570791 ) ) ;
#63736 = CARTESIAN_POINT ( 'NONE',  ( 93.67500000000001137, -212.2949673200287179, 87.01020833506763097 ) ) ;
#63737 = DIRECTION ( 'NONE',  ( 1.000000000000000000, 0.000000000000000000, 0.000000000000000000 ) ) ;
#63738 = LINE ( 'NONE', #53552, #23643 ) ;
#63739 = VERTEX_POINT ( 'NONE', #68834 ) ;
#63740 = CARTESIAN_POINT ( 'NONE',  ( -92.34999999999999432, -211.5299782133524502, 80.18395833506764347 ) ) ;
#63741 = ORIENTED_EDGE ( 'NONE', *, *, #14406, .T. ) ;
#63742 = DIRECTION ( 'NONE',  ( 0.000000000000000000, -0.000000000000000000, 1.000000000000000000 ) ) ;
#63743 = ORIENTED_EDGE ( 'NONE', *, *, #71718, .T. ) ;
#63745 = CARTESIAN_POINT ( 'NONE',  ( -92.35000000000005116, 91.52997821335253548, 78.38479166840096468 ) ) ;
#63744 = CARTESIAN_POINT ( 'NONE',  ( 93.67499999999998295, 92.29496732002878900, 78.54354166840096241 ) ) ;
#63746 =( BOUNDED_CURVE ( )  B_SPLINE_CURVE ( 2, ( #20025, #65918, #14394, #37343, #60282, #8761, #54621 ),
 .UNSPECIFIED., .F., .F. ) 
 B_SPLINE_CURVE_WITH_KNOTS ( ( 3, 2, 2, 3 ),
 ( 0.7499999999999996669, 0.7569444444444439757, 0.7638888888888883955, 0.7708333333333328152 ),
 .UNSPECIFIED. ) 
 CURVE ( )  GEOMETRIC_REPRESENTATION_ITEM ( )  RATIONAL_B_SPLINE_CURVE ( ( 1.000000000000006439, 0.8660254037844322683, 1.000000000000000000, 0.8660254037844387076, 1.000000000000000000, 0.8660254037844493658, 0.9999999999999893419 ) ) 
 REPRESENTATION_ITEM ( '' )  );
#63747 = ORIENTED_EDGE ( 'NONE', *, *, #50910, .T. ) ;
#63748 = CARTESIAN_POINT ( 'NONE',  ( 93.84685191531248449, 88.00268892867053694, 79.11239583420048405 ) ) ;
#63749 = DIRECTION ( 'NONE',  ( 1.000000000000000000, 0.000000000000000000, 0.000000000000000000 ) ) ;
#63750 = PRODUCT_DEFINITION ( 'UNKNOWN', '', #60394, #59703 ) ;
#63751 = CARTESIAN_POINT ( 'NONE',  ( 25.44550000000002399, 0.000000000000000000, 0.000000000000000000 ) ) ;
#63752 = ADVANCED_FACE ( 'NONE', ( #74084 ), #52269, .F. ) ;
#63753 = CARTESIAN_POINT ( 'NONE',  ( -93.67500000000003979, 92.29496732002878900, 86.69270833506763552 ) ) ;
#63754 = VECTOR ( 'NONE', #20278, 1000.000000000000000 ) ;
#63755 = CARTESIAN_POINT ( 'NONE',  ( 0.000000000000000000, 18.84667830672579925, 18.68964196561269020 ) ) ;
#63756 = B_SPLINE_CURVE_WITH_KNOTS ( 'NONE', 3,
 ( #50664, #57805, #28470, #16844, #40138, #39777, #23228, #51405 ),
 .UNSPECIFIED., .F., .F.,
 ( 4, 2, 2, 4 ),
 ( 0.002921158011986721599, 0.003648658599403073119, 0.004376159186819424639, 0.005831160361652126811 ),
 .UNSPECIFIED. ) ;
#63757 = EDGE_LOOP ( 'NONE', ( #58703, #36085, #27352, #46410 ) ) ;
#63758 = CARTESIAN_POINT ( 'NONE',  ( 97.64999999999999147, 90.00000000000002842, 78.25249999999999773 ) ) ;
#63759 = AXIS2_PLACEMENT_3D ( 'NONE', #64123, #17874, #1376 ) ;
#63760 = CARTESIAN_POINT ( 'NONE',  ( -2.287832656137188891, 4.452621892014637872, -6.000000000000004441 ) ) ;
#63761 = ORIENTED_EDGE ( 'NONE', *, *, #69941, .F. ) ;
#63762 = CIRCLE ( 'NONE', #73324, 31.99999999999999289 ) ;
#63763 = EDGE_CURVE ( 'NONE', #16380, #28262, #45909, .T. ) ;
#63764 = ORIENTED_EDGE ( 'NONE', *, *, #53986, .F. ) ;
#63765 = VECTOR ( 'NONE', #56382, 1000.000000000000000 ) ;
#63766 = EDGE_CURVE ( 'NONE', #19845, #56042, #811, .T. ) ;
#63767 = DIRECTION ( 'NONE',  ( 0.000000000000000000, 0.000000000000000000, 1.000000000000000000 ) ) ;
#63768 = CARTESIAN_POINT ( 'NONE',  ( -0.1709976663249050954, -5.674777143212785369, -1.879366290983713217 ) ) ;
#63769 = DIRECTION ( 'NONE',  ( 1.000000000000000000, 0.000000000000000000, 0.000000000000000000 ) ) ;
#63770 = CARTESIAN_POINT ( 'NONE',  ( -92.69370383062498320, -208.6684592857803011, 78.10697916753383652 ) ) ;
#63771 = EDGE_CURVE ( 'NONE', #45, #24268, #21578, .T. ) ;
#63772 = ORIENTED_EDGE ( 'NONE', *, *, #8569, .T. ) ;
#63773 = CYLINDRICAL_SURFACE ( 'NONE', #18695, 16.00000000000000000 ) ;
#63774 = CARTESIAN_POINT ( 'NONE',  ( -7.572224309238338336, -145.4393675041377492, 5.500000000000000000 ) ) ;
#63775 = LINE ( 'NONE', #64139, #51422 ) ;
#63776 = CARTESIAN_POINT ( 'NONE',  ( 0.000000000000000000, 77.19088730480524418, 6.903761155838049390 ) ) ;
#63777 = DIRECTION ( 'NONE',  ( 0.000000000000000000, 0.3090169943749410675, 0.9510565162951556406 ) ) ;
#63778 = LINE ( 'NONE', #59233, #36074 ) ;
#63779 = DIRECTION ( 'NONE',  ( 0.000000000000000000, 0.000000000000000000, 1.000000000000000000 ) ) ;
#63780 = DIRECTION ( 'NONE',  ( 0.000000000000000000, -0.5877852522924802425, 0.8090169943749422332 ) ) ;
#63781 = DIRECTION ( 'NONE',  ( -0.000000000000000000, -0.000000000000000000, 1.000000000000000000 ) ) ;
#63782 = ADVANCED_FACE ( 'NONE', ( #18063 ), #50387, .F. ) ;
#63783 = CARTESIAN_POINT ( 'NONE',  ( 100.0010000000000474, -65.00000000000002842, -90.00000000000000000 ) ) ;
#63784 = ADVANCED_FACE ( 'NONE', ( #6062 ), #51901, .T. ) ;
#63785 = CARTESIAN_POINT ( 'NONE',  ( 94.99999999999998579, 87.33691857156068750, 88.05531250086714579 ) ) ;
#63786 = CARTESIAN_POINT ( 'NONE',  ( 10.00000000000000000, 0.000000000000000000, 0.000000000000000000 ) ) ;
#63787 = LINE ( 'NONE', #57393, #2606 ) ;
#63788 = VERTEX_POINT ( 'NONE', #12412 ) ;
#63789 =( GEOMETRIC_REPRESENTATION_CONTEXT ( 3 ) GLOBAL_UNCERTAINTY_ASSIGNED_CONTEXT ( ( #15176 ) ) GLOBAL_UNIT_ASSIGNED_CONTEXT ( ( #38524, #10317, #11067 ) ) REPRESENTATION_CONTEXT ( 'NONE', 'WORKASPACE' ) );
#63790 = DIRECTION ( 'NONE',  ( 0.000000000000000000, 0.000000000000000000, 1.000000000000000000 ) ) ;
#63791 = CIRCLE ( 'NONE', #46971, 31.99999999999999289 ) ;
#63792 = CARTESIAN_POINT ( 'NONE',  ( -95.00000000000002842, 92.66308142843932671, 76.14906250086716000 ) ) ;
#63793 = CIRCLE ( 'NONE', #49376, 3.299999999999983391 ) ;
#63794 = EDGE_CURVE ( 'NONE', #74237, #41316, #35359, .T. ) ;
#63795 = CARTESIAN_POINT ( 'NONE',  ( 92.69370383062501162, -211.3315407142195852, 87.15572916753380639 ) ) ;
#63796 = APPLICATION_CONTEXT ( 'automotive_design' ) ;
#63797 = ORIENTED_EDGE ( 'NONE', *, *, #25310, .T. ) ;
#63798 = CARTESIAN_POINT ( 'NONE',  ( -92.34999999999999432, -210.0000000024460576, 75.15687493084206494 ) ) ;
#63799 = ORIENTED_EDGE ( 'NONE', *, *, #27672, .T. ) ;
#63800 = AXIS2_PLACEMENT_3D ( 'NONE', #21945, #50124, #33587 ) ;
#63801 = CARTESIAN_POINT ( 'NONE',  ( 10.00000000000000000, 0.000000000000000000, 0.000000000000000000 ) ) ;
#63803 = DIRECTION ( 'NONE',  ( -1.000000000000000000, -0.000000000000000000, 0.000000000000000000 ) ) ;
#63802 = AXIS2_PLACEMENT_3D ( 'NONE', #39800, #67619, #51068 ) ;
#63804 = EDGE_LOOP ( 'NONE', ( #50092, #4176, #7403, #72675 ) ) ;
#63805 = CIRCLE ( 'NONE', #1423, 16.00000000000000000 ) ;
#63806 = ORIENTED_EDGE ( 'NONE', *, *, #7902, .F. ) ;
#63807 = CARTESIAN_POINT ( 'NONE',  ( 93.84685191531249870, -208.0026889286704943, 83.34572916753383254 ) ) ;
#63808 = DIRECTION ( 'NONE',  ( 1.000000000000000000, 0.000000000000000000, 0.000000000000000000 ) ) ;
#63809 = DIRECTION ( 'NONE',  ( 0.000000000000000000, 0.000000000000000000, 1.000000000000000000 ) ) ;
#63810 = CARTESIAN_POINT ( 'NONE',  ( -97.64999999999996305, -208.4700217866474645, 77.32645833506762756 ) ) ;
#63811 = DIRECTION ( 'NONE',  ( 0.000000000000000000, 0.000000000000000000, 1.000000000000000000 ) ) ;
#63812 = CARTESIAN_POINT ( 'NONE',  ( -94.99999999999997158, -209.9999999999999716, 90.00000000000000000 ) ) ;
#63813 = CARTESIAN_POINT ( 'NONE',  ( 92.35000000000002274, -211.5299782133524502, 86.24291666666665890 ) ) ;
#63814 = EDGE_CURVE ( 'NONE', #3856, #54680, #66028, .T. ) ;
#63815 = ORIENTED_EDGE ( 'NONE', *, *, #17168, .T. ) ;
#63816 = VERTEX_POINT ( 'NONE', #23341 ) ;
#63817 = VERTEX_POINT ( 'NONE', #16957 ) ;
#63818 = ORIENTED_EDGE ( 'NONE', *, *, #19577, .T. ) ;
#63819 = CARTESIAN_POINT ( 'NONE',  ( 0.000000000000000000, -120.0000000000000000, 102.9091629284897493 ) ) ;
#63820 = CARTESIAN_POINT ( 'NONE',  ( -92.69370383062504004, 90.00000000000004263, 86.94406250086716170 ) ) ;
#63821 = DIRECTION ( 'NONE',  ( 0.000000000000000000, -0.8660254037844363761, 0.5000000000000039968 ) ) ;
#63822 = EDGE_CURVE ( 'NONE', #70403, #4935, #61192, .T. ) ;
#63823 = CARTESIAN_POINT ( 'NONE',  ( 97.65000000000000568, -208.4700217866474645, 78.38479166840096468 ) ) ;
#63824 = CARTESIAN_POINT ( 'NONE',  ( 93.67500000000001137, -212.2949673200287179, 76.85020833506763438 ) ) ;
#63825 = CARTESIAN_POINT ( 'NONE',  ( 94.99999999999998579, 93.05995642670504253, 79.68124999999999147 ) ) ;
#63826 = EDGE_CURVE ( 'NONE', #20056, #14688, #15623, .T. ) ;
#63827 = ORIENTED_EDGE ( 'NONE', *, *, #3407, .F. ) ;
#63828 = CARTESIAN_POINT ( 'NONE',  ( -94.99999999999997158, -213.0599564267049857, 88.33312500173428816 ) ) ;
#63829 = ORIENTED_EDGE ( 'NONE', *, *, #71563, .T. ) ;
#63830 = LINE ( 'NONE', #12670, #60266 ) ;
#63831 = ORIENTED_EDGE ( 'NONE', *, *, #53495, .T. ) ;
#63832 = CARTESIAN_POINT ( 'NONE',  ( -97.65000000000001990, 90.00000000000004263, 88.80937500173430976 ) ) ;
#63833 = CARTESIAN_POINT ( 'NONE',  ( -96.15314808468752972, 91.99731107132950569, 82.71072916753381321 ) ) ;
#63834 = CARTESIAN_POINT ( 'NONE',  ( 92.69370383062498320, 91.33154071421968467, 75.61989583420047722 ) ) ;
#63835 = ORIENTED_EDGE ( 'NONE', *, *, #68531, .F. ) ;
#63836 = CARTESIAN_POINT ( 'NONE',  ( -3.000000000000002665, 0.000000000000000000, 0.000000000000000000 ) ) ;
#63837 = EDGE_CURVE ( 'NONE', #55085, #63132, #15578, .T. ) ;
#63838 = LINE ( 'NONE', #7785, #66199 ) ;
#63839 = DIRECTION ( 'NONE',  ( 0.000000000000000000, -0.5000000000000046629, 0.8660254037844359321 ) ) ;
#63840 = VECTOR ( 'NONE', #68558, 1000.000000000000000 ) ;
#63841 = CARTESIAN_POINT ( 'NONE',  ( -93.07889023459844680, 91.30563282057288177, 74.79348190356849102 ) ) ;
#63842 = EDGE_LOOP ( 'NONE', ( #68946, #50365 ) ) ;
#63843 = CARTESIAN_POINT ( 'NONE',  ( 22.75000000000000000, 0.000000000000000000, 2.055000000000000160 ) ) ;
#63844 = VECTOR ( 'NONE', #2215, 1000.000000000000000 ) ;
#63845 = CARTESIAN_POINT ( 'NONE',  ( -92.69370383062498320, -209.9999999999999716, 75.35531250086714294 ) ) ;
#63846 = ORIENTED_EDGE ( 'NONE', *, *, #28711, .F. ) ;
#63847 = AXIS2_PLACEMENT_3D ( 'NONE', #50798, #44443, #16221 ) ;
#63848 = ORIENTED_EDGE ( 'NONE', *, *, #52015, .F. ) ;
#63849 = LINE ( 'NONE', #5600, #16946 ) ;
#63850 = ORIENTED_EDGE ( 'NONE', *, *, #18163, .F. ) ;
#63851 = CARTESIAN_POINT ( 'NONE',  ( 15.00000000000000000, 14.60985201121703980, -18.46759930825707841 ) ) ;
#63852 = DIRECTION ( 'NONE',  ( 0.4279312458753000703, 0.9038112904824842087, 0.000000000000000000 ) ) ;
#63853 = ORIENTED_EDGE ( 'NONE', *, *, #28185, .F. ) ;
#63854 = CARTESIAN_POINT ( 'NONE',  ( -92.69370383062498320, -211.3315407142195852, 87.52614583420049144 ) ) ;
#63855 = VERTEX_POINT ( 'NONE', #51151 ) ;
#63857 = ADVANCED_FACE ( 'NONE', ( #39894 ), #54131, .T. ) ;
#63856 = CARTESIAN_POINT ( 'NONE',  ( -15.70000000000000284, -120.0000000000000000, -85.59999999999999432 ) ) ;
#63858 = CARTESIAN_POINT ( 'NONE',  ( 0.000000000000000000, -37.16516213103280108, 4.992566952384862589 ) ) ;
#63859 = EDGE_LOOP ( 'NONE', ( #8418, #30931, #46320, #5589 ) ) ;
#63860 = ORIENTED_EDGE ( 'NONE', *, *, #60350, .F. ) ;
#63861 = DIRECTION ( 'NONE',  ( -1.000000000000000000, -0.000000000000000000, -0.000000000000000000 ) ) ;
#63862 = AXIS2_PLACEMENT_3D ( 'NONE', #29334, #820, #34612 ) ;
#63863 = CIRCLE ( 'NONE', #61441, 16.00000000000000000 ) ;
#63864 = CARTESIAN_POINT ( 'NONE',  ( 97.65000000000000568, -208.4700217866474645, 86.00479166840096923 ) ) ;
#63865 = CARTESIAN_POINT ( 'NONE',  ( 97.30629616937498838, 88.66845928578035796, 84.19239583420048234 ) ) ;
#63866 = DIRECTION ( 'NONE',  ( 0.000000000000000000, 0.000000000000000000, 1.000000000000000000 ) ) ;
#63867 = VECTOR ( 'NONE', #569, 1000.000000000000000 ) ;
#63868 = DIRECTION ( 'NONE',  ( 0.000000000000000000, 0.000000000000000000, 1.000000000000000000 ) ) ;
#63869 = DIRECTION ( 'NONE',  ( 0.000000000000000000, 0.5224985647159441360, 0.8526401643540952868 ) ) ;
#63870 = DIRECTION ( 'NONE',  ( -0.000000000000000000, -1.000000000000000000, -1.445602896647339656E-16 ) ) ;
#63871 = DIRECTION ( 'NONE',  ( -1.000000000000000000, -0.000000000000000000, 0.000000000000000000 ) ) ;
#63872 = ADVANCED_FACE ( 'NONE', ( #53021 ), #14261, .F. ) ;
#63873 = DIRECTION ( 'NONE',  ( 1.000000000000000000, 0.000000000000000000, -0.000000000000000000 ) ) ;
#63874 = DIRECTION ( 'NONE',  ( -1.000000000000000000, 0.000000000000000000, 0.000000000000000000 ) ) ;
#63875 = EDGE_CURVE ( 'NONE', #40071, #6388, #55171, .T. ) ;
#63876 = EDGE_CURVE ( 'NONE', #66429, #31341, #14387, .T. ) ;
#63877 = CARTESIAN_POINT ( 'NONE',  ( 0.000000000000000000, 39.47590169984944453, -71.87247863392373404 ) ) ;
#63878 = DIRECTION ( 'NONE',  ( -0.000000000000000000, -0.000000000000000000, -1.000000000000000000 ) ) ;
#63879 = DIRECTION ( 'NONE',  ( 0.000000000000000000, 0.000000000000000000, -1.000000000000000000 ) ) ;
#63880 = CARTESIAN_POINT ( 'NONE',  ( 0.4301293587033142574, -121.4370068666438556, 2.500000000000000000 ) ) ;
#63881 = DIRECTION ( 'NONE',  ( -1.000000000000000000, -0.000000000000000000, -0.000000000000000000 ) ) ;
#63882 = PRODUCT_DEFINITION_SHAPE ( 'NONE', 'NONE',  #74368 ) ;
#63883 = EDGE_LOOP ( 'NONE', ( #27279, #57905, #64581, #73453 ) ) ;
#63884 = CARTESIAN_POINT ( 'NONE',  ( -92.34999999999999432, -209.9999999999999716, 90.00000000000000000 ) ) ;
#63885 = CARTESIAN_POINT ( 'NONE',  ( 5.822613034544236399, -142.8165987265839760, -5.500000000000000000 ) ) ;
#63886 = CARTESIAN_POINT ( 'NONE',  ( 94.99999999999998579, 93.05995642670504253, 77.14124999999999943 ) ) ;
#63887 = DIRECTION ( 'NONE',  ( -1.000000000000000000, -0.000000000000000000, 0.000000000000000000 ) ) ;
#63888 = CARTESIAN_POINT ( 'NONE',  ( -97.64995975554930396, 88.46999855150308179, 77.43229327564789344 ) ) ;
#63889 = DIRECTION ( 'NONE',  ( -1.000000000000000000, 0.000000000000000000, -0.000000000000000000 ) ) ;
#63890 = CARTESIAN_POINT ( 'NONE',  ( 97.30629616937498838, -208.6684592857803011, 86.99697916753382287 ) ) ;
#63891 = VECTOR ( 'NONE', #16510, 1000.000000000000000 ) ;
#63892 = EDGE_LOOP ( 'NONE', ( #73740, #60788, #73501, #31611 ) ) ;
#63893 = ORIENTED_EDGE ( 'NONE', *, *, #18587, .F. ) ;
#63894 = AXIS2_PLACEMENT_3D ( 'NONE', #43606, #26657, #27390 ) ;
#63895 = DIRECTION ( 'NONE',  ( 0.000000000000000000, 0.000000000000000000, 1.000000000000000000 ) ) ;
#63896 = ORIENTED_EDGE ( 'NONE', *, *, #73133, .F. ) ;
#63897 = DIRECTION ( 'NONE',  ( 0.000000000000000000, 0.000000000000000000, 1.000000000000000000 ) ) ;
#63898 = CIRCLE ( 'NONE', #3855, 42.00000000000000000 ) ;
#63899 = LINE ( 'NONE', #1515, #48417 ) ;
#63900 = VERTEX_POINT ( 'NONE', #8254 ) ;
#63901 = CARTESIAN_POINT ( 'NONE',  ( 95.00000000000000000, -212.6630814284392557, 78.53031250086715431 ) ) ;
#63902 = ADVANCED_FACE ( 'NONE', ( #30799 ), #65775, .T. ) ;
#63903 = VERTEX_POINT ( 'NONE', #13149 ) ;
#63904 = FACE_OUTER_BOUND ( 'NONE', #34015, .T. ) ;
#63905 = EDGE_LOOP ( 'NONE', ( #3802, #50898, #717, #32075, #64161, #66215 ) ) ;
#63906 = CIRCLE ( 'NONE', #56727, 82.00000000000000000 ) ;
#63907 = ORIENTED_EDGE ( 'NONE', *, *, #48196, .F. ) ;
#63908 = DIRECTION ( 'NONE',  ( 0.000000000000000000, 0.000000000000000000, 1.000000000000000000 ) ) ;
#63909 = DIRECTION ( 'NONE',  ( -1.000000000000000000, 0.000000000000000000, 0.000000000000000000 ) ) ;
#63910 = ADVANCED_FACE ( 'NONE', ( #30434 ), #65050, .F. ) ;
#63911 = ORIENTED_EDGE ( 'NONE', *, *, #9989, .T. ) ;
#63912 = DIRECTION ( 'NONE',  ( 0.000000000000000000, 0.000000000000000000, 1.000000000000000000 ) ) ;
#63913 = CARTESIAN_POINT ( 'NONE',  ( 92.35000000000002274, -211.5299782133524502, 86.32229166840097889 ) ) ;
#63914 = CARTESIAN_POINT ( 'NONE',  ( 94.99999999999998579, 86.94004357329500010, 88.88875000000000171 ) ) ;
#63915 = EDGE_CURVE ( 'NONE', #19352, #26439, #18421, .T. ) ;
#63916 = VERTEX_POINT ( 'NONE', #19528 ) ;
#63917 = CARTESIAN_POINT ( 'NONE',  ( 11.99999999999999822, 0.000000000000000000, 0.000000000000000000 ) ) ;
#63918 = ORIENTED_EDGE ( 'NONE', *, *, #7468, .T. ) ;
#63919 = ORIENTED_EDGE ( 'NONE', *, *, #64279, .F. ) ;
#63920 = ORIENTED_EDGE ( 'NONE', *, *, #73737, .T. ) ;
#63921 = CARTESIAN_POINT ( 'NONE',  ( 94.99999999999998579, 93.05995642670504253, 86.11062500173430578 ) ) ;
#63922 = EDGE_CURVE ( 'NONE', #70343, #5982, #30072, .T. ) ;
#63923 = VERTEX_POINT ( 'NONE', #25182 ) ;
#63924 = EDGE_LOOP ( 'NONE', ( #6504, #21078, #63552, #37271 ) ) ;
#63925 = FACE_OUTER_BOUND ( 'NONE', #7317, .T. ) ;
#63926 = CARTESIAN_POINT ( 'NONE',  ( 6.000000000000000000, -74.18225833017864090, -34.94270380257717790 ) ) ;
#63927 = VERTEX_POINT ( 'NONE', #2664 ) ;
#63928 = ORIENTED_EDGE ( 'NONE', *, *, #45483, .F. ) ;
#63929 = ORIENTED_EDGE ( 'NONE', *, *, #64585, .F. ) ;
#63930 = CARTESIAN_POINT ( 'NONE',  ( 92.35000000021533140, 90.00002100773845370, 79.91868729553033290 ) ) ;
#63931 = DIRECTION ( 'NONE',  ( -1.000000000000000000, -0.000000000000000000, -0.000000000000000000 ) ) ;
#63932 = CARTESIAN_POINT ( 'NONE',  ( -95.00000000000002842, 93.05995642670501411, 87.30124999999999602 ) ) ;
#63933 = ORIENTED_EDGE ( 'NONE', *, *, #62083, .T. ) ;
#63934 = CARTESIAN_POINT ( 'NONE',  ( 0.000000000000000000, -2.663952781846440576, 41.91543099594817789 ) ) ;
#63935 = DIRECTION ( 'NONE',  ( 0.000000000000000000, 0.000000000000000000, -1.000000000000000000 ) ) ;
#63936 = VERTEX_POINT ( 'NONE', #69921 ) ;
#63937 = LINE ( 'NONE', #17691, #70722 ) ;
#63938 = CARTESIAN_POINT ( 'NONE',  ( -94.99999999999997158, -207.3369185715606307, 83.13406250086714522 ) ) ;
#63939 = ORIENTED_EDGE ( 'NONE', *, *, #3818, .F. ) ;
#63941 = EDGE_CURVE ( 'NONE', #70819, #48459, #49160, .T. ) ;
#63940 = FACE_OUTER_BOUND ( 'NONE', #22194, .T. ) ;
#63942 = DIRECTION ( 'NONE',  ( 0.000000000000000000, 0.000000000000000000, -1.000000000000000000 ) ) ;
#63943 = DIRECTION ( 'NONE',  ( -1.000000000000000000, 0.000000000000000000, -0.000000000000000000 ) ) ;
#63944 = CARTESIAN_POINT ( 'NONE',  ( -96.15314808468747287, -208.0026889286704943, 75.56697916753381605 ) ) ;
#63945 = MECHANICAL_DESIGN_GEOMETRIC_PRESENTATION_REPRESENTATION (  '', ( #62718 ), #44730 ) ;
#63946 = CARTESIAN_POINT ( 'NONE',  ( 10.00000000000000000, 0.000000000000000000, 0.000000000000000000 ) ) ;
#63947 = DIRECTION ( 'NONE',  ( -1.000000000000000000, 0.000000000000000000, 0.000000000000000000 ) ) ;
#63948 = CIRCLE ( 'NONE', #36287, 32.00000000000000000 ) ;
#63949 = DIRECTION ( 'NONE',  ( -0.000000000000000000, 0.9781476007338066880, -0.2079116908177543743 ) ) ;
#63950 = CARTESIAN_POINT ( 'NONE',  ( 2.500000000000034639, 90.00000000000000000, -310.0000000000000000 ) ) ;
#63951 = DIRECTION ( 'NONE',  ( 0.000000000000000000, 0.5877852522924685852, 0.8090169943749508930 ) ) ;
#63952 = DIRECTION ( 'NONE',  ( -1.000000000000000000, -0.000000000000000000, -0.000000000000000000 ) ) ;
#63953 = ADVANCED_FACE ( 'NONE', ( #1921 ), #3023, .T. ) ;
#63954 = CARTESIAN_POINT ( 'NONE',  ( -97.30629616937501680, 91.33154071421968467, 80.06489583420047040 ) ) ;
#63955 = DIRECTION ( 'NONE',  ( 0.000000000000000000, -0.1564344650402380854, 0.9876883405951365491 ) ) ;
#63956 = CARTESIAN_POINT ( 'NONE',  ( 10.00000000000000000, -30.80686688397025108, 21.53537804866070715 ) ) ;
#63957 = EDGE_CURVE ( 'NONE', #52806, #58070, #7929, .T. ) ;
#63958 = CIRCLE ( 'NONE', #12306, 82.00000000000000000 ) ;
#63959 =( BOUNDED_CURVE ( )  B_SPLINE_CURVE ( 2, ( #63930, #40246, #23692, #46626, #33859, #57545, #69556 ),
 .UNSPECIFIED., .F., .F. ) 
 B_SPLINE_CURVE_WITH_KNOTS ( ( 3, 2, 2, 3 ),
 ( 0.6350190250571090544, 0.6420746642202955767, 0.6491304297611778518, 0.6561861948910822084 ),
 .UNSPECIFIED. ) 
 CURVE ( )  GEOMETRIC_REPRESENTATION_ITEM ( )  RATIONAL_B_SPLINE_CURVE ( ( 0.9999952007766099715, 0.8660278034391145630, 1.000000000000000000, 0.8660254037844387076, 1.000000000000000000, 0.8660254037844387076, 1.000000000000000000 ) ) 
 REPRESENTATION_ITEM ( '' )  );
#63960 = ORIENTED_EDGE ( 'NONE', *, *, #33189, .T. ) ;
#63961 = CARTESIAN_POINT ( 'NONE',  ( 15.00000000000000000, 6.762365576493647445, 25.66652317338391498 ) ) ;
#63962 = AXIS2_PLACEMENT_3D ( 'NONE', #43612, #72879, #3763 ) ;
#63963 = DIRECTION ( 'NONE',  ( -0.000000000000000000, -0.000000000000000000, 1.000000000000000000 ) ) ;
#63964 = DIRECTION ( 'NONE',  ( -1.000000000000000000, -0.000000000000000000, 0.000000000000000000 ) ) ;
#63965 = AXIS2_PLACEMENT_3D ( 'NONE', #46279, #68851, #12427 ) ;
#63966 = CARTESIAN_POINT ( 'NONE',  ( 11.99999999999999822, 0.000000000000000000, 0.000000000000000000 ) ) ;
#63967 = DIRECTION ( 'NONE',  ( -0.000000000000000000, -0.6691306063588671194, 0.7431448254773862505 ) ) ;
#63968 = CARTESIAN_POINT ( 'NONE',  ( -97.64999999969894873, 90.00002455906438570, 87.53856274002211535 ) ) ;
#63969 = CARTESIAN_POINT ( 'NONE',  ( -96.15314808468745866, -211.9973110713294489, 75.93739583420048689 ) ) ;
#63970 = CARTESIAN_POINT ( 'NONE',  ( -95.00000000000002842, 90.00000000000004263, 90.00000000000000000 ) ) ;
#63971 = ORIENTED_EDGE ( 'NONE', *, *, #56204, .F. ) ;
#63972 = CARTESIAN_POINT ( 'NONE',  ( -22.67106064244953245, -113.6342314410295842, 5.500000000000000000 ) ) ;
#63973 = DIRECTION ( 'NONE',  ( 0.000000000000000000, -1.000000000000000000, -1.047444401652940007E-14 ) ) ;
#63974 = LINE ( 'NONE', #57219, #44948 ) ;
#63975 = DIRECTION ( 'NONE',  ( -1.000000000000000000, 0.000000000000000000, 0.000000000000000000 ) ) ;
#63976 = ORIENTED_EDGE ( 'NONE', *, *, #12230, .F. ) ;
#63977 = CARTESIAN_POINT ( 'NONE',  ( 0.000000000000000000, 0.000000000000000000, -270.0000000000000000 ) ) ;
#63978 = DIRECTION ( 'NONE',  ( 0.000000000000000000, 0.9723699203976773342, -0.2334453638559026156 ) ) ;
#63979 = ORIENTED_EDGE ( 'NONE', *, *, #66083, .F. ) ;
#63980 = ADVANCED_FACE ( 'NONE', ( #47011 ), #12777, .F. ) ;
#63981 = CARTESIAN_POINT ( 'NONE',  ( 97.30629616937498838, -211.3315407142195852, 84.82739583420048746 ) ) ;
#63982 = CARTESIAN_POINT ( 'NONE',  ( -95.00000000000002842, 93.05995642670504253, 82.30062500173427509 ) ) ;
#63983 = VERTEX_POINT ( 'NONE', #1553 ) ;
#63984 = ADVANCED_FACE ( 'NONE', ( #24439 ), #42113, .F. ) ;
#63985 = CARTESIAN_POINT ( 'NONE',  ( 11.41210121379327980, -99.40233154247455616, -2.500000000000000000 ) ) ;
#63986 = STYLED_ITEM ( 'NONE', ( #60035 ), #51651 ) ;
#63987 = ORIENTED_EDGE ( 'NONE', *, *, #34047, .T. ) ;
#63988 = FACE_OUTER_BOUND ( 'NONE', #48997, .T. ) ;
#63989 = EDGE_LOOP ( 'NONE', ( #38489, #21354, #39202, #59370 ) ) ;
#63990 = CARTESIAN_POINT ( 'NONE',  ( -96.15314808468752972, 91.99731107132950569, 81.44072916753381719 ) ) ;
#63991 = ADVANCED_FACE ( 'NONE', ( #43600 ), #66519, .F. ) ;
#63992 = AXIS2_PLACEMENT_3D ( 'NONE', #35487, #35847, #951 ) ;
#63993 = EDGE_LOOP ( 'NONE', ( #28864, #4361, #49193, #20604 ) ) ;
#63994 = EDGE_LOOP ( 'NONE', ( #60853, #67007, #35899, #6560 ) ) ;
#63995 = DIRECTION ( 'NONE',  ( 0.000000000000000000, 0.000000000000000000, 1.000000000000000000 ) ) ;
#63996 = EDGE_CURVE ( 'NONE', #33546, #68607, #32354, .T. ) ;
#63997 = ORIENTED_EDGE ( 'NONE', *, *, #48054, .F. ) ;
#63998 = CARTESIAN_POINT ( 'NONE',  ( 10.00000000000000000, 20.41045688087824317, 72.35160999960824313 ) ) ;
#63999 = CARTESIAN_POINT ( 'NONE',  ( 0.000000000000000000, 0.000000000000000000, 0.000000000000000000 ) ) ;
#64000 = VERTEX_POINT ( 'NONE', #72140 ) ;
#64001 = CARTESIAN_POINT ( 'NONE',  ( -11.68233973192911535, 0.000000000000000000, 0.000000000000000000 ) ) ;
#64002 = CIRCLE ( 'NONE', #55558, 22.90000000000041780 ) ;
#64003 = EDGE_LOOP ( 'NONE', ( #1743, #29357, #42273, #16536 ) ) ;
#64004 = CARTESIAN_POINT ( 'NONE',  ( 11.99999999999999822, -54.21277698773636899, -55.38113227695839669 ) ) ;
#64005 = ORIENTED_EDGE ( 'NONE', *, *, #23352, .T. ) ;
#64006 = EDGE_CURVE ( 'NONE', #36499, #44699, #11977, .T. ) ;
#64007 = ORIENTED_EDGE ( 'NONE', *, *, #37335, .F. ) ;
#64008 = CIRCLE ( 'NONE', #73587, 77.49899999999999523 ) ;
#64009 = VERTEX_POINT ( 'NONE', #28413 ) ;
#64010 = CARTESIAN_POINT ( 'NONE',  ( 97.30629616937498838, -211.3315407142195852, 81.01739583420048518 ) ) ;
#64011 = CIRCLE ( 'NONE', #56826, 37.49900000000000944 ) ;
#64012 = APPLICATION_PROTOCOL_DEFINITION ( 'draft international standard', 'automotive_design', 1998, #33027 ) ;
#64013 = DIRECTION ( 'NONE',  ( 0.000000000000000000, 0.000000000000000000, -1.000000000000000000 ) ) ;
#64014 = CARTESIAN_POINT ( 'NONE',  ( -94.26002770235174921, -212.5681771730648109, 75.00000000000000000 ) ) ;
#64015 = DIRECTION ( 'NONE',  ( 0.000000000000000000, 0.000000000000000000, 1.000000000000000000 ) ) ;
#64016 = CARTESIAN_POINT ( 'NONE',  ( 11.99999999999999822, -34.94270380257585629, -74.18225833017926618 ) ) ;
#64017 = CARTESIAN_POINT ( 'NONE',  ( -92.35000000000003695, 90.00000000000004263, 79.52249999999999375 ) ) ;
#64018 = LINE ( 'NONE', #1275, #44343 ) ;
#64019 = CARTESIAN_POINT ( 'NONE',  ( -93.84685191531248449, -208.0026889286704943, 85.62114583420046188 ) ) ;
#64020 = CARTESIAN_POINT ( 'NONE',  ( -92.69370383062502583, 88.66845928578038638, 82.44614583420049314 ) ) ;
#64021 = EDGE_LOOP ( 'NONE', ( #33386, #14337, #31972, #4381 ) ) ;
#64022 = ADVANCED_FACE ( 'NONE', ( #72506 ), #16782, .F. ) ;
#64023 = CARTESIAN_POINT ( 'NONE',  ( 96.15314808468748708, 88.00268892867053694, 84.77447916753381207 ) ) ;
#64024 = VERTEX_POINT ( 'NONE', #61252 ) ;
#64025 = CARTESIAN_POINT ( 'NONE',  ( 12.00000000000000000, 24.81905959214275370, 9.408202855044498492 ) ) ;
#64026 = DIRECTION ( 'NONE',  ( -0.000000000000000000, -0.000000000000000000, 1.000000000000000000 ) ) ;
#64028 = ADVANCED_FACE ( 'NONE', ( #14998 ), #32283, .T. ) ;
#64027 = FACE_OUTER_BOUND ( 'NONE', #37893, .T. ) ;
#64029 = CARTESIAN_POINT ( 'NONE',  ( 10.00000000000000000, -37.22597642581153821, 10.79786254984320415 ) ) ;
#64030 = DIRECTION ( 'NONE',  ( 1.000000000000000000, 0.000000000000000000, -0.000000000000000000 ) ) ;
#64031 = CARTESIAN_POINT ( 'NONE',  ( -93.84685191531248449, -208.0026889286704943, 84.98614583420047097 ) ) ;
#64032 = DIRECTION ( 'NONE',  ( 0.000000000000000000, 0.000000000000000000, -1.000000000000000000 ) ) ;
#64033 = DIRECTION ( 'NONE',  ( 0.000000000000000000, 0.3090169943749480619, -0.9510565162951533091 ) ) ;
#64034 = DIRECTION ( 'NONE',  ( 0.000000000000000000, -0.9723699203976741146, -0.2334453638559158550 ) ) ;
#64035 = ADVANCED_FACE ( 'NONE', ( #26277 ), #39719, .T. ) ;
#64036 = FACE_OUTER_BOUND ( 'NONE', #55382, .T. ) ;
#64037 = ORIENTED_EDGE ( 'NONE', *, *, #5001, .T. ) ;
#64038 = VERTEX_POINT ( 'NONE', #9360 ) ;
#64039 = CARTESIAN_POINT ( 'NONE',  ( -92.35000000000005116, 88.47002178664754979, 77.56458333333333144 ) ) ;
#64040 = CARTESIAN_POINT ( 'NONE',  ( 95.00000000000000000, -213.0599564267049857, 88.88875000000000171 ) ) ;
#64041 = ADVANCED_FACE ( 'NONE', ( #25915 ), #57009, .T. ) ;
#64042 = CARTESIAN_POINT ( 'NONE',  ( -92.69370383062502583, 88.66845928578038638, 89.27239583420048064 ) ) ;
#64043 = CARTESIAN_POINT ( 'NONE',  ( -21.67772167707813935, -110.8034581014852762, 5.500000000000000000 ) ) ;
#64044 = DIRECTION ( 'NONE',  ( -1.000000000000000000, -0.000000000000000000, -0.000000000000000000 ) ) ;
#64045 = AXIS2_PLACEMENT_3D ( 'NONE', #20583, #67556, #66449 ) ;
#64046 = DIRECTION ( 'NONE',  ( 1.000000000000000000, -7.571541139944063212E-15, -2.603472992745718826E-14 ) ) ;
#64047 = DIRECTION ( 'NONE',  ( -1.000000000000000000, -0.000000000000000000, -0.000000000000000000 ) ) ;
#64048 = ORIENTED_EDGE ( 'NONE', *, *, #59330, .F. ) ;
#64049 = PLANE ( 'NONE',  #58438 ) ;
#64050 = EDGE_CURVE ( 'NONE', #45116, #27941, #61741, .T. ) ;
#64051 = AXIS2_PLACEMENT_3D ( 'NONE', #58823, #64463, #29859 ) ;
#64052 = DIRECTION ( 'NONE',  ( 0.000000000000000000, 0.000000000000000000, -1.000000000000000000 ) ) ;
#64053 = DIRECTION ( 'NONE',  ( 0.000000000000000000, 0.000000000000000000, 1.000000000000000000 ) ) ;
#64054 = AXIS2_PLACEMENT_3D ( 'NONE', #26051, #15511, #14770 ) ;
#64055 = CARTESIAN_POINT ( 'NONE',  ( 0.000000000000000000, -0.6853352020787742971, -37.58145647212455032 ) ) ;
#64056 = DIRECTION ( 'NONE',  ( -0.000000000000000000, -0.000000000000000000, 1.000000000000000000 ) ) ;
#64057 = LINE ( 'NONE', #12531, #53319 ) ;
#64058 = CARTESIAN_POINT ( 'NONE',  ( -93.84685191531247028, -211.9973110713294489, 86.83822916753382515 ) ) ;
#64059 = FACE_OUTER_BOUND ( 'NONE', #11134, .T. ) ;
#64060 = VECTOR ( 'NONE', #54001, 1000.000000000000000 ) ;
#64061 = VECTOR ( 'NONE', #62693, 1000.000000000000000 ) ;
#64062 = CARTESIAN_POINT ( 'NONE',  ( 92.69370383062498320, 90.00000000000002842, 77.73656250086715147 ) ) ;
#64063 = CARTESIAN_POINT ( 'NONE',  ( -96.15314808468747287, -208.0026889286704943, 75.72572916753382799 ) ) ;
#64064 = DIRECTION ( 'NONE',  ( 0.000000000000000000, -0.3090169943749548342, 0.9510565162951510887 ) ) ;
#64065 = ORIENTED_EDGE ( 'NONE', *, *, #39730, .T. ) ;
#64066 = LINE ( 'NONE', #17812, #12460 ) ;
#64067 = DIRECTION ( 'NONE',  ( 0.000000000000000000, 0.9969173337331276308, 0.07845909572784873220 ) ) ;
#64068 = DIRECTION ( 'NONE',  ( -1.000000000000000000, 0.000000000000000000, 0.000000000000000000 ) ) ;
#64069 = AXIS2_PLACEMENT_3D ( 'NONE', #73178, #21679, #12252 ) ;
#64070 = VECTOR ( 'NONE', #71414, 999.9999999999998863 ) ;
#64071 = AXIS2_PLACEMENT_3D ( 'NONE', #43707, #49326, #50801 ) ;
#64072 = DIRECTION ( 'NONE',  ( 0.000000000000000000, 0.000000000000000000, -1.000000000000000000 ) ) ;
#64073 = CARTESIAN_POINT ( 'NONE',  ( 95.00000000000000000, -207.3369185715606307, 76.78406250086712248 ) ) ;
#64074 = ORIENTED_EDGE ( 'NONE', *, *, #24556, .T. ) ;
#64075 = CARTESIAN_POINT ( 'NONE',  ( 0.000000000000000000, 67.80270845531956070, -46.11716303203112943 ) ) ;
#64076 = ORIENTED_EDGE ( 'NONE', *, *, #67118, .F. ) ;
#64077 = CARTESIAN_POINT ( 'NONE',  ( 10.00000000000000000, -33.71516098798792171, 74.74816331893418919 ) ) ;
#64078 = EDGE_LOOP ( 'NONE', ( #41623, #55593, #36979, #49732 ) ) ;
#64079 = AXIS2_PLACEMENT_3D ( 'NONE', #1270, #34683, #58354 ) ;
#64080 = ADVANCED_FACE ( 'NONE', ( #5142 ), #28044, .F. ) ;
#64081 = CARTESIAN_POINT ( 'NONE',  ( 0.000000000000000000, 16.65972982744934683, 80.28980883073764119 ) ) ;
#64082 = EDGE_CURVE ( 'NONE', #39726, #30760, #31182, .T. ) ;
#64083 = EDGE_LOOP ( 'NONE', ( #63482, #21337 ) ) ;
#64084 = ORIENTED_EDGE ( 'NONE', *, *, #7974, .F. ) ;
#64086 = ORIENTED_EDGE ( 'NONE', *, *, #61458, .T. ) ;
#64085 = EDGE_CURVE ( 'NONE', #6463, #34044, #22784, .T. ) ;
#64087 = EDGE_CURVE ( 'NONE', #6766, #71207, #52769, .T. ) ;
#64088 = CARTESIAN_POINT ( 'NONE',  ( 97.64999999999996305, -211.0554082285335937, 75.04099707143595310 ) ) ;
#64089 = EDGE_LOOP ( 'NONE', ( #32831, #54460, #44179, #57128 ) ) ;
#64090 = VECTOR ( 'NONE', #72706, 1000.000000000000000 ) ;
#64091 = VERTEX_POINT ( 'NONE', #64909 ) ;
#64092 = CARTESIAN_POINT ( 'NONE',  ( 97.30629616937498838, 88.66845928578037217, 82.44614583420049314 ) ) ;
#64093 = DIRECTION ( 'NONE',  ( 0.000000000000000000, 0.000000000000000000, 1.000000000000000000 ) ) ;
#64094 = CARTESIAN_POINT ( 'NONE',  ( 92.35000000000002274, -208.4700217866474645, 75.34208333333333485 ) ) ;
#64095 = VERTEX_POINT ( 'NONE', #47602 ) ;
#64096 = ORIENTED_EDGE ( 'NONE', *, *, #23013, .T. ) ;
#64097 = ORIENTED_EDGE ( 'NONE', *, *, #69679, .T. ) ;
#64098 = ORIENTED_EDGE ( 'NONE', *, *, #33594, .T. ) ;
#64099 = DIRECTION ( 'NONE',  ( 0.000000000000000000, 0.8910065241883656784, 0.4539904997395511899 ) ) ;
#64100 = CYLINDRICAL_SURFACE ( 'NONE', #73530, 82.00000000000000000 ) ;
#64101 = EDGE_CURVE ( 'NONE', #56010, #18520, #50086, .T. ) ;
#64102 = CYLINDRICAL_SURFACE ( 'NONE', #44691, 16.00000000000000355 ) ;
#64103 = CARTESIAN_POINT ( 'NONE',  ( 92.35000000000000853, -211.5299782133524218, 82.51229166840094820 ) ) ;
#64104 = CARTESIAN_POINT ( 'NONE',  ( -94.99999999999997158, -209.9999999999999716, 90.00000000000000000 ) ) ;
#64105 = ADVANCED_FACE ( 'NONE', ( #37067 ), #2886, .F. ) ;
#64106 = CARTESIAN_POINT ( 'NONE',  ( 92.35000000000005116, 91.52997821335254969, 77.88208333333332689 ) ) ;
#64107 = CARTESIAN_POINT ( 'NONE',  ( -97.64999999999994884, -211.5299782133524502, 79.97229166840095615 ) ) ;
#64108 = ORIENTED_EDGE ( 'NONE', *, *, #47430, .T. ) ;
#64109 = LINE ( 'NONE', #13327, #300 ) ;
#64110 = VERTEX_POINT ( 'NONE', #27151 ) ;
#64112 = CARTESIAN_POINT ( 'NONE',  ( -96.32500000000001705, 87.70503267997129626, 76.85020833506763438 ) ) ;
#64111 = CARTESIAN_POINT ( 'NONE',  ( 96.32499999999997442, 92.29496732002878900, 79.70770833506762187 ) ) ;
#64113 = VECTOR ( 'NONE', #59090, 1000.000000000000000 ) ;
#64114 = ORIENTED_EDGE ( 'NONE', *, *, #6151, .T. ) ;
#64115 = CARTESIAN_POINT ( 'NONE',  ( 94.99999999999998579, 92.66308142843935514, 79.48281250086715488 ) ) ;
#64116 = VECTOR ( 'NONE', #46393, 1000.000000000000000 ) ;
#64117 = CARTESIAN_POINT ( 'NONE',  ( 11.99999999999999822, -56.15606465355001120, 59.75363087400055662 ) ) ;
#64118 = DIRECTION ( 'NONE',  ( 0.000000000000000000, 0.000000000000000000, -1.000000000000000000 ) ) ;
#64119 = CARTESIAN_POINT ( 'NONE',  ( 92.35000000000000853, -211.5299782133524218, 79.33729166840096525 ) ) ;
#64120 = CARTESIAN_POINT ( 'NONE',  ( -89.99999999999992895, -116.0000000000000000, -40.00000000000002132 ) ) ;
#64121 = VERTEX_POINT ( 'NONE', #19762 ) ;
#64123 = CARTESIAN_POINT ( 'NONE',  ( 11.99999999999999822, 0.000000000000000000, 0.000000000000000000 ) ) ;
#64122 = CIRCLE ( 'NONE', #73693, 14.09999999999999964 ) ;
#64124 = ADVANCED_FACE ( 'NONE', ( #60016 ), #8116, .T. ) ;
#64126 = ADVANCED_FACE ( 'NONE', ( #20131 ), #31042, .F. ) ;
#64125 = CIRCLE ( 'NONE', #5312, 37.49900000000000944 ) ;
#64127 = DIRECTION ( 'NONE',  ( 0.000000000000000000, 0.000000000000000000, 1.000000000000000000 ) ) ;
#64128 = VERTEX_POINT ( 'NONE', #8501 ) ;
#64129 = ORIENTED_EDGE ( 'NONE', *, *, #36307, .T. ) ;
#64130 = B_SPLINE_CURVE_WITH_KNOTS ( 'NONE', 3,
 ( #20508, #38160, #56199, #20122, #49803, #44178, #14861, #66017 ),
 .UNSPECIFIED., .F., .F.,
 ( 4, 2, 2, 4 ),
 ( 0.001653806717455073069, 0.002539064216007527134, 0.002981692965283746360, 0.003424321714559965153 ),
 .UNSPECIFIED. ) ;
#64131 = LINE ( 'NONE', #73627, #41764 ) ;
#64132 = DIRECTION ( 'NONE',  ( -1.000000000000000000, 0.000000000000000000, -0.000000000000000000 ) ) ;
#64133 = CARTESIAN_POINT ( 'NONE',  ( -96.32499999999996021, -207.7050326799711968, 75.92416666666666458 ) ) ;
#64134 = CARTESIAN_POINT ( 'NONE',  ( -94.99999999999997158, -207.3369185715606307, 76.30781250086715772 ) ) ;
#64135 = ORIENTED_EDGE ( 'NONE', *, *, #64085, .F. ) ;
#64136 = CIRCLE ( 'NONE', #66543, 42.00000000000000000 ) ;
#64137 = DIRECTION ( 'NONE',  ( 0.000000000000000000, 0.8526401643540936215, -0.5224985647159469115 ) ) ;
#64138 = CARTESIAN_POINT ( 'NONE',  ( -97.40333747838421630, -210.8453944377615414, 74.93511027845802630 ) ) ;
#64139 = CARTESIAN_POINT ( 'NONE',  ( -3.000000000000000000, 16.83928648764923253, 16.46020748918050458 ) ) ;
#64140 = LINE ( 'NONE', #29526, #30813 ) ;
#64141 = CARTESIAN_POINT ( 'NONE',  ( 10.00000000000000000, 56.15606465354958488, 59.75363087400094031 ) ) ;
#64142 = CARTESIAN_POINT ( 'NONE',  ( -23.30023580412278505, -123.4057321492263384, -5.500000000000000000 ) ) ;
#64143 = DIRECTION ( 'NONE',  ( -1.000000000000000000, 0.000000000000000000, 0.000000000000000000 ) ) ;
#64144 = DIRECTION ( 'NONE',  ( 0.000000000000000000, 0.000000000000000000, 1.000000000000000000 ) ) ;
#64145 = CARTESIAN_POINT ( 'NONE',  ( -93.67499999999998295, -212.2949673200287179, 76.24166666666666003 ) ) ;
#64146 = DIRECTION ( 'NONE',  ( -0.000000000000000000, -0.000000000000000000, 1.000000000000000000 ) ) ;
#64147 = AXIS2_PLACEMENT_3D ( 'NONE', #61535, #3300, #25463 ) ;
#64148 = CARTESIAN_POINT ( 'NONE',  ( 97.30629616937498838, 90.00000000000002842, 86.30906250086715659 ) ) ;
#64149 = CARTESIAN_POINT ( 'NONE',  ( -97.30629616937495996, -209.9999999999999716, 85.35656250086715602 ) ) ;
#64150 = DIRECTION ( 'NONE',  ( 0.000000000000000000, 1.000000000000000000, 3.469446951953615767E-15 ) ) ;
#64151 = ORIENTED_EDGE ( 'NONE', *, *, #37454, .F. ) ;
#64152 = CARTESIAN_POINT ( 'NONE',  ( 10.00000000000000000, -22.48208911017525580, 35.47612816024516036 ) ) ;
#64153 = CARTESIAN_POINT ( 'NONE',  ( -94.99999999999997158, -206.9400435732949575, 81.58624999999999261 ) ) ;
#64154 = CARTESIAN_POINT ( 'NONE',  ( -96.15314808468752972, 91.99731107132950569, 76.20197916753380696 ) ) ;
#64155 = VECTOR ( 'NONE', #62815, 1000.000000000000000 ) ;
#64156 = CARTESIAN_POINT ( 'NONE',  ( 92.69370383062501162, -211.3315407142195852, 88.42572916753380241 ) ) ;
#64157 = ORIENTED_EDGE ( 'NONE', *, *, #71173, .F. ) ;
#64158 = EDGE_LOOP ( 'NONE', ( #22491, #44435, #56415, #31253 ) ) ;
#64159 = VECTOR ( 'NONE', #4090, 1000.000000000000114 ) ;
#64160 = VECTOR ( 'NONE', #65817, 1000.000000000000000 ) ;
#64161 = ORIENTED_EDGE ( 'NONE', *, *, #35580, .T. ) ;
#64162 = ADVANCED_BREP_SHAPE_REPRESENTATION ( '', ( #12416, #43395 ), #45865 ) ;
#64163 = ADVANCED_FACE ( 'NONE', ( #54361 ), #53998, .T. ) ;
#64164 = CIRCLE ( 'NONE', #24387, 16.00000000000000000 ) ;
#64165 = CARTESIAN_POINT ( 'NONE',  ( 15.00000000000000000, 20.85821328998741109, -10.92862929874522671 ) ) ;
#64166 = DIRECTION ( 'NONE',  ( -1.000000000000000000, 0.000000000000000000, 0.000000000000000000 ) ) ;
#64167 = EDGE_CURVE ( 'NONE', #46710, #23851, #9878, .T. ) ;
#64168 = ORIENTED_EDGE ( 'NONE', *, *, #11949, .F. ) ;
#64169 = ORIENTED_EDGE ( 'NONE', *, *, #43828, .F. ) ;
#64170 = CIRCLE ( 'NONE', #55628, 31.99999999999998579 ) ;
#64171 = EDGE_CURVE ( 'NONE', #59929, #19226, #25781, .T. ) ;
#64172 = CARTESIAN_POINT ( 'NONE',  ( 93.84685191531249870, -208.0026889286704943, 80.17072916753382117 ) ) ;
#64173 = LINE ( 'NONE', #69793, #57257 ) ;
#64175 = FACE_OUTER_BOUND ( 'NONE', #14343, .T. ) ;
#64174 = VECTOR ( 'NONE', #25866, 1000.000000000000114 ) ;
#64176 = CARTESIAN_POINT ( 'NONE',  ( 92.34999999999999432, 90.00000000000002842, 83.01499999999998636 ) ) ;
#64177 =( BOUNDED_CURVE ( )  B_SPLINE_CURVE ( 2, ( #12922, #46414, #40786, #68979, #63345, #30222, #35857 ),
 .UNSPECIFIED., .F., .F. ) 
 B_SPLINE_CURVE_WITH_KNOTS ( ( 3, 2, 2, 3 ),
 ( 0.8125000000000002220, 0.8194444444444446418, 0.8263888888888889506, 0.8333333333333334814 ),
 .UNSPECIFIED. ) 
 CURVE ( )  GEOMETRIC_REPRESENTATION_ITEM ( )  RATIONAL_B_SPLINE_CURVE ( ( 0.9999999999999956701, 0.8660254037844430375, 1.000000000000000000, 0.8660254037844387076, 1.000000000000000000, 0.8660254037844365982, 1.000000000000002220 ) ) 
 REPRESENTATION_ITEM ( '' )  );
#64178 = CYLINDRICAL_SURFACE ( 'NONE', #15910, 31.99999999999999289 ) ;
#64179 = EDGE_CURVE ( 'NONE', #27633, #17145, #25042, .T. ) ;
#64180 = CARTESIAN_POINT ( 'NONE',  ( 10.00000000000000000, -27.74655509720723501, 77.16300072079651784 ) ) ;
#64181 = CARTESIAN_POINT ( 'NONE',  ( 93.67500000000001137, -212.2949673200287179, 85.66083333333332916 ) ) ;
#64182 = CIRCLE ( 'NONE', #42600, 16.00000000000000000 ) ;
#64183 = EDGE_LOOP ( 'NONE', ( #18551, #61168, #22336, #48090 ) ) ;
#64184 = VERTEX_POINT ( 'NONE', #14117 ) ;
#64185 = EDGE_LOOP ( 'NONE', ( #45360, #72916, #56257, #63528 ) ) ;
#64186 = VERTEX_POINT ( 'NONE', #47982 ) ;
#64187 = CARTESIAN_POINT ( 'NONE',  ( 0.000000000000000000, -0.8299999999999999600, -1.199999999999999956 ) ) ;
#64188 = CARTESIAN_POINT ( 'NONE',  ( -97.30629616937501680, 91.33154071421968467, 85.93864583420048575 ) ) ;
#64189 = LINE ( 'NONE', #17944, #23373 ) ;
#64190 = DIRECTION ( 'NONE',  ( -0.000000000000000000, -0.000000000000000000, 1.000000000000000000 ) ) ;
#64191 = CARTESIAN_POINT ( 'NONE',  ( 96.15314808468748708, -208.0026889286704943, 88.79614583420047325 ) ) ;
#64192 = CARTESIAN_POINT ( 'NONE',  ( 96.32499999999997442, 92.29496732002878900, 79.62833333333333030 ) ) ;
#64193 = EDGE_CURVE ( 'NONE', #17740, #40404, #25232, .T. ) ;
#64194 = ORIENTED_EDGE ( 'NONE', *, *, #15952, .T. ) ;
#64195 = CARTESIAN_POINT ( 'NONE',  ( -96.32499999999996021, -212.2949673200287179, 88.28020833506764120 ) ) ;
#64196 = EDGE_LOOP ( 'NONE', ( #54308, #60149, #62730, #61887 ) ) ;
#64197 = EDGE_CURVE ( 'NONE', #22572, #50206, #35947, .T. ) ;
#64198 = CARTESIAN_POINT ( 'NONE',  ( 10.00000000000000000, 73.72996012237440766, 14.67089635893739619 ) ) ;
#64199 = ORIENTED_EDGE ( 'NONE', *, *, #7385, .F. ) ;
#64200 = CARTESIAN_POINT ( 'NONE',  ( 10.00000000000000000, -35.92658777277502935, -10.74501242461320594 ) ) ;
#64201 = CARTESIAN_POINT ( 'NONE',  ( 97.30629616937498838, 88.66845928578037217, 89.43114583420049257 ) ) ;
#64202 = ORIENTED_EDGE ( 'NONE', *, *, #23134, .T. ) ;
#64203 = DIRECTION ( 'NONE',  ( 0.000000000000000000, 0.5877852522924742473, -0.8090169943749466741 ) ) ;
#64204 = CARTESIAN_POINT ( 'NONE',  ( 10.00000000000000000, 2.663952781846149254, 41.91543099594818500 ) ) ;
#64205 = FACE_OUTER_BOUND ( 'NONE', #16551, .T. ) ;
#64206 = DIRECTION ( 'NONE',  ( 1.000000000000000000, 0.000000000000000000, 0.000000000000000000 ) ) ;
#64207 = ORIENTED_EDGE ( 'NONE', *, *, #15248, .F. ) ;
#64208 = CARTESIAN_POINT ( 'NONE',  ( 12.00000000000000000, 23.59884966291538078, 12.14883922797231008 ) ) ;
#64209 = EDGE_CURVE ( 'NONE', #23556, #64095, #58898, .T. ) ;
#64210 = ADVANCED_FACE ( 'NONE', ( #15520 ), #38458, .T. ) ;
#64211 = CARTESIAN_POINT ( 'NONE',  ( -97.64998530214684536, 91.52998669916203767, 81.77145774807789280 ) ) ;
#64212 = CIRCLE ( 'NONE', #62987, 31.99999999999999289 ) ;
#64213 = ORIENTED_EDGE ( 'NONE', *, *, #62860, .T. ) ;
#64214 = ORIENTED_EDGE ( 'NONE', *, *, #40858, .T. ) ;
#64215 = CARTESIAN_POINT ( 'NONE',  ( 97.64999999999999147, -210.0000000255706709, 84.04687500080852658 ) ) ;
#64216 = DIRECTION ( 'NONE',  ( -1.000000000000000000, -0.000000000000000000, -0.000000000000000000 ) ) ;
#64217 = DIRECTION ( 'NONE',  ( 1.000000000000000000, -7.571537405616606460E-15, -2.598394312951952234E-14 ) ) ;
#64218 = ORIENTED_EDGE ( 'NONE', *, *, #10256, .F. ) ;
#64219 = CARTESIAN_POINT ( 'NONE',  ( -96.15314808468747287, -208.0026889286704943, 87.15572916753382060 ) ) ;
#64220 = EDGE_LOOP ( 'NONE', ( #49909, #47930 ) ) ;
#64221 = AXIS2_PLACEMENT_3D ( 'NONE', #44743, #26683, #44362 ) ;
#64222 = DIRECTION ( 'NONE',  ( -1.000000000000000000, 0.000000000000000000, -0.000000000000000000 ) ) ;
#64223 = CIRCLE ( 'NONE', #11396, 37.49900000000001654 ) ;
#64224 = ORIENTED_EDGE ( 'NONE', *, *, #54508, .F. ) ;
#64225 = ORIENTED_EDGE ( 'NONE', *, *, #14323, .T. ) ;
#64226 = LINE ( 'NONE', #11586, #65625 ) ;
#64227 = AXIS2_PLACEMENT_3D ( 'NONE', #55727, #16995, #22261 ) ;
#64228 = DIRECTION ( 'NONE',  ( 0.000000000000000000, 0.000000000000000000, 1.000000000000000000 ) ) ;
#64229 = CARTESIAN_POINT ( 'NONE',  ( 94.99999999999998579, 92.66308142843932671, 80.59406250086715318 ) ) ;
#64230 = CARTESIAN_POINT ( 'NONE',  ( 15.00000000000000000, 8.688484142254226938, 21.88630264137359305 ) ) ;
#64231 = FACE_OUTER_BOUND ( 'NONE', #68553, .T. ) ;
#64232 = FACE_OUTER_BOUND ( 'NONE', #51301, .T. ) ;
#64233 = DIRECTION ( 'NONE',  ( 0.000000000000000000, 0.000000000000000000, 1.000000000000000000 ) ) ;
#64234 = DIRECTION ( 'NONE',  ( 0.000000000000000000, 0.000000000000000000, 1.000000000000000000 ) ) ;
#64235 = CARTESIAN_POINT ( 'NONE',  ( 11.99999999999999822, -77.16300072079681627, 27.74655509720640367 ) ) ;
#64236 = LINE ( 'NONE', #28521, #6305 ) ;
#64237 = APPLICATION_CONTEXT ( 'automotive_design' ) ;
#64238 = AXIS2_PLACEMENT_3D ( 'NONE', #27561, #68161, #73418 ) ;
#64239 = DIRECTION ( 'NONE',  ( -1.000000000000000000, 3.061616997868382648E-16, 0.000000000000000000 ) ) ;
#64240 = VECTOR ( 'NONE', #70464, 1000.000000000000000 ) ;
#64241 = CARTESIAN_POINT ( 'NONE',  ( 26.47460221209471598, -121.8961639463267090, 5.500000000000000000 ) ) ;
#64242 = CARTESIAN_POINT ( 'NONE',  ( -97.30629616937501680, 90.00000000000004263, 85.19781250086714408 ) ) ;
#64243 = PLANE ( 'NONE',  #67152 ) ;
#64244 = EDGE_CURVE ( 'NONE', #16870, #71356, #55745, .T. ) ;
#64245 = EDGE_CURVE ( 'NONE', #60337, #36560, #67088, .T. ) ;
#64246 = PLANE ( 'NONE',  #56470 ) ;
#64247 = ADVANCED_FACE ( 'NONE', ( #59632 ), #48342, .T. ) ;
#64248 = ORIENTED_EDGE ( 'NONE', *, *, #20611, .F. ) ;
#64249 = DIRECTION ( 'NONE',  ( 0.000000000000000000, 0.000000000000000000, 1.000000000000000000 ) ) ;
#64250 = CARTESIAN_POINT ( 'NONE',  ( 93.67500000000001137, -207.7050326799711968, 76.00354166840097037 ) ) ;
#64251 = CARTESIAN_POINT ( 'NONE',  ( 6.938893903907228378E-15, 0.000000000000000000, 0.000000000000000000 ) ) ;
#64252 = ADVANCED_FACE ( 'NONE', ( #45964 ), #39200, .F. ) ;
#64253 = CARTESIAN_POINT ( 'NONE',  ( -20.63750000000000284, -2.946905753441389499E-14, -1.643265707204933640E-14 ) ) ;
#64254 = VECTOR ( 'NONE', #14892, 1000.000000000000000 ) ;
#64255 = CARTESIAN_POINT ( 'NONE',  ( 96.15314808468750130, -211.9973110713294489, 81.75822916753382685 ) ) ;
#64256 = EDGE_CURVE ( 'NONE', #57167, #43311, #13346, .T. ) ;
#64257 = ORIENTED_EDGE ( 'NONE', *, *, #39207, .F. ) ;
#64258 = EDGE_LOOP ( 'NONE', ( #14033, #52153, #60977, #57162, #73960 ) ) ;
#64259 = DIRECTION ( 'NONE',  ( 0.000000000000000000, 0.000000000000000000, 1.000000000000000000 ) ) ;
#64260 = ORIENTED_EDGE ( 'NONE', *, *, #3175, .F. ) ;
#64261 = FACE_OUTER_BOUND ( 'NONE', #60212, .T. ) ;
#64262 = CARTESIAN_POINT ( 'NONE',  ( -92.35000000000003695, 90.00000000000004263, 90.00000000000000000 ) ) ;
#64263 = AXIS2_PLACEMENT_3D ( 'NONE', #46875, #24310, #6287 ) ;
#64264 = EDGE_CURVE ( 'NONE', #17476, #23851, #27908, .T. ) ;
#64265 = ORIENTED_EDGE ( 'NONE', *, *, #61366, .F. ) ;
#64266 = CARTESIAN_POINT ( 'NONE',  ( 97.30629616937498838, -208.6684592857803011, 78.10697916753383652 ) ) ;
#64267 = ORIENTED_EDGE ( 'NONE', *, *, #42054, .F. ) ;
#64268 = CARTESIAN_POINT ( 'NONE',  ( 10.00000000000000000, 0.000000000000000000, 0.000000000000000000 ) ) ;
#64269 = ORIENTED_EDGE ( 'NONE', *, *, #44074, .T. ) ;
#64270 = AXIS2_PLACEMENT_3D ( 'NONE', #48058, #41670, #47322 ) ;
#64271 = ORIENTED_EDGE ( 'NONE', *, *, #54571, .F. ) ;
#64272 = DIRECTION ( 'NONE',  ( -1.000000000000000000, -0.000000000000000000, -0.000000000000000000 ) ) ;
#64273 = CARTESIAN_POINT ( 'NONE',  ( 12.69589495141918611, -96.69089767102708777, 5.500000000000000000 ) ) ;
#64274 = AXIS2_PLACEMENT_3D ( 'NONE', #38321, #5245, #51081 ) ;
#64275 = ORIENTED_EDGE ( 'NONE', *, *, #67071, .T. ) ;
#64276 = DIRECTION ( 'NONE',  ( 0.000000000000000000, -0.6494480483301739993, -0.7604059656000391465 ) ) ;
#64277 = CARTESIAN_POINT ( 'NONE',  ( 95.00000000000000000, -206.9400435732949575, 82.30062500173428930 ) ) ;
#64278 = CARTESIAN_POINT ( 'NONE',  ( 97.64999999999997726, 91.52997821335252127, 89.73541666666666572 ) ) ;
#64279 = EDGE_CURVE ( 'NONE', #35203, #30584, #139, .T. ) ;
#64280 = ORIENTED_EDGE ( 'NONE', *, *, #71981, .T. ) ;
#64281 = CARTESIAN_POINT ( 'NONE',  ( 0.000000000000000000, 0.000000000000000000, 0.000000000000000000 ) ) ;
#64282 = EDGE_CURVE ( 'NONE', #57971, #37558, #42043, .T. ) ;
#64283 = CARTESIAN_POINT ( 'NONE',  ( 0.000000000000000000, 0.000000000000000000, 0.000000000000000000 ) ) ;
#64284 = ORIENTED_EDGE ( 'NONE', *, *, #49695, .F. ) ;
#64285 = ORIENTED_EDGE ( 'NONE', *, *, #31836, .T. ) ;
#64286 = CARTESIAN_POINT ( 'NONE',  ( 0.000000000000000000, 0.000000000000000000, 0.000000000000000000 ) ) ;
#64287 = ORIENTED_EDGE ( 'NONE', *, *, #19019, .T. ) ;
#64288 = AXIS2_PLACEMENT_3D ( 'NONE', #11755, #35800, #47108 ) ;
#64289 = CARTESIAN_POINT ( 'NONE',  ( 96.32499999999997442, 92.29496732002878900, 84.78770833506763438 ) ) ;
#64290 = ORIENTED_EDGE ( 'NONE', *, *, #40513, .T. ) ;
#64291 = ORIENTED_EDGE ( 'NONE', *, *, #56987, .T. ) ;
#64292 = DIRECTION ( 'NONE',  ( -1.000000000000000000, 0.000000000000000000, 0.000000000000000000 ) ) ;
#64293 = CARTESIAN_POINT ( 'NONE',  ( 10.00000000000000000, 0.000000000000000000, 0.000000000000000000 ) ) ;
#64294 = ORIENTED_EDGE ( 'NONE', *, *, #13247, .T. ) ;
#64295 = VERTEX_POINT ( 'NONE', #17013 ) ;
#64296 = VECTOR ( 'NONE', #70863, 1000.000000000000000 ) ;
#64297 = ORIENTED_EDGE ( 'NONE', *, *, #22924, .T. ) ;
#64298 = LINE ( 'NONE', #53373, #18119 ) ;
#64299 = CARTESIAN_POINT ( 'NONE',  ( 10.00000000000000000, 37.48860685352291000, 0.8828120875901893649 ) ) ;
#64300 = CARTESIAN_POINT ( 'NONE',  ( -97.65000000000001990, 91.52997821335253548, 88.67708333333332860 ) ) ;
#64301 = ORIENTED_EDGE ( 'NONE', *, *, #45709, .F. ) ;
#64302 = CYLINDRICAL_SURFACE ( 'NONE', #52792, 42.00000000000000000 ) ;
#64303 = DIRECTION ( 'NONE',  ( 0.000000000000000000, 0.000000000000000000, 1.000000000000000000 ) ) ;
#64304 = ORIENTED_EDGE ( 'NONE', *, *, #15292, .F. ) ;
#64305 = CARTESIAN_POINT ( 'NONE',  ( -97.30629616937497417, -211.3315407142195852, 82.07572916753380809 ) ) ;
#64306 = ORIENTED_EDGE ( 'NONE', *, *, #22268, .F. ) ;
#64307 = CARTESIAN_POINT ( 'NONE',  ( 10.00000000000000000, 17.80606268964540462, 33.00180498840053644 ) ) ;
#64308 = CARTESIAN_POINT ( 'NONE',  ( 92.48632958231168288, -210.0000000000000284, 74.91808492278046572 ) ) ;
#64309 = FACE_OUTER_BOUND ( 'NONE', #32915, .T. ) ;
#64310 = CARTESIAN_POINT ( 'NONE',  ( -97.30629616937497417, -211.3315407142195852, 75.72572916753381378 ) ) ;
#64311 = DIRECTION ( 'NONE',  ( 0.000000000000000000, -1.000000000000000000, -1.040834085586084257E-14 ) ) ;
#64312 = AXIS2_PLACEMENT_3D ( 'NONE', #59195, #7686, #24974 ) ;
#64313 = CARTESIAN_POINT ( 'NONE',  ( 10.00000000000000000, -33.79645857604501913, -16.45098606841161626 ) ) ;
#64314 = CARTESIAN_POINT ( 'NONE',  ( 10.00000000000000000, -59.75363087400034345, -56.15606465355021015 ) ) ;
#64315 = PLANE ( 'NONE',  #8732 ) ;
#64316 = DIRECTION ( 'NONE',  ( -0.000000000000000000, 0.5000000000000004441, 0.8660254037844383745 ) ) ;
#64317 = EDGE_CURVE ( 'NONE', #25333, #23675, #70411, .T. ) ;
#64318 = CARTESIAN_POINT ( 'NONE',  ( -95.00000000000002842, 87.33691857156074434, 78.37156250086714238 ) ) ;
#64319 = DIRECTION ( 'NONE',  ( -1.000000000000000000, -0.000000000000000000, 0.000000000000000000 ) ) ;
#64320 = FACE_OUTER_BOUND ( 'NONE', #42012, .T. ) ;
#64321 = B_SPLINE_CURVE_WITH_KNOTS ( 'NONE', 3,
 ( #6128, #11729, #34672, #6489, #57623, #12844, #47442, #29029, #63639, #29759, #64369, #18855, #35418, #46704, #52709, #1622, #51595, #29390 ),
 .UNSPECIFIED., .F., .F.,
 ( 4, 2, 2, 2, 2, 2, 2, 2, 4 ),
 ( -0.004093595874563310012, -0.003575961937392308637, -0.003058328000221307262, -0.002540694063050305887, -0.002023060125879304512, -0.001505426188708303137, -0.0009877922515373017617, -0.0004701583143663003866, 4.747562280470098844E-05 ),
 .UNSPECIFIED. ) ;
#64322 = AXIS2_PLACEMENT_3D ( 'NONE', #2836, #25727, #48664 ) ;
#64323 = CARTESIAN_POINT ( 'NONE',  ( 0.000000000000000000, 0.000000000000000000, 0.000000000000000000 ) ) ;
#64325 = DIRECTION ( 'NONE',  ( -1.000000000000000000, 0.000000000000000000, 0.000000000000000000 ) ) ;
#64324 = AXIS2_PLACEMENT_3D ( 'NONE', #38939, #21636, #67880 ) ;
#64326 = DIRECTION ( 'NONE',  ( -1.000000000000000000, 0.000000000000000000, -0.000000000000000000 ) ) ;
#64327 = CARTESIAN_POINT ( 'NONE',  ( -92.34999999999999432, -209.9999999999999716, 90.00000000000000000 ) ) ;
#64328 = DIRECTION ( 'NONE',  ( -1.000000000000000000, 0.000000000000000000, 0.000000000000000000 ) ) ;
#64329 = LINE ( 'NONE', #51560, #8934 ) ;
#64330 = CARTESIAN_POINT ( 'NONE',  ( -92.69370383062498320, -208.6684592857803011, 75.56697916753383026 ) ) ;
#64331 = ADVANCED_FACE ( 'NONE', ( #22280 ), #61768, .F. ) ;
#64332 = AXIS2_PLACEMENT_3D ( 'NONE', #71309, #19814, #60077 ) ;
#64333 = EDGE_CURVE ( 'NONE', #47446, #57658, #22829, .T. ) ;
#64334 = CARTESIAN_POINT ( 'NONE',  ( 5.000000000000000000, -0.9724665692850895660, -5.958069561147902427 ) ) ;
#64335 = CIRCLE ( 'NONE', #43941, 17.50000000000000355 ) ;
#64336 = AXIS2_PLACEMENT_3D ( 'NONE', #42571, #9457, #13979 ) ;
#64337 = EDGE_LOOP ( 'NONE', ( #22219, #20462, #34664, #46976 ) ) ;
#64338 = CARTESIAN_POINT ( 'NONE',  ( 11.99999999999999822, 0.000000000000000000, 0.000000000000000000 ) ) ;
#64339 = LINE ( 'NONE', #12811, #25085 ) ;
#64340 = DIRECTION ( 'NONE',  ( 0.000000000000000000, -0.2079116908177651990, -0.9781476007338044676 ) ) ;
#64341 = ADVANCED_FACE ( 'NONE', ( #56504 ), #63255, .T. ) ;
#64342 = CARTESIAN_POINT ( 'NONE',  ( -92.35000000000003695, 90.00000000000004263, 86.50750000000000739 ) ) ;
#64343 = EDGE_CURVE ( 'NONE', #13949, #43951, #50840, .T. ) ;
#64344 = AXIS2_PLACEMENT_3D ( 'NONE', #29010, #22269, #62125 ) ;
#64345 = FACE_OUTER_BOUND ( 'NONE', #42069, .T. ) ;
#64346 = ORIENTED_EDGE ( 'NONE', *, *, #31473, .T. ) ;
#64347 = LINE ( 'NONE', #41768, #65950 ) ;
#64348 = FACE_OUTER_BOUND ( 'NONE', #16941, .T. ) ;
#64349 = ORIENTED_EDGE ( 'NONE', *, *, #44199, .T. ) ;
#64350 = CARTESIAN_POINT ( 'NONE',  ( 92.69370383062501162, -208.6684592857803295, 86.41489583420047893 ) ) ;
#64351 = CARTESIAN_POINT ( 'NONE',  ( 96.15314808468748708, -208.0026889286704943, 87.68489583420048916 ) ) ;
#64352 = EDGE_CURVE ( 'NONE', #69125, #41920, #6044, .T. ) ;
#64353 = ORIENTED_EDGE ( 'NONE', *, *, #10532, .F. ) ;
#64354 = CARTESIAN_POINT ( 'NONE',  ( 92.69370383062501162, -209.9999999999999716, 89.16656250086715829 ) ) ;
#64355 = VERTEX_POINT ( 'NONE', #10246 ) ;
#64356 = CARTESIAN_POINT ( 'NONE',  ( 11.59999999999999787, 1.420590287010929336E-15, 42.00000000000001421 ) ) ;
#64357 = VERTEX_POINT ( 'NONE', #33170 ) ;
#64358 = CARTESIAN_POINT ( 'NONE',  ( -95.00000000000002842, 87.33691857156074434, 80.43531250086715545 ) ) ;
#64359 = VERTEX_POINT ( 'NONE', #56118 ) ;
#64360 = ORIENTED_EDGE ( 'NONE', *, *, #50430, .T. ) ;
#64361 = CARTESIAN_POINT ( 'NONE',  ( -97.64999999999996305, -209.9999999999999716, 87.53937500173429953 ) ) ;
#64362 = VERTEX_POINT ( 'NONE', #68138 ) ;
#64363 = DIRECTION ( 'NONE',  ( 2.603472992746261562E-14, 2.546204323184492723E-14, -1.000000000000000000 ) ) ;
#64364 = CARTESIAN_POINT ( 'NONE',  ( -10.00000000000000000, 0.000000000000000000, 0.000000000000000000 ) ) ;
#64365 = EDGE_CURVE ( 'NONE', #23903, #40406, #5006, .T. ) ;
#64366 = ORIENTED_EDGE ( 'NONE', *, *, #60350, .T. ) ;
#64367 = FACE_OUTER_BOUND ( 'NONE', #66993, .T. ) ;
#64368 = ORIENTED_EDGE ( 'NONE', *, *, #56650, .T. ) ;
#64369 = CARTESIAN_POINT ( 'NONE',  ( 93.46017751755557867, 87.90457393955796306, 74.96680960279266515 ) ) ;
#64370 = ADVANCED_FACE ( 'NONE', ( #50472 ), #21901, .F. ) ;
#64371 = VECTOR ( 'NONE', #71117, 1000.000000000000227 ) ;
#64372 = ORIENTED_EDGE ( 'NONE', *, *, #33725, .T. ) ;
#64373 = EDGE_LOOP ( 'NONE', ( #68087, #56879, #23830, #53126 ) ) ;
#64374 = ORIENTED_EDGE ( 'NONE', *, *, #45851, .T. ) ;
#64375 = CARTESIAN_POINT ( 'NONE',  ( 92.69370383062501162, -211.3315407142195852, 80.80572916753382628 ) ) ;
#64376 = CONTEXT_DEPENDENT_SHAPE_REPRESENTATION ( #67622, #22418 ) ;
#64377 = FACE_OUTER_BOUND ( 'NONE', #2703, .T. ) ;
#64378 = CARTESIAN_POINT ( 'NONE',  ( -92.35000000000003695, 90.00000000000004263, 90.00000000000000000 ) ) ;
#64379 = AXIS2_PLACEMENT_3D ( 'NONE', #33908, #62884, #1230 ) ;
#64380 = CARTESIAN_POINT ( 'NONE',  ( 0.000000000000000000, 0.000000000000000000, 0.000000000000000000 ) ) ;
#64381 = CARTESIAN_POINT ( 'NONE',  ( 2.500000000000000000, 0.000000000000000000, -5.624496230895140947 ) ) ;
#64382 = VECTOR ( 'NONE', #27965, 1000.000000000000000 ) ;
#64383 = PLANE ( 'NONE',  #57631 ) ;
#64384 = DIRECTION ( 'NONE',  ( 1.000000000000000000, 0.000000000000000000, 0.000000000000000000 ) ) ;
#64385 = CARTESIAN_POINT ( 'NONE',  ( -94.99999999999997158, -212.6630814284392557, 84.72156250086713669 ) ) ;
#64386 = CARTESIAN_POINT ( 'NONE',  ( -97.30629616937501680, 90.00000000000004263, 84.08656250086716000 ) ) ;
#64387 = VERTEX_POINT ( 'NONE', #20455 ) ;
#64388 = CIRCLE ( 'NONE', #69217, 2.650000000000540812 ) ;
#64389 = CARTESIAN_POINT ( 'NONE',  ( 92.69370383062498320, 90.00000000000002842, 81.38781250086714181 ) ) ;
#64390 = VECTOR ( 'NONE', #4213, 999.9999999999998863 ) ;
#64391 =( BOUNDED_CURVE ( )  B_SPLINE_CURVE ( 2, ( #34174, #57117, #50715, #51092, #12343, #35283, #58210, #69139, #11239 ),
 .UNSPECIFIED., .F., .F. ) 
 B_SPLINE_CURVE_WITH_KNOTS ( ( 3, 2, 2, 2, 3 ),
 ( 0.3386766260338262002, 0.3386767459623536980, 0.3457325115032360840, 0.3527882770441184701, 0.3598440426530882807 ),
 .UNSPECIFIED. ) 
 CURVE ( )  GEOMETRIC_REPRESENTATION_ITEM ( )  RATIONAL_B_SPLINE_CURVE ( ( 0.9999954456811669390, 0.9999977228018773756, 1.000000000000000000, 0.8660254037844387076, 1.000000000000000000, 0.8660254037844387076, 1.000000000000000000, 0.8660254037844387076, 1.000000000000000000 ) ) 
 REPRESENTATION_ITEM ( '' )  );
#64392 = ORIENTED_EDGE ( 'NONE', *, *, #16615, .T. ) ;
#64393 = FACE_OUTER_BOUND ( 'NONE', #64003, .T. ) ;
#64394 = CARTESIAN_POINT ( 'NONE',  ( 0.000000000000000000, 79.10210256391368944, 21.60688246758614994 ) ) ;
#64395 = CARTESIAN_POINT ( 'NONE',  ( 11.99999999999999822, 0.000000000000000000, 0.000000000000000000 ) ) ;
#64396 = DIRECTION ( 'NONE',  ( 0.000000000000000000, -0.8910065241883626808, -0.4539904997395568520 ) ) ;
#64397 = CARTESIAN_POINT ( 'NONE',  ( -10.00000000000000000, 0.000000000000000000, 0.000000000000000000 ) ) ;
#64398 = CARTESIAN_POINT ( 'NONE',  ( -97.30629616937497417, -211.3315407142195852, 86.52072916753381548 ) ) ;
#64399 = DIRECTION ( 'NONE',  ( 1.000000000000000000, -0.000000000000000000, 0.000000000000000000 ) ) ;
#64400 = CARTESIAN_POINT ( 'NONE',  ( 10.00000000000000000, -39.47590169984896136, 71.87247863392398983 ) ) ;
#64401 = FACE_OUTER_BOUND ( 'NONE', #39128, .T. ) ;
#64402 = DIRECTION ( 'NONE',  ( -1.000000000000000000, -0.000000000000000000, 0.000000000000000000 ) ) ;
#64403 = ORIENTED_EDGE ( 'NONE', *, *, #67667, .F. ) ;
#64404 = ORIENTED_EDGE ( 'NONE', *, *, #8133, .F. ) ;
#64405 = DIRECTION ( 'NONE',  ( 0.000000000000000000, -0.2079116908177532363, 0.9781476007338069101 ) ) ;
#64406 = CARTESIAN_POINT ( 'NONE',  ( 97.64999999999999147, -209.9999999999999716, 89.04749999999999943 ) ) ;
#64407 = CARTESIAN_POINT ( 'NONE',  ( -93.84685191531252713, 88.00268892867056536, 87.31447916753380412 ) ) ;
#64408 = CARTESIAN_POINT ( 'NONE',  ( 95.04693102382854875, 87.35041560265749183, 75.00000002508419072 ) ) ;
#64409 = DIRECTION ( 'NONE',  ( -0.8571673007021122226, 1.049727191138618572E-16, 0.5150380749100542666 ) ) ;
#64410 = EDGE_CURVE ( 'NONE', #70238, #22507, #25356, .T. ) ;
#64411 = FACE_OUTER_BOUND ( 'NONE', #61885, .T. ) ;
#64412 = CARTESIAN_POINT ( 'NONE',  ( -94.99999999999997158, -206.9400435732949575, 78.41125000000000966 ) ) ;
#64413 = ORIENTED_EDGE ( 'NONE', *, *, #46401, .F. ) ;
#64414 = CARTESIAN_POINT ( 'NONE',  ( -92.69370383062504004, 90.00000000000004263, 75.99031250086714806 ) ) ;
#64415 = CARTESIAN_POINT ( 'NONE',  ( 0.000000000000000000, 0.000000000000000000, 0.000000000000000000 ) ) ;
#64416 = ADVANCED_FACE ( 'NONE', ( #26455 ), #66330, .T. ) ;
#64417 = CLOSED_SHELL ( 'NONE', ( #16153, #53742, #2069, #73600, #43163, #43987, #39548, #73495, #20540, #72125, #1818, #20373, #15801, #20689, #10679, #72284, #16282, #43622, #26925, #30445, #15173, #50486, #3923, #61815, #11457, #827, #10784, #34099, #17586, #1888, #34747, #47978, #68144, #28174, #60532, #48950, #68515, #806, #19198, #17477, #16908, #59152, #67641, #40912, #39928, #74071, #19173, #5214, #59519, #1940, #68928, #44811, #20828, #61740, #53205, #39847, #23490, #56575, #28867, #56389, #58331, #26383, #15616, #46484, #34869, #33973, #41740, #58295, #32227, #46041, #27781, #57289, #70874, #1986, #14869, #59224, #13597, #41361, #58076, #48392, #39926, #1185, #38441, #63984, #65223, #74162, #10588, #57168, #45916, #73669, #27244, #35877, #40659, #15079, #66460, #69595, #68593, #26582, #46537, #12078, #23025, #52205, #46927, #38906, #15555, #10091, #21394, #67398, #63583, #42796, #45952, #17301, #64080, #42512, #18322, #50404, #61904, #36940, #69264, #63991, #28249, #71527, #18267, #28963, #27752, #62477, #3757, #56970, #7804, #60714, #17379, #57718, #33779, #60366, #42549, #57436, #24960, #68915, #2953, #34214, #31118, #54151, #31081, #38288, #25783, #54575, #19848, #58449, #64507, #9869, #60546, #32072, #68609, #13902, #51585, #2455, #31384, #46358, #44851, #30818, #31585, #49573, #30209, #71994, #37706, #23948, #74268, #46881, #38626, #38811, #42458, #68999, #11144, #10509, #72467, #9607, #57546, #64370, #19918, #3511, #20249, #16324, #24551, #65982, #51028, #46170, #23417, #2226, #39293, #7554, #63675, #60305, #25533, #31615, #17155, #63782, #13924, #4600, #556, #62706, #56510, #70031, #38255, #51174, #65770, #32483, #14001, #63752, #51843, #8938, #52218, #70764, #71102, #36341, #33780, #57053, #206, #60953, #15305, #26032, #19757, #61531, #53921, #12294, #13919, #7742, #31966, #466, #12552, #41444, #1265, #69597, #56450, #51406, #54920, #50927, #57787, #5617, #21579, #65534, #69585, #1967, #3613, #59651, #20785, #39837, #35485, #24204, #64022, #3033, #69172, #32259, #6899, #17990, #13596, #73332, #19768, #72902, #40754, #5694, #9650, #61948, #221, #33518, #55269, #63189, #10247, #37860, #45874, #2866, #14276, #65526, #53873 ) ) ;
#64418 = CARTESIAN_POINT ( 'NONE',  ( 10.00000000000000000, 0.000000000000000000, 0.000000000000000000 ) ) ;
#64419 = LINE ( 'NONE', #47852, #5730 ) ;
#64420 = DIRECTION ( 'NONE',  ( 0.000000000000000000, -0.4067366430758010409, 0.9135454576426005335 ) ) ;
#64421 = CARTESIAN_POINT ( 'NONE',  ( -97.30629616937497417, -211.3315407142195852, 87.31447916753381833 ) ) ;
#64422 =( LENGTH_UNIT ( ) NAMED_UNIT ( * ) SI_UNIT ( .MILLI., .METRE. ) );
#64423 = ADVANCED_FACE ( 'NONE', ( #54662 ), #20066, .F. ) ;
#64424 = CARTESIAN_POINT ( 'NONE',  ( 4.999999999999999112, 40.68715046381943523, -10.41901085202036370 ) ) ;
#64425 = CARTESIAN_POINT ( 'NONE',  ( 0.000000000000000000, 40.65526001592611749, 71.21200624218811015 ) ) ;
#64426 = CARTESIAN_POINT ( 'NONE',  ( -97.30629616937497417, -211.3315407142195852, 77.15447916753382174 ) ) ;
#64427 = CARTESIAN_POINT ( 'NONE',  ( 0.000000000000000000, 17.67226234102874116, -33.17418723428288274 ) ) ;
#64428 = EDGE_LOOP ( 'NONE', ( #21910, #60674, #44201, #59089 ) ) ;
#64429 = EDGE_CURVE ( 'NONE', #305, #44128, #63683, .T. ) ;
#64430 = CARTESIAN_POINT ( 'NONE',  ( -92.35000000000003695, 89.99999413691148220, 82.77687479895028844 ) ) ;
#64431 = CARTESIAN_POINT ( 'NONE',  ( -1.192633404626841198, -119.0902607174754451, 2.500000000000000000 ) ) ;
#64432 = CIRCLE ( 'NONE', #52395, 82.00000000000000000 ) ;
#64433 = VECTOR ( 'NONE', #44214, 1000.000000000000000 ) ;
#64434 = CARTESIAN_POINT ( 'NONE',  ( -92.69370383062504004, 89.06968786819598449, 74.84209103131394158 ) ) ;
#64435 = CARTESIAN_POINT ( 'NONE',  ( 92.69370383062501162, -209.9999999999999716, 78.21281250086714465 ) ) ;
#64436 = EDGE_LOOP ( 'NONE', ( #20588, #33551, #16767, #16823, #65857, #41433, #65137, #1412, #439, #60572, #72584, #52259, #18924, #10330, #29280, #61243, #36630, #56624, #41699, #66773, #8420, #33717, #56206, #15705, #7384, #49924, #8229, #4775, #5660, #74083, #65103, #63761, #33834, #17658, #66414, #69421, #17565, #49075, #57237, #17673, #64444, #42104, #20171, #55638, #5412, #713, #25274, #63846, #15509, #60841, #5392, #14895, #72672, #60692, #66661, #36702, #31704, #3926, #71082, #38009, #5916, #22489, #59627, #29109, #66235, #6409, #57317, #25694, #11555, #31144, #2718, #19300, #55853, #24311, #47693, #24683, #42744, #59188, #13880, #55646, #12930, #63029, #28251, #28652, #364, #52366, #2549, #48887, #50782, #38781, #32158, #16163, #72279, #3982, #46621, #25184, #66750, #63979, #2324, #26326, #59035, #41504, #17877, #6108, #27842, #63976, #43335, #67534, #72062, #10523, #26419, #13204, #60313, #28849, #31506, #20802, #21800, #46232, #16490, #33644, #36897, #46904, #4206, #9730, #4549, #32841, #57950, #23613, #59215, #56731, #63251, #27924, #16364, #52224, #42978, #64908, #38667, #70441, #69981, #62180, #66283, #73700, #57685, #68446, #43934, #17587, #17300, #46187, #36068, #12151, #24001, #37032, #37279, #65938, #59001, #74144, #10437, #30332, #54999, #29944, #23564, #64135, #44582, #67916, #3077 ) ) ;
#64437 = AXIS2_PLACEMENT_3D ( 'NONE', #45846, #5620, #15 ) ;
#64438 = FACE_OUTER_BOUND ( 'NONE', #30142, .T. ) ;
#64439 = EDGE_CURVE ( 'NONE', #56500, #1655, #61043, .T. ) ;
#64440 = VERTEX_POINT ( 'NONE', #37001 ) ;
#64441 = CARTESIAN_POINT ( 'NONE',  ( 10.00000000000000000, 16.95692799528845640, -2.500000000000000000 ) ) ;
#64442 = EDGE_CURVE ( 'NONE', #33185, #41089, #44279, .T. ) ;
#64443 = EDGE_CURVE ( 'NONE', #21975, #420, #16814, .T. ) ;
#64444 = ORIENTED_EDGE ( 'NONE', *, *, #10421, .F. ) ;
#64445 = DIRECTION ( 'NONE',  ( 0.000000000000000000, 0.3090169943749482839, -0.9510565162951533091 ) ) ;
#64446 = EDGE_CURVE ( 'NONE', #14708, #1257, #71192, .T. ) ;
#64447 = ORIENTED_EDGE ( 'NONE', *, *, #68193, .T. ) ;
#64448 = VERTEX_POINT ( 'NONE', #71571 ) ;
#64449 = ORIENTED_EDGE ( 'NONE', *, *, #59435, .T. ) ;
#64450 = DIRECTION ( 'NONE',  ( 0.000000000000000000, 0.000000000000000000, 1.000000000000000000 ) ) ;
#64451 = EDGE_CURVE ( 'NONE', #17447, #44755, #43022, .T. ) ;
#64452 = ORIENTED_EDGE ( 'NONE', *, *, #45669, .T. ) ;
#64453 = ORIENTED_EDGE ( 'NONE', *, *, #64597, .F. ) ;
#64454 = CARTESIAN_POINT ( 'NONE',  ( 96.15314808468748708, 91.99731107132950569, 80.69989583420047552 ) ) ;
#64455 = LINE ( 'NONE', #12926, #73181 ) ;
#64456 = FACE_OUTER_BOUND ( 'NONE', #4940, .T. ) ;
#64457 = ORIENTED_EDGE ( 'NONE', *, *, #12546, .T. ) ;
#64458 = ORIENTED_EDGE ( 'NONE', *, *, #44734, .T. ) ;
#64459 = EDGE_LOOP ( 'NONE', ( #5225, #30765, #6748, #54856 ) ) ;
#64460 = FACE_OUTER_BOUND ( 'NONE', #21321, .T. ) ;
#64461 = ORIENTED_EDGE ( 'NONE', *, *, #32932, .F. ) ;
#64462 = AXIS2_PLACEMENT_3D ( 'NONE', #59142, #30549, #24918 ) ;
#64463 = DIRECTION ( 'NONE',  ( 0.000000000000000000, 0.000000000000000000, 1.000000000000000000 ) ) ;
#64464 = CARTESIAN_POINT ( 'NONE',  ( 97.64999999999999147, 90.00000000000002842, 90.00000000000000000 ) ) ;
#64465 = CARTESIAN_POINT ( 'NONE',  ( 12.50000000000000000, -132.5000000000000000, -40.00000000000000000 ) ) ;
#64466 = DIRECTION ( 'NONE',  ( -1.000000000000000000, -0.000000000000000000, -0.000000000000000000 ) ) ;
#64467 = DIRECTION ( 'NONE',  ( -1.000000000000000000, -0.000000000000000000, 0.000000000000000000 ) ) ;
#64468 = CARTESIAN_POINT ( 'NONE',  ( 11.99999999999999822, 26.01480285779933510, -70.53064760720289428 ) ) ;
#64469 = CARTESIAN_POINT ( 'NONE',  ( -4.250000000000000000, -13.95926121303099343, -1.199999999999999956 ) ) ;
#64470 = CARTESIAN_POINT ( 'NONE',  ( -97.64999999999996305, -209.9999999999999716, 78.01437500173430806 ) ) ;
#64471 = DIRECTION ( 'NONE',  ( 1.000000000000000000, 0.000000000000000000, 0.000000000000000000 ) ) ;
#64472 = ORIENTED_EDGE ( 'NONE', *, *, #24284, .F. ) ;
#64474 = CARTESIAN_POINT ( 'NONE',  ( -92.35000000000003695, 90.00000000000004263, 76.42687500173430237 ) ) ;
#64473 = CARTESIAN_POINT ( 'NONE',  ( 96.32499999999997442, 92.29496732002878900, 76.53270833506762472 ) ) ;
#64475 = VERTEX_POINT ( 'NONE', #15550 ) ;
#64476 = CARTESIAN_POINT ( 'NONE',  ( 93.84685191531248449, 88.00268892867053694, 81.65239583420049030 ) ) ;
#64477 = CARTESIAN_POINT ( 'NONE',  ( 96.32499999999998863, 87.70503267997126784, 75.60666666666665492 ) ) ;
#64478 = CARTESIAN_POINT ( 'NONE',  ( 0.000000000000000000, 29.81001611431041098, -22.74946021919100403 ) ) ;
#64479 = DIRECTION ( 'NONE',  ( 0.9580045777625452175, 0.2867529058022035837, -0.000000000000000000 ) ) ;
#64480 = VECTOR ( 'NONE', #68057, 1000.000000000000000 ) ;
#64481 = DIRECTION ( 'NONE',  ( 0.000000000000000000, 0.000000000000000000, 1.000000000000000000 ) ) ;
#64482 = ORIENTED_EDGE ( 'NONE', *, *, #88, .T. ) ;
#64483 = LINE ( 'NONE', #12958, #62581 ) ;
#64484 = DIRECTION ( 'NONE',  ( 0.000000000000000000, 0.000000000000000000, 1.000000000000000000 ) ) ;
#64485 = ORIENTED_EDGE ( 'NONE', *, *, #44654, .F. ) ;
#64486 = AXIS2_PLACEMENT_3D ( 'NONE', #72372, #13471, #38915 ) ;
#64487 = ORIENTED_EDGE ( 'NONE', *, *, #67054, .F. ) ;
#64488 = AXIS2_PLACEMENT_3D ( 'NONE', #10740, #16757, #39696 ) ;
#64489 = DIRECTION ( 'NONE',  ( 0.000000000000000000, 0.6494480483301793283, 0.7604059656000345946 ) ) ;
#64490 = AXIS2_PLACEMENT_3D ( 'NONE', #17621, #744, #23633 ) ;
#64491 = CARTESIAN_POINT ( 'NONE',  ( 10.00000000000000000, 37.58145647212455032, -0.6853352020786441789 ) ) ;
#64492 = CARTESIAN_POINT ( 'NONE',  ( -97.64999999999996305, -209.9999999999999716, 76.03000000000000114 ) ) ;
#64493 = CARTESIAN_POINT ( 'NONE',  ( -96.15314808468745866, -211.9973110713294489, 78.47739583420049314 ) ) ;
#64494 = VERTEX_POINT ( 'NONE', #60685 ) ;
#64495 = ADVANCED_FACE ( 'NONE', ( #49388 ), #3189, .T. ) ;
#64496 = ADVANCED_FACE ( 'NONE', ( #32086 ), #38107, .T. ) ;
#64497 = DIRECTION ( 'NONE',  ( 0.000000000000000000, -0.8660254037844363761, 0.5000000000000039968 ) ) ;
#64498 = DIRECTION ( 'NONE',  ( 0.8660254037844382635, 0.5000000000000005551, 0.000000000000000000 ) ) ;
#64499 = EDGE_CURVE ( 'NONE', #68371, #73400, #26406, .T. ) ;
#64500 = AXIS2_PLACEMENT_3D ( 'NONE', #58150, #69069, #41229 ) ;
#64501 = CARTESIAN_POINT ( 'NONE',  ( 7.103376864691351012E-17, -120.0000000000000000, -85.59999999999999432 ) ) ;
#64502 = DIRECTION ( 'NONE',  ( 1.000000000000000000, 0.000000000000000000, 0.000000000000000000 ) ) ;
#64503 = LINE ( 'NONE', #53223, #48529 ) ;
#64504 = DIRECTION ( 'NONE',  ( -1.000000000000000000, -0.000000000000000000, -0.000000000000000000 ) ) ;
#64505 = DIRECTION ( 'NONE',  ( -0.8225049752423776450, -0.5687579148473765889, 0.000000000000000000 ) ) ;
#64506 = CARTESIAN_POINT ( 'NONE',  ( 92.34999999999999432, 89.99997747911952217, 86.26937578065384571 ) ) ;
#64507 = ADVANCED_FACE ( 'NONE', ( #8439 ), #2471, .F. ) ;
#64508 = CYLINDRICAL_SURFACE ( 'NONE', #48454, 31.99999999999999289 ) ;
#64509 = CIRCLE ( 'NONE', #60852, 77.49900000000000944 ) ;
#64510 = PLANE ( 'NONE',  #74183 ) ;
#64511 = EDGE_CURVE ( 'NONE', #4927, #30858, #9443, .T. ) ;
#64512 = CARTESIAN_POINT ( 'NONE',  ( 93.84685191531248449, 91.99731107132950569, 82.71072916753381321 ) ) ;
#64513 = CARTESIAN_POINT ( 'NONE',  ( -97.30629616937495996, -209.9999999999999716, 87.89656250086714806 ) ) ;
#64514 = CARTESIAN_POINT ( 'NONE',  ( 92.35001655588500569, 91.52998777189721125, 79.23145767387346439 ) ) ;
#64515 = VERTEX_POINT ( 'NONE', #59953 ) ;
#64516 = DIRECTION ( 'NONE',  ( 2.603472992746261562E-14, 2.546204323184492723E-14, -1.000000000000000000 ) ) ;
#64517 = CARTESIAN_POINT ( 'NONE',  ( -93.67499999999998295, -212.2949673200287179, 81.32166666666667254 ) ) ;
#64518 = CARTESIAN_POINT ( 'NONE',  ( -96.15314808468751551, 88.00268892867056536, 75.14364583420046984 ) ) ;
#64519 = CARTESIAN_POINT ( 'NONE',  ( 92.69370383062501162, -208.6684592857803011, 87.68489583420047495 ) ) ;
#64520 = ORIENTED_EDGE ( 'NONE', *, *, #43256, .F. ) ;
#64521 = ORIENTED_EDGE ( 'NONE', *, *, #17726, .T. ) ;
#64522 = MECHANICAL_DESIGN_GEOMETRIC_PRESENTATION_REPRESENTATION (  '', ( #62110 ), #74118 ) ;
#64523 = ORIENTED_EDGE ( 'NONE', *, *, #50647, .T. ) ;
#64524 = VECTOR ( 'NONE', #23685, 1000.000000000000000 ) ;
#64525 = FACE_OUTER_BOUND ( 'NONE', #45604, .T. ) ;
#64526 = EDGE_CURVE ( 'NONE', #60365, #63446, #32458, .T. ) ;
#64527 = EDGE_CURVE ( 'NONE', #70418, #46611, #28650, .T. ) ;
#64528 = LINE ( 'NONE', #41973, #7843 ) ;
#64529 = CIRCLE ( 'NONE', #38067, 2.500000000000000000 ) ;
#64530 = VERTEX_POINT ( 'NONE', #44874 ) ;
#64531 = AXIS2_PLACEMENT_3D ( 'NONE', #50147, #15953, #22341 ) ;
#64532 = ORIENTED_EDGE ( 'NONE', *, *, #29005, .F. ) ;
#64533 = CARTESIAN_POINT ( 'NONE',  ( 10.00000000000000000, 10.96151621346540317, -35.95386929396244113 ) ) ;
#64534 = CARTESIAN_POINT ( 'NONE',  ( 97.30629616937498838, -208.6684592857803295, 81.91697916753383879 ) ) ;
#64535 = CARTESIAN_POINT ( 'NONE',  ( 10.00000000000000000, 0.8261519478441983200, -77.49459641780885022 ) ) ;
#64536 = EDGE_CURVE ( 'NONE', #10181, #28846, #68448, .T. ) ;
#64537 = CARTESIAN_POINT ( 'NONE',  ( 5.000000000000000000, -32.34446384429951138, -26.79245525562750530 ) ) ;
#64538 = LINE ( 'NONE', #46502, #68874 ) ;
#64539 = CARTESIAN_POINT ( 'NONE',  ( 92.35000000000006537, -211.5299782133524786, 76.71791666666666742 ) ) ;
#64540 = DIRECTION ( 'NONE',  ( 1.000000000000000000, 0.000000000000000000, 0.000000000000000000 ) ) ;
#64541 = CARTESIAN_POINT ( 'NONE',  ( 95.00000000000000000, -206.9400435732949575, 83.49125000000000796 ) ) ;
#64542 = ORIENTED_EDGE ( 'NONE', *, *, #37165, .T. ) ;
#64543 = VERTEX_POINT ( 'NONE', #27567 ) ;
#64544 = ORIENTED_EDGE ( 'NONE', *, *, #5463, .T. ) ;
#64545 = ORIENTED_EDGE ( 'NONE', *, *, #14842, .F. ) ;
#64546 = CARTESIAN_POINT ( 'NONE',  ( -92.35000000000003695, 90.00000000000004263, 75.07749999999998636 ) ) ;
#64547 = VECTOR ( 'NONE', #66480, 1000.000000000000000 ) ;
#64548 =( LENGTH_UNIT ( ) NAMED_UNIT ( * ) SI_UNIT ( .MILLI., .METRE. ) );
#64549 = CARTESIAN_POINT ( 'NONE',  ( -92.69370383062502583, 91.33154071421968467, 87.63197916753382799 ) ) ;
#64550 = DIRECTION ( 'NONE',  ( 0.000000000000000000, 0.000000000000000000, 1.000000000000000000 ) ) ;
#64551 = DIRECTION ( 'NONE',  ( -1.000000000000000000, 0.000000000000000000, 0.000000000000000000 ) ) ;
#64552 = CARTESIAN_POINT ( 'NONE',  ( 97.30629616937498838, -209.9999999999999716, 89.32531250086714181 ) ) ;
#64553 = CARTESIAN_POINT ( 'NONE',  ( 96.32499999999997442, 92.29496732002878900, 77.72333333333332916 ) ) ;
#64554 = VERTEX_POINT ( 'NONE', #16665 ) ;
#64555 = CARTESIAN_POINT ( 'NONE',  ( -96.32499999999996021, -207.7050326799711968, 89.33854166840096411 ) ) ;
#64556 = ORIENTED_EDGE ( 'NONE', *, *, #66974, .T. ) ;
#64557 = CARTESIAN_POINT ( 'NONE',  ( -93.67499999999998295, -212.2949673200287179, 85.13166666666666060 ) ) ;
#64558 = ORIENTED_EDGE ( 'NONE', *, *, #69953, .T. ) ;
#64559 = CARTESIAN_POINT ( 'NONE',  ( -95.00000000000002842, 93.05995642670501411, 85.47562500173431488 ) ) ;
#64560 = CARTESIAN_POINT ( 'NONE',  ( 97.30629616937498838, 88.66845928578037217, 75.30239583420048177 ) ) ;
#64561 = EDGE_LOOP ( 'NONE', ( #21556, #12742, #20871, #35586 ) ) ;
#64562 = CARTESIAN_POINT ( 'NONE',  ( 2.499999999999979572, -90.00000000000000000, -280.0000000000000000 ) ) ;
#64563 = CARTESIAN_POINT ( 'NONE',  ( 10.00000000000000000, 39.78640506895604290, 66.50666863322015843 ) ) ;
#64564 = DIRECTION ( 'NONE',  ( 0.000000000000000000, -0.7071067811865535679, 0.7071067811865413555 ) ) ;
#64565 = FACE_OUTER_BOUND ( 'NONE', #16921, .T. ) ;
#64566 = ORIENTED_EDGE ( 'NONE', *, *, #64179, .T. ) ;
#64567 = CARTESIAN_POINT ( 'NONE',  ( -7.400000000000013678, 1.347575714539655834E-13, 12.49999999999999467 ) ) ;
#64568 = CARTESIAN_POINT ( 'NONE',  ( -93.84685191531248449, -208.0026889286704943, 74.82614583420047438 ) ) ;
#64569 = ORIENTED_EDGE ( 'NONE', *, *, #71604, .T. ) ;
#64570 = EDGE_LOOP ( 'NONE', ( #37197, #17380, #8710, #18284 ) ) ;
#64571 = DIRECTION ( 'NONE',  ( -1.000000000000000000, 0.000000000000000000, 0.000000000000000000 ) ) ;
#64572 = CARTESIAN_POINT ( 'NONE',  ( 5.000000000000000888, 0.000000000000000000, -6.000000000000000000 ) ) ;
#64573 = CARTESIAN_POINT ( 'NONE',  ( 4.999999999999999112, -10.41901085202107247, 40.68715046381925049 ) ) ;
#64574 = CARTESIAN_POINT ( 'NONE',  ( -93.84685191531247028, -211.9973110713294489, 88.10822916753382117 ) ) ;
#64575 = ORIENTED_EDGE ( 'NONE', *, *, #15651, .T. ) ;
#64576 = AXIS2_PLACEMENT_3D ( 'NONE', #63537, #46977, #12014 ) ;
#64577 = DIRECTION ( 'NONE',  ( -0.6064928550163533050, -0.7950889364178781449, 0.000000000000000000 ) ) ;
#64578 = EDGE_LOOP ( 'NONE', ( #17320, #8303, #66603, #17225 ) ) ;
#64579 = AXIS2_PLACEMENT_3D ( 'NONE', #3307, #37133, #14555 ) ;
#64580 = CIRCLE ( 'NONE', #4599, 16.00000000000000355 ) ;
#64581 = ORIENTED_EDGE ( 'NONE', *, *, #26993, .F. ) ;
#64582 = CARTESIAN_POINT ( 'NONE',  ( 5.000000000000000000, -26.79245525562690844, -32.34446384430000876 ) ) ;
#64583 = CARTESIAN_POINT ( 'NONE',  ( 93.67499999999998295, 92.29496732002878900, 86.71916666666666629 ) ) ;
#64584 = AXIS2_PLACEMENT_3D ( 'NONE', #43434, #43049, #37413 ) ;
#64585 = EDGE_CURVE ( 'NONE', #64719, #18846, #56143, .T. ) ;
#64586 = DIRECTION ( 'NONE',  ( 0.000000000000000000, 0.000000000000000000, 1.000000000000000000 ) ) ;
#64587 = CARTESIAN_POINT ( 'NONE',  ( 94.99999999999998579, 87.33691857156068750, 82.81656250086712134 ) ) ;
#64588 = PLANE ( 'NONE',  #67592 ) ;
#64589 = DIRECTION ( 'NONE',  ( -1.000000000000000000, 0.000000000000000000, 0.000000000000000000 ) ) ;
#64590 = DIRECTION ( 'NONE',  ( 0.6064928550163531940, 0.7950889364178782559, 0.000000000000000000 ) ) ;
#64591 = DIRECTION ( 'NONE',  ( 0.000000000000000000, 0.000000000000000000, 1.000000000000000000 ) ) ;
#64593 = EDGE_CURVE ( 'NONE', #70197, #32025, #5406, .T. ) ;
#64592 = LINE ( 'NONE', #71318, #12841 ) ;
#64594 = DIRECTION ( 'NONE',  ( -0.000000000000000000, -0.000000000000000000, 1.000000000000000000 ) ) ;
#64595 = DIRECTION ( 'NONE',  ( -1.000000000000000000, 0.000000000000000000, -0.000000000000000000 ) ) ;
#64596 =( BOUNDED_CURVE ( )  B_SPLINE_CURVE ( 2, ( #28705, #52001, #29804, #64412, #12150, #41471, #24190 ),
 .UNSPECIFIED., .F., .F. ) 
 B_SPLINE_CURVE_WITH_KNOTS ( ( 3, 2, 2, 3 ),
 ( 0.7499999999999996669, 0.7569444444444439757, 0.7638888888888883955, 0.7708333333333328152 ),
 .UNSPECIFIED. ) 
 CURVE ( )  GEOMETRIC_REPRESENTATION_ITEM ( )  RATIONAL_B_SPLINE_CURVE ( ( 1.000000000000006439, 0.8660254037844322683, 1.000000000000000000, 0.8660254037844387076, 1.000000000000000000, 0.8660254037844493658, 0.9999999999999893419 ) ) 
 REPRESENTATION_ITEM ( '' )  );
#64597 = EDGE_CURVE ( 'NONE', #35941, #48178, #23318, .T. ) ;
#64598 = CARTESIAN_POINT ( 'NONE',  ( 96.32499999999998863, -207.7050326799711968, 85.42270833506762528 ) ) ;
#64599 = FACE_OUTER_BOUND ( 'NONE', #68040, .T. ) ;
#64600 = CARTESIAN_POINT ( 'NONE',  ( -93.84685191531252713, 88.00268892867056536, 86.67947916753381321 ) ) ;
#64601 = LINE ( 'NONE', #30741, #43180 ) ;
#64602 = CIRCLE ( 'NONE', #26157, 30.50000000000000000 ) ;
#64603 = AXIS2_PLACEMENT_3D ( 'NONE', #63464, #29583, #30701 ) ;
#64604 = EDGE_CURVE ( 'NONE', #4428, #74042, #50497, .T. ) ;
#64605 = VECTOR ( 'NONE', #31661, 1000.000000000000000 ) ;
#64606 = DIRECTION ( 'NONE',  ( 0.000000000000000000, 0.000000000000000000, -1.000000000000000000 ) ) ;
#64607 = ADVANCED_FACE ( 'NONE', ( #21932 ), #22683, .T. ) ;
#64608 = VERTEX_POINT ( 'NONE', #33951 ) ;
#64609 = AXIS2_PLACEMENT_3D ( 'NONE', #44826, #5724, #33521 ) ;
#64610 = CARTESIAN_POINT ( 'NONE',  ( 15.00000000000000000, 20.85821328998756385, 10.92862929874494249 ) ) ;
#64611 = CARTESIAN_POINT ( 'NONE',  ( 10.00000000000000000, 18.89407956138362010, -75.16055320797013906 ) ) ;
#64612 = DIRECTION ( 'NONE',  ( 0.000000000000000000, -0.4539904997395542430, 0.8910065241883641241 ) ) ;
#64613 = CARTESIAN_POINT ( 'NONE',  ( 15.00000000000000000, -22.32062822937469093, 14.36278369418830181 ) ) ;
#64614 = EDGE_CURVE ( 'NONE', #19224, #11648, #56529, .T. ) ;
#64615 = ADVANCED_FACE ( 'NONE', ( #4662 ), #51237, .T. ) ;
#64616 = CARTESIAN_POINT ( 'NONE',  ( 93.84685191531251292, -211.9973110713294489, 81.01739583420049939 ) ) ;
#64617 = ORIENTED_EDGE ( 'NONE', *, *, #25121, .F. ) ;
#64618 = VERTEX_POINT ( 'NONE', #4291 ) ;
#64619 = DIRECTION ( 'NONE',  ( -1.000000000000000000, 0.000000000000000000, 0.000000000000000000 ) ) ;
#64620 = VERTEX_POINT ( 'NONE', #73791 ) ;
#64621 = LINE ( 'NONE', #40962, #65415 ) ;
#64622 = DIRECTION ( 'NONE',  ( -0.000000000000000000, -0.000000000000000000, 1.000000000000000000 ) ) ;
#64623 = ORIENTED_EDGE ( 'NONE', *, *, #24892, .T. ) ;
#64624 = CARTESIAN_POINT ( 'NONE',  ( 97.30629616937498838, -209.9999999999999716, 78.05406250086716113 ) ) ;
#64625 = CIRCLE ( 'NONE', #10634, 31.99999999999998934 ) ;
#64626 = ORIENTED_EDGE ( 'NONE', *, *, #37215, .T. ) ;
#64627 = DIRECTION ( 'NONE',  ( 0.000000000000000000, 0.000000000000000000, 1.000000000000000000 ) ) ;
#64628 = VERTEX_POINT ( 'NONE', #50108 ) ;
#64629 = ORIENTED_EDGE ( 'NONE', *, *, #19247, .F. ) ;
#64630 = CARTESIAN_POINT ( 'NONE',  ( 10.00000000000000000, 0.000000000000000000, 0.000000000000000000 ) ) ;
#64631 = CIRCLE ( 'NONE', #43016, 31.99999999999998579 ) ;
#64632 =( LENGTH_UNIT ( ) NAMED_UNIT ( * ) SI_UNIT ( .MILLI., .METRE. ) );
#64633 = DIRECTION ( 'NONE',  ( 0.9038112904824853189, -0.4279312458752977388, 0.000000000000000000 ) ) ;
#64634 = CIRCLE ( 'NONE', #50179, 37.49900000000000233 ) ;
#64635 = ORIENTED_EDGE ( 'NONE', *, *, #26509, .T. ) ;
#64636 = DIRECTION ( 'NONE',  ( -0.000000000000000000, -0.000000000000000000, 1.000000000000000000 ) ) ;
#64637 = CARTESIAN_POINT ( 'NONE',  ( 92.35000000000000853, -209.9999999999999716, 83.72937500173429726 ) ) ;
#64638 = CARTESIAN_POINT ( 'NONE',  ( 92.34999999999999432, 90.00000000000002842, 88.73000000000000398 ) ) ;
#64639 = ORIENTED_EDGE ( 'NONE', *, *, #16752, .F. ) ;
#64640 = CARTESIAN_POINT ( 'NONE',  ( 0.000000000000000000, 36.13751322684449008, -21.40280677340332716 ) ) ;
#64641 = FACE_OUTER_BOUND ( 'NONE', #27444, .T. ) ;
#64642 = ORIENTED_EDGE ( 'NONE', *, *, #17425, .T. ) ;
#64643 = ORIENTED_EDGE ( 'NONE', *, *, #35303, .T. ) ;
#64644 = CARTESIAN_POINT ( 'NONE',  ( -96.15314808468752972, 91.99731107132950569, 87.15572916753382060 ) ) ;
#64645 = EDGE_LOOP ( 'NONE', ( #49947, #35137, #46922, #58846 ) ) ;
#64646 = CARTESIAN_POINT ( 'NONE',  ( 92.34999999999999432, 88.47002178664753558, 86.32229166840097889 ) ) ;
#64647 = AXIS2_PLACEMENT_3D ( 'NONE', #15589, #8473, #32865 ) ;
#64648 = SURFACE_SIDE_STYLE ('',( #41710 ) ) ;
#64649 = ORIENTED_EDGE ( 'NONE', *, *, #19496, .T. ) ;
#64650 = CARTESIAN_POINT ( 'NONE',  ( 10.00000000000000000, 41.81611651403867569, -3.925862922255714871 ) ) ;
#64651 = DIRECTION ( 'NONE',  ( 1.000000000000000000, -0.000000000000000000, -0.000000000000000000 ) ) ;
#64652 = ORIENTED_EDGE ( 'NONE', *, *, #52908, .F. ) ;
#64653 = CIRCLE ( 'NONE', #13009, 21.00000000000000000 ) ;
#64654 = ORIENTED_EDGE ( 'NONE', *, *, #27120, .T. ) ;
#64655 = VERTEX_POINT ( 'NONE', #57262 ) ;
#64656 = FACE_OUTER_BOUND ( 'NONE', #55690, .T. ) ;
#64657 = CARTESIAN_POINT ( 'NONE',  ( 10.00000000000000000, -81.50828551894220197, -8.966570791701579779 ) ) ;
#64658 = VECTOR ( 'NONE', #44758, 1000.000000000000000 ) ;
#64659 = VECTOR ( 'NONE', #63964, 1000.000000000000000 ) ;
#64660 = CARTESIAN_POINT ( 'NONE',  ( -97.65000000000001990, 91.52997821335253548, 89.31208333333333371 ) ) ;
#64661 = EDGE_LOOP ( 'NONE', ( #5212, #38825, #3458, #24615 ) ) ;
#64662 = DIRECTION ( 'NONE',  ( -1.000000000000000000, -0.000000000000000000, 0.000000000000000000 ) ) ;
#64663 = EDGE_CURVE ( 'NONE', #22671, #23737, #65, .T. ) ;
#64664 = DIRECTION ( 'NONE',  ( 1.000000000000000000, 0.000000000000000000, 0.000000000000000000 ) ) ;
#64665 = ORIENTED_EDGE ( 'NONE', *, *, #8653, .T. ) ;
#64666 = CARTESIAN_POINT ( 'NONE',  ( 95.00000000000000000, -213.0599564267049857, 85.07875000000001364 ) ) ;
#64667 = CARTESIAN_POINT ( 'NONE',  ( -92.69370383062498320, -208.6684592857803011, 81.75822916753381264 ) ) ;
#64668 = VERTEX_POINT ( 'NONE', #5767 ) ;
#64669 = DIRECTION ( 'NONE',  ( -0.9827303690289279636, -0.1850432970638682117, 0.000000000000000000 ) ) ;
#64670 = CYLINDRICAL_SURFACE ( 'NONE', #54802, 31.99999999999999289 ) ;
#64671 = DIRECTION ( 'NONE',  ( 0.000000000000000000, 0.000000000000000000, 1.000000000000000000 ) ) ;
#64672 = CYLINDRICAL_SURFACE ( 'NONE', #60302, 16.00000000000000000 ) ;
#64673 = PRODUCT_RELATED_PRODUCT_CATEGORY ( 'part', '', ( #68031 ) ) ;
#64674 = EDGE_CURVE ( 'NONE', #7335, #36701, #31064, .T. ) ;
#64675 = DIRECTION ( 'NONE',  ( -0.000000000000000000, -0.000000000000000000, -1.000000000000000000 ) ) ;
#64676 = ADVANCED_FACE ( 'NONE', ( #33198 ), #45630, .T. ) ;
#64677 = DIRECTION ( 'NONE',  ( 0.000000000000000000, 0.6691306063588569053, 0.7431448254773954654 ) ) ;
#64678 = CYLINDRICAL_SURFACE ( 'NONE', #12035, 82.00000000000000000 ) ;
#64679 = CARTESIAN_POINT ( 'NONE',  ( -7.499999999999969802, 76.29999999999999716, -255.0000000000000000 ) ) ;
#64680 = CARTESIAN_POINT ( 'NONE',  ( 0.000000000000000000, 63.97538442413426907, 51.29473840253246664 ) ) ;
#64682 = ADVANCED_FACE ( 'NONE', ( #39972 ), #73042, .T. ) ;
#64681 = CARTESIAN_POINT ( 'NONE',  ( -97.64999999996709334, -209.9999916080759306, 86.90410584369134028 ) ) ;
#64683 = CARTESIAN_POINT ( 'NONE',  ( -96.15314808468752972, 91.99731107132950569, 89.69572916753382685 ) ) ;
#64684 = DIRECTION ( 'NONE',  ( 0.000000000000000000, -0.3090169943749349057, -0.9510565162951577500 ) ) ;
#64685 = CARTESIAN_POINT ( 'NONE',  ( 0.000000000000000000, -120.0000000000000000, 40.00000000000000711 ) ) ;
#64686 = EDGE_CURVE ( 'NONE', #17385, #21499, #20283, .T. ) ;
#64687 = AXIS2_PLACEMENT_3D ( 'NONE', #5485, #58436, #23493 ) ;
#64688 = CARTESIAN_POINT ( 'NONE',  ( 10.00000000000000000, 21.53537804866081373, 30.80686688397018358 ) ) ;
#64689 = CIRCLE ( 'NONE', #74293, 77.49900000000000944 ) ;
#64690 = CARTESIAN_POINT ( 'NONE',  ( 11.99999999999999822, -55.16347631943085617, 60.67117009219116852 ) ) ;
#64691 = DIRECTION ( 'NONE',  ( 0.000000000000000000, 0.000000000000000000, 1.000000000000000000 ) ) ;
#64693 = AXIS2_PLACEMENT_3D ( 'NONE', #102, #46284, #1208 ) ;
#64692 = CARTESIAN_POINT ( 'NONE',  ( 0.000000000000000000, 81.34940948281337114, 10.30890764327411446 ) ) ;
#64694 = CARTESIAN_POINT ( 'NONE',  ( 95.04693102382874770, -212.6495843973424940, 75.00000002508419072 ) ) ;
#64695 = CARTESIAN_POINT ( 'NONE',  ( -10.00000000000000000, 0.000000000000000000, 0.000000000000000000 ) ) ;
#64696 = CARTESIAN_POINT ( 'NONE',  ( -93.33920801875063944, -211.6002412367801071, 74.80065669543250806 ) ) ;
#64697 = AXIS2_PLACEMENT_3D ( 'NONE', #43633, #71061, #36859 ) ;
#64698 = EDGE_CURVE ( 'NONE', #23222, #19226, #50273, .T. ) ;
#64699 = LINE ( 'NONE', #70680, #6183 ) ;
#64700 = EDGE_CURVE ( 'NONE', #43660, #46588, #6501, .T. ) ;
#64701 = ORIENTED_EDGE ( 'NONE', *, *, #59580, .T. ) ;
#64702 = DIRECTION ( 'NONE',  ( -1.000000000000000000, 0.000000000000000000, 0.000000000000000000 ) ) ;
#64703 = CARTESIAN_POINT ( 'NONE',  ( 93.67500000000001137, -212.2949673200287179, 88.20083333333332121 ) ) ;
#64705 = CARTESIAN_POINT ( 'NONE',  ( 0.000000000000000000, 37.16516213103277266, 4.992566952385114831 ) ) ;
#64704 = VECTOR ( 'NONE', #50885, 1000.000000000000000 ) ;
#64706 = DIRECTION ( 'NONE',  ( 1.000000000000000000, -0.000000000000000000, -0.000000000000000000 ) ) ;
#64707 = VECTOR ( 'NONE', #72138, 1000.000000000000000 ) ;
#64708 = CIRCLE ( 'NONE', #29918, 3.299999999999969624 ) ;
#64710 = DIRECTION ( 'NONE',  ( 0.6575728627325954090, -0.7533909544171998318, 0.000000000000000000 ) ) ;
#64709 = CIRCLE ( 'NONE', #1158, 37.49900000000000233 ) ;
#64711 = ORIENTED_EDGE ( 'NONE', *, *, #71300, .T. ) ;
#64712 = AXIS2_PLACEMENT_3D ( 'NONE', #57216, #68118, #17354 ) ;
#64713 = CARTESIAN_POINT ( 'NONE',  ( 6.000000000000000000, 79.10210256391398786, -21.60688246758503794 ) ) ;
#64714 = DIRECTION ( 'NONE',  ( -1.000000000000000000, 0.000000000000000000, 0.000000000000000000 ) ) ;
#64715 = ORIENTED_EDGE ( 'NONE', *, *, #57494, .T. ) ;
#64716 = VECTOR ( 'NONE', #37809, 1000.000000000000114 ) ;
#64717 = CARTESIAN_POINT ( 'NONE',  ( 92.69370383062501162, -208.6684592857803295, 85.77989583420048803 ) ) ;
#64718 = CARTESIAN_POINT ( 'NONE',  ( 97.30629616937498838, -208.6684592857803295, 86.99697916753382287 ) ) ;
#64719 = VERTEX_POINT ( 'NONE', #69277 ) ;
#64720 = CARTESIAN_POINT ( 'NONE',  ( 96.15314808468748708, -208.0026889286704943, 89.58989583420049030 ) ) ;
#64721 = EDGE_LOOP ( 'NONE', ( #66047, #17211, #3641, #13294 ) ) ;
#64722 = FACE_BOUND ( 'NONE', #7196, .T. ) ;
#64723 = ORIENTED_EDGE ( 'NONE', *, *, #8347, .F. ) ;
#64724 = CARTESIAN_POINT ( 'NONE',  ( -93.84685191531254134, 91.99731107132950569, 80.06489583420048461 ) ) ;
#64725 = VERTEX_POINT ( 'NONE', #57997 ) ;
#64726 = ORIENTED_EDGE ( 'NONE', *, *, #19287, .F. ) ;
#64727 = CARTESIAN_POINT ( 'NONE',  ( 23.11608002360578240, -124.4885236261218182, 5.500000000000000000 ) ) ;
#64728 =( BOUNDED_CURVE ( )  B_SPLINE_CURVE ( 2, ( #73743, #45579, #63234, #50064, #4614, #50812, #28254, #45199, #6095 ),
 .UNSPECIFIED., .F., .F. ) 
 B_SPLINE_CURVE_WITH_KNOTS ( ( 3, 2, 2, 2, 3 ),
 ( 0.5715170088666297055, 0.5785727743523534361, 0.5856285398932350450, 0.5926843054341167649, 0.5926843883797354717 ),
 .UNSPECIFIED. ) 
 CURVE ( )  GEOMETRIC_REPRESENTATION_ITEM ( )  RATIONAL_B_SPLINE_CURVE ( ( 1.000000000000000000, 0.8660254037844387076, 1.000000000000000000, 0.8660254037844387076, 1.000000000000000000, 0.8660254037844387076, 1.000000000000000000, 0.9999984250318816326, 0.9999968501007930888 ) ) 
 REPRESENTATION_ITEM ( '' )  );
#64729 = VERTEX_POINT ( 'NONE', #57641 ) ;
#64730 = DIRECTION ( 'NONE',  ( -1.000000000000000000, -0.000000000000000000, -0.000000000000000000 ) ) ;
#64731 =( LENGTH_UNIT ( ) NAMED_UNIT ( * ) SI_UNIT ( .MILLI., .METRE. ) );
#64732 = AXIS2_PLACEMENT_3D ( 'NONE', #54214, #72582, #25269 ) ;
#64733 = VERTEX_POINT ( 'NONE', #7238 ) ;
#64734 = CARTESIAN_POINT ( 'NONE',  ( 10.00000000000000000, -65.58780272294100655, 36.73666225445870737 ) ) ;
#64735 = EDGE_LOOP ( 'NONE', ( #24791, #37515, #38855, #6767 ) ) ;
#64736 = DIRECTION ( 'NONE',  ( -1.000000000000000000, 0.000000000000000000, -0.000000000000000000 ) ) ;
#64737 = AXIS2_PLACEMENT_3D ( 'NONE', #902, #12131, #12502 ) ;
#64738 = VECTOR ( 'NONE', #62992, 1000.000000000000000 ) ;
#64739 = ORIENTED_EDGE ( 'NONE', *, *, #14142, .F. ) ;
#64740 = ADVANCED_FACE ( 'NONE', ( #29401 ), #53464, .T. ) ;
#64741 = AXIS2_PLACEMENT_3D ( 'NONE', #48780, #2225, #71328 ) ;
#64742 = CIRCLE ( 'NONE', #7275, 15.99999999999999822 ) ;
#64743 = ORIENTED_EDGE ( 'NONE', *, *, #73169, .T. ) ;
#64744 = ORIENTED_EDGE ( 'NONE', *, *, #72896, .T. ) ;
#64745 = CARTESIAN_POINT ( 'NONE',  ( 93.84685191531249870, -208.0026889286704943, 81.91697916753381037 ) ) ;
#64746 = DIRECTION ( 'NONE',  ( -1.000000000000000000, 0.000000000000000000, -0.000000000000000000 ) ) ;
#64747 = CARTESIAN_POINT ( 'NONE',  ( 10.00000000000000000, 0.000000000000000000, 0.000000000000000000 ) ) ;
#64748 = DIRECTION ( 'NONE',  ( -1.000000000000000000, -0.000000000000000000, 0.000000000000000000 ) ) ;
#64749 = VECTOR ( 'NONE', #8947, 1000.000000000000000 ) ;
#64750 = DIRECTION ( 'NONE',  ( 0.000000000000000000, 0.000000000000000000, 1.000000000000000000 ) ) ;
#64751 = EDGE_CURVE ( 'NONE', #24954, #16487, #71902, .T. ) ;
#64752 = CARTESIAN_POINT ( 'NONE',  ( 10.00000000000000000, -39.78640506895559525, -66.50666863322042843 ) ) ;
#64753 = CARTESIAN_POINT ( 'NONE',  ( 0.000000000000000000, 0.000000000000000000, -6.000000000000001776 ) ) ;
#64754 = CARTESIAN_POINT ( 'NONE',  ( -92.69370383062498320, -209.9999999999999716, 82.97531250086714749 ) ) ;
#64755 = EDGE_CURVE ( 'NONE', #36601, #18028, #14275, .T. ) ;
#64756 = CARTESIAN_POINT ( 'NONE',  ( -97.30629616937501680, 91.33154071421968467, 84.03364583420049883 ) ) ;
#64757 = ORIENTED_EDGE ( 'NONE', *, *, #70883, .F. ) ;
#64758 = CARTESIAN_POINT ( 'NONE',  ( 97.30629616937498838, 88.66845928578037217, 80.38239583420049428 ) ) ;
#64759 = VERTEX_POINT ( 'NONE', #24888 ) ;
#64760 = DIRECTION ( 'NONE',  ( -0.000000000000000000, -0.000000000000000000, 1.000000000000000000 ) ) ;
#64761 = DIRECTION ( 'NONE',  ( 0.000000000000000000, 0.9876883405951371042, 0.1564344650402346437 ) ) ;
#64762 = CARTESIAN_POINT ( 'NONE',  ( -92.34999999999999432, -211.5299782133524218, 83.35895833506764063 ) ) ;
#64763 = LINE ( 'NONE', #54584, #64371 ) ;
#64764 = DIRECTION ( 'NONE',  ( 0.000000000000000000, -0.9510565162951507556, 0.3090169943749561110 ) ) ;
#64765 = CARTESIAN_POINT ( 'NONE',  ( -94.99999999999997158, -207.3369185715606307, 81.86406250086713499 ) ) ;
#64766 = DIRECTION ( 'NONE',  ( 0.000000000000000000, 0.000000000000000000, 1.000000000000000000 ) ) ;
#64767 = EDGE_CURVE ( 'NONE', #55701, #25862, #2354, .T. ) ;
#64768 = CIRCLE ( 'NONE', #31141, 82.00000000000000000 ) ;
#64769 = CARTESIAN_POINT ( 'NONE',  ( -42.50000000000000000, 1.932465207890948911E-15, 15.77977592589476608 ) ) ;
#64770 = CARTESIAN_POINT ( 'NONE',  ( 97.64999999999999147, 90.00000000000002842, 78.88750000000000284 ) ) ;
#64771 = LINE ( 'NONE', #23798, #96 ) ;
#64772 = ORIENTED_EDGE ( 'NONE', *, *, #43746, .F. ) ;
#64773 = VECTOR ( 'NONE', #57344, 999.9999999999998863 ) ;
#64774 = AXIS2_PLACEMENT_3D ( 'NONE', #65682, #14161, #49490 ) ;
#64775 = ORIENTED_EDGE ( 'NONE', *, *, #7744, .F. ) ;
#64776 = CONICAL_SURFACE ( 'NONE', #74315, 12.83284365640956182, 0.3490658503988688377 ) ;
#64777 = CIRCLE ( 'NONE', #32328, 82.00000000000000000 ) ;
#64778 = DIRECTION ( 'NONE',  ( -1.000000000000000000, -0.000000000000000000, -0.000000000000000000 ) ) ;
#64779 = CARTESIAN_POINT ( 'NONE',  ( 0.000000000000000000, -22.90783923731575911, -78.73519480814978522 ) ) ;
#64780 = CARTESIAN_POINT ( 'NONE',  ( -97.30629616937501680, 91.33154071421968467, 88.31989583420046586 ) ) ;
#64781 = LINE ( 'NONE', #47842, #74231 ) ;
#64782 = FACE_OUTER_BOUND ( 'NONE', #41334, .T. ) ;
#64783 =( REPRESENTATION_RELATIONSHIP ('NONE','NONE', #31117, #50888 ) REPRESENTATION_RELATIONSHIP_WITH_TRANSFORMATION ( #15071 )SHAPE_REPRESENTATION_RELATIONSHIP( ) );
#64784 = DIRECTION ( 'NONE',  ( 0.000000000000000000, 0.000000000000000000, 1.000000000000000000 ) ) ;
#64785 = DIRECTION ( 'NONE',  ( 0.000000000000000000, 0.6494480483301849905, -0.7604059656000299317 ) ) ;
#64786 = ADVANCED_FACE ( 'NONE', ( #35785 ), #53097, .T. ) ;
#64787 = EDGE_LOOP ( 'NONE', ( #29020, #67532, #47701, #20268 ) ) ;
#64788 = CARTESIAN_POINT ( 'NONE',  ( -95.00000000000002842, 92.66308142843932671, 74.87906250086713555 ) ) ;
#64789 = CARTESIAN_POINT ( 'NONE',  ( 1.250000000000000000, -12.36245420541525597, -1.199999999999999956 ) ) ;
#64790 = DIRECTION ( 'NONE',  ( -1.000000000000000000, 0.000000000000000000, -0.000000000000000000 ) ) ;
#64791 = CARTESIAN_POINT ( 'NONE',  ( 92.35000000000000853, -208.4700217866474645, 84.31145833506762699 ) ) ;
#64792 = CARTESIAN_POINT ( 'NONE',  ( -11.70000000000000107, 2.535018874235021196E-15, 20.69999999999999929 ) ) ;
#64793 = CARTESIAN_POINT ( 'NONE',  ( -96.15314808468747287, -208.0026889286704943, 86.52072916753382970 ) ) ;
#64794 =( NAMED_UNIT ( * ) SI_UNIT ( $, .STERADIAN. ) SOLID_ANGLE_UNIT ( ) );
#64795 = EDGE_CURVE ( 'NONE', #9779, #34381, #69503, .T. ) ;
#64796 = LINE ( 'NONE', #20015, #37692 ) ;
#64797 = EDGE_CURVE ( 'NONE', #71422, #28318, #55114, .T. ) ;
#64798 = VECTOR ( 'NONE', #7393, 1000.000000000000000 ) ;
#64799 = EDGE_CURVE ( 'NONE', #4573, #9802, #69977, .T. ) ;
#64800 = DIRECTION ( 'NONE',  ( -0.000000000000000000, -0.000000000000000000, 1.000000000000000000 ) ) ;
#64801 = AXIS2_PLACEMENT_3D ( 'NONE', #37762, #44517, #60696 ) ;
#64802 = CARTESIAN_POINT ( 'NONE',  ( -97.30629616937497417, -208.6684592857803295, 77.68364583420047609 ) ) ;
#64803 = CARTESIAN_POINT ( 'NONE',  ( 94.99999999999998579, 93.05995642670504253, 88.57124999999999204 ) ) ;
#64804 = VERTEX_POINT ( 'NONE', #40711 ) ;
#64805 = CARTESIAN_POINT ( 'NONE',  ( 97.64999999999999147, 89.99999996655866141, 87.85687500050293863 ) ) ;
#64806 = CARTESIAN_POINT ( 'NONE',  ( -94.99999999999997158, -209.9999999999999716, 90.00000000000000000 ) ) ;
#64807 = AXIS2_PLACEMENT_3D ( 'NONE', #13972, #36539, #2385 ) ;
#64808 = DIRECTION ( 'NONE',  ( -1.000000000000000000, 0.000000000000000000, 0.000000000000000000 ) ) ;
#64809 = CIRCLE ( 'NONE', #32365, 62.50000000000000000 ) ;
#64810 = CARTESIAN_POINT ( 'NONE',  ( -26.53422223201112828, -120.6595836127786043, 2.500000000000000000 ) ) ;
#64811 = CARTESIAN_POINT ( 'NONE',  ( 97.30629616937498838, -208.6684592857803011, 76.04322916753380923 ) ) ;
#64812 = VERTEX_POINT ( 'NONE', #47818 ) ;
#64813 = CARTESIAN_POINT ( 'NONE',  ( 10.00000000000000000, -37.22597642581153821, 10.79786254984320415 ) ) ;
#64814 = CARTESIAN_POINT ( 'NONE',  ( 0.000000000000000000, 0.000000000000000000, 0.000000000000000000 ) ) ;
#64815 = ORIENTED_EDGE ( 'NONE', *, *, #70494, .T. ) ;
#64816 = DIRECTION ( 'NONE',  ( 0.000000000000000000, 0.000000000000000000, 1.000000000000000000 ) ) ;
#64817 = ORIENTED_EDGE ( 'NONE', *, *, #5543, .F. ) ;
#64818 = CIRCLE ( 'NONE', #46787, 62.50000000000000000 ) ;
#64819 = VECTOR ( 'NONE', #53567, 1000.000000000000000 ) ;
#64820 = ORIENTED_EDGE ( 'NONE', *, *, #9020, .F. ) ;
#64821 = ORIENTED_EDGE ( 'NONE', *, *, #9319, .T. ) ;
#64822 = CIRCLE ( 'NONE', #35993, 82.00000000000000000 ) ;
#64823 = VERTEX_POINT ( 'NONE', #18868 ) ;
#64824 = VECTOR ( 'NONE', #36029, 1000.000000000000114 ) ;
#64825 = CARTESIAN_POINT ( 'NONE',  ( 15.00000000000000000, 22.07842321921492612, 8.187992925817123790 ) ) ;
#64826 = ORIENTED_EDGE ( 'NONE', *, *, #11426, .T. ) ;
#64827 = EDGE_LOOP ( 'NONE', ( #27000, #24585, #67686, #66775 ) ) ;
#64828 =( BOUNDED_CURVE ( )  B_SPLINE_CURVE ( 2, ( #19769, #66398, #55477, #31786, #8872, #2544, #3988, #71641, #43840 ),
 .UNSPECIFIED., .F., .F. ) 
 B_SPLINE_CURVE_WITH_KNOTS ( ( 3, 2, 2, 2, 3 ),
 ( 0.4021785743327777052, 0.4021786358302963382, 0.4092344013711782802, 0.4162901669120601666, 0.4233457466685772164 ),
 .UNSPECIFIED. ) 
 CURVE ( )  GEOMETRIC_REPRESENTATION_ITEM ( )  RATIONAL_B_SPLINE_CURVE ( ( 0.9999976645954666843, 0.9999988322875555946, 1.000000000000000000, 0.8660254037844387076, 1.000000000000000000, 0.8660254037844387076, 1.000000000000000000, 0.8660289314505905667, 0.9999929448534692344 ) ) 
 REPRESENTATION_ITEM ( '' )  );
#64829 = CARTESIAN_POINT ( 'NONE',  ( 94.99999999999998579, 92.66308142843935514, 80.75281250086715090 ) ) ;
#64830 = CARTESIAN_POINT ( 'NONE',  ( 18.80329974962065265, -105.8248132807389084, 5.500000000000000000 ) ) ;
#64831 = CARTESIAN_POINT ( 'NONE',  ( 93.67500000000001137, -207.7050326799711968, 75.92416666666666458 ) ) ;
#64832 = ORIENTED_EDGE ( 'NONE', *, *, #17384, .T. ) ;
#64833 = ORIENTED_EDGE ( 'NONE', *, *, #8897, .F. ) ;
#64834 = ADVANCED_FACE ( 'NONE', ( #36166 ), #63654, .T. ) ;
#64835 = EDGE_LOOP ( 'NONE', ( #35139, #22777, #53086, #72473 ) ) ;
#64836 = CARTESIAN_POINT ( 'NONE',  ( 11.99999999999999822, -51.02545421589363883, 55.20638768913742922 ) ) ;
#64837 = ORIENTED_EDGE ( 'NONE', *, *, #14862, .T. ) ;
#64838 = DIRECTION ( 'NONE',  ( 0.000000000000000000, 0.000000000000000000, 1.000000000000000000 ) ) ;
#64839 = LINE ( 'NONE', #60318, #1943 ) ;
#64840 = CARTESIAN_POINT ( 'NONE',  ( -95.67252605959640732, 92.31128197830616955, 74.85222950654855367 ) ) ;
#64841 = FACE_OUTER_BOUND ( 'NONE', #67012, .T. ) ;
#64842 = DIRECTION ( 'NONE',  ( 0.000000000000000000, -0.9510565162951500895, -0.3090169943749581649 ) ) ;
#64843 = EDGE_CURVE ( 'NONE', #4256, #36714, #3709, .T. ) ;
#64844 = CARTESIAN_POINT ( 'NONE',  ( -92.34999999999992326, 88.47002178664760663, 78.19958333333332234 ) ) ;
#64845 = PLANE ( 'NONE',  #27219 ) ;
#64846 = CARTESIAN_POINT ( 'NONE',  ( -97.64999999999996305, -209.9999999999999716, 78.64937500173429896 ) ) ;
#64847 = EDGE_CURVE ( 'NONE', #33390, #46803, #64018, .T. ) ;
#64848 = DIRECTION ( 'NONE',  ( -1.000000000000000000, -0.000000000000000000, 0.000000000000000000 ) ) ;
#64850 = CARTESIAN_POINT ( 'NONE',  ( -97.65000000000001990, 90.00000000000004263, 76.10937500173430692 ) ) ;
#64849 = CARTESIAN_POINT ( 'NONE',  ( 96.32499999999998863, 87.70503267997126784, 75.05104166840095559 ) ) ;
#64851 = VERTEX_POINT ( 'NONE', #34688 ) ;
#64852 = CARTESIAN_POINT ( 'NONE',  ( 97.30629616937498838, 91.33154071421968467, 76.83697916753382628 ) ) ;
#64853 = CARTESIAN_POINT ( 'NONE',  ( 22.94323693612312809, -114.6983135802921083, -5.500000000000000000 ) ) ;
#64854 = DIRECTION ( 'NONE',  ( 0.000000000000000000, -0.9876883405951359940, -0.1564344650402420545 ) ) ;
#64855 = CARTESIAN_POINT ( 'NONE',  ( 95.00000000000000000, -209.9999999999999716, 90.00000000000000000 ) ) ;
#64856 = CARTESIAN_POINT ( 'NONE',  ( 97.65000000000000568, -211.5299782133524218, 77.64395833506762301 ) ) ;
#64857 = CARTESIAN_POINT ( 'NONE',  ( 15.00000000000000000, -13.04903810567646971, 19.60159698893442481 ) ) ;
#64858 = EDGE_CURVE ( 'NONE', #4038, #17670, #32368, .T. ) ;
#64859 = AXIS2_PLACEMENT_3D ( 'NONE', #46014, #23447, #6528 ) ;
#64860 = ORIENTED_EDGE ( 'NONE', *, *, #17808, .T. ) ;
#64861 = DIRECTION ( 'NONE',  ( 0.000000000000000000, 0.000000000000000000, 1.000000000000000000 ) ) ;
#64862 = LINE ( 'NONE', #13341, #27558 ) ;
#64863 = VERTEX_POINT ( 'NONE', #26365 ) ;
#64864 = ORIENTED_EDGE ( 'NONE', *, *, #71287, .F. ) ;
#64865 = AXIS2_PLACEMENT_3D ( 'NONE', #5966, #67613, #61606 ) ;
#64866 = CARTESIAN_POINT ( 'NONE',  ( 0.000000000000000000, 65.64334221924909230, 41.19522573413756561 ) ) ;
#64868 = EDGE_CURVE ( 'NONE', #23851, #67138, #71844, .T. ) ;
#64867 = CARTESIAN_POINT ( 'NONE',  ( 0.000000000000000000, 35.92658777277525672, -10.74501242461245809 ) ) ;
#64869 = CARTESIAN_POINT ( 'NONE',  ( 10.00000000000000000, 68.67312586194995561, 35.91791733033500122 ) ) ;
#64870 = CARTESIAN_POINT ( 'NONE',  ( 11.41210121379328335, -99.40233154247455616, 5.500000000000000000 ) ) ;
#64871 = CARTESIAN_POINT ( 'NONE',  ( -94.99999999999997158, -212.6630814284392557, 78.53031250086715431 ) ) ;
#64872 = ADVANCED_FACE ( 'NONE', ( #55311 ), #14348, .F. ) ;
#64873 = ORIENTED_EDGE ( 'NONE', *, *, #56901, .T. ) ;
#64874 = CARTESIAN_POINT ( 'NONE',  ( 10.00000000000000000, 15.48615015657638239, -39.04073710021328480 ) ) ;
#64875 = AXIS2_PLACEMENT_3D ( 'NONE', #45850, #29260, #46942 ) ;
#64876 = VECTOR ( 'NONE', #70359, 1000.000000000000000 ) ;
#64877 = CIRCLE ( 'NONE', #55086, 16.00000000000000000 ) ;
#64878 = DIRECTION ( 'NONE',  ( 0.000000000000000000, 0.000000000000000000, 1.000000000000000000 ) ) ;
#64879 = DIRECTION ( 'NONE',  ( 0.000000000000000000, -0.8090169943749402348, -0.5877852522924830181 ) ) ;
#64880 = CARTESIAN_POINT ( 'NONE',  ( -6.782329983125267248, 10.49999999999999645, -105.0000000000000000 ) ) ;
#64881 = CARTESIAN_POINT ( 'NONE',  ( -6.782329983125270800, 10.49999999999999467, 20.00000000000000000 ) ) ;
#64882 = DIRECTION ( 'NONE',  ( 0.000000000000000000, -0.6494480483301739993, -0.7604059656000390355 ) ) ;
#64883 = LINE ( 'NONE', #17895, #20512 ) ;
#64884 = AXIS2_PLACEMENT_3D ( 'NONE', #27080, #66938, #33848 ) ;
#64885 = DIRECTION ( 'NONE',  ( -1.000000000000000000, -0.000000000000000000, -0.000000000000000000 ) ) ;
#64886 = CIRCLE ( 'NONE', #68481, 42.00000000000000000 ) ;
#64887 = CARTESIAN_POINT ( 'NONE',  ( -92.34999999999999432, -208.4700217866474645, 77.74979166840097378 ) ) ;
#64888 = LINE ( 'NONE', #28243, #47831 ) ;
#64889 = EDGE_CURVE ( 'NONE', #56961, #70524, #59854, .T. ) ;
#64890 = EDGE_CURVE ( 'NONE', #45343, #66667, #49654, .T. ) ;
#64891 = CARTESIAN_POINT ( 'NONE',  ( 96.15314808468748708, 91.99731107132950569, 84.50989583420049200 ) ) ;
#64892 = CARTESIAN_POINT ( 'NONE',  ( -96.15314808468747287, -208.0026889286704943, 85.25072916753381946 ) ) ;
#64893 = DIRECTION ( 'NONE',  ( -1.000000000000000000, 0.000000000000000000, 0.000000000000000000 ) ) ;
#64894 = VERTEX_POINT ( 'NONE', #20723 ) ;
#64895 = CARTESIAN_POINT ( 'NONE',  ( 11.99999999999999822, -44.99326035066006568, -68.55367621811190304 ) ) ;
#64896 = CARTESIAN_POINT ( 'NONE',  ( -92.34999999999999432, -209.9999999999999716, 80.15749999999999886 ) ) ;
#64897 = CARTESIAN_POINT ( 'NONE',  ( -92.69370383062505425, 91.33154071421968467, 77.94822916753381037 ) ) ;
#64898 = CARTESIAN_POINT ( 'NONE',  ( 97.30629616937498838, -208.6684592857803011, 87.47322916753381605 ) ) ;
#64899 = ORIENTED_EDGE ( 'NONE', *, *, #70005, .F. ) ;
#64900 = ORIENTED_EDGE ( 'NONE', *, *, #46130, .T. ) ;
#64901 = ORIENTED_EDGE ( 'NONE', *, *, #58225, .T. ) ;
#64902 = CIRCLE ( 'NONE', #25301, 77.49900000000000944 ) ;
#64904 = AXIS2_PLACEMENT_3D ( 'NONE', #12616, #2127, #42320 ) ;
#64903 = CARTESIAN_POINT ( 'NONE',  ( 10.00000000000000000, -0.6853352020793173072, 37.58145647212453611 ) ) ;
#64905 = DIRECTION ( 'NONE',  ( 2.628368902995164490E-16, 1.000000000000000000, 0.000000000000000000 ) ) ;
#64906 = CIRCLE ( 'NONE', #45714, 31.99999999999998579 ) ;
#64907 = ORIENTED_EDGE ( 'NONE', *, *, #52728, .F. ) ;
#64908 = ORIENTED_EDGE ( 'NONE', *, *, #51096, .F. ) ;
#64909 = CARTESIAN_POINT ( 'NONE',  ( 11.59999999999999964, -0.8299999999999999600, -1.199999999999999956 ) ) ;
#64910 = CARTESIAN_POINT ( 'NONE',  ( 93.84685191531249870, -208.0026889286704943, 82.07572916753382231 ) ) ;
#64911 = CARTESIAN_POINT ( 'NONE',  ( 10.00000000000000000, -62.20884554313985149, -46.21855187248698371 ) ) ;
#64912 = CARTESIAN_POINT ( 'NONE',  ( 95.00000000000000000, -209.9999999999999716, 90.00000000000000000 ) ) ;
#64913 = FACE_OUTER_BOUND ( 'NONE', #54294, .T. ) ;
#64914 = CARTESIAN_POINT ( 'NONE',  ( -3.000000000000000000, -3.948201729842038432, -23.21447184625298021 ) ) ;
#64915 = CARTESIAN_POINT ( 'NONE',  ( 10.00000000000000000, -75.11725578898466438, -2.956366410621452001 ) ) ;
#64916 = CARTESIAN_POINT ( 'NONE',  ( 95.00000000000000000, -213.0599564267049857, 85.71374999999997613 ) ) ;
#64917 = EDGE_CURVE ( 'NONE', #53011, #14729, #32297, .T. ) ;
#64918 = VECTOR ( 'NONE', #34996, 1000.000000000000000 ) ;
#64919 = ORIENTED_EDGE ( 'NONE', *, *, #28240, .T. ) ;
#64920 = ORIENTED_EDGE ( 'NONE', *, *, #15615, .T. ) ;
#64921 = ORIENTED_EDGE ( 'NONE', *, *, #15449, .T. ) ;
#64922 = B_SPLINE_CURVE_WITH_KNOTS ( 'NONE', 3,
 ( #35905, #63768, #35537, #46838, #69754, #35175, #23899, #6968, #29889, #52092, #11496, #12239, #58473, #6608, #74286, #52455, #40081, #23525, #12606, #24274 ),
 .UNSPECIFIED., .F., .F.,
 ( 4, 2, 2, 2, 2, 2, 2, 2, 2, 4 ),
 ( 2.781148923622390442E-07, 0.0008372784139766601373, 0.001674278713060957900, 0.002511279012145256097, 0.003348279311229553860, 0.003766779460771703825, 0.004185279610313853357, 0.005022279909398152421, 0.005859280208482451485, 0.006696280507566749682 ),
 .UNSPECIFIED. ) ;
#64923 = ORIENTED_EDGE ( 'NONE', *, *, #65848, .T. ) ;
#64924 = DIRECTION ( 'NONE',  ( -1.000000000000000000, 0.000000000000000000, 0.000000000000000000 ) ) ;
#64925 = AXIS2_PLACEMENT_3D ( 'NONE', #57914, #5679, #51895 ) ;
#64926 = EDGE_CURVE ( 'NONE', #32262, #63489, #38019, .T. ) ;
#64927 = CIRCLE ( 'NONE', #2552, 31.99999999999998579 ) ;
#64928 = PRESENTATION_STYLE_ASSIGNMENT (( #6662 ) ) ;
#64929 = CARTESIAN_POINT ( 'NONE',  ( -97.30629616937501680, 88.66845928578038638, 87.31447916753381833 ) ) ;
#64930 = DIRECTION ( 'NONE',  ( 1.000000000000000000, 0.000000000000000000, 0.000000000000000000 ) ) ;
#64931 = AXIS2_PLACEMENT_3D ( 'NONE', #48248, #70412, #54624 ) ;
#64932 = CARTESIAN_POINT ( 'NONE',  ( -92.34999999999998010, 88.47002178664759242, 83.91458333333333997 ) ) ;
#64933 = CARTESIAN_POINT ( 'NONE',  ( 92.69370383062501162, -211.3315407142195852, 87.15572916753380639 ) ) ;
#64934 = EDGE_CURVE ( 'NONE', #60240, #26714, #3513, .T. ) ;
#64935 = LINE ( 'NONE', #32166, #34707 ) ;
#64936 = ORIENTED_EDGE ( 'NONE', *, *, #14016, .T. ) ;
#64937 = CARTESIAN_POINT ( 'NONE',  ( -97.64999999999996305, -209.9999999999999716, 88.80937500173430976 ) ) ;
#64938 = EDGE_LOOP ( 'NONE', ( #69242, #27531, #17142, #36810, #57003 ) ) ;
#64939 = CARTESIAN_POINT ( 'NONE',  ( 5.999999999999999112, -63.97538442413390669, -51.29473840253292138 ) ) ;
#64940 = EDGE_LOOP ( 'NONE', ( #38793, #40832, #40787, #55563 ) ) ;
#64941 = CARTESIAN_POINT ( 'NONE',  ( -95.00000000000002842, 86.94004357329504273, 85.79312500173431033 ) ) ;
#64942 = CARTESIAN_POINT ( 'NONE',  ( 97.30629616937498838, 88.66845928578037217, 88.79614583420050167 ) ) ;
#64943 = CARTESIAN_POINT ( 'NONE',  ( -9.332068499558245023, 6.890028847512374988, 52.00000000000002132 ) ) ;
#64944 = CARTESIAN_POINT ( 'NONE',  ( 4.999999999999999112, -3.925862922255855647, -41.81611651403866858 ) ) ;
#64945 = CARTESIAN_POINT ( 'NONE',  ( -97.64999999989191792, -209.9999848944890175, 78.64888723590522090 ) ) ;
#64946 = EDGE_CURVE ( 'NONE', #4178, #464, #59478, .T. ) ;
#64947 = DIRECTION ( 'NONE',  ( 0.000000000000000000, -0.7604059656000369261, 0.6494480483301766638 ) ) ;
#64948 = VERTEX_POINT ( 'NONE', #25629 ) ;
#64949 = DIRECTION ( 'NONE',  ( 1.000000000000000000, 0.000000000000000000, 0.000000000000000000 ) ) ;
#64950 = CARTESIAN_POINT ( 'NONE',  ( -92.35000000000553655, 89.99999459739531460, 81.50687481489494246 ) ) ;
#64951 = ORIENTED_EDGE ( 'NONE', *, *, #30115, .T. ) ;
#64952 = VERTEX_POINT ( 'NONE', #71477 ) ;
#64953 = LINE ( 'NONE', #30713, #72150 ) ;
#64954 = DIRECTION ( 'NONE',  ( -1.000000000000000000, 0.000000000000000000, 0.000000000000000000 ) ) ;
#64955 = ADVANCED_FACE ( 'NONE', ( #21081, #14712 ), #43679, .T. ) ;
#64956 = FACE_OUTER_BOUND ( 'NONE', #6119, .T. ) ;
#64957 = CARTESIAN_POINT ( 'NONE',  ( -92.69370383062498320, -208.6684592857803011, 86.36197916753383197 ) ) ;
#64958 = ORIENTED_EDGE ( 'NONE', *, *, #62312, .F. ) ;
#64959 = DIRECTION ( 'NONE',  ( -1.000000000000000000, 0.000000000000000000, 0.000000000000000000 ) ) ;
#64960 = EDGE_CURVE ( 'NONE', #59850, #71821, #9442, .T. ) ;
#64961 = ORIENTED_EDGE ( 'NONE', *, *, #66239, .T. ) ;
#64962 = VERTEX_POINT ( 'NONE', #36907 ) ;
#64963 = AXIS2_PLACEMENT_3D ( 'NONE', #59235, #47952, #63779 ) ;
#64964 = AXIS2_PLACEMENT_3D ( 'NONE', #19708, #42655, #54672 ) ;
#64965 = CARTESIAN_POINT ( 'NONE',  ( 10.00000000000000000, -75.11764819372145041, 29.05362095685286761 ) ) ;
#64966 = AXIS2_PLACEMENT_3D ( 'NONE', #14828, #66714, #53957 ) ;
#64967 = EDGE_CURVE ( 'NONE', #45508, #7045, #43115, .T. ) ;
#64968 = EDGE_CURVE ( 'NONE', #20059, #67482, #41927, .T. ) ;
#64969 = CARTESIAN_POINT ( 'NONE',  ( 92.69370383062498320, 91.33154071421968467, 89.74864583420048803 ) ) ;
#64970 = FACE_OUTER_BOUND ( 'NONE', #17294, .T. ) ;
#64971 = CARTESIAN_POINT ( 'NONE',  ( 94.99999999999998579, 92.66308142843932671, 81.22906250086714408 ) ) ;
#64972 = DIRECTION ( 'NONE',  ( 0.000000000000000000, 0.000000000000000000, 1.000000000000000000 ) ) ;
#64973 = CARTESIAN_POINT ( 'NONE',  ( -97.65000000000001990, 90.00000000000004263, 88.09499999999999886 ) ) ;
#64974 = DIRECTION ( 'NONE',  ( -1.000000000000000000, 0.000000000000000000, 0.000000000000000000 ) ) ;
#64975 = FACE_OUTER_BOUND ( 'NONE', #63559, .T. ) ;
#64976 = DIRECTION ( 'NONE',  ( -1.000000000000000000, 0.000000000000000000, 0.000000000000000000 ) ) ;
#64977 = DIRECTION ( 'NONE',  ( 1.000000000000000000, 0.000000000000000000, 0.000000000000000000 ) ) ;
#64978 = DIRECTION ( 'NONE',  ( 0.000000000000000000, 0.000000000000000000, 1.000000000000000000 ) ) ;
#64979 = ADVANCED_FACE ( 'NONE', ( #65128 ), #13605, .F. ) ;
#64980 = FACE_OUTER_BOUND ( 'NONE', #52929, .T. ) ;
#64981 = COLOUR_RGB ( '', 0.66274510, 0.83137255, 0.94901961) ;
#64982 = EDGE_CURVE ( 'NONE', #35679, #11281, #3100, .T. ) ;
#64983 = FACE_OUTER_BOUND ( 'NONE', #61500, .T. ) ;
#64984 = ORIENTED_EDGE ( 'NONE', *, *, #52548, .T. ) ;
#64985 = CARTESIAN_POINT ( 'NONE',  ( -92.69370383062504004, 90.00000000000004263, 84.88031250086713442 ) ) ;
#64986 = AXIS2_PLACEMENT_3D ( 'NONE', #40074, #29509, #5876 ) ;
#64987 = DIRECTION ( 'NONE',  ( 1.000000000000000000, 0.000000000000000000, 0.000000000000000000 ) ) ;
#64988 = CIRCLE ( 'NONE', #3760, 31.99999999999999289 ) ;
#64989 = AXIS2_PLACEMENT_3D ( 'NONE', #6717, #52569, #1121 ) ;
#64990 = DIRECTION ( 'NONE',  ( 1.000000000000000000, 0.000000000000000000, 0.000000000000000000 ) ) ;
#64991 = VERTEX_POINT ( 'NONE', #42932 ) ;
#64992 = VECTOR ( 'NONE', #37970, 1000.000000000000000 ) ;
#64993 = DIRECTION ( 'NONE',  ( -1.000000000000000000, -0.000000000000000000, 0.000000000000000000 ) ) ;
#64994 = DIRECTION ( 'NONE',  ( -1.343011723336883198E-16, 1.000000000000000000, 0.000000000000000000 ) ) ;
#64995 = LINE ( 'NONE', #4347, #23642 ) ;
#64996 = CARTESIAN_POINT ( 'NONE',  ( 92.69370383062501162, -211.3315407142195852, 82.23447916753383424 ) ) ;
#64997 = EDGE_LOOP ( 'NONE', ( #8790, #66254, #65116, #61955 ) ) ;
#64998 = ORIENTED_EDGE ( 'NONE', *, *, #10383, .T. ) ;
#64999 = CARTESIAN_POINT ( 'NONE',  ( -96.32499999999996021, -207.7050326799711968, 86.08416666666666117 ) ) ;
#65000 = ORIENTED_EDGE ( 'NONE', *, *, #41577, .T. ) ;
#65001 = DIRECTION ( 'NONE',  ( -1.000000000000000000, -0.000000000000000000, -0.000000000000000000 ) ) ;
#65002 = CARTESIAN_POINT ( 'NONE',  ( 92.69370383062501162, -209.9999999999999716, 75.03781250086713328 ) ) ;
#65003 = ORIENTED_EDGE ( 'NONE', *, *, #60444, .T. ) ;
#65004 = CARTESIAN_POINT ( 'NONE',  ( 97.30629616937498838, -211.3315407142195852, 81.17614583420048291 ) ) ;
#65005 = CIRCLE ( 'NONE', #73409, 11.59999999999999964 ) ;
#65006 = EDGE_LOOP ( 'NONE', ( #72044, #47256, #3631, #49352 ) ) ;
#65007 = EDGE_CURVE ( 'NONE', #36975, #44200, #13963, .T. ) ;
#65008 = DIRECTION ( 'NONE',  ( -0.000000000000000000, -0.000000000000000000, -1.000000000000000000 ) ) ;
#65009 = ORIENTED_EDGE ( 'NONE', *, *, #48624, .T. ) ;
#65010 = AXIS2_PLACEMENT_3D ( 'NONE', #30544, #6170, #6526 ) ;
#65011 = ORIENTED_EDGE ( 'NONE', *, *, #21668, .T. ) ;
#65012 = LINE ( 'NONE', #13847, #23729 ) ;
#65013 = ADVANCED_FACE ( 'NONE', ( #60235 ), #8712, .T. ) ;
#65014 = CIRCLE ( 'NONE', #42215, 82.00000000000000000 ) ;
#65015 = FILL_AREA_STYLE_COLOUR ( '', #41026 ) ;
#65016 = CARTESIAN_POINT ( 'NONE',  ( -92.35000000000000853, 91.52997821335252127, 82.75041666666666629 ) ) ;
#65017 = VERTEX_POINT ( 'NONE', #62073 ) ;
#65018 = CARTESIAN_POINT ( 'NONE',  ( 0.000000000000000000, 0.000000000000000000, 0.000000000000000000 ) ) ;
#65019 = CARTESIAN_POINT ( 'NONE',  ( 95.00000000000000000, -206.9400435732949575, 82.93562500173429441 ) ) ;
#65020 = EDGE_CURVE ( 'NONE', #67983, #50757, #62836, .T. ) ;
#65021 = CARTESIAN_POINT ( 'NONE',  ( 97.64999999999999147, 90.00000000000002842, 87.77749999999998920 ) ) ;
#65022 = EDGE_CURVE ( 'NONE', #47168, #64184, #5318, .T. ) ;
#65023 = ORIENTED_EDGE ( 'NONE', *, *, #50846, .T. ) ;
#65024 = DIRECTION ( 'NONE',  ( 0.000000000000000000, 0.000000000000000000, 1.000000000000000000 ) ) ;
#65025 = AXIS2_PLACEMENT_3D ( 'NONE', #47638, #40902, #18684 ) ;
#65026 = CARTESIAN_POINT ( 'NONE',  ( 10.00000000000000000, -62.20884554314051940, 46.21855187248608132 ) ) ;
#65027 = EDGE_LOOP ( 'NONE', ( #7578, #39490, #43556, #40297 ) ) ;
#65028 = ORIENTED_EDGE ( 'NONE', *, *, #55322, .T. ) ;
#65029 = CARTESIAN_POINT ( 'NONE',  ( -97.30629616937501680, 88.66845928578038638, 88.58447916753382856 ) ) ;
#65030 = CARTESIAN_POINT ( 'NONE',  ( 96.15314808468748708, 88.00268892867053694, 84.13947916753380696 ) ) ;
#65031 = VERTEX_POINT ( 'NONE', #22213 ) ;
#65032 = CARTESIAN_POINT ( 'NONE',  ( 92.34999999999999432, 90.00000000000002842, 87.53937500173429953 ) ) ;
#65033 = ORIENTED_EDGE ( 'NONE', *, *, #26830, .F. ) ;
#65034 = DIRECTION ( 'NONE',  ( 0.000000000000000000, -0.000000000000000000, 1.000000000000000000 ) ) ;
#65035 = ORIENTED_EDGE ( 'NONE', *, *, #56940, .F. ) ;
#65036 = CIRCLE ( 'NONE', #73442, 31.99999999999998579 ) ;
#65037 = ORIENTED_EDGE ( 'NONE', *, *, #73513, .F. ) ;
#65038 = EDGE_CURVE ( 'NONE', #24628, #53485, #4947, .T. ) ;
#65039 = ORIENTED_EDGE ( 'NONE', *, *, #72571, .F. ) ;
#65040 = CARTESIAN_POINT ( 'NONE',  ( 12.00000000000000000, -10.45096189432314127, 21.10159698893440350 ) ) ;
#65041 = CIRCLE ( 'NONE', #60211, 77.49899999999999523 ) ;
#65042 = DIRECTION ( 'NONE',  ( -1.000000000000000000, 0.000000000000000000, 0.000000000000000000 ) ) ;
#65043 = EDGE_CURVE ( 'NONE', #72004, #10345, #15506, .T. ) ;
#65044 = CARTESIAN_POINT ( 'NONE',  ( -97.65000000000001990, 90.00000000000004263, 83.65000000000000568 ) ) ;
#65045 = VERTEX_POINT ( 'NONE', #51146 ) ;
#65046 = CARTESIAN_POINT ( 'NONE',  ( -97.64999999953499810, 89.99996900126896548, 83.09538598081491045 ) ) ;
#65047 =( BOUNDED_CURVE ( )  B_SPLINE_CURVE ( 2, ( #30567, #20411, #26411, #53512, #71151, #48964, #2048, #19292, #65541 ),
 .UNSPECIFIED., .F., .F. ) 
 B_SPLINE_CURVE_WITH_KNOTS ( ( 3, 2, 2, 2, 3 ),
 ( 0.4868478063952913493, 0.4939035878641909738, 0.5009593534051074437, 0.5080151189460238026, 0.5080151867278726030 ),
 .UNSPECIFIED. ) 
 CURVE ( )  GEOMETRIC_REPRESENTATION_ITEM ( )  RATIONAL_B_SPLINE_CURVE ( ( 1.000000000000000000, 0.8660254037844387076, 1.000000000000000000, 0.8660254037844387076, 1.000000000000000000, 0.8660254037844387076, 1.000000000000000000, 0.9999987129609425596, 0.9999974259466133386 ) ) 
 REPRESENTATION_ITEM ( '' )  );
#65048 = DIRECTION ( 'NONE',  ( 0.000000000000000000, 0.000000000000000000, -1.000000000000000000 ) ) ;
#65049 = EDGE_LOOP ( 'NONE', ( #61020, #51225, #73205, #53444 ) ) ;
#65050 = CYLINDRICAL_SURFACE ( 'NONE', #35953, 2.650000000000540812 ) ;
#65051 = CARTESIAN_POINT ( 'NONE',  ( -97.30629616937495996, -209.9999999999999716, 83.92781250086714806 ) ) ;
#65052 = VERTEX_POINT ( 'NONE', #27091 ) ;
#65053 = DIRECTION ( 'NONE',  ( -1.000000000000000000, 0.000000000000000000, 0.000000000000000000 ) ) ;
#65054 = CARTESIAN_POINT ( 'NONE',  ( 11.99999999999999822, -59.03342792756231461, -46.54456581323868392 ) ) ;
#65055 = CARTESIAN_POINT ( 'NONE',  ( 10.00000000000000000, 0.000000000000000000, 0.000000000000000000 ) ) ;
#65056 = CYLINDRICAL_SURFACE ( 'NONE', #2695, 31.99999999999998579 ) ;
#65057 = DIRECTION ( 'NONE',  ( 1.000000000000000000, 0.000000000000000000, 0.000000000000000000 ) ) ;
#65058 = EDGE_CURVE ( 'NONE', #1375, #27107, #40692, .T. ) ;
#65059 = EDGE_CURVE ( 'NONE', #29201, #40792, #33860, .T. ) ;
#65060 = CARTESIAN_POINT ( 'NONE',  ( 92.35000000010803944, 90.00001510551041406, 78.64888723592453346 ) ) ;
#65061 = LINE ( 'NONE', #8645, #31241 ) ;
#65062 = CARTESIAN_POINT ( 'NONE',  ( 97.30629616937498838, -210.2956651733038314, 74.79348190356851944 ) ) ;
#65063 = CARTESIAN_POINT ( 'NONE',  ( 10.00000000000000000, -58.39081064771713869, -50.95692526931392052 ) ) ;
#65064 = FACE_OUTER_BOUND ( 'NONE', #32760, .T. ) ;
#65065 = CARTESIAN_POINT ( 'NONE',  ( -97.30629616937501680, 90.00000000000004263, 75.67281250086713840 ) ) ;
#65066 = LINE ( 'NONE', #13540, #15405 ) ;
#65067 = FACE_OUTER_BOUND ( 'NONE', #21058, .T. ) ;
#65068 =( BOUNDED_SURFACE ( )  B_SPLINE_SURFACE ( 1, 2, ( 
 ( #56294, #27712, #22075, #62700, #22827, #46123, #17540, #67944, #39371, #57037, #45770, #62313, #69057, #10797, #33724, #70139, #19011, #69411, #6996, #35939, #6634, #17914, #13000, #64156, #12636, #19385, #7741, #47230, #23555, #41583, #41966, #35568, #47971, #24662, #58499, #58884, #42335, #64519, #40857, #29546, #12268, #64898, #46483, #69779, #7379, #30295, #29921, #63795, #53237, #57774, #52120, #35199, #41217, #52483, #666, #1776, #13376, #58137, #47592, #6279, #1036, #52871, #29178, #65267, #23931, #13740, #53601, #46867, #36308, #25030, #59248, #70499, #30659, #2140, #18282, #1411, #70884, #24303, #18640, #49801, #26511, #65635, #8105, #48699, #14107, #31030, #53989, #71622, #21225, #71242, #48335, #25769, #49440, #72721, #61100, #2525, #71999, #44176, #67102, #36678, #14485, #25409, #60372, #37057, #59625, #55079, #19749, #26871, #72368, #3612, #20118, #43460, #54713, #66742, #3974, #37443, #42698, #43083, #66015, #20867, #60006, #15228, #9215, #8490, #31404, #43822, #54353, #8855, #66383, #37806, #31769, #2875, #14858, #3242, #26130, #49068, #20506, #60739, #32134, #38158, #9598, #32513, #55458, #38539, #27233, #10703, #15608, #23109, #50165, #217, #11436, #38909, #51291, #57311, #22741, #16724, #62978, #74222, #33247, #56197, #68603, #32875, #61476, #28731, #5458, #44557, #9957, #27625, #67478, #55826, #4343, #50548, #46039, #73100, #21607, #4719, #28354, #51670, #40026, #15968, #50922, #61845, #10329, #73474, #67852, #21983, #39284, #44928, #16344, #34002, #62216, #5823, #45683, #56949, #33632, #22359, #56584, #17091, #5086, #27986, #73844, #45305, #68223, #34371, #39660, #62599, #11080, #18919, #40767, #575, #69325, #69698, #30573, #17817, #63708, #18194, #64435, #47507, #7653, #23469, #12177, #46778, #58413, #35115, #30207, #58051, #53149, #6911, #1689, #6192, #41137, #47147, #6552, #29094, #24217, #945, #23836, #53516, #41862, #29826, #34752, #52784, #24575, #64073, #59162, #35842, #12548, #70055, #2054, #1328, #52030, #57693, #18556, #70413, #41495, #35482, #36219, #64811, #13289, #12909, #24940, #68967, #17453, #29454, #40383, #58793, #7293, #63334, #11794, #46399, #52398, #13653, #65181, #37351, #14399, #49983, #72903, #48249, #65920, #19299, #25322, #8021, #73288, #25681, #39096 ),
 ( #55637, #61290, #4527, #16159, #48615, #36586, #8399, #54265, #67292, #30939, #27427, #21406, #21795, #19662, #53886, #71156, #71529, #10511, #42610, #65545, #20029, #44366, #50364, #62034, #2433, #14020, #42988, #9777, #36964, #10142, #59911, #33062, #32692, #56008, #59535, #4154, #27051, #31316, #2793, #15791, #38727, #61656, #33435, #44747, #67668, #56399, #4908, #47870, #70794, #42247, #69155, #57136, #6017, #63890, #11614, #39473, #51111, #56770, #34937, #16526, #39849, #57504, #28919, #5645, #10900, #34556, #27806, #22175, #62419, #11261, #74037, #45115, #51854, #57872, #5275, #400, #50734, #33820, #22932, #73660, #35306, #28176, #12362, #23651, #22548, #58233, #28540, #68038, #51478, #45492, #40957, #46221, #68423, #18014, #63523, #17643, #62799, #23294, #45868, #6377, #69513, #37, #16912, #34191, #68794, #40575, #17274, #29279, #11999, #52220, #40208, #63155, #764, #46584, #42791, #7097, #30018, #30387, #2238, #59717, #19843, #12725, #52965, #58981, #70597, #1504, #42426, #24393, #65364, #19115, #13829, #18370, #53332, #59347, #47326, #41313, #36400, #13099, #36035, #65727, #31128, #42063, #46959, #64996, #36770, #7471, #71337, #48065, #1869, #7836, #14206, #13472, #64255, #70228, #35658, #8197, #69872, #18735, #30748, #53696, #24753, #58597, #25133, #6733, #1135, #41675, #64616, #47687, #24034, #70977, #54081, #19476, #2616, #29640, #25494, #48428, #52583, #37160, #20214, #44661, #55921, #8950, #21318, #27335, #67203, #61200, #32974, #44276, #3335, #26228, #38639, #2971, #31497, #73203, #49897, #14581, #54441, #72092, #37530, #25859, #48791, #20601, #67575, #43182, #71712, #49167, #72817, #21704, #10056, #66108, #20962, #16073, #60104, #15703, #60470, #43553, #15318, #9687, #37898, #31867, #66833, #8583, #54806, #66472, #14959, #60826, #9308, #32610, #61571, #32229, #55551, #55179, #3705, #26600, #49530, #72458, #43915, #38257, #4436, #4070, #50270, #26967, #63073, #28453, #5922, #17187, #62321, #10808, #34466, #33340, #61941, #46134, #68703, #22086, #10424, #33734, #45026, #56303, #4821, #56681, #17548, #50644, #27721, #5182, #40120, #23204, #28830, #73569, #11173, #40481, #39009, #67950, #51384, #28087, #74323, #22458, #16439, #69064, #51025, #39379, #73947, #45398, #11532, #68325, #16820 ) ),
 .UNSPECIFIED., .F., .F., .F. ) 
 B_SPLINE_SURFACE_WITH_KNOTS ( ( 2, 2 ),
 ( 3, 2, 2, 2, 2, 2, 2, 2, 2, 2, 2, 2, 2, 2, 2, 2, 2, 2, 2, 2, 2, 2, 2, 2, 2, 2, 2, 2, 2, 2, 2, 2, 2, 2, 2, 2, 2, 2, 2, 2, 2, 2, 2, 2, 2, 2, 2, 2, 2, 2, 2, 2, 2, 2, 2, 2, 2, 2, 2, 2, 2, 2, 2, 2, 2, 2, 2, 2, 2, 2, 2, 2, 2, 2, 2, 2, 2, 2, 2, 2, 2, 2, 2, 2, 2, 2, 2, 2, 2, 2, 2, 2, 2, 2, 2, 2, 2, 2, 2, 2, 2, 2, 2, 2, 2, 2, 2, 2, 2, 2, 2, 2, 2, 2, 2, 2, 2, 2, 2, 2, 2, 2, 2, 2, 2, 2, 2, 2, 2, 2, 2, 2, 2, 2, 2, 2, 2, 2, 2, 2, 2, 2, 3 ),
 ( 0.000000000000000000, 1.000000000000000000 ),
 ( 0.000000000000000000, 0.006944444444444444059, 0.01388888888888888812, 0.02083333333333333218, 0.02777777777777777624, 0.03472222222222222376, 0.04166666666666666435, 0.04861111111111111188, 0.05555555555555555247, 0.06250000000000000000, 0.06944444444444444753, 0.07638888888888889506, 0.08333333333333332871, 0.09027777777777777624, 0.09722222222222222376, 0.1041666666666666713, 0.1111111111111111049, 0.1180555555555555525, 0.1250000000000000000, 0.1319444444444444475, 0.1388888888888888951, 0.1458333333333333426, 0.1527777777777777901, 0.1597222222222222099, 0.1666666666666666574, 0.1736111111111111049, 0.1805555555555555525, 0.1875000000000000000, 0.1944444444444444475, 0.2013888888888888951, 0.2083333333333333426, 0.2152777777777777901, 0.2222222222222222099, 0.2291666666666666574, 0.2361111111111111049, 0.2430555555555555525, 0.2500000000000000000, 0.2569444444444444198, 0.2638888888888888951, 0.2708333333333333148, 0.2777777777777777901, 0.2847222222222222099, 0.2916666666666666852, 0.2986111111111111049, 0.3055555555555555802, 0.3125000000000000000, 0.3194444444444444198, 0.3263888888888888951, 0.3333333333333333148, 0.3402777777777777901, 0.3472222222222222099, 0.3541666666666666852, 0.3611111111111111049, 0.3680555555555555802, 0.3750000000000000000, 0.3819444444444444198, 0.3888888888888888951, 0.3958333333333333148, 0.4027777777777777901, 0.4097222222222222099, 0.4166666666666666852, 0.4236111111111111049, 0.4305555555555555802, 0.4375000000000000000, 0.4444444444444444198, 0.4513888888888888951, 0.4583333333333333148, 0.4652777777777777901, 0.4722222222222222099, 0.4791666666666666852, 0.4861111111111111049, 0.4930555555555555802, 0.5000000000000000000, 0.5069444444444444198, 0.5138888888888888395, 0.5208333333333333703, 0.5277777777777777901, 0.5347222222222222099, 0.5416666666666666297, 0.5486111111111111605, 0.5555555555555555802, 0.5625000000000000000, 0.5694444444444444198, 0.5763888888888888395, 0.5833333333333333703, 0.5902777777777777901, 0.5972222222222222099, 0.6041666666666666297, 0.6111111111111111605, 0.6180555555555555802, 0.6250000000000000000, 0.6319444444444444198, 0.6388888888888888395, 0.6458333333333333703, 0.6527777777777777901, 0.6597222222222222099, 0.6666666666666666297, 0.6736111111111111605, 0.6805555555555555802, 0.6875000000000000000, 0.6944444444444444198, 0.7013888888888888395, 0.7083333333333333703, 0.7152777777777777901, 0.7222222222222222099, 0.7291666666666666297, 0.7361111111111111605, 0.7430555555555555802, 0.7500000000000000000, 0.7569444444444444198, 0.7638888888888888395, 0.7708333333333333703, 0.7777777777777777901, 0.7847222222222222099, 0.7916666666666666297, 0.7986111111111111605, 0.8055555555555555802, 0.8125000000000000000, 0.8194444444444444198, 0.8263888888888888395, 0.8333333333333333703, 0.8402777777777777901, 0.8472222222222222099, 0.8541666666666666297, 0.8611111111111111605, 0.8680555555555555802, 0.8750000000000000000, 0.8819444444444444198, 0.8888888888888888395, 0.8958333333333333703, 0.9027777777777777901, 0.9097222222222222099, 0.9166666666666666297, 0.9236111111111111605, 0.9305555555555555802, 0.9375000000000000000, 0.9444444444444444198, 0.9513888888888888395, 0.9583333333333333703, 0.9652777777777777901, 0.9722222222222222099, 0.9791666666666666297, 0.9842227634901432598 ),
 .UNSPECIFIED. ) 
 GEOMETRIC_REPRESENTATION_ITEM ( )  RATIONAL_B_SPLINE_SURFACE ( (
 ( 1.000000000000000000, 0.8660254037844387076, 1.000000000000000000, 0.8660254037844387076, 1.000000000000000000, 0.8660254037844387076, 1.000000000000000000, 0.8660254037844387076, 1.000000000000000000, 0.8660254037844387076, 1.000000000000000000, 0.8660254037844387076, 1.000000000000000000, 0.8660254037844387076, 1.000000000000000000, 0.8660254037844387076, 1.000000000000000000, 0.8660254037844387076, 1.000000000000000000, 0.8660254037844387076, 1.000000000000000000, 0.8660254037844387076, 1.000000000000000000, 0.8660254037844387076, 1.000000000000000000, 0.8660254037844387076, 1.000000000000000000, 0.8660254037844387076, 1.000000000000000000, 0.8660254037844387076, 1.000000000000000000, 0.8660254037844387076, 1.000000000000000000, 0.8660254037844387076, 1.000000000000000000, 0.8660254037844387076, 1.000000000000000000, 0.8660254037844387076, 1.000000000000000000, 0.8660254037844387076, 1.000000000000000000, 0.8660254037844387076, 1.000000000000000000, 0.8660254037844387076, 1.000000000000000000, 0.8660254037844387076, 1.000000000000000000, 0.8660254037844387076, 1.000000000000000000, 0.8660254037844387076, 1.000000000000000000, 0.8660254037844387076, 1.000000000000000000, 0.8660254037844387076, 1.000000000000000000, 0.8660254037844387076, 1.000000000000000000, 0.8660254037844387076, 1.000000000000000000, 0.8660254037844387076, 1.000000000000000000, 0.8660254037844387076, 1.000000000000000000, 0.8660254037844387076, 1.000000000000000000, 0.8660254037844387076, 1.000000000000000000, 0.8660254037844387076, 1.000000000000000000, 0.8660254037844387076, 1.000000000000000000, 0.8660254037844387076, 1.000000000000000000, 0.8660254037844387076, 1.000000000000000000, 0.8660254037844387076, 1.000000000000000000, 0.8660254037844387076, 1.000000000000000000, 0.8660254037844387076, 1.000000000000000000, 0.8660254037844387076, 1.000000000000000000, 0.8660254037844387076, 1.000000000000000000, 0.8660254037844387076, 1.000000000000000000, 0.8660254037844387076, 1.000000000000000000, 0.8660254037844387076, 1.000000000000000000, 0.8660254037844387076, 1.000000000000000000, 0.8660254037844387076, 1.000000000000000000, 0.8660254037844387076, 1.000000000000000000, 0.8660254037844387076, 1.000000000000000000, 0.8660254037844387076, 1.000000000000000000, 0.8660254037844387076, 1.000000000000000000, 0.8660254037844387076, 1.000000000000000000, 0.8660254037844387076, 1.000000000000000000, 0.8660254037844387076, 1.000000000000000000, 0.8660254037844387076, 1.000000000000000000, 0.8660254037844387076, 1.000000000000000000, 0.8660254037844387076, 1.000000000000000000, 0.8660254037844387076, 1.000000000000000000, 0.8660254037844387076, 1.000000000000000000, 0.8660254037844387076, 1.000000000000000000, 0.8660254037844387076, 1.000000000000000000, 0.8660254037844387076, 1.000000000000000000, 0.8660254037844387076, 1.000000000000000000, 0.8660254037844387076, 1.000000000000000000, 0.8660254037844387076, 1.000000000000000000, 0.8660254037844387076, 1.000000000000000000, 0.8660254037844387076, 1.000000000000000000, 0.8660254037844387076, 1.000000000000000000, 0.8660254037844387076, 1.000000000000000000, 0.8660254037844387076, 1.000000000000000000, 0.8660254037844387076, 1.000000000000000000, 0.8660254037844387076, 1.000000000000000000, 0.8660254037844387076, 1.000000000000000000, 0.8660254037844387076, 1.000000000000000000, 0.8660254037844387076, 1.000000000000000000, 0.8660254037844387076, 1.000000000000000000, 0.8660254037844387076, 1.000000000000000000, 0.8660254037844387076, 1.000000000000000000, 0.8660254037844387076, 1.000000000000000000, 0.8660254037844387076, 1.000000000000000000, 0.8660254037844387076, 1.000000000000000000, 0.8660254037844387076, 1.000000000000000000, 0.8660254037844387076, 1.000000000000000000, 0.8660254037844387076, 1.000000000000000000, 0.8660254037844387076, 1.000000000000000000, 0.8660254037844387076, 1.000000000000000000, 0.8660254037844387076, 1.000000000000000000, 0.8660254037844387076, 1.000000000000000000, 0.8660254037844387076, 1.000000000000000000, 0.8660254037844387076, 1.000000000000000000, 0.8660254037844387076, 1.000000000000000000, 0.8660254037844387076, 1.000000000000000000, 0.8660254037844387076, 1.000000000000000000, 0.8660254037844387076, 1.000000000000000000, 0.8660254037844387076, 1.000000000000000000, 0.8660254037844387076, 1.000000000000000000, 0.8660254037844387076, 1.000000000000000000, 0.8660254037844387076, 1.000000000000000000, 0.8660254037844387076, 1.000000000000000000, 0.8660254037844387076, 1.000000000000000000, 0.8660254037844387076, 1.000000000000000000, 0.8660254037844387076, 1.000000000000000000, 0.8660254037844387076, 1.000000000000000000, 0.8660254037844387076, 1.000000000000000000, 0.8660254037844387076, 1.000000000000000000, 0.8660254037844387076, 1.000000000000000000, 0.8660254037844387076, 1.000000000000000000, 0.8660254037844387076, 1.000000000000000000, 0.8660254037844387076, 1.000000000000000000, 0.8660254037844387076, 1.000000000000000000, 0.8660254037844387076, 1.000000000000000000, 0.8660254037844387076, 1.000000000000000000, 0.8660254037844387076, 1.000000000000000000, 0.8660254037844387076, 1.000000000000000000, 0.8660254037844387076, 1.000000000000000000, 0.8660254037844387076, 1.000000000000000000, 0.8660254037844387076, 1.000000000000000000, 0.8660254037844387076, 1.000000000000000000, 0.8660254037844387076, 1.000000000000000000, 0.8660254037844387076, 1.000000000000000000, 0.8660254037844387076, 1.000000000000000000, 0.8660254037844387076, 1.000000000000000000, 0.8660254037844387076, 1.000000000000000000, 0.8660254037844387076, 1.000000000000000000, 0.8660254037844387076, 1.000000000000000000, 0.8660254037844387076, 1.000000000000000000, 0.8660254037844387076, 1.000000000000000000, 0.8660254037844387076, 1.000000000000000000, 0.8660254037844387076, 1.000000000000000000, 0.8660254037844387076, 1.000000000000000000, 0.8660254037844387076, 1.000000000000000000, 0.8660254037844387076, 1.000000000000000000, 0.8660254037844387076, 1.000000000000000000, 0.8660254037844387076, 1.000000000000000000, 0.8660254037844387076, 1.000000000000000000, 0.8660254037844387076, 1.000000000000000000, 0.8660254037844387076, 1.000000000000000000, 0.8660254037844387076, 1.000000000000000000, 0.8660254037844387076, 1.000000000000000000, 0.8660254037844387076, 1.000000000000000000, 0.8660254037844387076, 1.000000000000000000, 0.9024560516293040902, 0.9469512977404621612),
 ( 1.000000000000000000, 0.8660254037844387076, 1.000000000000000000, 0.8660254037844387076, 1.000000000000000000, 0.8660254037844387076, 1.000000000000000000, 0.8660254037844387076, 1.000000000000000000, 0.8660254037844387076, 1.000000000000000000, 0.8660254037844387076, 1.000000000000000000, 0.8660254037844387076, 1.000000000000000000, 0.8660254037844387076, 1.000000000000000000, 0.8660254037844387076, 1.000000000000000000, 0.8660254037844387076, 1.000000000000000000, 0.8660254037844387076, 1.000000000000000000, 0.8660254037844387076, 1.000000000000000000, 0.8660254037844387076, 1.000000000000000000, 0.8660254037844387076, 1.000000000000000000, 0.8660254037844387076, 1.000000000000000000, 0.8660254037844387076, 1.000000000000000000, 0.8660254037844387076, 1.000000000000000000, 0.8660254037844387076, 1.000000000000000000, 0.8660254037844387076, 1.000000000000000000, 0.8660254037844387076, 1.000000000000000000, 0.8660254037844387076, 1.000000000000000000, 0.8660254037844387076, 1.000000000000000000, 0.8660254037844387076, 1.000000000000000000, 0.8660254037844387076, 1.000000000000000000, 0.8660254037844387076, 1.000000000000000000, 0.8660254037844387076, 1.000000000000000000, 0.8660254037844387076, 1.000000000000000000, 0.8660254037844387076, 1.000000000000000000, 0.8660254037844387076, 1.000000000000000000, 0.8660254037844387076, 1.000000000000000000, 0.8660254037844387076, 1.000000000000000000, 0.8660254037844387076, 1.000000000000000000, 0.8660254037844387076, 1.000000000000000000, 0.8660254037844387076, 1.000000000000000000, 0.8660254037844387076, 1.000000000000000000, 0.8660254037844387076, 1.000000000000000000, 0.8660254037844387076, 1.000000000000000000, 0.8660254037844387076, 1.000000000000000000, 0.8660254037844387076, 1.000000000000000000, 0.8660254037844387076, 1.000000000000000000, 0.8660254037844387076, 1.000000000000000000, 0.8660254037844387076, 1.000000000000000000, 0.8660254037844387076, 1.000000000000000000, 0.8660254037844387076, 1.000000000000000000, 0.8660254037844387076, 1.000000000000000000, 0.8660254037844387076, 1.000000000000000000, 0.8660254037844387076, 1.000000000000000000, 0.8660254037844387076, 1.000000000000000000, 0.8660254037844387076, 1.000000000000000000, 0.8660254037844387076, 1.000000000000000000, 0.8660254037844387076, 1.000000000000000000, 0.8660254037844387076, 1.000000000000000000, 0.8660254037844387076, 1.000000000000000000, 0.8660254037844387076, 1.000000000000000000, 0.8660254037844387076, 1.000000000000000000, 0.8660254037844387076, 1.000000000000000000, 0.8660254037844387076, 1.000000000000000000, 0.8660254037844387076, 1.000000000000000000, 0.8660254037844387076, 1.000000000000000000, 0.8660254037844387076, 1.000000000000000000, 0.8660254037844387076, 1.000000000000000000, 0.8660254037844387076, 1.000000000000000000, 0.8660254037844387076, 1.000000000000000000, 0.8660254037844387076, 1.000000000000000000, 0.8660254037844387076, 1.000000000000000000, 0.8660254037844387076, 1.000000000000000000, 0.8660254037844387076, 1.000000000000000000, 0.8660254037844387076, 1.000000000000000000, 0.8660254037844387076, 1.000000000000000000, 0.8660254037844387076, 1.000000000000000000, 0.8660254037844387076, 1.000000000000000000, 0.8660254037844387076, 1.000000000000000000, 0.8660254037844387076, 1.000000000000000000, 0.8660254037844387076, 1.000000000000000000, 0.8660254037844387076, 1.000000000000000000, 0.8660254037844387076, 1.000000000000000000, 0.8660254037844387076, 1.000000000000000000, 0.8660254037844387076, 1.000000000000000000, 0.8660254037844387076, 1.000000000000000000, 0.8660254037844387076, 1.000000000000000000, 0.8660254037844387076, 1.000000000000000000, 0.8660254037844387076, 1.000000000000000000, 0.8660254037844387076, 1.000000000000000000, 0.8660254037844387076, 1.000000000000000000, 0.8660254037844387076, 1.000000000000000000, 0.8660254037844387076, 1.000000000000000000, 0.8660254037844387076, 1.000000000000000000, 0.8660254037844387076, 1.000000000000000000, 0.8660254037844387076, 1.000000000000000000, 0.8660254037844387076, 1.000000000000000000, 0.8660254037844387076, 1.000000000000000000, 0.8660254037844387076, 1.000000000000000000, 0.8660254037844387076, 1.000000000000000000, 0.8660254037844387076, 1.000000000000000000, 0.8660254037844387076, 1.000000000000000000, 0.8660254037844387076, 1.000000000000000000, 0.8660254037844387076, 1.000000000000000000, 0.8660254037844387076, 1.000000000000000000, 0.8660254037844387076, 1.000000000000000000, 0.8660254037844387076, 1.000000000000000000, 0.8660254037844387076, 1.000000000000000000, 0.8660254037844387076, 1.000000000000000000, 0.8660254037844387076, 1.000000000000000000, 0.8660254037844387076, 1.000000000000000000, 0.8660254037844387076, 1.000000000000000000, 0.8660254037844387076, 1.000000000000000000, 0.8660254037844387076, 1.000000000000000000, 0.8660254037844387076, 1.000000000000000000, 0.8660254037844387076, 1.000000000000000000, 0.8660254037844387076, 1.000000000000000000, 0.8660254037844387076, 1.000000000000000000, 0.8660254037844387076, 1.000000000000000000, 0.8660254037844387076, 1.000000000000000000, 0.8660254037844387076, 1.000000000000000000, 0.8660254037844387076, 1.000000000000000000, 0.8660254037844387076, 1.000000000000000000, 0.8660254037844387076, 1.000000000000000000, 0.8660254037844387076, 1.000000000000000000, 0.8660254037844387076, 1.000000000000000000, 0.8660254037844387076, 1.000000000000000000, 0.8660254037844387076, 1.000000000000000000, 0.8660254037844387076, 1.000000000000000000, 0.8660254037844387076, 1.000000000000000000, 0.8660254037844387076, 1.000000000000000000, 0.8660254037844387076, 1.000000000000000000, 0.8660254037844387076, 1.000000000000000000, 0.8660254037844387076, 1.000000000000000000, 0.8660254037844387076, 1.000000000000000000, 0.8660254037844387076, 1.000000000000000000, 0.8660254037844387076, 1.000000000000000000, 0.8660254037844387076, 1.000000000000000000, 0.8660254037844387076, 1.000000000000000000, 0.8660254037844387076, 1.000000000000000000, 0.8660254037844387076, 1.000000000000000000, 0.8660254037844387076, 1.000000000000000000, 0.8660254037844387076, 1.000000000000000000, 0.8660254037844387076, 1.000000000000000000, 0.8660254037844387076, 1.000000000000000000, 0.8660254037844387076, 1.000000000000000000, 0.8660254037844387076, 1.000000000000000000, 0.8660254037844387076, 1.000000000000000000, 0.9024560516293040902, 0.9469512977404621612) ) ) 
 REPRESENTATION_ITEM ( '' )  SURFACE ( )  );
#65069 = CARTESIAN_POINT ( 'NONE',  ( 8.000000000000007105, 13.10000000000016485, 1.604118440328575499E-13 ) ) ;
#65070 = DIRECTION ( 'NONE',  ( 0.000000000000000000, -0.4539904997395541320, 0.8910065241883640130 ) ) ;
#65071 = DIRECTION ( 'NONE',  ( 0.000000000000000000, 0.000000000000000000, 1.000000000000000000 ) ) ;
#65072 = DIRECTION ( 'NONE',  ( -2.628368902995175337E-16, -1.000000000000000000, 0.000000000000000000 ) ) ;
#65073 = LINE ( 'NONE', #67188, #12999 ) ;
#65074 = AXIS2_PLACEMENT_3D ( 'NONE', #49595, #50716, #55619 ) ;
#65075 = DIRECTION ( 'NONE',  ( 0.000000000000000000, 0.000000000000000000, 1.000000000000000000 ) ) ;
#65076 = CARTESIAN_POINT ( 'NONE',  ( -97.64999999999994884, -208.4700217866474645, 89.31208333333333371 ) ) ;
#65077 = VECTOR ( 'NONE', #25368, 1000.000000000000000 ) ;
#65078 = CARTESIAN_POINT ( 'NONE',  ( 100.0010000000000190, -123.9999999999999858, 39.99999999999996447 ) ) ;
#65079 = AXIS2_PLACEMENT_3D ( 'NONE', #58083, #23498, #40413 ) ;
#65080 = ORIENTED_EDGE ( 'NONE', *, *, #14757, .F. ) ;
#65081 = FACE_OUTER_BOUND ( 'NONE', #10105, .T. ) ;
#65082 = CARTESIAN_POINT ( 'NONE',  ( 11.99999999999999822, -41.76106447765443619, -62.50884508063471401 ) ) ;
#65083 = FACE_OUTER_BOUND ( 'NONE', #6507, .T. ) ;
#65084 = CARTESIAN_POINT ( 'NONE',  ( -92.35000000000003695, 90.00000000000004263, 84.60249999999999204 ) ) ;
#65085 = AXIS2_PLACEMENT_3D ( 'NONE', #56452, #50035, #38033 ) ;
#65086 = CIRCLE ( 'NONE', #7492, 31.99999999999998579 ) ;
#65087 = DIRECTION ( 'NONE',  ( -1.000000000000000000, 0.000000000000000000, 0.000000000000000000 ) ) ;
#65088 = ORIENTED_EDGE ( 'NONE', *, *, #49505, .T. ) ;
#65089 = DIRECTION ( 'NONE',  ( 3.035766082959412415E-16, 1.000000000000000000, 0.000000000000000000 ) ) ;
#65090 = CARTESIAN_POINT ( 'NONE',  ( 11.99999999999999822, -73.72996012237449293, 14.67089635893687571 ) ) ;
#65091 = VERTEX_POINT ( 'NONE', #79 ) ;
#65092 = CARTESIAN_POINT ( 'NONE',  ( 92.69370383062501162, -208.6684592857803295, 85.14489583420045449 ) ) ;
#65093 = CARTESIAN_POINT ( 'NONE',  ( 92.69370383062501162, -211.3315407142195852, 88.58447916753382856 ) ) ;
#65094 = ORIENTED_EDGE ( 'NONE', *, *, #52197, .F. ) ;
#65095 = EDGE_CURVE ( 'NONE', #63816, #15441, #68461, .T. ) ;
#65096 = CARTESIAN_POINT ( 'NONE',  ( 92.69370383062501162, -211.3315407142195852, 88.58447916753382856 ) ) ;
#65097 = ADVANCED_BREP_SHAPE_REPRESENTATION ( '', ( #39004, #43395 ), #39845 ) ;
#65098 = ORIENTED_EDGE ( 'NONE', *, *, #42049, .T. ) ;
#65099 = EDGE_CURVE ( 'NONE', #51207, #58350, #10937, .T. ) ;
#65100 = CARTESIAN_POINT ( 'NONE',  ( -94.99999999999997158, -213.0599564267049857, 80.63375000000000625 ) ) ;
#65101 = EDGE_LOOP ( 'NONE', ( #74269, #71016, #68355, #73015 ) ) ;
#65102 = CARTESIAN_POINT ( 'NONE',  ( -96.15314808468752972, 91.99731107132950569, 79.53572916753381605 ) ) ;
#65103 = ORIENTED_EDGE ( 'NONE', *, *, #65275, .F. ) ;
#65104 = EDGE_CURVE ( 'NONE', #25068, #19568, #10688, .T. ) ;
#65105 = ORIENTED_EDGE ( 'NONE', *, *, #48119, .F. ) ;
#65106 = CARTESIAN_POINT ( 'NONE',  ( -7.499999999999970690, 69.70000000000003126, -255.0000000000000000 ) ) ;
#65107 = ORIENTED_EDGE ( 'NONE', *, *, #54725, .T. ) ;
#65108 = CARTESIAN_POINT ( 'NONE',  ( -10.00000000000000000, 0.000000000000000000, 0.000000000000000000 ) ) ;
#65109 = CARTESIAN_POINT ( 'NONE',  ( -3.000000000000000000, 20.85821328998756385, -10.92862929874494959 ) ) ;
#65110 = EDGE_CURVE ( 'NONE', #10549, #38728, #45155, .T. ) ;
#65111 = EDGE_LOOP ( 'NONE', ( #44031, #36248, #8998, #40044 ) ) ;
#65112 = FACE_OUTER_BOUND ( 'NONE', #13966, .T. ) ;
#65113 = VERTEX_POINT ( 'NONE', #45535 ) ;
#65114 = DIRECTION ( 'NONE',  ( 1.000000000000000000, 1.427937372958405461E-15, 7.962523111839130290E-16 ) ) ;
#65115 = EDGE_CURVE ( 'NONE', #63637, #21721, #63762, .T. ) ;
#65116 = ORIENTED_EDGE ( 'NONE', *, *, #56436, .F. ) ;
#65117 = VERTEX_POINT ( 'NONE', #61701 ) ;
#65118 = VERTEX_POINT ( 'NONE', #21449 ) ;
#65119 = CARTESIAN_POINT ( 'NONE',  ( 93.84685191531249870, -208.0026889286704943, 78.74197916753381321 ) ) ;
#65120 = CARTESIAN_POINT ( 'NONE',  ( -92.35000000000017906, 91.52997821335260653, 83.38541666666667140 ) ) ;
#65121 = DIRECTION ( 'NONE',  ( 0.000000000000000000, 0.5877852522924797984, -0.8090169943749426773 ) ) ;
#65122 = ORIENTED_EDGE ( 'NONE', *, *, #15334, .T. ) ;
#65124 = CARTESIAN_POINT ( 'NONE',  ( 10.00000000000000000, -0.6853352020793173072, 37.58145647212453611 ) ) ;
#65123 = VECTOR ( 'NONE', #62778, 1000.000000000000000 ) ;
#65125 = DIRECTION ( 'NONE',  ( -1.000000000000000000, 0.000000000000000000, 0.000000000000000000 ) ) ;
#65126 = DIRECTION ( 'NONE',  ( -1.000000000000000000, 0.000000000000000000, 0.000000000000000000 ) ) ;
#65127 = DIRECTION ( 'NONE',  ( 0.1276937514489679404, 0.9918136447140103451, -0.000000000000000000 ) ) ;
#65128 = FACE_OUTER_BOUND ( 'NONE', #67896, .T. ) ;
#65129 = CARTESIAN_POINT ( 'NONE',  ( -97.30629616937497417, -208.6684592857803011, 80.06489583420047040 ) ) ;
#65130 = EDGE_CURVE ( 'NONE', #12484, #56884, #56568, .T. ) ;
#65131 = CARTESIAN_POINT ( 'NONE',  ( -96.15314808468751551, 88.00268892867056536, 77.84239583420048803 ) ) ;
#65132 = AXIS2_PLACEMENT_3D ( 'NONE', #36648, #8824, #2849 ) ;
#65133 = ADVANCED_FACE ( 'NONE', ( #39136 ), #57177, .T. ) ;
#65134 = ORIENTED_EDGE ( 'NONE', *, *, #41579, .T. ) ;
#65135 = CARTESIAN_POINT ( 'NONE',  ( 92.69370383062498320, 88.66845928578037217, 80.17072916753379275 ) ) ;
#65136 = CIRCLE ( 'NONE', #345, 42.00000000000000000 ) ;
#65137 = ORIENTED_EDGE ( 'NONE', *, *, #46713, .F. ) ;
#65138 = DIRECTION ( 'NONE',  ( 0.000000000000000000, 0.000000000000000000, -1.000000000000000000 ) ) ;
#65139 = PLANE ( 'NONE',  #16774 ) ;
#65140 = CARTESIAN_POINT ( 'NONE',  ( 94.99999999999998579, 86.94004357329502852, 77.53812500173428646 ) ) ;
#65141 = DIRECTION ( 'NONE',  ( 0.000000000000000000, -0.3090169943749548898, 0.9510565162951511997 ) ) ;
#65142 = LINE ( 'NONE', #59126, #20027 ) ;
#65143 = CARTESIAN_POINT ( 'NONE',  ( -92.69370383062498320, -211.3315407142195852, 81.65239583420047609 ) ) ;
#65144 = DIRECTION ( 'NONE',  ( 1.000000000000000000, 1.427937372958405461E-15, 7.962523111839130290E-16 ) ) ;
#65145 = DIRECTION ( 'NONE',  ( -1.000000000000000000, 0.000000000000000000, -0.000000000000000000 ) ) ;
#65146 = CIRCLE ( 'NONE', #24301, 16.00000000000000000 ) ;
#65147 = CARTESIAN_POINT ( 'NONE',  ( 21.85433023846371370, -135.0628101570779620, 5.500000000000000000 ) ) ;
#65148 = EDGE_LOOP ( 'NONE', ( #21446, #25723, #69379, #28584, #66473 ) ) ;
#65149 = EDGE_CURVE ( 'NONE', #14677, #20502, #8518, .T. ) ;
#65150 = EDGE_CURVE ( 'NONE', #48479, #21836, #49347, .T. ) ;
#65151 = ORIENTED_EDGE ( 'NONE', *, *, #17730, .T. ) ;
#65152 = CARTESIAN_POINT ( 'NONE',  ( -12.50000000000000000, -132.5000000000000000, 40.00000000000000000 ) ) ;
#65153 = CARTESIAN_POINT ( 'NONE',  ( -94.46769236096046995, 86.73322217287214642, 74.92222617501695936 ) ) ;
#65154 = CARTESIAN_POINT ( 'NONE',  ( 11.99999999999999822, -71.27951684758045303, 30.41916302227090085 ) ) ;
#65155 = CARTESIAN_POINT ( 'NONE',  ( -97.30629616937501680, 88.66845928578038638, 83.98072916753380923 ) ) ;
#65156 = DIRECTION ( 'NONE',  ( 0.9781476007338070211, 0.000000000000000000, -0.2079116908177527367 ) ) ;
#65157 = DIRECTION ( 'NONE',  ( -1.000000000000000000, -0.000000000000000000, -0.000000000000000000 ) ) ;
#65158 = CARTESIAN_POINT ( 'NONE',  ( 92.34999999999999432, 88.47002178664752137, 81.24229166840096639 ) ) ;
#65159 = FACE_OUTER_BOUND ( 'NONE', #9401, .T. ) ;
#65160 = ORIENTED_EDGE ( 'NONE', *, *, #37442, .T. ) ;
#65161 = CARTESIAN_POINT ( 'NONE',  ( -93.84685191531252713, 88.00268892867056536, 76.51947916753380241 ) ) ;
#65162 = DIRECTION ( 'NONE',  ( -1.000000000000000000, 0.000000000000000000, 0.000000000000000000 ) ) ;
#65163 = CARTESIAN_POINT ( 'NONE',  ( -9.332068499558252128, 6.890028847512362553, -44.99999999999998579 ) ) ;
#65164 = DIRECTION ( 'NONE',  ( 0.9781476007338070211, 0.000000000000000000, -0.2079116908177526257 ) ) ;
#65165 = CARTESIAN_POINT ( 'NONE',  ( -94.99999999999997158, -206.9400435732949575, 79.12562500173429214 ) ) ;
#65166 = CARTESIAN_POINT ( 'NONE',  ( -96.15314808468747287, -208.0026889286704943, 87.79072916753381151 ) ) ;
#65167 =( LENGTH_UNIT ( ) NAMED_UNIT ( * ) SI_UNIT ( .MILLI., .METRE. ) );
#65168 = CYLINDRICAL_SURFACE ( 'NONE', #40103, 37.49900000000000233 ) ;
#65169 = CARTESIAN_POINT ( 'NONE',  ( 93.84685191531248449, 91.99731107132950569, 75.09072916753380866 ) ) ;
#65170 = EDGE_CURVE ( 'NONE', #17494, #68748, #10182, .T. ) ;
#65171 = CARTESIAN_POINT ( 'NONE',  ( -97.30629616937495996, -209.9999999999999716, 77.10156250086714635 ) ) ;
#65172 = CARTESIAN_POINT ( 'NONE',  ( 11.99999999999999822, -74.65374052328644439, -8.840884882375878107 ) ) ;
#65173 = VERTEX_POINT ( 'NONE', #63561 ) ;
#65174 = FACE_OUTER_BOUND ( 'NONE', #53151, .T. ) ;
#65175 = DIRECTION ( 'NONE',  ( 0.000000000000000000, -0.1045284632676436454, 0.9945218953682744001 ) ) ;
#65176 = CARTESIAN_POINT ( 'NONE',  ( 10.00000000000000000, 68.26794271651307611, -31.47745569255064169 ) ) ;
#65177 = VECTOR ( 'NONE', #69703, 1000.000000000000000 ) ;
#65178 = EDGE_CURVE ( 'NONE', #14992, #70524, #69915, .T. ) ;
#65179 = SHAPE_REPRESENTATION ( 'housing', ( #43395 ), #14652 ) ;
#65180 = DIRECTION ( 'NONE',  ( -1.000000000000000000, 0.000000000000000000, -0.000000000000000000 ) ) ;
#65181 = CARTESIAN_POINT ( 'NONE',  ( 96.15314808468750130, -211.9973110713294489, 75.24947916753380639 ) ) ;
#65182 = ORIENTED_EDGE ( 'NONE', *, *, #55588, .T. ) ;
#65183 = EDGE_CURVE ( 'NONE', #10228, #25590, #12770, .T. ) ;
#65184 = DIRECTION ( 'NONE',  ( -1.000000000000000000, -0.000000000000000000, 0.000000000000000000 ) ) ;
#65185 = CARTESIAN_POINT ( 'NONE',  ( 11.99999999999999822, 20.41045688087930898, -72.35160999960793049 ) ) ;
#65186 = ORIENTED_EDGE ( 'NONE', *, *, #8325, .F. ) ;
#65187 = EDGE_CURVE ( 'NONE', #53274, #6219, #66168, .T. ) ;
#65188 = FACE_OUTER_BOUND ( 'NONE', #30251, .T. ) ;
#65189 = VERTEX_POINT ( 'NONE', #57915 ) ;
#65190 = EDGE_CURVE ( 'NONE', #27660, #45520, #61331, .T. ) ;
#65191 = CARTESIAN_POINT ( 'NONE',  ( 11.99999999999999822, -44.99326035066103202, 68.55367621811127776 ) ) ;
#65192 = CIRCLE ( 'NONE', #36357, 31.99999999999998579 ) ;
#65193 = ORIENTED_EDGE ( 'NONE', *, *, #37002, .F. ) ;
#65194 = VERTEX_POINT ( 'NONE', #64657 ) ;
#65195 = ORIENTED_EDGE ( 'NONE', *, *, #23015, .F. ) ;
#65196 = DIRECTION ( 'NONE',  ( 0.000000000000000000, 0.000000000000000000, 1.000000000000000000 ) ) ;
#65197 = EDGE_LOOP ( 'NONE', ( #4730, #72862, #72006, #8733 ) ) ;
#65198 = VERTEX_POINT ( 'NONE', #53375 ) ;
#65199 = CARTESIAN_POINT ( 'NONE',  ( 92.69370383062498320, 90.00000000000002842, 78.37156250086715659 ) ) ;
#65200 = CARTESIAN_POINT ( 'NONE',  ( 0.000000000000000000, 16.61724383029390140, -20.69703378468904020 ) ) ;
#65201 = EDGE_CURVE ( 'NONE', #26020, #33066, #29319, .T. ) ;
#65202 = CARTESIAN_POINT ( 'NONE',  ( 7.400000000000003908, 1.056673655987569448E-14, 5.892267102770835596E-15 ) ) ;
#65203 = ORIENTED_EDGE ( 'NONE', *, *, #43471, .T. ) ;
#65204 = ORIENTED_EDGE ( 'NONE', *, *, #11990, .T. ) ;
#65205 = VERTEX_POINT ( 'NONE', #34597 ) ;
#65206 = DIRECTION ( 'NONE',  ( 0.000000000000000000, -0.2334453638558922350, -0.9723699203976797767 ) ) ;
#65207 = EDGE_LOOP ( 'NONE', ( #31430, #26800, #56622, #8038 ) ) ;
#65208 = CARTESIAN_POINT ( 'NONE',  ( 0.2325368248550523098, -0.7967600800029647212, -45.00000000000000000 ) ) ;
#65209 = DIRECTION ( 'NONE',  ( -1.000000000000000000, -0.000000000000000000, -0.000000000000000000 ) ) ;
#65210 = CARTESIAN_POINT ( 'NONE',  ( -93.41453557521646189, 91.70561969393801860, 74.79912739178801928 ) ) ;
#65211 = DIRECTION ( 'NONE',  ( 1.000000000000000000, 0.000000000000000000, 0.000000000000000000 ) ) ;
#65212 = LINE ( 'NONE', #13686, #21032 ) ;
#65213 = DIRECTION ( 'NONE',  ( -1.000000000000000000, -0.000000000000000000, 0.000000000000000000 ) ) ;
#65214 = DIRECTION ( 'NONE',  ( 1.000000000000000000, 0.000000000000000000, 0.000000000000000000 ) ) ;
#65215 = CARTESIAN_POINT ( 'NONE',  ( -92.34999999999999432, -209.9999999999999716, 77.06187500173429328 ) ) ;
#65216 = EDGE_CURVE ( 'NONE', #52827, #45343, #28564, .T. ) ;
#65217 = CARTESIAN_POINT ( 'NONE',  ( -96.15314808468752972, 91.99731107132950569, 88.42572916753381662 ) ) ;
#65218 = EDGE_CURVE ( 'NONE', #14622, #39686, #59029, .T. ) ;
#65219 = VECTOR ( 'NONE', #3313, 1000.000000000000000 ) ;
#65221 = CARTESIAN_POINT ( 'NONE',  ( -93.67500000000003979, 92.29496732002878900, 77.16770833506762983 ) ) ;
#65220 = CARTESIAN_POINT ( 'NONE',  ( 92.34999999999999432, 88.47002178664753558, 77.43229166840096411 ) ) ;
#65223 = ADVANCED_FACE ( 'NONE', ( #805 ), #68827, .F. ) ;
#65222 = VERTEX_POINT ( 'NONE', #58642 ) ;
#65224 = CARTESIAN_POINT ( 'NONE',  ( 93.84685191531248449, 88.00268892867053694, 77.84239583420048803 ) ) ;
#65225 = FACE_OUTER_BOUND ( 'NONE', #62817, .T. ) ;
#65226 = CARTESIAN_POINT ( 'NONE',  ( 97.64999999999999147, 90.00000000000002842, 90.00000000000000000 ) ) ;
#65227 = CARTESIAN_POINT ( 'NONE',  ( 96.32499999999998863, -207.7050326799711968, 77.16770833506762983 ) ) ;
#65228 = CARTESIAN_POINT ( 'NONE',  ( 11.99999999999999822, 0.000000000000000000, 0.000000000000000000 ) ) ;
#65229 = AXIS2_PLACEMENT_3D ( 'NONE', #65578, #36992, #32815 ) ;
#65230 = ORIENTED_EDGE ( 'NONE', *, *, #40309, .F. ) ;
#65231 = DIRECTION ( 'NONE',  ( 0.000000000000000000, 0.000000000000000000, 1.000000000000000000 ) ) ;
#65232 = CARTESIAN_POINT ( 'NONE',  ( 11.99999999999999822, 0.000000000000000000, 0.000000000000000000 ) ) ;
#65233 = ORIENTED_EDGE ( 'NONE', *, *, #65449, .F. ) ;
#65234 = AXIS2_PLACEMENT_3D ( 'NONE', #3156, #43373, #60653 ) ;
#65235 = ORIENTED_EDGE ( 'NONE', *, *, #41769, .F. ) ;
#65236 = DIRECTION ( 'NONE',  ( 0.000000000000000000, 0.000000000000000000, 1.000000000000000000 ) ) ;
#65237 = CARTESIAN_POINT ( 'NONE',  ( 10.00000000000000000, 0.000000000000000000, 0.000000000000000000 ) ) ;
#65238 = DIRECTION ( 'NONE',  ( -2.628368902995164490E-16, -1.000000000000000000, 0.000000000000000000 ) ) ;
#65239 = DIRECTION ( 'NONE',  ( -1.000000000000000000, 0.000000000000000000, 0.000000000000000000 ) ) ;
#65240 = CYLINDRICAL_SURFACE ( 'NONE', #52936, 31.99999999999999289 ) ;
#65241 = VECTOR ( 'NONE', #69427, 1000.000000000000000 ) ;
#65242 = DIRECTION ( 'NONE',  ( -1.000000000000000000, -0.000000000000000000, 0.000000000000000000 ) ) ;
#65243 = AXIS2_PLACEMENT_3D ( 'NONE', #14746, #14384, #30924 ) ;
#65244 = ORIENTED_EDGE ( 'NONE', *, *, #40419, .F. ) ;
#65245 = AXIS2_PLACEMENT_3D ( 'NONE', #62631, #5852, #17119 ) ;
#65246 = CARTESIAN_POINT ( 'NONE',  ( 10.00000000000000000, -21.40280677340398441, 36.13751322684410638 ) ) ;
#65247 = VECTOR ( 'NONE', #39446, 1000.000000000000000 ) ;
#65248 = CIRCLE ( 'NONE', #13594, 31.99999999999999289 ) ;
#65249 = AXIS2_PLACEMENT_3D ( 'NONE', #13362, #59236, #46473 ) ;
#65250 = CARTESIAN_POINT ( 'NONE',  ( 0.000000000000000000, -26.79245525562690844, -32.34446384430000876 ) ) ;
#65251 = CARTESIAN_POINT ( 'NONE',  ( 10.00000000000000000, -37.58145647212455032, 16.68533520207890319 ) ) ;
#65252 = DIRECTION ( 'NONE',  ( -1.000000000000000000, 0.000000000000000000, -0.000000000000000000 ) ) ;
#65253 = CARTESIAN_POINT ( 'NONE',  ( -0.4301293587032979371, -118.5629931333561871, 2.500000000000000000 ) ) ;
#65254 = DIRECTION ( 'NONE',  ( 0.000000000000000000, 0.3090169943749482839, -0.9510565162951533091 ) ) ;
#65255 = CYLINDRICAL_SURFACE ( 'NONE', #64963, 31.99999999999998579 ) ;
#65256 = DIRECTION ( 'NONE',  ( 0.4565542962317865050, 0.000000000000000000, 0.8896955516311735312 ) ) ;
#65257 = CARTESIAN_POINT ( 'NONE',  ( 97.64999999999999147, 90.00000000000002842, 90.00000000000000000 ) ) ;
#65258 = EDGE_CURVE ( 'NONE', #44809, #30760, #30427, .T. ) ;
#65259 = CARTESIAN_POINT ( 'NONE',  ( 92.69370383062498320, 90.00000000000002842, 83.45156250086715488 ) ) ;
#65260 = CARTESIAN_POINT ( 'NONE',  ( -93.84685191531247028, -211.9973110713294489, 88.10822916753382117 ) ) ;
#65261 = CARTESIAN_POINT ( 'NONE',  ( 92.35000000000000853, -209.9999999999999716, 90.00000000000000000 ) ) ;
#65262 = ORIENTED_EDGE ( 'NONE', *, *, #63036, .F. ) ;
#65263 = CARTESIAN_POINT ( 'NONE',  ( -97.64999999999984936, -211.5299782133525071, 81.16291666666667481 ) ) ;
#65264 = CARTESIAN_POINT ( 'NONE',  ( -93.67499999999998295, -212.2949673200287179, 80.68666666666665321 ) ) ;
#65265 = CARTESIAN_POINT ( 'NONE',  ( -97.30629616937501680, 88.66845928578038638, 75.72572916753381378 ) ) ;
#65266 = EDGE_CURVE ( 'NONE', #48094, #18937, #7146, .T. ) ;
#65267 = CARTESIAN_POINT ( 'NONE',  ( 95.00000000000000000, -207.3369185715606307, 86.30906250086715659 ) ) ;
#65268 = ORIENTED_EDGE ( 'NONE', *, *, #33415, .T. ) ;
#65269 = ADVANCED_FACE ( 'NONE', ( #40620 ), #63196, .T. ) ;
#65270 = VECTOR ( 'NONE', #48553, 1000.000000000000000 ) ;
#65271 = DIRECTION ( 'NONE',  ( -0.5200609990132993854, -0.8541291221503275466, 0.000000000000000000 ) ) ;
#65272 = ORIENTED_EDGE ( 'NONE', *, *, #73643, .T. ) ;
#65273 =( BOUNDED_CURVE ( )  B_SPLINE_CURVE ( 2, ( #18603, #17502, #69740, #40816, #63753, #29141, #47556 ),
 .UNSPECIFIED., .F., .F. ) 
 B_SPLINE_CURVE_WITH_KNOTS ( ( 3, 2, 2, 3 ),
 ( 0.1693384224419976214, 0.1763941385220586799, 0.1834499040629413436, 0.1905056698837213069 ),
 .UNSPECIFIED. ) 
 CURVE ( )  GEOMETRIC_REPRESENTATION_ITEM ( )  RATIONAL_B_SPLINE_CURVE ( ( 0.9999981216929294536, 0.8660263429445574923, 1.000000000000000000, 0.8660254037844387076, 1.000000000000000000, 0.8660254037844387076, 1.000000000000000000 ) ) 
 REPRESENTATION_ITEM ( '' )  );
#65274 = ORIENTED_EDGE ( 'NONE', *, *, #52648, .F. ) ;
#65275 = EDGE_CURVE ( 'NONE', #64110, #65939, #9688, .T. ) ;
#65276 = FILL_AREA_STYLE_COLOUR ( '', #5079 ) ;
#65277 = ADVANCED_FACE ( 'NONE', ( #46627 ), #52261, .T. ) ;
#65278 = CARTESIAN_POINT ( 'NONE',  ( -97.65000000000001990, 88.47002178664754979, 79.33729166840096525 ) ) ;
#65279 = CARTESIAN_POINT ( 'NONE',  ( 0.000000000000000000, -76.41127070299280888, 12.93880638057290788 ) ) ;
#65280 = ORIENTED_EDGE ( 'NONE', *, *, #1674, .T. ) ;
#65281 = CARTESIAN_POINT ( 'NONE',  ( 12.00000000000000000, 6.762365576493647445, 25.66652317338391498 ) ) ;
#65282 = CARTESIAN_POINT ( 'NONE',  ( 92.69370383062501162, -208.6684592857803295, 79.58864583420049144 ) ) ;
#65283 = CARTESIAN_POINT ( 'NONE',  ( -11.69999999999999929, 0.000000000000000000, -20.99999999999999645 ) ) ;
#65284 = FACE_OUTER_BOUND ( 'NONE', #32159, .T. ) ;
#65285 = VECTOR ( 'NONE', #48172, 1000.000000000000000 ) ;
#65286 = FACE_OUTER_BOUND ( 'NONE', #63989, .T. ) ;
#65287 = CARTESIAN_POINT ( 'NONE',  ( 94.99999999999998579, 86.94004357329502852, 76.82374999999998977 ) ) ;
#65288 = VECTOR ( 'NONE', #59800, 1000.000000000000000 ) ;
#65289 = EDGE_CURVE ( 'NONE', #42030, #38665, #62524, .T. ) ;
#65290 = DIRECTION ( 'NONE',  ( -1.000000000000000000, 0.000000000000000000, 0.000000000000000000 ) ) ;
#65291 = CARTESIAN_POINT ( 'NONE',  ( 92.35000000000002274, -208.4700217866474645, 80.42208333333331893 ) ) ;
#65292 = VERTEX_POINT ( 'NONE', #35352 ) ;
#65293 = VERTEX_POINT ( 'NONE', #29683 ) ;
#65294 = VERTEX_POINT ( 'NONE', #24081 ) ;
#65295 = ORIENTED_EDGE ( 'NONE', *, *, #8387, .T. ) ;
#65296 = DIRECTION ( 'NONE',  ( 0.000000000000000000, -6.938893903907228378E-15, 1.000000000000000000 ) ) ;
#65297 = AXIS2_PLACEMENT_3D ( 'NONE', #4897, #50350, #39086 ) ;
#65298 =( NAMED_UNIT ( * ) SI_UNIT ( $, .STERADIAN. ) SOLID_ANGLE_UNIT ( ) );
#65299 = CARTESIAN_POINT ( 'NONE',  ( -97.30629616937501680, 88.66845928578038638, 82.86947916753382515 ) ) ;
#65300 = DIRECTION ( 'NONE',  ( -1.000000000000000000, -0.000000000000000000, 0.000000000000000000 ) ) ;
#65301 = DIRECTION ( 'NONE',  ( 0.000000000000000000, 0.000000000000000000, 1.000000000000000000 ) ) ;
#65302 = CARTESIAN_POINT ( 'NONE',  ( 97.64999999999997726, 88.47002178664753558, 75.65958333333333030 ) ) ;
#65303 = ORIENTED_EDGE ( 'NONE', *, *, #66536, .T. ) ;
#65304 = CARTESIAN_POINT ( 'NONE',  ( -97.64999999999994884, -208.4700217866474645, 88.12145833506762926 ) ) ;
#65306 = ORIENTED_EDGE ( 'NONE', *, *, #58490, .T. ) ;
#65305 = EDGE_CURVE ( 'NONE', #29501, #33770, #47004, .T. ) ;
#65307 = ADVANCED_FACE ( 'NONE', ( #2658 ), #37937, .T. ) ;
#65308 = DIRECTION ( 'NONE',  ( 0.000000000000000000, 0.4539904997395479702, -0.8910065241883673437 ) ) ;
#65309 = ORIENTED_EDGE ( 'NONE', *, *, #64446, .F. ) ;
#65310 = CARTESIAN_POINT ( 'NONE',  ( -92.35000000000003695, 90.00000000000004263, 84.68187500173429783 ) ) ;
#65311 = EDGE_CURVE ( 'NONE', #14991, #62129, #52955, .T. ) ;
#65312 = CARTESIAN_POINT ( 'NONE',  ( 93.84685191531248449, 91.99731107132950569, 85.25072916753381946 ) ) ;
#65313 = CARTESIAN_POINT ( 'NONE',  ( 10.00000000000000000, 33.79645857604513992, -16.45098606841138178 ) ) ;
#65314 = CIRCLE ( 'NONE', #28052, 31.99999999999998934 ) ;
#65315 = CARTESIAN_POINT ( 'NONE',  ( 10.00000000000000000, -27.13269053701078448, -25.88420570971428702 ) ) ;
#65316 = DIRECTION ( 'NONE',  ( 1.000000000000000000, 0.000000000000000000, 0.000000000000000000 ) ) ;
#65317 = CARTESIAN_POINT ( 'NONE',  ( 11.99999999999999822, 46.21855187248630870, 62.20884554314035597 ) ) ;
#65318 = ORIENTED_EDGE ( 'NONE', *, *, #39127, .T. ) ;
#65319 = CARTESIAN_POINT ( 'NONE',  ( 11.99999999999999822, 31.46837873495072913, -68.27212725128242710 ) ) ;
#65320 = CARTESIAN_POINT ( 'NONE',  ( 15.00000000000000000, -3.948201729842032215, 23.21447184625297666 ) ) ;
#65321 = ORIENTED_EDGE ( 'NONE', *, *, #35471, .T. ) ;
#65322 = ORIENTED_EDGE ( 'NONE', *, *, #23089, .T. ) ;
#65323 = FACE_OUTER_BOUND ( 'NONE', #69966, .T. ) ;
#65324 = CARTESIAN_POINT ( 'NONE',  ( 11.99999999999999822, -62.20884554314051229, 46.21855187248609553 ) ) ;
#65325 = CIRCLE ( 'NONE', #14916, 15.80000000000028315 ) ;
#65326 = CARTESIAN_POINT ( 'NONE',  ( 16.30584220631899228, -140.9432449716519784, -5.500000000000000000 ) ) ;
#65327 = CARTESIAN_POINT ( 'NONE',  ( -92.69370383062498320, -208.6684592857803011, 89.53697916753382913 ) ) ;
#65328 = ORIENTED_EDGE ( 'NONE', *, *, #30992, .F. ) ;
#65329 =( NAMED_UNIT ( * ) SI_UNIT ( $, .STERADIAN. ) SOLID_ANGLE_UNIT ( ) );
#65330 = ORIENTED_EDGE ( 'NONE', *, *, #8212, .F. ) ;
#65331 = ORIENTED_EDGE ( 'NONE', *, *, #58058, .T. ) ;
#65332 = CARTESIAN_POINT ( 'NONE',  ( 0.000000000000000000, -120.0000000000000000, -2.500000000000000000 ) ) ;
#65333 = AXIS2_PLACEMENT_3D ( 'NONE', #67121, #33648, #44946 ) ;
#65334 = CARTESIAN_POINT ( 'NONE',  ( 97.30629616937498838, 90.00000000000002842, 88.84906250086716284 ) ) ;
#65335 = CARTESIAN_POINT ( 'NONE',  ( 94.99999999999998579, 90.00000000000002842, 75.00000000000000000 ) ) ;
#65336 = CARTESIAN_POINT ( 'NONE',  ( 97.30629616937498838, 91.33154071421968467, 82.39322916753381776 ) ) ;
#65337 = DIRECTION ( 'NONE',  ( 0.8571673007021122226, 0.000000000000000000, 0.5150380749100542666 ) ) ;
#65338 = DIRECTION ( 'NONE',  ( 0.000000000000000000, -0.9510565162951500895, -0.3090169943749581649 ) ) ;
#65339 = CARTESIAN_POINT ( 'NONE',  ( -97.64999999999997726, 91.52997821335256390, 85.50208333333331723 ) ) ;
#65340 = CYLINDRICAL_SURFACE ( 'NONE', #26746, 77.49899999999999523 ) ;
#65341 = FACE_OUTER_BOUND ( 'NONE', #42304, .T. ) ;
#65342 = CARTESIAN_POINT ( 'NONE',  ( 11.99999999999999822, -66.50666863322028632, 39.78640506895582973 ) ) ;
#65343 = EDGE_CURVE ( 'NONE', #51588, #58261, #21706, .T. ) ;
#65344 = AXIS2_PLACEMENT_3D ( 'NONE', #45043, #16463, #39399 ) ;
#65345 = CIRCLE ( 'NONE', #36559, 82.00000000000000000 ) ;
#65346 = DIRECTION ( 'NONE',  ( 0.000000000000000000, 0.000000000000000000, 1.000000000000000000 ) ) ;
#65347 = EDGE_CURVE ( 'NONE', #19224, #70328, #31313, .T. ) ;
#65348 = CARTESIAN_POINT ( 'NONE',  ( 10.00000000000000000, 9.188173127307898369, -40.98264845739739570 ) ) ;
#65349 = ORIENTED_EDGE ( 'NONE', *, *, #53449, .T. ) ;
#65350 = AXIS2_PLACEMENT_3D ( 'NONE', #11507, #34439, #28808 ) ;
#65351 = CARTESIAN_POINT ( 'NONE',  ( -92.69370383062505425, 88.66845928578038638, 86.73239583420047438 ) ) ;
#65352 = CIRCLE ( 'NONE', #56978, 15.99999999999999822 ) ;
#65353 = CARTESIAN_POINT ( 'NONE',  ( 0.000000000000000000, -0.8299999999999999600, 0.000000000000000000 ) ) ;
#65354 = EDGE_CURVE ( 'NONE', #55116, #60419, #36813, .T. ) ;
#65355 = EDGE_CURVE ( 'NONE', #5291, #30315, #8989, .T. ) ;
#65356 = DIRECTION ( 'NONE',  ( -1.000000000000000000, -0.000000000000000000, -0.000000000000000000 ) ) ;
#65357 = AXIS2_PLACEMENT_3D ( 'NONE', #15323, #49172, #71346 ) ;
#65358 = ORIENTED_EDGE ( 'NONE', *, *, #29092, .T. ) ;
#65359 = CARTESIAN_POINT ( 'NONE',  ( 0.000000000000000000, 16.00000000000000000, 2.500000000000000000 ) ) ;
#65360 = CARTESIAN_POINT ( 'NONE',  ( 5.000000000000000000, 64.81221759200417409, -50.23322058963276504 ) ) ;
#65361 = CARTESIAN_POINT ( 'NONE',  ( 92.34999999999999432, 90.00000000000002842, 82.37999999999999545 ) ) ;
#65362 = AXIS2_PLACEMENT_3D ( 'NONE', #34684, #46345, #41804 ) ;
#65363 = ADVANCED_FACE ( 'NONE', ( #49205 ), #60869, .T. ) ;
#65364 = CARTESIAN_POINT ( 'NONE',  ( 96.15314808468750130, -211.9973110713294489, 83.02822916753380866 ) ) ;
#65365 = ORIENTED_EDGE ( 'NONE', *, *, #11964, .T. ) ;
#65366 = ORIENTED_EDGE ( 'NONE', *, *, #32976, .T. ) ;
#65367 = DIRECTION ( 'NONE',  ( -0.5000000000000006661, -0.8660254037844382635, 0.000000000000000000 ) ) ;
#65368 = ORIENTED_EDGE ( 'NONE', *, *, #17580, .T. ) ;
#65369 = AXIS2_PLACEMENT_3D ( 'NONE', #57374, #46097, #16031 ) ;
#65370 = EDGE_CURVE ( 'NONE', #11290, #57825, #19296, .T. ) ;
#65371 = DIRECTION ( 'NONE',  ( -0.7533909544171994987, -0.6575728627325958531, 2.465190328815662439E-32 ) ) ;
#65372 = DIRECTION ( 'NONE',  ( -1.000000000000000000, -0.000000000000000000, 0.000000000000000000 ) ) ;
#65374 = ORIENTED_EDGE ( 'NONE', *, *, #66532, .T. ) ;
#65373 = EDGE_CURVE ( 'NONE', #69413, #23763, #9354, .T. ) ;
#65375 = CARTESIAN_POINT ( 'NONE',  ( 92.69370383062501162, -209.9999999999999716, 79.00656250086716170 ) ) ;
#65376 = ORIENTED_EDGE ( 'NONE', *, *, #17184, .T. ) ;
#65377 = DIRECTION ( 'NONE',  ( -1.000000000000000000, 0.000000000000000000, -0.000000000000000000 ) ) ;
#65378 = ORIENTED_EDGE ( 'NONE', *, *, #16028, .T. ) ;
#65379 = ADVANCED_FACE ( 'NONE', ( #59762 ), #30793, .F. ) ;
#65380 = ORIENTED_EDGE ( 'NONE', *, *, #69994, .F. ) ;
#65381 = DIRECTION ( 'NONE',  ( 0.000000000000000000, -1.000000000000000000, 0.000000000000000000 ) ) ;
#65382 = CIRCLE ( 'NONE', #61786, 62.50000000000000000 ) ;
#65383 = CARTESIAN_POINT ( 'NONE',  ( -93.67500000000003979, 92.29496732002878900, 82.80333333333332746 ) ) ;
#65384 = EDGE_LOOP ( 'NONE', ( #56022, #15053, #33552, #30660 ) ) ;
#65385 = CARTESIAN_POINT ( 'NONE',  ( 92.35000000000002274, -211.5299782133524502, 82.51229166840094820 ) ) ;
#65386 = CARTESIAN_POINT ( 'NONE',  ( 93.67499999999999716, 87.70503267997126784, 86.29583333333333428 ) ) ;
#65387 = ORIENTED_EDGE ( 'NONE', *, *, #2246, .T. ) ;
#65388 = DIRECTION ( 'NONE',  ( 0.000000000000000000, 0.000000000000000000, -1.000000000000000000 ) ) ;
#65389 = EDGE_CURVE ( 'NONE', #43729, #24000, #71754, .T. ) ;
#65390 = CARTESIAN_POINT ( 'NONE',  ( -94.95306897617113862, 87.35041560265752025, 75.00000002508417651 ) ) ;
#65391 = CIRCLE ( 'NONE', #43774, 16.00000000000000000 ) ;
#65392 = ORIENTED_EDGE ( 'NONE', *, *, #64967, .T. ) ;
#65393 = ORIENTED_EDGE ( 'NONE', *, *, #7951, .T. ) ;
#65394 = CARTESIAN_POINT ( 'NONE',  ( -92.69370383062505425, 91.33154071421968467, 86.99697916753382287 ) ) ;
#65395 = AXIS2_PLACEMENT_3D ( 'NONE', #29364, #16994, #63236 ) ;
#65396 = ADVANCED_FACE ( 'NONE', ( #8243 ), #70642, .T. ) ;
#65397 = CARTESIAN_POINT ( 'NONE',  ( 94.99999999999998579, 92.66308142843935514, 80.59406250086715318 ) ) ;
#65398 = CIRCLE ( 'NONE', #32957, 12.50000000000000000 ) ;
#65399 = ORIENTED_EDGE ( 'NONE', *, *, #71287, .T. ) ;
#65400 = CARTESIAN_POINT ( 'NONE',  ( 94.99999999999998579, 86.94004357329500010, 85.79312500173431033 ) ) ;
#65401 = EDGE_CURVE ( 'NONE', #66590, #54849, #3706, .T. ) ;
#65402 = LINE ( 'NONE', #48463, #67269 ) ;
#65403 = EDGE_LOOP ( 'NONE', ( #35166, #22648, #18786 ) ) ;
#65404 = FACE_BOUND ( 'NONE', #57831, .T. ) ;
#65405 = AXIS2_PLACEMENT_3D ( 'NONE', #36216, #70406, #18916 ) ;
#65406 = ORIENTED_EDGE ( 'NONE', *, *, #45168, .F. ) ;
#65407 = ORIENTED_EDGE ( 'NONE', *, *, #33505, .T. ) ;
#65408 = ORIENTED_EDGE ( 'NONE', *, *, #38618, .F. ) ;
#65409 = LINE ( 'NONE', #31172, #37288 ) ;
#65411 = AXIS2_PLACEMENT_3D ( 'NONE', #21482, #43346, #15481 ) ;
#65410 = CARTESIAN_POINT ( 'NONE',  ( 1.243286885786405054E-17, -120.0000000000000000, -80.00000000000001421 ) ) ;
#65412 = CARTESIAN_POINT ( 'NONE',  ( -96.32500000000001705, 87.70503267997129626, 83.75583333333332803 ) ) ;
#65413 = ORIENTED_EDGE ( 'NONE', *, *, #40131, .T. ) ;
#65414 = DIRECTION ( 'NONE',  ( -0.000000000000000000, -0.000000000000000000, 1.000000000000000000 ) ) ;
#65415 = VECTOR ( 'NONE', #7841, 999.9999999999998863 ) ;
#65416 = CYLINDRICAL_SURFACE ( 'NONE', #34702, 16.00000000000000000 ) ;
#65417 = VERTEX_POINT ( 'NONE', #14628 ) ;
#65418 = DIRECTION ( 'NONE',  ( 0.000000000000000000, 0.000000000000000000, 1.000000000000000000 ) ) ;
#65419 = CARTESIAN_POINT ( 'NONE',  ( -97.30629616937495996, -209.9999999999999716, 82.65781250086713783 ) ) ;
#65420 = ORIENTED_EDGE ( 'NONE', *, *, #42616, .F. ) ;
#65421 = CARTESIAN_POINT ( 'NONE',  ( 0.000000000000000000, -72.35432306680469594, -20.40083707022958848 ) ) ;
#65422 = CARTESIAN_POINT ( 'NONE',  ( 0.000000000000000000, -30.80686688396994910, -21.53537804866113703 ) ) ;
#65423 = CARTESIAN_POINT ( 'NONE',  ( 92.34999999999999432, 90.00000000000002842, 89.44437500173430067 ) ) ;
#65424 = CARTESIAN_POINT ( 'NONE',  ( 0.000000000000000000, -81.96053171279901051, -2.543863470249246195 ) ) ;
#65425 = AXIS2_PLACEMENT_3D ( 'NONE', #73984, #62743, #11211 ) ;
#65426 = CARTESIAN_POINT ( 'NONE',  ( -9.937067298023311679, 7.583184918921313411, 125.0000000000000000 ) ) ;
#65427 = CARTESIAN_POINT ( 'NONE',  ( -23.54415474984308787, -120.4156646670583086, 2.500000000000000000 ) ) ;
#65428 = DIRECTION ( 'NONE',  ( 0.000000000000000000, 0.9238795325112877377, -0.3826834323650873948 ) ) ;
#65429 = DIRECTION ( 'NONE',  ( 0.000000000000000000, 0.000000000000000000, 1.000000000000000000 ) ) ;
#65430 = CARTESIAN_POINT ( 'NONE',  ( 97.64999999997402824, 89.99998827382246702, 82.77687459617033028 ) ) ;
#65431 = DIRECTION ( 'NONE',  ( -1.000000000000000000, -0.000000000000000000, -0.000000000000000000 ) ) ;
#65432 = CARTESIAN_POINT ( 'NONE',  ( -92.69370383062504004, 90.00000000000004263, 75.35531250086714294 ) ) ;
#65433 = DIRECTION ( 'NONE',  ( -1.000000000000000000, 0.000000000000000000, 0.000000000000000000 ) ) ;
#65434 = CARTESIAN_POINT ( 'NONE',  ( -43.60332556124591719, -117.0000000000000000, -2.500000000000002220 ) ) ;
#65435 = PLANE ( 'NONE',  #54811 ) ;
#65436 = UNCERTAINTY_MEASURE_WITH_UNIT (LENGTH_MEASURE( 1.000000000000000082E-05 ), #44088, 'distance_accuracy_value', 'NONE');
#65437 = CARTESIAN_POINT ( 'NONE',  ( 0.000000000000000000, 21.53537804866126137, -30.80686688396986028 ) ) ;
#65438 = EDGE_CURVE ( 'NONE', #66007, #68543, #55307, .T. ) ;
#65439 = DIRECTION ( 'NONE',  ( -1.000000000000000000, 0.000000000000000000, -0.000000000000000000 ) ) ;
#65440 = CARTESIAN_POINT ( 'NONE',  ( 0.000000000000000000, -120.0000000000000000, 102.9091629284897493 ) ) ;
#65441 = CIRCLE ( 'NONE', #59420, 11.59999999999999787 ) ;
#65442 = CARTESIAN_POINT ( 'NONE',  ( 11.99999999999999822, 23.16143007188426850, 73.95703589263983702 ) ) ;
#65443 = EDGE_CURVE ( 'NONE', #67992, #15234, #64927, .T. ) ;
#65444 = DIRECTION ( 'NONE',  ( -1.000000000000000000, -0.000000000000000000, 0.000000000000000000 ) ) ;
#65445 = CARTESIAN_POINT ( 'NONE',  ( 0.000000000000000000, 35.38097989696512968, 12.42422080174651100 ) ) ;
#65446 = CARTESIAN_POINT ( 'NONE',  ( -92.34999999999999432, -208.4700217866474645, 86.56041666666665435 ) ) ;
#65447 = EDGE_CURVE ( 'NONE', #44202, #17922, #36264, .T. ) ;
#65448 = CARTESIAN_POINT ( 'NONE',  ( 24.94940289813197509, -237.3777120880564553, 5.500000000000000000 ) ) ;
#65449 = EDGE_CURVE ( 'NONE', #43589, #19072, #38682, .T. ) ;
#65450 = ORIENTED_EDGE ( 'NONE', *, *, #5244, .T. ) ;
#65451 = AXIS2_PLACEMENT_3D ( 'NONE', #40205, #23649, #6373 ) ;
#65452 = CARTESIAN_POINT ( 'NONE',  ( 15.00000000000000000, 16.83928648764922542, -16.46020748918050458 ) ) ;
#65453 = DIRECTION ( 'NONE',  ( 1.000000000000000000, 0.000000000000000000, -0.000000000000000000 ) ) ;
#65454 = LINE ( 'NONE', #31583, #57418 ) ;
#65455 = CARTESIAN_POINT ( 'NONE',  ( 6.000000000000000000, 34.94270380257639630, 74.18225833017899618 ) ) ;
#65456 = AXIS2_PLACEMENT_3D ( 'NONE', #12355, #50069, #10598 ) ;
#65457 = AXIS2_PLACEMENT_3D ( 'NONE', #49136, #31469, #48032 ) ;
#65458 = ORIENTED_EDGE ( 'NONE', *, *, #71635, .T. ) ;
#65459 = LINE ( 'NONE', #25228, #51497 ) ;
#65460 = DIRECTION ( 'NONE',  ( -1.000000000000000000, 0.000000000000000000, 0.000000000000000000 ) ) ;
#65461 = EDGE_LOOP ( 'NONE', ( #17069, #57328, #15098, #70522 ) ) ;
#65462 = CARTESIAN_POINT ( 'NONE',  ( 92.69370383062501162, -211.3315407142195852, 83.34572916753381833 ) ) ;
#65463 = CARTESIAN_POINT ( 'NONE',  ( 97.30629616937498838, -209.9999999999999716, 88.84906250086716284 ) ) ;
#65464 = ORIENTED_EDGE ( 'NONE', *, *, #49036, .F. ) ;
#65465 = AXIS2_PLACEMENT_3D ( 'NONE', #34051, #53197, #52443 ) ;
#65466 = CARTESIAN_POINT ( 'NONE',  ( 97.30629616937498838, -208.6684592857803011, 88.90197916753382401 ) ) ;
#65467 = VERTEX_POINT ( 'NONE', #67251 ) ;
#65468 = FACE_BOUND ( 'NONE', #35805, .T. ) ;
#65469 = EDGE_LOOP ( 'NONE', ( #71451, #33376, #72450, #17112 ) ) ;
#65470 = EDGE_CURVE ( 'NONE', #68435, #60775, #70911, .T. ) ;
#65471 = EDGE_CURVE ( 'NONE', #20976, #38823, #16488, .T. ) ;
#65472 = CARTESIAN_POINT ( 'NONE',  ( -96.15314808468751551, 88.00268892867056536, 75.93739583420048689 ) ) ;
#65473 = VERTEX_POINT ( 'NONE', #61991 ) ;
#65474 = AXIS2_PLACEMENT_3D ( 'NONE', #18986, #47573, #59601 ) ;
#65475 = ORIENTED_EDGE ( 'NONE', *, *, #48775, .F. ) ;
#65476 = CARTESIAN_POINT ( 'NONE',  ( 11.99999999999999822, 71.87247863392470038, -39.47590169984768949 ) ) ;
#65477 = VERTEX_POINT ( 'NONE', #39429 ) ;
#65478 = CARTESIAN_POINT ( 'NONE',  ( 96.32499999999998863, -207.7050326799711968, 84.78770833506763438 ) ) ;
#65479 = ORIENTED_EDGE ( 'NONE', *, *, #14839, .T. ) ;
#65480 = DIRECTION ( 'NONE',  ( -1.000000000000000000, 0.000000000000000000, -0.000000000000000000 ) ) ;
#65481 = EDGE_CURVE ( 'NONE', #52479, #66194, #5549, .T. ) ;
#65482 = VERTEX_POINT ( 'NONE', #68380 ) ;
#65483 =( BOUNDED_CURVE ( )  B_SPLINE_CURVE ( 2, ( #30569, #52780, #59531, #19294, #53145, #47505, #46395 ),
 .UNSPECIFIED., .F., .F. ) 
 B_SPLINE_CURVE_WITH_KNOTS ( ( 3, 2, 2, 3 ),
 ( 0.06350193517735455706, 0.07055765540882334708, 0.07761342094970608008, 0.08466915177892317401 ),
 .UNSPECIFIED. ) 
 CURVE ( )  GEOMETRIC_REPRESENTATION_ITEM ( )  RATIONAL_B_SPLINE_CURVE ( ( 0.9999982793443398243, 0.8660262641177934873, 1.000000000000000000, 0.8660254037844387076, 1.000000000000000000, 0.8660260628881689682, 0.9999986817990245136 ) ) 
 REPRESENTATION_ITEM ( '' )  );
#65484 = DIRECTION ( 'NONE',  ( -1.000000000000000000, -0.000000000000000000, -0.000000000000000000 ) ) ;
#65485 = ORIENTED_EDGE ( 'NONE', *, *, #59405, .F. ) ;
#65486 = ORIENTED_EDGE ( 'NONE', *, *, #5359, .F. ) ;
#65487 = EDGE_LOOP ( 'NONE', ( #66819, #52051, #51931, #55367 ) ) ;
#65488 = CARTESIAN_POINT ( 'NONE',  ( 97.30629616937498838, -211.3315407142195852, 78.47739583420047893 ) ) ;
#65489 = DIRECTION ( 'NONE',  ( 0.000000000000000000, 0.000000000000000000, 1.000000000000000000 ) ) ;
#65490 = CARTESIAN_POINT ( 'NONE',  ( 10.00000000000000000, 5.256550761633969060, -77.32052557432835727 ) ) ;
#65491 = VERTEX_POINT ( 'NONE', #16869 ) ;
#65492 = DIRECTION ( 'NONE',  ( 0.000000000000000000, 0.000000000000000000, 1.000000000000000000 ) ) ;
#65493 = EDGE_LOOP ( 'NONE', ( #49090, #21958, #29118, #63327 ) ) ;
#65494 = CARTESIAN_POINT ( 'NONE',  ( -3.000000000000000000, 3.673940397442059868E-16, -6.000000000000001776 ) ) ;
#65495 = DIRECTION ( 'NONE',  ( 0.000000000000000000, 0.8660254037844384856, -0.5000000000000004441 ) ) ;
#65496 = DIRECTION ( 'NONE',  ( 0.000000000000000000, 0.07845909572783793529, 0.9969173337331285190 ) ) ;
#65497 = CARTESIAN_POINT ( 'NONE',  ( 10.00000000000000000, -37.16516213103280108, 4.992566952384862589 ) ) ;
#65498 = CARTESIAN_POINT ( 'NONE',  ( -96.15314808468747287, -208.0026889286704943, 82.55197916753380127 ) ) ;
#65499 = CARTESIAN_POINT ( 'NONE',  ( -97.30629616937501680, 91.33154071421968467, 78.95364583420048632 ) ) ;
#65500 = ORIENTED_EDGE ( 'NONE', *, *, #74108, .T. ) ;
#65501 = CARTESIAN_POINT ( 'NONE',  ( 97.30629616937498838, 88.66845928578037217, 81.01739583420048518 ) ) ;
#65502 = EDGE_LOOP ( 'NONE', ( #9418, #36935, #32436, #3647 ) ) ;
#65503 = FACE_OUTER_BOUND ( 'NONE', #28920, .T. ) ;
#65505 = CIRCLE ( 'NONE', #42686, 16.00000000000000000 ) ;
#65504 = DIRECTION ( 'NONE',  ( -1.000000000000000000, 0.000000000000000000, 0.000000000000000000 ) ) ;
#65506 = VECTOR ( 'NONE', #1731, 1000.000000000000000 ) ;
#65507 = DIRECTION ( 'NONE',  ( -0.000000000000000000, 0.000000000000000000, 1.000000000000000000 ) ) ;
#65508 = DIRECTION ( 'NONE',  ( 0.000000000000000000, 0.000000000000000000, 1.000000000000000000 ) ) ;
#65509 = CARTESIAN_POINT ( 'NONE',  ( -92.69370383062498320, -209.9999999999999716, 81.70531250086713726 ) ) ;
#65510 = LINE ( 'NONE', #2759, #7387 ) ;
#65511 = CARTESIAN_POINT ( 'NONE',  ( -26.41226275915097332, -122.1546173538626761, 2.500000000000000000 ) ) ;
#65512 = LINE ( 'NONE', #3844, #66066 ) ;
#65513 = ORIENTED_EDGE ( 'NONE', *, *, #35735, .T. ) ;
#65514 = ORIENTED_EDGE ( 'NONE', *, *, #74325, .T. ) ;
#65515 = DIRECTION ( 'NONE',  ( -1.000000000000000000, 0.000000000000000000, 0.000000000000000000 ) ) ;
#65516 = CARTESIAN_POINT ( 'NONE',  ( -95.00000000000002842, 86.94004357329504273, 76.18874999999999886 ) ) ;
#65517 = DIRECTION ( 'NONE',  ( -2.603472992746261562E-14, -2.546204323184492723E-14, 1.000000000000000000 ) ) ;
#65518 = CARTESIAN_POINT ( 'NONE',  ( -97.30629616937501680, 91.33154071421968467, 83.87489583420047268 ) ) ;
#65519 = CARTESIAN_POINT ( 'NONE',  ( -96.44578755843112106, -208.0396902886533894, 74.86947676125085138 ) ) ;
#65520 = CARTESIAN_POINT ( 'NONE',  ( -3.961125083139900749, -143.2122702051246677, 2.500000000000000000 ) ) ;
#65521 = CIRCLE ( 'NONE', #58315, 77.49899999999999523 ) ;
#65522 = DIRECTION ( 'NONE',  ( -0.000000000000000000, -2.312964634635746211E-15, 1.000000000000000000 ) ) ;
#65523 = ORIENTED_EDGE ( 'NONE', *, *, #7714, .T. ) ;
#65524 = CARTESIAN_POINT ( 'NONE',  ( -97.30629616937501680, 91.33154071421968467, 74.98489583420048632 ) ) ;
#65525 = AXIS2_PLACEMENT_3D ( 'NONE', #19712, #54677, #61058 ) ;
#65526 = ADVANCED_FACE ( 'NONE', ( #21753 ), #22129, .T. ) ;
#65527 = CARTESIAN_POINT ( 'NONE',  ( 12.00000000000000000, -0.9646360437375368635, -23.52805723605589705 ) ) ;
#65528 = CYLINDRICAL_SURFACE ( 'NONE', #51475, 77.49899999999999523 ) ;
#65529 = EDGE_CURVE ( 'NONE', #1257, #55684, #15704, .T. ) ;
#65530 = CARTESIAN_POINT ( 'NONE',  ( -4.829002333675109782, 2.985476894631601485, -1.879366290983708110 ) ) ;
#65531 = CARTESIAN_POINT ( 'NONE',  ( 2.500000000000000444, 8.494897427831771708, -10.00000000000000178 ) ) ;
#65532 = CARTESIAN_POINT ( 'NONE',  ( 93.67499999999999716, 87.70503267997126784, 86.29583333333333428 ) ) ;
#65533 = CARTESIAN_POINT ( 'NONE',  ( -94.99999999999997158, -212.6630814284392557, 81.70531250086715147 ) ) ;
#65534 = ADVANCED_FACE ( 'NONE', ( #73247 ), #50694, .F. ) ;
#65535 = DIRECTION ( 'NONE',  ( -1.000000000000000000, -0.000000000000000000, -0.000000000000000000 ) ) ;
#65536 = EDGE_CURVE ( 'NONE', #5511, #68580, #60207, .T. ) ;
#65537 = DIRECTION ( 'NONE',  ( 1.000000000000000000, 0.000000000000000000, 0.000000000000000000 ) ) ;
#65538 = CARTESIAN_POINT ( 'NONE',  ( 0.000000000000000000, -55.16347631942998220, -60.67117009219196433 ) ) ;
#65539 = DIRECTION ( 'NONE',  ( 0.000000000000000000, -0.6691306063588577935, -0.7431448254773946882 ) ) ;
#65540 = ORIENTED_EDGE ( 'NONE', *, *, #34616, .F. ) ;
#65541 = CARTESIAN_POINT ( 'NONE',  ( -97.64999999993850111, -209.9999881787635729, 81.82400613094797848 ) ) ;
#65542 = CARTESIAN_POINT ( 'NONE',  ( 0.000000000000000000, 50.23322058963348979, 64.81221759200361987 ) ) ;
#65543 = CARTESIAN_POINT ( 'NONE',  ( 15.70000000000000284, -120.0000000000000000, -90.00000000000000000 ) ) ;
#65544 = DIRECTION ( 'NONE',  ( -1.000000000000000000, -0.000000000000000000, -0.000000000000000000 ) ) ;
#65546 = EDGE_CURVE ( 'NONE', #3451, #16833, #26533, .T. ) ;
#65545 = CARTESIAN_POINT ( 'NONE',  ( 97.30629616937498838, -211.3315407142195852, 88.79614583420050167 ) ) ;
#65547 = ORIENTED_EDGE ( 'NONE', *, *, #52512, .T. ) ;
#65548 = EDGE_CURVE ( 'NONE', #30219, #14528, #8573, .T. ) ;
#65549 = CARTESIAN_POINT ( 'NONE',  ( 10.00000000000000000, -77.19088730480528682, 6.903761155837488062 ) ) ;
#65550 = DIRECTION ( 'NONE',  ( -0.000000000000000000, -0.000000000000000000, -1.000000000000000000 ) ) ;
#65551 = ORIENTED_EDGE ( 'NONE', *, *, #49158, .T. ) ;
#65552 = CARTESIAN_POINT ( 'NONE',  ( 0.000000000000000000, -21.53537804866058991, -30.80686688397033635 ) ) ;
#65553 = AXIS2_PLACEMENT_3D ( 'NONE', #39982, #46730, #41097 ) ;
#65554 = ORIENTED_EDGE ( 'NONE', *, *, #12645, .F. ) ;
#65555 = LINE ( 'NONE', #14029, #50199 ) ;
#65556 = AXIS2_PLACEMENT_3D ( 'NONE', #29860, #34397, #6934 ) ;
#65557 = EDGE_CURVE ( 'NONE', #47974, #5670, #38686, .T. ) ;
#65558 = EDGE_CURVE ( 'NONE', #64952, #70364, #50576, .T. ) ;
#65559 = ORIENTED_EDGE ( 'NONE', *, *, #64597, .T. ) ;
#65560 = AXIS2_PLACEMENT_3D ( 'NONE', #54805, #3334, #37897 ) ;
#65561 = ORIENTED_EDGE ( 'NONE', *, *, #39195, .T. ) ;
#65562 = VECTOR ( 'NONE', #23451, 1000.000000000000000 ) ;
#65563 = ORIENTED_EDGE ( 'NONE', *, *, #21526, .F. ) ;
#65564 = CARTESIAN_POINT ( 'NONE',  ( 15.00000000000000000, 8.688484142253932063, -21.88630264137371029 ) ) ;
#65565 = ORIENTED_EDGE ( 'NONE', *, *, #17803, .F. ) ;
#65566 = PRODUCT_DEFINITION_SHAPE ( 'NONE', 'NONE',  #74348 ) ;
#65567 = CIRCLE ( 'NONE', #29472, 42.00000000000000000 ) ;
#65568 = VECTOR ( 'NONE', #53028, 1000.000000000000000 ) ;
#65569 = EDGE_LOOP ( 'NONE', ( #58243, #28380, #65193, #14913 ) ) ;
#65570 = CARTESIAN_POINT ( 'NONE',  ( 92.69370383062498320, 91.33154071421968467, 81.49364583420047836 ) ) ;
#65571 = DIRECTION ( 'NONE',  ( -1.000000000000000000, -0.000000000000000000, -0.000000000000000000 ) ) ;
#65572 = CARTESIAN_POINT ( 'NONE',  ( 11.99999999999999822, 20.40083707022987625, -72.35432306680462489 ) ) ;
#65573 = ORIENTED_EDGE ( 'NONE', *, *, #48535, .T. ) ;
#65574 = EDGE_LOOP ( 'NONE', ( #60108, #32871, #43400, #8974 ) ) ;
#65575 = ORIENTED_EDGE ( 'NONE', *, *, #50937, .F. ) ;
#65576 = CARTESIAN_POINT ( 'NONE',  ( 0.000000000000000000, -17.28742895386031719, -75.54627589209962935 ) ) ;
#65577 = ORIENTED_EDGE ( 'NONE', *, *, #61604, .T. ) ;
#65578 = CARTESIAN_POINT ( 'NONE',  ( 8.499999999999992895, -72.99999999999998579, -255.0000000000000000 ) ) ;
#65579 = DIRECTION ( 'NONE',  ( 0.7950889364178796992, -0.6064928550163510845, 0.000000000000000000 ) ) ;
#65580 = STYLED_ITEM ( 'NONE', ( #24129 ), #37782 ) ;
#65581 = CARTESIAN_POINT ( 'NONE',  ( -97.64999999990722301, -209.9999861897314304, 80.55392363651652943 ) ) ;
#65582 = LINE ( 'NONE', #60680, #19727 ) ;
#65583 = FACE_OUTER_BOUND ( 'NONE', #124, .T. ) ;
#65584 = DIRECTION ( 'NONE',  ( 0.000000000000000000, 0.000000000000000000, -1.000000000000000000 ) ) ;
#65585 = DIRECTION ( 'NONE',  ( 1.000000000000000000, 0.000000000000000000, 0.000000000000000000 ) ) ;
#65586 = CARTESIAN_POINT ( 'NONE',  ( -93.67499999999998295, -212.2949673200287179, 76.95604166840095672 ) ) ;
#65587 = CARTESIAN_POINT ( 'NONE',  ( -92.69370383062504004, 90.00000000000004263, 88.84906250086716284 ) ) ;
#65589 = CARTESIAN_POINT ( 'NONE',  ( -92.35000000000003695, 90.00000000000004263, 77.69687500173431260 ) ) ;
#65588 = CARTESIAN_POINT ( 'NONE',  ( 93.67499999999999716, 87.70503267997126784, 77.48520833506763950 ) ) ;
#65590 = VERTEX_POINT ( 'NONE', #10471 ) ;
#65591 = CARTESIAN_POINT ( 'NONE',  ( 94.99999999999998579, 87.33691857156068750, 76.62531250086715318 ) ) ;
#65592 = CYLINDRICAL_SURFACE ( 'NONE', #34948, 82.00000000000000000 ) ;
#65593 = LINE ( 'NONE', #30613, #24703 ) ;
#65594 = CARTESIAN_POINT ( 'NONE',  ( 0.000000000000000000, -77.19088730480528682, 6.903761155837488062 ) ) ;
#65595 = DIRECTION ( 'NONE',  ( 0.000000000000000000, 0.000000000000000000, 1.000000000000000000 ) ) ;
#65596 = DIRECTION ( 'NONE',  ( 0.000000000000000000, 0.9510565162951521989, 0.3090169943749515591 ) ) ;
#65597 = ORIENTED_EDGE ( 'NONE', *, *, #46415, .T. ) ;
#65598 = DIRECTION ( 'NONE',  ( 0.000000000000000000, 0.4539904997395412534, 0.8910065241883706744 ) ) ;
#65599 = CYLINDRICAL_SURFACE ( 'NONE', #49239, 32.00000000000000000 ) ;
#65600 = EDGE_LOOP ( 'NONE', ( #51018, #19311, #6840, #50010 ) ) ;
#65601 = EDGE_LOOP ( 'NONE', ( #71271, #28212, #5483, #60613 ) ) ;
#65602 = EDGE_CURVE ( 'NONE', #42918, #66947, #33793, .T. ) ;
#65603 = DIRECTION ( 'NONE',  ( 0.000000000000000000, 0.000000000000000000, 1.000000000000000000 ) ) ;
#65604 = DIRECTION ( 'NONE',  ( 0.000000000000000000, -0.7071067811865537900, 0.7071067811865413555 ) ) ;
#65605 = CARTESIAN_POINT ( 'NONE',  ( -7.499999999999969802, 73.00000000000001421, -204.9999999999999716 ) ) ;
#65606 = EDGE_CURVE ( 'NONE', #40982, #19944, #7349, .T. ) ;
#65607 = CARTESIAN_POINT ( 'NONE',  ( 50.00005079999999680, 0.000000000000000000, 0.000000000000000000 ) ) ;
#65608 = CARTESIAN_POINT ( 'NONE',  ( -100.0000000000260059, -214.9999999999999716, -64.99999999999350564 ) ) ;
#65609 = CARTESIAN_POINT ( 'NONE',  ( 12.00000000000000355, 0.000000000000000000, 0.000000000000000000 ) ) ;
#65610 = AXIS2_PLACEMENT_3D ( 'NONE', #73340, #55693, #27100 ) ;
#65611 = ORIENTED_EDGE ( 'NONE', *, *, #4159, .F. ) ;
#65612 = EDGE_CURVE ( 'NONE', #58054, #2275, #44587, .T. ) ;
#65613 = DIRECTION ( 'NONE',  ( 0.000000000000000000, 0.000000000000000000, 1.000000000000000000 ) ) ;
#65614 = CARTESIAN_POINT ( 'NONE',  ( -7.500000000000016875, -80.00000000000001421, -189.9999999999999147 ) ) ;
#65615 = CYLINDRICAL_SURFACE ( 'NONE', #1026, 31.99999999999998579 ) ;
#65616 = AXIS2_PLACEMENT_3D ( 'NONE', #13236, #42555, #36164 ) ;
#65617 = EDGE_CURVE ( 'NONE', #49569, #14685, #64988, .T. ) ;
#65618 = DIRECTION ( 'NONE',  ( 0.000000000000000000, 0.8090169943749445647, 0.5877852522924770229 ) ) ;
#65619 = CARTESIAN_POINT ( 'NONE',  ( 0.000000000000000000, 0.000000000000000000, 0.000000000000000000 ) ) ;
#65620 = CARTESIAN_POINT ( 'NONE',  ( -92.35000000000000853, -208.4700217866474929, 87.19541666666667368 ) ) ;
#65621 = UNCERTAINTY_MEASURE_WITH_UNIT (LENGTH_MEASURE( 1.000000000000000082E-05 ), #38188, 'distance_accuracy_value', 'NONE');
#65622 = CARTESIAN_POINT ( 'NONE',  ( -92.35000000000000853, -209.9999996502046429, 77.69687501385436690 ) ) ;
#65623 = DIRECTION ( 'NONE',  ( 0.000000000000000000, -0.9969173337331287410, 0.07845909572783495156 ) ) ;
#65624 = VECTOR ( 'NONE', #19543, 1000.000000000000227 ) ;
#65625 = VECTOR ( 'NONE', #23624, 1000.000000000000000 ) ;
#65626 = ADVANCED_FACE ( 'NONE', ( #46541 ), #52924, .T. ) ;
#65627 = CARTESIAN_POINT ( 'NONE',  ( 92.69370383062498320, 91.33154071421968467, 84.03364583420049883 ) ) ;
#65628 = CARTESIAN_POINT ( 'NONE',  ( -92.69370383062498320, -209.9999999999999716, 86.30906250086715659 ) ) ;
#65629 = CARTESIAN_POINT ( 'NONE',  ( 97.65000000000000568, -211.5299782133524218, 83.99395833506763154 ) ) ;
#65630 = ORIENTED_EDGE ( 'NONE', *, *, #73088, .T. ) ;
#65631 = FACE_OUTER_BOUND ( 'NONE', #19013, .T. ) ;
#65632 = CARTESIAN_POINT ( 'NONE',  ( -94.99999999999997158, -206.9400435732949575, 82.85625000000000284 ) ) ;
#65633 = LINE ( 'NONE', #55823, #46195 ) ;
#65634 = AXIS2_PLACEMENT_3D ( 'NONE', #29645, #1141, #53335 ) ;
#65636 = ADVANCED_FACE ( 'NONE', ( #18333 ), #69831, .F. ) ;
#65635 = CARTESIAN_POINT ( 'NONE',  ( 95.00000000000000000, -212.6630814284392557, 85.35656250086714181 ) ) ;
#65637 = VERTEX_POINT ( 'NONE', #11575 ) ;
#65638 = ADVANCED_FACE ( 'NONE', ( #17231 ), #7052, .T. ) ;
#65639 = CARTESIAN_POINT ( 'NONE',  ( -3.000000000000000000, -4.261787119645322974, 26.19803753235774835 ) ) ;
#65640 = ORIENTED_EDGE ( 'NONE', *, *, #4042, .T. ) ;
#65641 = VERTEX_POINT ( 'NONE', #64215 ) ;
#65642 = CARTESIAN_POINT ( 'NONE',  ( 92.35000000000000853, -209.9999999999999716, 84.28499999999999659 ) ) ;
#65643 = VERTEX_POINT ( 'NONE', #35618 ) ;
#65644 = DIRECTION ( 'NONE',  ( -1.000000000000000000, -0.000000000000000000, 0.000000000000000000 ) ) ;
#65645 = CARTESIAN_POINT ( 'NONE',  ( 92.69370383062501162, -209.9999999999999716, 77.73656250086715147 ) ) ;
#65646 = DIRECTION ( 'NONE',  ( -1.000000000000000000, 0.000000000000000000, 0.000000000000000000 ) ) ;
#65647 = DIRECTION ( 'NONE',  ( 0.000000000000000000, 0.000000000000000000, 1.000000000000000000 ) ) ;
#65648 = CARTESIAN_POINT ( 'NONE',  ( 10.00000000000000000, 33.17418723428307459, 17.67226234102837878 ) ) ;
#65649 = CARTESIAN_POINT ( 'NONE',  ( 11.99999999999999822, 69.42325613327440692, 34.44570377933622041 ) ) ;
#65650 = CIRCLE ( 'NONE', #23637, 77.49899999999999523 ) ;
#65651 = CARTESIAN_POINT ( 'NONE',  ( -93.09170270117142820, -211.8387227684682159, 74.99954709728268654 ) ) ;
#65652 = CARTESIAN_POINT ( 'NONE',  ( 97.64999999999997726, -208.4700217866474645, 82.11541666666666117 ) ) ;
#65653 = STYLED_ITEM ( 'NONE', ( #43297 ), #14123 ) ;
#65654 = ORIENTED_EDGE ( 'NONE', *, *, #13987, .T. ) ;
#65655 = VERTEX_POINT ( 'NONE', #12687 ) ;
#65656 = EDGE_LOOP ( 'NONE', ( #3456, #15804, #26267, #7061 ) ) ;
#65657 = EDGE_LOOP ( 'NONE', ( #72290, #67788, #65105, #51138 ) ) ;
#65658 = DIRECTION ( 'NONE',  ( -0.000000000000000000, -0.000000000000000000, -1.000000000000000000 ) ) ;
#65659 = CARTESIAN_POINT ( 'NONE',  ( -92.69370383062502583, 91.33154071421968467, 83.18697916753382060 ) ) ;
#65660 = VECTOR ( 'NONE', #19256, 1000.000000000000000 ) ;
#65661 = AXIS2_PLACEMENT_3D ( 'NONE', #8092, #24285, #18623 ) ;
#65662 = CARTESIAN_POINT ( 'NONE',  ( 5.000000000000000000, 46.11716303203284184, -67.80270845531839541 ) ) ;
#65663 = CARTESIAN_POINT ( 'NONE',  ( 94.15631797925330204, 85.30516711421525144, 74.84535815546860249 ) ) ;
#65664 = LINE ( 'NONE', #14519, #11551 ) ;
#65665 = ORIENTED_EDGE ( 'NONE', *, *, #3350, .F. ) ;
#65666 = CARTESIAN_POINT ( 'NONE',  ( -92.34999999999999432, -208.4700217866474645, 86.00479166840096923 ) ) ;
#65667 = EDGE_CURVE ( 'NONE', #48290, #15280, #70969, .T. ) ;
#65668 = EDGE_LOOP ( 'NONE', ( #54133, #5170, #27665, #54717 ) ) ;
#65669 = DIRECTION ( 'NONE',  ( 0.000000000000000000, 0.000000000000000000, 1.000000000000000000 ) ) ;
#65670 = VECTOR ( 'NONE', #20664, 999.9999999999998863 ) ;
#65671 = ORIENTED_EDGE ( 'NONE', *, *, #1649, .F. ) ;
#65672 = CARTESIAN_POINT ( 'NONE',  ( -96.32500000000001705, 87.70503267997129626, 86.37520833506764006 ) ) ;
#65673 = ORIENTED_EDGE ( 'NONE', *, *, #57747, .T. ) ;
#65674 = CARTESIAN_POINT ( 'NONE',  ( 96.15314808468748708, 88.00268892867053694, 87.47322916753381605 ) ) ;
#65675 = VECTOR ( 'NONE', #69862, 1000.000000000000000 ) ;
#65676 = DIRECTION ( 'NONE',  ( -1.000000000000000000, 0.000000000000000000, 0.000000000000000000 ) ) ;
#65677 = DIRECTION ( 'NONE',  ( -0.000000000000000000, -0.000000000000000000, 1.000000000000000000 ) ) ;
#65678 = CARTESIAN_POINT ( 'NONE',  ( 97.64999999999999147, -209.9999999999999716, 90.00000000000000000 ) ) ;
#65679 = DIRECTION ( 'NONE',  ( -0.9580045777625456616, -0.2867529058022021404, 0.000000000000000000 ) ) ;
#65680 = ORIENTED_EDGE ( 'NONE', *, *, #36155, .T. ) ;
#65681 = DIRECTION ( 'NONE',  ( -1.000000000000000000, -0.000000000000000000, 0.000000000000000000 ) ) ;
#65682 = CARTESIAN_POINT ( 'NONE',  ( 0.000000000000000000, 65.59268652807263322, -36.72794159290169347 ) ) ;
#65683 = ORIENTED_EDGE ( 'NONE', *, *, #39338, .F. ) ;
#65684 = VECTOR ( 'NONE', #40872, 1000.000000000000000 ) ;
#65685 = ORIENTED_EDGE ( 'NONE', *, *, #60280, .F. ) ;
#65686 = EDGE_CURVE ( 'NONE', #59366, #22794, #63849, .T. ) ;
#65687 = DIRECTION ( 'NONE',  ( -0.1276937514489679404, -0.9918136447140103451, 0.000000000000000000 ) ) ;
#65689 = ADVANCED_FACE ( 'NONE', ( #69470 ), #35260, .T. ) ;
#65688 = CIRCLE ( 'NONE', #20049, 16.00000000000000000 ) ;
#65690 = FACE_OUTER_BOUND ( 'NONE', #23126, .T. ) ;
#65691 = DIRECTION ( 'NONE',  ( -1.000000000000000000, -1.427937372958405461E-15, -7.962523111839130290E-16 ) ) ;
#65692 = CARTESIAN_POINT ( 'NONE',  ( -96.15314808468745866, -211.9973110713294489, 82.92239583420048632 ) ) ;
#65693 = VERTEX_POINT ( 'NONE', #46919 ) ;
#65694 = DIRECTION ( 'NONE',  ( -0.7950889364178781449, 0.6064928550163533050, 0.000000000000000000 ) ) ;
#65695 = EDGE_LOOP ( 'NONE', ( #3437, #60954, #55680, #16117 ) ) ;
#65696 = ADVANCED_FACE ( 'NONE', ( #6689, #34148, #28495, #63476, #29595, #51434, #40166, #17599, #17968, #12447, #22888, #63121, #45825, #68747, #34510, #51813, #57458 ), #23249, .F. ) ;
#65697 = EDGE_CURVE ( 'NONE', #53602, #24570, #43429, .T. ) ;
#65698 = ORIENTED_EDGE ( 'NONE', *, *, #66954, .F. ) ;
#65699 = DIRECTION ( 'NONE',  ( 0.000000000000000000, 0.000000000000000000, 1.000000000000000000 ) ) ;
#65700 = CARTESIAN_POINT ( 'NONE',  ( 0.000000000000000000, 0.000000000000000000, 0.000000000000000000 ) ) ;
#65701 =( NAMED_UNIT ( * ) SI_UNIT ( $, .STERADIAN. ) SOLID_ANGLE_UNIT ( ) );
#65702 = CARTESIAN_POINT ( 'NONE',  ( 92.69370383062498320, 90.00000000000002842, 80.11781250086713158 ) ) ;
#65703 = DIRECTION ( 'NONE',  ( 0.000000000000000000, -1.000000000000000000, -1.040834085586084730E-14 ) ) ;
#65704 = CARTESIAN_POINT ( 'NONE',  ( 0.000000000000000000, 51.29473840253317718, -63.97538442413369353 ) ) ;
#65705 = CARTESIAN_POINT ( 'NONE',  ( -12.00000000000000000, 0.000000000000000000, 0.000000000000000000 ) ) ;
#65706 = CARTESIAN_POINT ( 'NONE',  ( 95.99319914654111585, 92.13398380010835353, 74.81432998548488911 ) ) ;
#65707 = CARTESIAN_POINT ( 'NONE',  ( 0.000000000000000000, 51.29473840253317007, -63.97538442413369353 ) ) ;
#65708 = CARTESIAN_POINT ( 'NONE',  ( 0.000000000000000000, 0.000000000000000000, 0.000000000000000000 ) ) ;
#65709 =( BOUNDED_CURVE ( )  B_SPLINE_CURVE ( 2, ( #16933, #10917, #56416, #68810, #39871, #28199, #33842, #28558, #28942 ),
 .UNSPECIFIED., .F., .F. ) 
 B_SPLINE_CURVE_WITH_KNOTS ( ( 3, 2, 2, 2, 3 ),
 ( 0.8255245790564498254, 0.8325803338241194451, 0.8396360993650018312, 0.8466918649058842172, 0.8466920362367558184 ),
 .UNSPECIFIED. ) 
 CURVE ( )  GEOMETRIC_REPRESENTATION_ITEM ( )  RATIONAL_B_SPLINE_CURVE ( ( 1.000000000000000000, 0.8660254037844387076, 1.000000000000000000, 0.8660254037844387076, 1.000000000000000000, 0.8660254037844387076, 1.000000000000000000, 0.9999967467762058693, 0.9999934937104038024 ) ) 
 REPRESENTATION_ITEM ( '' )  );
#65710 = EDGE_CURVE ( 'NONE', #16558, #11817, #11363, .T. ) ;
#65711 = VECTOR ( 'NONE', #10022, 1000.000000000000000 ) ;
#65712 = DIRECTION ( 'NONE',  ( -0.6862798483830534479, -0.7273375899149810975, 0.000000000000000000 ) ) ;
#65713 = AXIS2_PLACEMENT_3D ( 'NONE', #40990, #64292, #51890 ) ;
#65714 = CARTESIAN_POINT ( 'NONE',  ( -92.34999999999999432, -209.9999999999999716, 90.00000000000000000 ) ) ;
#65715 = ORIENTED_EDGE ( 'NONE', *, *, #57579, .F. ) ;
#65716 = CARTESIAN_POINT ( 'NONE',  ( -92.69370383062505425, 88.66845928578038638, 86.09739583420048348 ) ) ;
#65717 = LINE ( 'NONE', #25486, #45593 ) ;
#65718 = CIRCLE ( 'NONE', #57294, 16.00000000000000000 ) ;
#65719 = AXIS2_PLACEMENT_3D ( 'NONE', #55061, #3593, #43806 ) ;
#65721 = EDGE_CURVE ( 'NONE', #54492, #70171, #62629, .T. ) ;
#65720 = DIRECTION ( 'NONE',  ( -1.000000000000000000, -0.000000000000000000, -0.000000000000000000 ) ) ;
#65722 = ORIENTED_EDGE ( 'NONE', *, *, #5398, .T. ) ;
#65723 = DIRECTION ( 'NONE',  ( 0.000000000000000000, -0.8660254037844363761, -0.5000000000000039968 ) ) ;
#65724 = ADVANCED_FACE ( 'NONE', ( #7794 ), #2930, .T. ) ;
#65725 = DIRECTION ( 'NONE',  ( -0.000000000000000000, -0.000000000000000000, 1.000000000000000000 ) ) ;
#65726 = DIRECTION ( 'NONE',  ( 0.000000000000000000, 0.000000000000000000, 1.000000000000000000 ) ) ;
#65727 = CARTESIAN_POINT ( 'NONE',  ( 97.30629616937498838, -211.3315407142195852, 82.44614583420049314 ) ) ;
#65728 = VERTEX_POINT ( 'NONE', #14165 ) ;
#65729 = ORIENTED_EDGE ( 'NONE', *, *, #61612, .F. ) ;
#65730 = AXIS2_PLACEMENT_3D ( 'NONE', #30777, #54109, #42452 ) ;
#65731 = FACE_OUTER_BOUND ( 'NONE', #26133, .T. ) ;
#65732 = FACE_OUTER_BOUND ( 'NONE', #29555, .T. ) ;
#65733 = CYLINDRICAL_SURFACE ( 'NONE', #52009, 31.99999999999998579 ) ;
#65734 = ORIENTED_EDGE ( 'NONE', *, *, #56301, .F. ) ;
#65735 = PRESENTATION_STYLE_ASSIGNMENT (( #31139 ) ) ;
#65736 = CARTESIAN_POINT ( 'NONE',  ( 95.46326757314950839, -212.8430781844920432, 74.72378867588406592 ) ) ;
#65737 = ORIENTED_EDGE ( 'NONE', *, *, #71030, .T. ) ;
#65738 = CARTESIAN_POINT ( 'NONE',  ( 94.99999999999998579, 86.94004357329502852, 79.36374999999996760 ) ) ;
#65739 = VERTEX_POINT ( 'NONE', #36361 ) ;
#65740 = ORIENTED_EDGE ( 'NONE', *, *, #16824, .F. ) ;
#65741 = CARTESIAN_POINT ( 'NONE',  ( 11.99999999999999822, 71.27951684758069462, -30.41916302227037150 ) ) ;
#65742 =( NAMED_UNIT ( * ) SI_UNIT ( $, .STERADIAN. ) SOLID_ANGLE_UNIT ( ) );
#65743 = DIRECTION ( 'NONE',  ( 0.000000000000000000, 0.2079116908177525702, 0.9781476007338071321 ) ) ;
#65744 = EDGE_LOOP ( 'NONE', ( #8390, #7018, #57174, #19726 ) ) ;
#65745 = CARTESIAN_POINT ( 'NONE',  ( 11.99999999999999822, 0.000000000000000000, 0.000000000000000000 ) ) ;
#65746 = CARTESIAN_POINT ( 'NONE',  ( 97.64999999999997726, -208.4700217866474645, 84.73479166840097321 ) ) ;
#65747 = CARTESIAN_POINT ( 'NONE',  ( 97.64999999999997726, 88.47002178664753558, 85.18458333333332178 ) ) ;
#65748 = VERTEX_POINT ( 'NONE', #30348 ) ;
#65749 = CARTESIAN_POINT ( 'NONE',  ( 10.00000000000000000, 0.000000000000000000, 0.000000000000000000 ) ) ;
#65750 = CARTESIAN_POINT ( 'NONE',  ( -1.200000000000000030E-05, 16.95692799528845995, 2.500000000000000000 ) ) ;
#65751 = ORIENTED_EDGE ( 'NONE', *, *, #56204, .T. ) ;
#65752 = ORIENTED_EDGE ( 'NONE', *, *, #60190, .F. ) ;
#65753 = CARTESIAN_POINT ( 'NONE',  ( -92.69370383062505425, 88.66845928578038638, 86.25614583420048120 ) ) ;
#65754 = CARTESIAN_POINT ( 'NONE',  ( 92.69370383062498320, 91.33154071421968467, 80.06489583420047040 ) ) ;
#65755 = ORIENTED_EDGE ( 'NONE', *, *, #12961, .T. ) ;
#65757 = CARTESIAN_POINT ( 'NONE',  ( 93.67499999999998295, 92.29496732002878900, 81.71854166840095957 ) ) ;
#65756 = VECTOR ( 'NONE', #24366, 1000.000000000000114 ) ;
#65758 = EDGE_CURVE ( 'NONE', #30795, #21162, #67378, .T. ) ;
#65759 = DIRECTION ( 'NONE',  ( -1.000000000000000000, 0.000000000000000000, 0.000000000000000000 ) ) ;
#65760 = ORIENTED_EDGE ( 'NONE', *, *, #16710, .T. ) ;
#65761 = CARTESIAN_POINT ( 'NONE',  ( -93.67499999999998295, -212.2949673200287179, 86.40166666666667084 ) ) ;
#65762 = ORIENTED_EDGE ( 'NONE', *, *, #28533, .T. ) ;
#65763 = EDGE_LOOP ( 'NONE', ( #68342, #17084, #1799, #16244 ) ) ;
#65764 = VERTEX_POINT ( 'NONE', #13433 ) ;
#65765 = CIRCLE ( 'NONE', #27325, 16.00000000000000000 ) ;
#65766 = CYLINDRICAL_SURFACE ( 'NONE', #19348, 31.99999999999998579 ) ;
#65767 = EDGE_CURVE ( 'NONE', #51229, #22980, #43139, .T. ) ;
#65768 = CARTESIAN_POINT ( 'NONE',  ( -10.00000000000000000, 0.000000000000000000, 0.000000000000000000 ) ) ;
#65769 = CARTESIAN_POINT ( 'NONE',  ( -92.35000000000003695, 90.00000000000004263, 84.60249999999999204 ) ) ;
#65770 = ADVANCED_FACE ( 'NONE', ( #71299, #60067, #59301, #42752, #65323 ), #54040, .F. ) ;
#65771 = EDGE_LOOP ( 'NONE', ( #65280, #48370, #6950, #23235 ) ) ;
#65772 = DIRECTION ( 'NONE',  ( -1.000000000000000000, -0.000000000000000000, -0.000000000000000000 ) ) ;
#65773 = CARTESIAN_POINT ( 'NONE',  ( 4.999999999999999112, 41.81611651403868990, -3.925862922255709542 ) ) ;
#65774 = VERTEX_POINT ( 'NONE', #2574 ) ;
#65775 = CYLINDRICAL_SURFACE ( 'NONE', #70781, 82.00000000000000000 ) ;
#65776 = CARTESIAN_POINT ( 'NONE',  ( -93.84685191531248449, -208.0026889286704943, 80.54114583420046358 ) ) ;
#65777 = VERTEX_POINT ( 'NONE', #20174 ) ;
#65778 = DIRECTION ( 'NONE',  ( 1.000000000000000000, 0.000000000000000000, 0.000000000000000000 ) ) ;
#65779 = CARTESIAN_POINT ( 'NONE',  ( -23.30023580412278505, -123.4057321492263384, 5.500000000000000000 ) ) ;
#65780 = DIRECTION ( 'NONE',  ( -1.000000000000000000, 0.000000000000000000, 0.000000000000000000 ) ) ;
#65781 = CARTESIAN_POINT ( 'NONE',  ( 11.99999999999999822, -54.21277698773713638, 55.38113227695764351 ) ) ;
#65782 = ADVANCED_FACE ( 'NONE', ( #13791 ), #20560, .T. ) ;
#65783 = CARTESIAN_POINT ( 'NONE',  ( 10.00000000000000000, 0.000000000000000000, 0.000000000000000000 ) ) ;
#65784 = AXIS2_PLACEMENT_3D ( 'NONE', #39305, #26892, #49820 ) ;
#65785 = DIRECTION ( 'NONE',  ( -1.000000000000000000, -0.000000000000000000, 0.000000000000000000 ) ) ;
#65787 = AXIS2_PLACEMENT_3D ( 'NONE', #69102, #53648, #6324 ) ;
#65786 = DIRECTION ( 'NONE',  ( -1.000000000000000000, 0.000000000000000000, 0.000000000000000000 ) ) ;
#65788 = DIRECTION ( 'NONE',  ( -1.000000000000000000, -0.000000000000000000, -0.000000000000000000 ) ) ;
#65789 = CIRCLE ( 'NONE', #20321, 16.00000000000000355 ) ;
#65790 = CARTESIAN_POINT ( 'NONE',  ( 11.99999999999999822, -55.38113227695745167, -54.21277698773732823 ) ) ;
#65791 = AXIS2_PLACEMENT_3D ( 'NONE', #39921, #11685, #23000 ) ;
#65792 = CARTESIAN_POINT ( 'NONE',  ( 10.00000000000000000, -46.54456581323762521, -59.03342792756313884 ) ) ;
#65793 = CARTESIAN_POINT ( 'NONE',  ( -97.30629616937501680, 88.66845928578038638, 89.21947916753381946 ) ) ;
#65794 = CARTESIAN_POINT ( 'NONE',  ( 5.000000000000000000, 55.16347631943042984, 60.67117009219156643 ) ) ;
#65795 = DIRECTION ( 'NONE',  ( 0.000000000000000000, 0.000000000000000000, 1.000000000000000000 ) ) ;
#65796 = ADVANCED_FACE ( 'NONE', ( #35992 ), #25459, .T. ) ;
#65797 = AXIS2_PLACEMENT_3D ( 'NONE', #48962, #48609, #71893 ) ;
#65798 = CARTESIAN_POINT ( 'NONE',  ( -3.000000000000000000, 16.61724383029390140, -20.69703378468903665 ) ) ;
#65799 = EDGE_CURVE ( 'NONE', #28741, #8298, #32540, .T. ) ;
#65800 = CARTESIAN_POINT ( 'NONE',  ( 11.99999999999999822, 67.80270845531956070, -46.11716303203111522 ) ) ;
#65801 = EDGE_CURVE ( 'NONE', #45219, #8157, #8158, .T. ) ;
#65802 = CARTESIAN_POINT ( 'NONE',  ( -94.99999999999997158, -213.0599564267049857, 84.52312500173428589 ) ) ;
#65803 = CARTESIAN_POINT ( 'NONE',  ( 11.99999999999999822, -66.50666863321974631, -39.78640506895675344 ) ) ;
#65804 = CARTESIAN_POINT ( 'NONE',  ( 10.00000000000000000, -62.50329211542465657, 41.76937507738766442 ) ) ;
#65805 = CARTESIAN_POINT ( 'NONE',  ( 92.35000000000009379, -211.5299782133524502, 78.62291666666668277 ) ) ;
#65806 = CARTESIAN_POINT ( 'NONE',  ( -2.499999999999965361, 90.00000000000000000, -310.0000000000000000 ) ) ;
#65807 = CARTESIAN_POINT ( 'NONE',  ( -97.64999999999996305, -209.9999999999999716, 89.36499999999999488 ) ) ;
#65808 = CARTESIAN_POINT ( 'NONE',  ( 0.000000000000000000, -0.8299999999999999600, 0.000000000000000000 ) ) ;
#65809 = ADVANCED_FACE ( 'NONE', ( #53290 ), #1828, .T. ) ;
#65810 = VERTEX_POINT ( 'NONE', #47649 ) ;
#65811 = CIRCLE ( 'NONE', #31018, 12.50000000000000000 ) ;
#65812 = LINE ( 'NONE', #55633, #70762 ) ;
#65813 = CARTESIAN_POINT ( 'NONE',  ( 92.35000000003358878, -210.0000076551254153, 78.01464417100928017 ) ) ;
#65814 = CARTESIAN_POINT ( 'NONE',  ( 11.99999999999999822, -58.39081064771786345, 50.95692526931308919 ) ) ;
#65815 = CIRCLE ( 'NONE', #55010, 2.650000000000540812 ) ;
#65816 = VECTOR ( 'NONE', #53591, 1000.000000000000000 ) ;
#65817 = DIRECTION ( 'NONE',  ( -1.000000000000000000, 0.000000000000000000, 0.000000000000000000 ) ) ;
#65818 = AXIS2_PLACEMENT_3D ( 'NONE', #32481, #27591, #21193 ) ;
#65819 = AXIS2_PLACEMENT_3D ( 'NONE', #9859, #43358, #32774 ) ;
#65820 = ORIENTED_EDGE ( 'NONE', *, *, #46851, .T. ) ;
#65821 = DIRECTION ( 'NONE',  ( 2.603472992746261562E-14, 2.546204323184492723E-14, -1.000000000000000000 ) ) ;
#65822 = DIRECTION ( 'NONE',  ( 0.000000000000000000, 0.000000000000000000, -1.000000000000000000 ) ) ;
#65823 = ORIENTED_EDGE ( 'NONE', *, *, #40768, .T. ) ;
#65824 = CARTESIAN_POINT ( 'NONE',  ( 96.15314808468750130, -211.9973110713294489, 80.32947916753380468 ) ) ;
#65825 = CARTESIAN_POINT ( 'NONE',  ( 97.30629616937498838, -211.3315407142195852, 88.16114583420048234 ) ) ;
#65826 = ORIENTED_EDGE ( 'NONE', *, *, #63324, .F. ) ;
#65827 = CARTESIAN_POINT ( 'NONE',  ( 93.84685191531251292, -211.9973110713294489, 88.00239583420048461 ) ) ;
#65828 = ORIENTED_EDGE ( 'NONE', *, *, #17176, .F. ) ;
#65829 = DIRECTION ( 'NONE',  ( 1.000000000000000000, 0.000000000000000000, -0.000000000000000000 ) ) ;
#65830 = ORIENTED_EDGE ( 'NONE', *, *, #53238, .T. ) ;
#65831 = CARTESIAN_POINT ( 'NONE',  ( -92.69370383062502583, 91.33154071421968467, 78.74197916753382742 ) ) ;
#65832 = VECTOR ( 'NONE', #1618, 1000.000000000000000 ) ;
#65833 = ORIENTED_EDGE ( 'NONE', *, *, #74204, .F. ) ;
#65834 = EDGE_LOOP ( 'NONE', ( #39667, #37668, #35985, #51148 ) ) ;
#65835 = AXIS2_PLACEMENT_3D ( 'NONE', #45349, #44971, #4019 ) ;
#65836 = LINE ( 'NONE', #21816, #48477 ) ;
#65837 = AXIS2_PLACEMENT_3D ( 'NONE', #22277, #15140, #61013 ) ;
#65838 = ORIENTED_EDGE ( 'NONE', *, *, #13920, .T. ) ;
#65839 = LINE ( 'NONE', #14325, #68934 ) ;
#65840 = CARTESIAN_POINT ( 'NONE',  ( 24.95699195200417364, -110.9640411295978595, -2.500000000000000000 ) ) ;
#65841 = VECTOR ( 'NONE', #12801, 1000.000000000000000 ) ;
#65842 = ORIENTED_EDGE ( 'NONE', *, *, #23604, .T. ) ;
#65843 = DIRECTION ( 'NONE',  ( 0.000000000000000000, 0.000000000000000000, 1.000000000000000000 ) ) ;
#65844 = ORIENTED_EDGE ( 'NONE', *, *, #17455, .F. ) ;
#65845 = VECTOR ( 'NONE', #46668, 1000.000000000000000 ) ;
#65846 = DIRECTION ( 'NONE',  ( 0.000000000000000000, 0.000000000000000000, -1.000000000000000000 ) ) ;
#65847 = ORIENTED_EDGE ( 'NONE', *, *, #55749, .T. ) ;
#65848 = EDGE_CURVE ( 'NONE', #22283, #63788, #64953, .T. ) ;
#65849 = EDGE_LOOP ( 'NONE', ( #40078, #73027, #40035, #6426 ) ) ;
#65850 = ORIENTED_EDGE ( 'NONE', *, *, #21450, .T. ) ;
#65851 = CARTESIAN_POINT ( 'NONE',  ( 93.84685191531249870, -208.0026889286704943, 78.10697916753380809 ) ) ;
#65852 = CARTESIAN_POINT ( 'NONE',  ( 12.00000000000000000, -0.9646360437372099028, 23.52805723605590771 ) ) ;
#65853 = FACE_OUTER_BOUND ( 'NONE', #2434, .T. ) ;
#65855 = EDGE_CURVE ( 'NONE', #27913, #28647, #51764, .T. ) ;
#65854 = ORIENTED_EDGE ( 'NONE', *, *, #34629, .T. ) ;
#65856 = CARTESIAN_POINT ( 'NONE',  ( -96.32499999999996021, -212.2949673200287179, 78.75520833506763552 ) ) ;
#65857 = ORIENTED_EDGE ( 'NONE', *, *, #71433, .F. ) ;
#65858 = FACE_OUTER_BOUND ( 'NONE', #55348, .T. ) ;
#65859 = EDGE_CURVE ( 'NONE', #60921, #23922, #14570, .T. ) ;
#65860 = CARTESIAN_POINT ( 'NONE',  ( -94.99999999999997158, -213.0599564267049857, 75.55375000000000796 ) ) ;
#65861 = EDGE_LOOP ( 'NONE', ( #12768, #49646, #52983, #52171 ) ) ;
#65862 = CARTESIAN_POINT ( 'NONE',  ( -97.64999999999996305, -209.9999999999999716, 88.80937500173430976 ) ) ;
#65863 = EDGE_CURVE ( 'NONE', #22041, #55469, #55137, .T. ) ;
#65864 = CARTESIAN_POINT ( 'NONE',  ( 12.00000000000000000, 9.615535125378766423, -24.73947219025917121 ) ) ;
#65865 = CARTESIAN_POINT ( 'NONE',  ( -94.99999999999997158, -207.3369185715606307, 79.95906250086713385 ) ) ;
#65866 = CARTESIAN_POINT ( 'NONE',  ( -92.69370383062502583, 91.33154071421968467, 77.47197916753381719 ) ) ;
#65867 = ORIENTED_EDGE ( 'NONE', *, *, #24199, .F. ) ;
#65868 = CARTESIAN_POINT ( 'NONE',  ( 93.84685191531248449, 91.99731107132950569, 81.91697916753381037 ) ) ;
#65869 = EDGE_CURVE ( 'NONE', #16005, #31772, #31368, .T. ) ;
#65870 = ORIENTED_EDGE ( 'NONE', *, *, #42673, .T. ) ;
#65871 = FACE_OUTER_BOUND ( 'NONE', #58709, .T. ) ;
#65872 = CARTESIAN_POINT ( 'NONE',  ( -92.69370383062498320, -211.3315407142195852, 88.00239583420047040 ) ) ;
#65873 = VECTOR ( 'NONE', #57336, 1000.000000000000000 ) ;
#65874 = CARTESIAN_POINT ( 'NONE',  ( -94.99999999999997158, -213.0599564267049857, 76.82374999999998977 ) ) ;
#65875 = DIRECTION ( 'NONE',  ( 1.000000000000000000, 0.000000000000000000, 0.000000000000000000 ) ) ;
#65876 = CYLINDRICAL_SURFACE ( 'NONE', #40439, 82.00000000000000000 ) ;
#65877 = CARTESIAN_POINT ( 'NONE',  ( -96.15314808468747287, -208.0026889286704943, 82.55197916753380127 ) ) ;
#65878 = AXIS2_PLACEMENT_3D ( 'NONE', #35821, #58776, #53130 ) ;
#65879 = AXIS2_PLACEMENT_3D ( 'NONE', #16983, #6446, #52295 ) ;
#65880 = EDGE_CURVE ( 'NONE', #20073, #1781, #16682, .T. ) ;
#65881 = DIRECTION ( 'NONE',  ( -1.000000000000000000, 0.000000000000000000, 0.000000000000000000 ) ) ;
#65882 = DIRECTION ( 'NONE',  ( 0.1736481776669309696, 0.9848077530122080203, 0.000000000000000000 ) ) ;
#65883 = FACE_OUTER_BOUND ( 'NONE', #11368, .T. ) ;
#65884 = ORIENTED_EDGE ( 'NONE', *, *, #46330, .T. ) ;
#65885 = CIRCLE ( 'NONE', #5893, 16.00000000000000000 ) ;
#65886 = ORIENTED_EDGE ( 'NONE', *, *, #43550, .F. ) ;
#65887 = DIRECTION ( 'NONE',  ( 0.000000000000000000, 0.000000000000000000, 1.000000000000000000 ) ) ;
#65888 = AXIS2_PLACEMENT_3D ( 'NONE', #68416, #50728, #62414 ) ;
#65889 = CARTESIAN_POINT ( 'NONE',  ( -96.32500000000001705, 92.29496732002878900, 75.28916666666665947 ) ) ;
#65890 = CARTESIAN_POINT ( 'NONE',  ( 10.00000000000000000, 71.91182617369189245, 28.89263327155772743 ) ) ;
#65891 = CARTESIAN_POINT ( 'NONE',  ( -92.69370383062504004, 90.00000000000004263, 84.88031250086713442 ) ) ;
#65892 = DIRECTION ( 'NONE',  ( -0.000000000000000000, -0.000000000000000000, -1.000000000000000000 ) ) ;
#65893 = DIRECTION ( 'NONE',  ( -1.000000000000000000, -0.000000000000000000, 0.000000000000000000 ) ) ;
#65894 = DIRECTION ( 'NONE',  ( -1.000000000000000000, -0.000000000000000000, -0.000000000000000000 ) ) ;
#65895 = ORIENTED_EDGE ( 'NONE', *, *, #18109, .F. ) ;
#65896 = ADVANCED_FACE ( 'NONE', ( #68931 ), #11402, .T. ) ;
#65897 = FACE_OUTER_BOUND ( 'NONE', #53914, .T. ) ;
#65898 = AXIS2_PLACEMENT_3D ( 'NONE', #55813, #66724, #32121 ) ;
#65899 = EDGE_CURVE ( 'NONE', #14594, #42482, #34975, .T. ) ;
#65900 = EDGE_CURVE ( 'NONE', #54327, #59857, #33966, .T. ) ;
#65901 = LINE ( 'NONE', #3131, #57369 ) ;
#65902 = VECTOR ( 'NONE', #60129, 1000.000000000000114 ) ;
#65903 = DIRECTION ( 'NONE',  ( 0.000000000000000000, 0.000000000000000000, -1.000000000000000000 ) ) ;
#65904 = DIRECTION ( 'NONE',  ( 0.000000000000000000, 1.000000000000000000, 0.000000000000000000 ) ) ;
#65905 = DIRECTION ( 'NONE',  ( 0.000000000000000000, 0.000000000000000000, 1.000000000000000000 ) ) ;
#65906 = FACE_OUTER_BOUND ( 'NONE', #4983, .T. ) ;
#65907 = CARTESIAN_POINT ( 'NONE',  ( -97.30629616937495996, -209.9999999999999716, 83.45156250086715488 ) ) ;
#65908 = AXIS2_PLACEMENT_3D ( 'NONE', #56411, #16541, #38365 ) ;
#65909 = AXIS2_PLACEMENT_3D ( 'NONE', #51932, #23375, #35020 ) ;
#65910 = LINE ( 'NONE', #31302, #50930 ) ;
#65911 = EDGE_CURVE ( 'NONE', #52257, #7708, #73377, .T. ) ;
#65912 = AXIS2_PLACEMENT_3D ( 'NONE', #38541, #49443, #21229 ) ;
#65913 = CARTESIAN_POINT ( 'NONE',  ( 94.99999999999998579, 87.33691857156068750, 75.35531250086715715 ) ) ;
#65914 = LINE ( 'NONE', #44078, #34636 ) ;
#65915 = CARTESIAN_POINT ( 'NONE',  ( -93.67500000000003979, 87.70503267997129626, 88.94166666666666288 ) ) ;
#65916 = EDGE_LOOP ( 'NONE', ( #14324, #60837, #25440, #21129 ) ) ;
#65917 = DIRECTION ( 'NONE',  ( 0.000000000000000000, 0.000000000000000000, 1.000000000000000000 ) ) ;
#65918 = CARTESIAN_POINT ( 'NONE',  ( -97.65000000000009095, 91.52997821335249284, 78.51708333333334622 ) ) ;
#65919 = FACE_OUTER_BOUND ( 'NONE', #39372, .T. ) ;
#65920 = CARTESIAN_POINT ( 'NONE',  ( 93.84685191531249870, -208.0026889286704943, 74.93197916753379673 ) ) ;
#65921 = VERTEX_POINT ( 'NONE', #10661 ) ;
#65922 = VECTOR ( 'NONE', #15448, 1000.000000000000000 ) ;
#65923 = CARTESIAN_POINT ( 'NONE',  ( 97.64999999999999147, 90.00000000000002842, 87.22187500173430408 ) ) ;
#65924 = ORIENTED_EDGE ( 'NONE', *, *, #23333, .T. ) ;
#65925 =( BOUNDED_CURVE ( )  B_SPLINE_CURVE ( 2, ( #38699, #34529, #28897, #57476, #5990, #17617, #7811 ),
 .UNSPECIFIED., .F., .F. ) 
 B_SPLINE_CURVE_WITH_KNOTS ( ( 3, 2, 2, 3 ),
 ( 0.3958333333333330373, 0.4027777777777774570, 0.4097222222222218768, 0.4166666666666662966 ),
 .UNSPECIFIED. ) 
 CURVE ( )  GEOMETRIC_REPRESENTATION_ITEM ( )  RATIONAL_B_SPLINE_CURVE ( ( 1.000000000000005329, 0.8660254037844333785, 1.000000000000000000, 0.8660254037844387076, 1.000000000000000000, 0.8660254037844462571, 0.9999999999999924505 ) ) 
 REPRESENTATION_ITEM ( '' )  );
#65926 = AXIS2_PLACEMENT_3D ( 'NONE', #35869, #41893, #43012 ) ;
#65927 = CARTESIAN_POINT ( 'NONE',  ( 6.000000000000000000, -80.28980883073769803, 16.65972982744905551 ) ) ;
#65928 = ORIENTED_EDGE ( 'NONE', *, *, #49056, .T. ) ;
#65929 = CIRCLE ( 'NONE', #73090, 42.00000000000000000 ) ;
#65930 = DIRECTION ( 'NONE',  ( -0.000000000000000000, -0.000000000000000000, -1.000000000000000000 ) ) ;
#65931 = VECTOR ( 'NONE', #8181, 1000.000000000000227 ) ;
#65932 = ORIENTED_EDGE ( 'NONE', *, *, #32341, .F. ) ;
#65933 = ORIENTED_EDGE ( 'NONE', *, *, #45546, .F. ) ;
#65934 = AXIS2_PLACEMENT_3D ( 'NONE', #394, #63517, #7093 ) ;
#65935 = ORIENTED_EDGE ( 'NONE', *, *, #41679, .F. ) ;
#65936 = ORIENTED_EDGE ( 'NONE', *, *, #73736, .T. ) ;
#65937 = DIRECTION ( 'NONE',  ( 1.000000000000000000, 0.000000000000000000, 0.000000000000000000 ) ) ;
#65938 = ORIENTED_EDGE ( 'NONE', *, *, #44687, .F. ) ;
#65939 = VERTEX_POINT ( 'NONE', #11757 ) ;
#65940 = CARTESIAN_POINT ( 'NONE',  ( 94.99999999999998579, 87.33691857156068750, 81.07031250086716057 ) ) ;
#65941 = LINE ( 'NONE', #37736, #56401 ) ;
#65942 = CARTESIAN_POINT ( 'NONE',  ( 0.000000000000000000, 2.571758278209441661E-15, -21.00000000000000000 ) ) ;
#65943 = EDGE_LOOP ( 'NONE', ( #66134, #1612, #51955, #38933 ) ) ;
#65945 = VERTEX_POINT ( 'NONE', #46002 ) ;
#65944 = VECTOR ( 'NONE', #6060, 1000.000000000000000 ) ;
#65946 = EDGE_CURVE ( 'NONE', #71000, #50841, #46999, .T. ) ;
#65947 = ORIENTED_EDGE ( 'NONE', *, *, #48876, .T. ) ;
#65948 = CARTESIAN_POINT ( 'NONE',  ( 15.00000000000000000, -23.29833615347109088, -3.418703333116486665 ) ) ;
#65949 = ORIENTED_EDGE ( 'NONE', *, *, #21666, .F. ) ;
#65950 = VECTOR ( 'NONE', #60194, 1000.000000000000000 ) ;
#65951 = VECTOR ( 'NONE', #68356, 1000.000000000000000 ) ;
#65952 = CARTESIAN_POINT ( 'NONE',  ( -0.6292498812908471351, 0.7209408956789961076, -45.00000000000000000 ) ) ;
#65953 = DIRECTION ( 'NONE',  ( 0.9997280174009349762, -0.02332147558787674158, 0.000000000000000000 ) ) ;
#65954 = EDGE_CURVE ( 'NONE', #11454, #18706, #65521, .T. ) ;
#65955 = CARTESIAN_POINT ( 'NONE',  ( -96.44578755843129159, 91.96030971134661058, 74.86947676125078033 ) ) ;
#65956 = DIRECTION ( 'NONE',  ( 1.000000000000000000, -0.000000000000000000, -0.000000000000000000 ) ) ;
#65957 = CARTESIAN_POINT ( 'NONE',  ( 11.99999999999999822, 46.21855187248719687, -62.20884554313968806 ) ) ;
#65958 = CARTESIAN_POINT ( 'NONE',  ( -93.67500000000003979, 87.70503267997129626, 78.14666666666667538 ) ) ;
#65959 = AXIS2_PLACEMENT_3D ( 'NONE', #49178, #43926, #26240 ) ;
#65960 = ADVANCED_FACE ( 'NONE', ( #68566 ), #73807, .T. ) ;
#65961 = CARTESIAN_POINT ( 'NONE',  ( 4.999999999999999112, -40.68715046381921496, -10.41901085202121280 ) ) ;
#65962 = VECTOR ( 'NONE', #51473, 1000.000000000000000 ) ;
#65963 = EDGE_CURVE ( 'NONE', #34327, #16195, #41512, .T. ) ;
#65964 = CARTESIAN_POINT ( 'NONE',  ( -97.64999999999994884, -208.4700217866474645, 76.69145833506763665 ) ) ;
#65965 = CARTESIAN_POINT ( 'NONE',  ( -92.69370383062504004, 90.00000000000004263, 88.21406250086714351 ) ) ;
#65966 = ORIENTED_EDGE ( 'NONE', *, *, #63922, .F. ) ;
#65968 = CARTESIAN_POINT ( 'NONE',  ( -95.00000000000002842, 92.66308142843932671, 88.21406250086714351 ) ) ;
#65967 = CARTESIAN_POINT ( 'NONE',  ( 92.34999999999999432, 88.47002178664753558, 76.16229166840095388 ) ) ;
#65969 = AXIS2_PLACEMENT_3D ( 'NONE', #20514, #14867, #54723 ) ;
#65970 = ORIENTED_EDGE ( 'NONE', *, *, #4681, .F. ) ;
#65971 = CARTESIAN_POINT ( 'NONE',  ( 96.15314808468748708, 88.00268892867053694, 77.94822916753382458 ) ) ;
#65972 = DIRECTION ( 'NONE',  ( -1.000000000000000000, -0.000000000000000000, 0.000000000000000000 ) ) ;
#65973 = LINE ( 'NONE', #24985, #21090 ) ;
#65974 = PLANE ( 'NONE',  #65992 ) ;
#65975 = CARTESIAN_POINT ( 'NONE',  ( -92.35000000000003695, 90.00000000000004263, 78.33187500173430351 ) ) ;
#65976 = DIRECTION ( 'NONE',  ( 0.000000000000000000, 0.000000000000000000, 1.000000000000000000 ) ) ;
#65977 = VERTEX_POINT ( 'NONE', #22320 ) ;
#65978 = CARTESIAN_POINT ( 'NONE',  ( -92.34999999999999432, -209.9999999999999716, 87.77749999999998920 ) ) ;
#65979 = DIRECTION ( 'NONE',  ( -1.000000000000000000, 0.000000000000000000, 0.000000000000000000 ) ) ;
#65980 = EDGE_LOOP ( 'NONE', ( #61319, #34786, #62233, #36956 ) ) ;
#65981 = EDGE_LOOP ( 'NONE', ( #63086, #62070, #60651, #13402 ) ) ;
#65982 = ADVANCED_FACE ( 'NONE', ( #57655 ), #16307, .F. ) ;
#65983 = DIRECTION ( 'NONE',  ( 0.000000000000000000, 0.3090169943749410120, 0.9510565162951556406 ) ) ;
#65984 = CARTESIAN_POINT ( 'NONE',  ( 93.67500000000001137, -207.7050326799711968, 82.90916666666666401 ) ) ;
#65985 = CARTESIAN_POINT ( 'NONE',  ( 92.35000000001612364, -210.0000060634596082, 88.17456390440206349 ) ) ;
#65986 = DIRECTION ( 'NONE',  ( 0.000000000000000000, 0.000000000000000000, 1.000000000000000000 ) ) ;
#65987 = CARTESIAN_POINT ( 'NONE',  ( -95.00000000000002842, 86.94004357329504273, 76.26812500173430465 ) ) ;
#65988 = CARTESIAN_POINT ( 'NONE',  ( -94.99999999999997158, -207.3369185715606307, 75.03781250086714749 ) ) ;
#65989 = AXIS2_PLACEMENT_3D ( 'NONE', #30523, #71483, #8721 ) ;
#65990 = EDGE_LOOP ( 'NONE', ( #31178, #52895, #22033, #58511 ) ) ;
#65991 = CIRCLE ( 'NONE', #43179, 31.99999999999999289 ) ;
#65992 = AXIS2_PLACEMENT_3D ( 'NONE', #2837, #1732, #59206 ) ;
#65993 = LINE ( 'NONE', #71223, #720 ) ;
#65994 = ADVANCED_FACE ( 'NONE', ( #39618 ), #9272, .T. ) ;
#65995 = EDGE_CURVE ( 'NONE', #56884, #29668, #32191, .T. ) ;
#65996 = DIRECTION ( 'NONE',  ( -1.000000000000000000, -0.000000000000000000, 0.000000000000000000 ) ) ;
#65997 = CARTESIAN_POINT ( 'NONE',  ( -96.32500000000001705, 92.29496732002878900, 79.09916666666666174 ) ) ;
#65998 = CARTESIAN_POINT ( 'NONE',  ( 97.64999999999999147, 90.00000000000002842, 90.00000000000000000 ) ) ;
#65999 = LINE ( 'NONE', #20493, #62963 ) ;
#66000 = CARTESIAN_POINT ( 'NONE',  ( 0.000000000000000000, -8.840884882375609877, 74.65374052328647281 ) ) ;
#66001 = CYLINDRICAL_SURFACE ( 'NONE', #67408, 42.00000000000000000 ) ;
#66002 = CARTESIAN_POINT ( 'NONE',  ( 12.13205353604972991, -140.1820037904669789, 5.500000000000000000 ) ) ;
#66003 = CARTESIAN_POINT ( 'NONE',  ( 6.000000000000000000, 2.543863470249533965, -81.96053171279901051 ) ) ;
#66004 = CARTESIAN_POINT ( 'NONE',  ( 97.30629616937498838, 88.66845928578035796, 83.08114583420048405 ) ) ;
#66005 = CARTESIAN_POINT ( 'NONE',  ( -96.15314808468747287, -208.0026889286704943, 83.98072916753382344 ) ) ;
#66006 = DIRECTION ( 'NONE',  ( -0.000000000000000000, -0.000000000000000000, 1.000000000000000000 ) ) ;
#66007 = VERTEX_POINT ( 'NONE', #67811 ) ;
#66008 = DIRECTION ( 'NONE',  ( 0.000000000000000000, 0.000000000000000000, 1.000000000000000000 ) ) ;
#66009 = CARTESIAN_POINT ( 'NONE',  ( -97.64999999999994884, -211.5299782133524502, 78.62291666666668277 ) ) ;
#66010 = CARTESIAN_POINT ( 'NONE',  ( 15.00000000000000000, -26.23277895567245466, 4.042438405570107918 ) ) ;
#66011 = AXIS2_PLACEMENT_3D ( 'NONE', #29491, #47175, #35517 ) ;
#66012 = CIRCLE ( 'NONE', #28804, 31.99999999999999289 ) ;
#66013 = AXIS2_PLACEMENT_3D ( 'NONE', #68151, #4645, #56514 ) ;
#66014 = AXIS2_PLACEMENT_3D ( 'NONE', #11528, #51758, #67571 ) ;
#66015 = CARTESIAN_POINT ( 'NONE',  ( 93.84685191531251292, -211.9973110713294489, 83.39864583420047950 ) ) ;
#66016 = ORIENTED_EDGE ( 'NONE', *, *, #3433, .T. ) ;
#66017 = CARTESIAN_POINT ( 'NONE',  ( 96.66135172262724495, 88.39919842643632819, 74.79754476654878204 ) ) ;
#66018 = ORIENTED_EDGE ( 'NONE', *, *, #38718, .F. ) ;
#66019 = VERTEX_POINT ( 'NONE', #62177 ) ;
#66020 = DIRECTION ( 'NONE',  ( -1.000000000000000000, -0.000000000000000000, 0.000000000000000000 ) ) ;
#66021 = VERTEX_POINT ( 'NONE', #45263 ) ;
#66022 = DIRECTION ( 'NONE',  ( -0.000000000000000000, -0.000000000000000000, -1.000000000000000000 ) ) ;
#66023 = CARTESIAN_POINT ( 'NONE',  ( 95.00000000000000000, -212.6630814284392557, 79.16531250086715943 ) ) ;
#66024 = LINE ( 'NONE', #36321, #889 ) ;
#66025 = CARTESIAN_POINT ( 'NONE',  ( 0.000000000000000000, -21.60688246758642705, 79.10210256391360417 ) ) ;
#66026 = FACE_OUTER_BOUND ( 'NONE', #60088, .T. ) ;
#66027 = CARTESIAN_POINT ( 'NONE',  ( -95.00000000000002842, 90.00000000000004263, 90.00000000000000000 ) ) ;
#66028 = CIRCLE ( 'NONE', #73196, 16.00000000000000000 ) ;
#66029 = CARTESIAN_POINT ( 'NONE',  ( 11.99999999999999822, -74.65491531819111515, 23.16904090965678265 ) ) ;
#66030 = CARTESIAN_POINT ( 'NONE',  ( 95.00000000000000000, -206.9400435732949575, 80.31624999999998238 ) ) ;
#66031 = PRODUCT_RELATED_PRODUCT_CATEGORY ( 'part', '', ( #11005 ) ) ;
#66032 = AXIS2_PLACEMENT_3D ( 'NONE', #25728, #4672, #21942 ) ;
#66033 = ADVANCED_FACE ( 'NONE', ( #56914 ), #28316, .T. ) ;
#66034 = EDGE_LOOP ( 'NONE', ( #30400, #14354, #10176, #17305 ) ) ;
#66035 = ORIENTED_EDGE ( 'NONE', *, *, #20175, .T. ) ;
#66036 = VECTOR ( 'NONE', #67825, 1000.000000000000000 ) ;
#66037 = ORIENTED_EDGE ( 'NONE', *, *, #58219, .F. ) ;
#66038 = ORIENTED_EDGE ( 'NONE', *, *, #33885, .T. ) ;
#66039 = CYLINDRICAL_SURFACE ( 'NONE', #63461, 16.00000000000000000 ) ;
#66040 = CARTESIAN_POINT ( 'NONE',  ( -96.15314808468751551, 88.00268892867056536, 84.82739583420048746 ) ) ;
#66041 = EDGE_CURVE ( 'NONE', #5572, #39383, #39103, .T. ) ;
#66042 = CARTESIAN_POINT ( 'NONE',  ( 0.000000000000000000, 0.000000000000000000, 0.000000000000000000 ) ) ;
#66043 = DIRECTION ( 'NONE',  ( -1.000000000000000000, 0.000000000000000000, 0.000000000000000000 ) ) ;
#66044 = FACE_OUTER_BOUND ( 'NONE', #52487, .T. ) ;
#66045 = CARTESIAN_POINT ( 'NONE',  ( -92.34999999999999432, -210.0000000255707278, 84.04687500080852658 ) ) ;
#66047 = ORIENTED_EDGE ( 'NONE', *, *, #43833, .T. ) ;
#66046 = EDGE_CURVE ( 'NONE', #22373, #8165, #28307, .T. ) ;
#66048 = CARTESIAN_POINT ( 'NONE',  ( -97.64999999999994884, -208.4700217866474645, 87.48645833506763836 ) ) ;
#66049 = ORIENTED_EDGE ( 'NONE', *, *, #54257, .F. ) ;
#66050 = DIRECTION ( 'NONE',  ( 0.000000000000000000, 0.000000000000000000, 1.000000000000000000 ) ) ;
#66051 = EDGE_LOOP ( 'NONE', ( #39673, #49255, #55195, #7390 ) ) ;
#66052 = CARTESIAN_POINT ( 'NONE',  ( -93.67500000000003979, 87.70503267997129626, 87.75104166840095843 ) ) ;
#66053 = EDGE_CURVE ( 'NONE', #33537, #11359, #59493, .T. ) ;
#66054 = VERTEX_POINT ( 'NONE', #70015 ) ;
#66055 = CARTESIAN_POINT ( 'NONE',  ( 94.99999999999998579, 92.66308142843935514, 88.37281250086715545 ) ) ;
#66056 = CARTESIAN_POINT ( 'NONE',  ( 10.00000000000000000, -79.10210256391353312, -21.60688246758667574 ) ) ;
#66057 = CARTESIAN_POINT ( 'NONE',  ( -95.00000000000002842, 86.94004357329504273, 85.79312500173431033 ) ) ;
#66058 = CARTESIAN_POINT ( 'NONE',  ( 10.00000000000000000, 10.96151621346487914, 35.95386929396260456 ) ) ;
#66059 = VECTOR ( 'NONE', #72422, 1000.000000000000000 ) ;
#66060 = DIRECTION ( 'NONE',  ( -0.000000000000000000, -0.000000000000000000, 1.000000000000000000 ) ) ;
#66061 = LINE ( 'NONE', #42743, #10870 ) ;
#66062 = EDGE_LOOP ( 'NONE', ( #6018, #17014, #17575, #65378 ) ) ;
#66063 = LINE ( 'NONE', #7789, #48325 ) ;
#66064 = AXIS2_PLACEMENT_3D ( 'NONE', #72440, #36756, #2598 ) ;
#66065 = CIRCLE ( 'NONE', #48018, 31.99999999999998934 ) ;
#66067 = DIRECTION ( 'NONE',  ( -1.000000000000000000, 0.000000000000000000, 0.000000000000000000 ) ) ;
#66066 = VECTOR ( 'NONE', #54590, 1000.000000000000000 ) ;
#66068 = ORIENTED_EDGE ( 'NONE', *, *, #16366, .T. ) ;
#66069 = ORIENTED_EDGE ( 'NONE', *, *, #26060, .F. ) ;
#66070 = DIRECTION ( 'NONE',  ( -1.000000000000000000, -0.000000000000000000, 0.000000000000000000 ) ) ;
#66071 = AXIS2_PLACEMENT_3D ( 'NONE', #61321, #55667, #27834 ) ;
#66072 = VECTOR ( 'NONE', #28634, 1000.000000000000000 ) ;
#66073 = EDGE_CURVE ( 'NONE', #67235, #50834, #58377, .T. ) ;
#66074 = ADVANCED_FACE ( 'NONE', ( #18883 ), #1290, .T. ) ;
#66075 = FACE_OUTER_BOUND ( 'NONE', #50295, .T. ) ;
#66076 = CARTESIAN_POINT ( 'NONE',  ( -92.34999999999999432, -209.9999999999999716, 83.33250000000001023 ) ) ;
#66077 = CARTESIAN_POINT ( 'NONE',  ( -96.15314808468747287, -208.0026889286704943, 85.88572916753381037 ) ) ;
#66078 = ORIENTED_EDGE ( 'NONE', *, *, #34734, .T. ) ;
#66079 = DIRECTION ( 'NONE',  ( -1.000000000000000000, -0.000000000000000000, -0.000000000000000000 ) ) ;
#66080 = ORIENTED_EDGE ( 'NONE', *, *, #43997, .F. ) ;
#66081 = CARTESIAN_POINT ( 'NONE',  ( 10.00000000000000000, 74.65374052328660071, -8.840884882374309583 ) ) ;
#66082 = CIRCLE ( 'NONE', #39668, 0.2999999999999999334 ) ;
#66083 = EDGE_CURVE ( 'NONE', #11727, #1166, #33071, .T. ) ;
#66084 = CARTESIAN_POINT ( 'NONE',  ( -10.00000000000000000, 0.000000000000000000, 0.000000000000000000 ) ) ;
#66085 = DIRECTION ( 'NONE',  ( -1.000000000000000000, -0.000000000000000000, 0.000000000000000000 ) ) ;
#66086 = CARTESIAN_POINT ( 'NONE',  ( 93.84685191531248449, 91.99731107132950569, 79.37697916753380412 ) ) ;
#66087 = LINE ( 'NONE', #55151, #53262 ) ;
#66088 = CARTESIAN_POINT ( 'NONE',  ( 0.000000000000000000, 0.000000000000000000, -80.00000000000000000 ) ) ;
#66089 = DIRECTION ( 'NONE',  ( -1.000000000000000000, 0.000000000000000000, -0.000000000000000000 ) ) ;
#66090 = CARTESIAN_POINT ( 'NONE',  ( 93.86969025972511815, 92.14422361751726953, 74.86230178910948041 ) ) ;
#66091 = DIRECTION ( 'NONE',  ( -1.000000000000000000, 0.000000000000000000, -0.000000000000000000 ) ) ;
#66092 = FACE_OUTER_BOUND ( 'NONE', #51728, .T. ) ;
#66093 = CARTESIAN_POINT ( 'NONE',  ( 0.000000000000000000, 77.19088730480532945, -6.903761155836913410 ) ) ;
#66094 = VERTEX_POINT ( 'NONE', #24178 ) ;
#66095 = VECTOR ( 'NONE', #9665, 1000.000000000000000 ) ;
#66096 = CARTESIAN_POINT ( 'NONE',  ( -92.69370383062505425, 88.66845928578038638, 82.92239583420045790 ) ) ;
#66097 = VECTOR ( 'NONE', #53586, 1000.000000000000000 ) ;
#66098 = PLANE ( 'NONE',  #40757 ) ;
#66099 = AXIS2_PLACEMENT_3D ( 'NONE', #18686, #13047, #69106 ) ;
#66100 = CARTESIAN_POINT ( 'NONE',  ( 10.00000000000000000, -35.47612816024506088, -22.48208911017539435 ) ) ;
#66101 = ORIENTED_EDGE ( 'NONE', *, *, #43379, .T. ) ;
#66102 = CARTESIAN_POINT ( 'NONE',  ( -97.64999999996706492, -209.9999916046304520, 84.99910573338409847 ) ) ;
#66103 = DIRECTION ( 'NONE',  ( -1.000000000000000000, 0.000000000000000000, -0.000000000000000000 ) ) ;
#66104 = DIRECTION ( 'NONE',  ( -7.959965316982041921E-16, -1.065814103640131188E-14, -1.000000000000000000 ) ) ;
#66105 = EDGE_CURVE ( 'NONE', #27755, #19421, #6693, .T. ) ;
#66106 = AXIS2_PLACEMENT_3D ( 'NONE', #45365, #32934, #62664 ) ;
#66107 = AXIS2_PLACEMENT_3D ( 'NONE', #1998, #2742, #36905 ) ;
#66108 = CARTESIAN_POINT ( 'NONE',  ( 97.30629616937498838, -208.6684592857803011, 78.74197916753382742 ) ) ;
#66109 = EDGE_LOOP ( 'NONE', ( #19218, #74223, #36173, #42573 ) ) ;
#66110 = EDGE_CURVE ( 'NONE', #46803, #25695, #30900, .T. ) ;
#66111 = ORIENTED_EDGE ( 'NONE', *, *, #71864, .F. ) ;
#66112 = EDGE_CURVE ( 'NONE', #26348, #17504, #40725, .T. ) ;
#66113 = CARTESIAN_POINT ( 'NONE',  ( 5.000000000000002665, -34.94270380257586339, -74.18225833017926618 ) ) ;
#66114 = DIRECTION ( 'NONE',  ( -1.000000000000000000, 0.000000000000000000, -0.000000000000000000 ) ) ;
#66115 = CARTESIAN_POINT ( 'NONE',  ( 0.000000000000000000, 35.53030884539102630, -12.26510123303222599 ) ) ;
#66116 = ORIENTED_EDGE ( 'NONE', *, *, #69780, .T. ) ;
#66117 = CARTESIAN_POINT ( 'NONE',  ( 22.08297821871651934, -111.8242998470044540, 5.500000000000000000 ) ) ;
#66118 = CARTESIAN_POINT ( 'NONE',  ( 92.69370383062501162, -209.9999999999999716, 75.19656250086714522 ) ) ;
#66119 = ADVANCED_FACE ( 'NONE', ( #2392 ), #12872, .T. ) ;
#66120 = EDGE_LOOP ( 'NONE', ( #65274, #64285, #70003, #58426 ) ) ;
#66121 = CARTESIAN_POINT ( 'NONE',  ( 0.000000000000000000, 0.000000000000000000, 0.000000000000000000 ) ) ;
#66122 = ORIENTED_EDGE ( 'NONE', *, *, #15592, .F. ) ;
#66123 = ORIENTED_EDGE ( 'NONE', *, *, #41830, .T. ) ;
#66124 = CARTESIAN_POINT ( 'NONE',  ( -11.70000000000000107, 0.000000000000000000, -20.69999999999999929 ) ) ;
#66125 =( LENGTH_UNIT ( ) NAMED_UNIT ( * ) SI_UNIT ( .MILLI., .METRE. ) );
#66126 = CARTESIAN_POINT ( 'NONE',  ( 22.08297821871651934, -111.8242998470044540, -5.500000000000000000 ) ) ;
#66127 = ORIENTED_EDGE ( 'NONE', *, *, #59699, .T. ) ;
#66128 = FACE_OUTER_BOUND ( 'NONE', #64337, .T. ) ;
#66129 = CARTESIAN_POINT ( 'NONE',  ( 93.67500000000001137, -212.2949673200287179, 79.39020833506762642 ) ) ;
#66130 = CARTESIAN_POINT ( 'NONE',  ( 92.34999999999999432, 88.47002178664753558, 84.97291666666666288 ) ) ;
#66131 = ORIENTED_EDGE ( 'NONE', *, *, #58726, .T. ) ;
#66132 = CARTESIAN_POINT ( 'NONE',  ( 6.000000000000000000, -74.18225833017913828, 34.94270380257611208 ) ) ;
#66133 = CARTESIAN_POINT ( 'NONE',  ( -10.21100092698785033, -95.54625877152835756, 2.500000000000000000 ) ) ;
#66134 = ORIENTED_EDGE ( 'NONE', *, *, #42219, .T. ) ;
#66135 = ORIENTED_EDGE ( 'NONE', *, *, #43810, .T. ) ;
#66136 = CARTESIAN_POINT ( 'NONE',  ( -96.15314808468751551, 88.00268892867056536, 89.27239583420049485 ) ) ;
#66137 = ADVANCED_FACE ( 'NONE', ( #42211 ), #7616, .F. ) ;
#66138 = CARTESIAN_POINT ( 'NONE',  ( 92.69370383062498320, 90.00000000000002842, 80.75281250086715090 ) ) ;
#66139 = ORIENTED_EDGE ( 'NONE', *, *, #4186, .T. ) ;
#66140 = CARTESIAN_POINT ( 'NONE',  ( 92.34999999999999432, 90.00000000000002842, 82.45937500173430124 ) ) ;
#66141 = VECTOR ( 'NONE', #66089, 1000.000000000000000 ) ;
#66142 = CARTESIAN_POINT ( 'NONE',  ( 10.00000000000000000, 0.000000000000000000, 77.49899999999999523 ) ) ;
#66143 = ORIENTED_EDGE ( 'NONE', *, *, #15958, .T. ) ;
#66144 = AXIS2_PLACEMENT_3D ( 'NONE', #47201, #58112, #70114 ) ;
#66145 = VERTEX_POINT ( 'NONE', #29416 ) ;
#66146 = ORIENTED_EDGE ( 'NONE', *, *, #28786, .F. ) ;
#66147 = ORIENTED_EDGE ( 'NONE', *, *, #26837, .F. ) ;
#66148 = DIRECTION ( 'NONE',  ( -1.000000000000000000, -0.000000000000000000, -0.000000000000000000 ) ) ;
#66149 = DIRECTION ( 'NONE',  ( 0.000000000000000000, 0.000000000000000000, 1.000000000000000000 ) ) ;
#66150 = CARTESIAN_POINT ( 'NONE',  ( -93.67500000000003979, 92.29496732002878900, 84.07333333333333769 ) ) ;
#66151 = EDGE_CURVE ( 'NONE', #51673, #54454, #70378, .T. ) ;
#66152 = ORIENTED_EDGE ( 'NONE', *, *, #23887, .T. ) ;
#66153 = EDGE_CURVE ( 'NONE', #42089, #32443, #35502, .T. ) ;
#66154 = LINE ( 'NONE', #67254, #69584 ) ;
#66155 = CARTESIAN_POINT ( 'NONE',  ( 97.64999999999997726, 88.47002178664753558, 88.43895833506762472 ) ) ;
#66156 = EDGE_LOOP ( 'NONE', ( #67911, #58183, #60425, #26422 ) ) ;
#66157 =( BOUNDED_CURVE ( )  B_SPLINE_CURVE ( 2, ( #40531, #44709, #6340, #62378, #39058, #67625, #69118 ),
 .UNSPECIFIED., .F., .F. ) 
 B_SPLINE_CURVE_WITH_KNOTS ( ( 3, 2, 2, 3 ),
 ( 0.6041666666666670737, 0.6111111111111116045, 0.6180555555555559133, 0.6250000000000003331 ),
 .UNSPECIFIED. ) 
 CURVE ( )  GEOMETRIC_REPRESENTATION_ITEM ( )  RATIONAL_B_SPLINE_CURVE ( ( 0.9999999999999914513, 0.8660254037844472563, 1.000000000000000000, 0.8660254037844387076, 1.000000000000000000, 0.8660254037844322683, 1.000000000000006439 ) ) 
 REPRESENTATION_ITEM ( '' )  );
#66158 = DIRECTION ( 'NONE',  ( 1.000000000000000000, 0.000000000000000000, 0.000000000000000000 ) ) ;
#66159 = CARTESIAN_POINT ( 'NONE',  ( -94.99999999999997158, -207.3369185715606307, 79.32406250086714294 ) ) ;
#66160 = VERTEX_POINT ( 'NONE', #29790 ) ;
#66161 = ADVANCED_FACE ( 'NONE', ( #64401 ), #52742, .T. ) ;
#66162 = PLANE ( 'NONE',  #19429 ) ;
#66163 = FACE_OUTER_BOUND ( 'NONE', #65403, .T. ) ;
#66164 = CYLINDRICAL_SURFACE ( 'NONE', #46557, 2.649999999999985700 ) ;
#66165 = DIRECTION ( 'NONE',  ( 1.000000000000000000, 1.427937372958405461E-15, 7.962523111839130290E-16 ) ) ;
#66166 = PLANE ( 'NONE',  #57200 ) ;
#66167 = AXIS2_PLACEMENT_3D ( 'NONE', #53948, #60335, #64861 ) ;
#66168 = CIRCLE ( 'NONE', #33735, 31.99999999999998934 ) ;
#66169 = DIRECTION ( 'NONE',  ( 0.9227826878668540234, 0.3853207896976547087, 0.000000000000000000 ) ) ;
#66170 = CARTESIAN_POINT ( 'NONE',  ( 93.84685191531248449, 88.00268892867053694, 87.20864583420046756 ) ) ;
#66171 = CARTESIAN_POINT ( 'NONE',  ( 92.35000000006145626, -209.9999881787626919, 81.82400613091914465 ) ) ;
#66172 = AXIS2_PLACEMENT_3D ( 'NONE', #73644, #2777, #54610 ) ;
#66173 = CARTESIAN_POINT ( 'NONE',  ( -97.64999999992174651, -209.9999869687493685, 79.28395951166956479 ) ) ;
#66174 = CARTESIAN_POINT ( 'NONE',  ( -97.65000000000001990, 90.00000000000004263, 81.74500000000000455 ) ) ;
#66175 = CARTESIAN_POINT ( 'NONE',  ( -96.15314808468752972, 91.99731107132950569, 74.93197916753379673 ) ) ;
#66176 = DIRECTION ( 'NONE',  ( 0.000000000000000000, 0.9723699203976773342, -0.2334453638559024491 ) ) ;
#66177 = FACE_OUTER_BOUND ( 'NONE', #47074, .T. ) ;
#66178 = CARTESIAN_POINT ( 'NONE',  ( 92.35000000000009379, -208.4700217866474361, 75.34208333333333485 ) ) ;
#66179 = CARTESIAN_POINT ( 'NONE',  ( 10.00000000000000000, -67.80270845531921964, 46.11716303203163392 ) ) ;
#66180 = CARTESIAN_POINT ( 'NONE',  ( 0.000000000000000000, -55.38113227695820484, 54.21277698773656084 ) ) ;
#66181 = CARTESIAN_POINT ( 'NONE',  ( 12.00000000000000000, -18.13022148937242761, 15.02647892043569122 ) ) ;
#66182 = LINE ( 'NONE', #51751, #26851 ) ;
#66183 = CARTESIAN_POINT ( 'NONE',  ( -94.99999999999997158, -213.0599564267049857, 87.61875000000000568 ) ) ;
#66184 = CARTESIAN_POINT ( 'NONE',  ( 10.00000000000000000, 0.000000000000000000, 0.000000000000000000 ) ) ;
#66185 = PRODUCT ( 'CIRCLIP DIN 471 - 25 \X2\00d7\X0\ 1.2_GB_CONNECTING_PIECE_RING_RRA 25', 'CIRCLIP DIN 471 - 25 \X2\00d7\X0\ 1.2_GB_CONNECTING_PIECE_RING_RRA 25', '', ( #27559 ) ) ;
#66186 = ORIENTED_EDGE ( 'NONE', *, *, #59623, .T. ) ;
#66187 = DIRECTION ( 'NONE',  ( 0.000000000000000000, 0.000000000000000000, 1.000000000000000000 ) ) ;
#66188 = CARTESIAN_POINT ( 'NONE',  ( 97.64998213368573943, -211.5299885284737513, 78.27895762153872283 ) ) ;
#66189 = CARTESIAN_POINT ( 'NONE',  ( -95.00000000000002842, 93.05995642670504253, 84.76125000000000398 ) ) ;
#66190 = EDGE_CURVE ( 'NONE', #25525, #52624, #41824, .T. ) ;
#66191 = PRESENTATION_LAYER_ASSIGNMENT (  '', '', ( #24175 ) ) ;
#66192 = AXIS2_PLACEMENT_3D ( 'NONE', #15653, #49847, #72764 ) ;
#66193 = AXIS2_PLACEMENT_3D ( 'NONE', #30181, #63681, #64046 ) ;
#66194 = VERTEX_POINT ( 'NONE', #64770 ) ;
#66195 = EDGE_CURVE ( 'NONE', #68891, #68659, #2016, .T. ) ;
#66196 = EDGE_LOOP ( 'NONE', ( #18826, #16176, #31024, #20783 ) ) ;
#66198 = EDGE_CURVE ( 'NONE', #14207, #22781, #37313, .T. ) ;
#66197 = DIRECTION ( 'NONE',  ( -1.000000000000000000, 0.000000000000000000, 0.000000000000000000 ) ) ;
#66199 = VECTOR ( 'NONE', #47279, 1000.000000000000000 ) ;
#66200 = DIRECTION ( 'NONE',  ( 0.000000000000000000, 0.000000000000000000, 1.000000000000000000 ) ) ;
#66201 = VERTEX_POINT ( 'NONE', #48579 ) ;
#66202 = APPLICATION_CONTEXT ( 'automotive_design' ) ;
#66203 = CARTESIAN_POINT ( 'NONE',  ( 92.69370383062501162, -211.3315407142195852, 80.17072916753380696 ) ) ;
#66204 = CARTESIAN_POINT ( 'NONE',  ( 97.30629616937498838, -209.9999999999999716, 85.03906250086714635 ) ) ;
#66205 = EDGE_LOOP ( 'NONE', ( #48616, #3051, #44008, #41640 ) ) ;
#66206 = CARTESIAN_POINT ( 'NONE',  ( 97.30629616937498838, -211.3315407142195852, 85.62114583420047609 ) ) ;
#66207 = EDGE_CURVE ( 'NONE', #729, #9618, #18699, .T. ) ;
#66208 = VERTEX_POINT ( 'NONE', #26008 ) ;
#66209 = FACE_BOUND ( 'NONE', #51527, .T. ) ;
#66210 = ORIENTED_EDGE ( 'NONE', *, *, #28400, .T. ) ;
#66211 = VECTOR ( 'NONE', #538, 1000.000000000000000 ) ;
#66212 = CARTESIAN_POINT ( 'NONE',  ( -95.00000000000002842, 92.66308142843932671, 76.94281250086714863 ) ) ;
#66213 = AXIS2_PLACEMENT_3D ( 'NONE', #38306, #61247, #73617 ) ;
#66214 = ORIENTED_EDGE ( 'NONE', *, *, #6378, .T. ) ;
#66215 = ORIENTED_EDGE ( 'NONE', *, *, #66871, .F. ) ;
#66216 = LINE ( 'NONE', #3440, #50896 ) ;
#66217 = ORIENTED_EDGE ( 'NONE', *, *, #37349, .T. ) ;
#66218 = DIRECTION ( 'NONE',  ( 0.000000000000000000, 0.9876883405951381034, -0.1564344650402276216 ) ) ;
#66219 = CARTESIAN_POINT ( 'NONE',  ( 10.00000000000000000, 75.11764819372142199, 2.946379043147685728 ) ) ;
#66220 = VERTEX_POINT ( 'NONE', #3114 ) ;
#66221 = CARTESIAN_POINT ( 'NONE',  ( 11.99999999999999822, 34.94270380257741238, -74.18225833017854143 ) ) ;
#66222 = ORIENTED_EDGE ( 'NONE', *, *, #55327, .F. ) ;
#66223 = LINE ( 'NONE', #13946, #97 ) ;
#66224 = EDGE_CURVE ( 'NONE', #68284, #9787, #55698, .T. ) ;
#66225 = ORIENTED_EDGE ( 'NONE', *, *, #25206, .F. ) ;
#66226 = ORIENTED_EDGE ( 'NONE', *, *, #36266, .F. ) ;
#66227 = ORIENTED_EDGE ( 'NONE', *, *, #22061, .F. ) ;
#66228 = CARTESIAN_POINT ( 'NONE',  ( 95.00000000000000000, -212.6630814284392557, 79.64156250086713840 ) ) ;
#66229 = DIRECTION ( 'NONE',  ( -1.000000000000000000, 7.571537405616606460E-15, 2.598394312951952234E-14 ) ) ;
#66230 = ITEM_DEFINED_TRANSFORMATION ( 'NONE', 'NONE', #54423,  #43395 ) ;
#66231 = DIRECTION ( 'NONE',  ( 1.000000000000000000, 0.000000000000000000, 0.000000000000000000 ) ) ;
#66232 = EDGE_LOOP ( 'NONE', ( #18559, #44302, #22690, #32257 ) ) ;
#66233 = EDGE_LOOP ( 'NONE', ( #40466, #55869, #57169, #30904 ) ) ;
#66234 = DIRECTION ( 'NONE',  ( -1.000000000000000000, 0.000000000000000000, -0.000000000000000000 ) ) ;
#66235 = ORIENTED_EDGE ( 'NONE', *, *, #58326, .F. ) ;
#66236 = CARTESIAN_POINT ( 'NONE',  ( 2.117611129180199558, -93.54218975225703048, 5.500000000000000000 ) ) ;
#66237 = DIRECTION ( 'NONE',  ( 0.000000000000000000, 0.000000000000000000, 1.000000000000000000 ) ) ;
#66238 = CARTESIAN_POINT ( 'NONE',  ( -97.30629616937501680, 90.00000000000004263, 79.64156250086715261 ) ) ;
#66239 = EDGE_CURVE ( 'NONE', #62527, #991, #3843, .T. ) ;
#66240 = ORIENTED_EDGE ( 'NONE', *, *, #68842, .T. ) ;
#66241 = EDGE_CURVE ( 'NONE', #47803, #56493, #42947, .T. ) ;
#66242 = CARTESIAN_POINT ( 'NONE',  ( 92.69370383062498320, 90.00000000000002842, 76.94281250086713442 ) ) ;
#66243 = ORIENTED_EDGE ( 'NONE', *, *, #16617, .F. ) ;
#66244 = FACE_OUTER_BOUND ( 'NONE', #18983, .T. ) ;
#66245 = LINE ( 'NONE', #61342, #41989 ) ;
#66246 = FACE_OUTER_BOUND ( 'NONE', #61860, .T. ) ;
#66247 = CARTESIAN_POINT ( 'NONE',  ( 5.000000000000000000, 26.79245525562762253, -32.34446384429941901 ) ) ;
#66248 = CARTESIAN_POINT ( 'NONE',  ( -92.69370383062498320, -209.9999999999999716, 84.24531250086714351 ) ) ;
#66249 = STYLED_ITEM ( 'NONE', ( #40973 ), #34586 ) ;
#66250 = AXIS2_PLACEMENT_3D ( 'NONE', #58286, #28592, #12780 ) ;
#66251 = CARTESIAN_POINT ( 'NONE',  ( -3.000000000000000000, 8.688484142253939169, 21.88630264137371029 ) ) ;
#66252 = DIRECTION ( 'NONE',  ( -1.000000000000000000, 0.000000000000000000, -0.000000000000000000 ) ) ;
#66253 = DIRECTION ( 'NONE',  ( 0.000000000000000000, 0.000000000000000000, 1.000000000000000000 ) ) ;
#66254 = ORIENTED_EDGE ( 'NONE', *, *, #15216, .T. ) ;
#66255 = AXIS2_PLACEMENT_3D ( 'NONE', #37230, #42865, #59051 ) ;
#66256 = ORIENTED_EDGE ( 'NONE', *, *, #14084, .T. ) ;
#66257 = CARTESIAN_POINT ( 'NONE',  ( 23.49955575014745435, 0.001194404164629722436, -64.00000000000000000 ) ) ;
#66258 = DIRECTION ( 'NONE',  ( 0.000000000000000000, -0.1045284632676578424, 0.9945218953682729568 ) ) ;
#66259 = LINE ( 'NONE', #65890, #62028 ) ;
#66260 = VECTOR ( 'NONE', #46083, 1000.000000000000000 ) ;
#66261 = CARTESIAN_POINT ( 'NONE',  ( -92.69370383062502583, 91.33154071421968467, 86.83822916753381094 ) ) ;
#66262 = DIRECTION ( 'NONE',  ( 0.000000000000000000, 0.1564344650402311743, -0.9876883405951377704 ) ) ;
#66263 = DIRECTION ( 'NONE',  ( 0.000000000000000000, 0.000000000000000000, -1.000000000000000000 ) ) ;
#66264 = FACE_OUTER_BOUND ( 'NONE', #48897, .T. ) ;
#66265 = ORIENTED_EDGE ( 'NONE', *, *, #15006, .F. ) ;
#66266 = DIRECTION ( 'NONE',  ( 0.4565542962317865050, 0.000000000000000000, 0.8896955516311735312 ) ) ;
#66267 = AXIS2_PLACEMENT_3D ( 'NONE', #32380, #55323, #15847 ) ;
#66268 = LINE ( 'NONE', #1396, #40075 ) ;
#66269 = CARTESIAN_POINT ( 'NONE',  ( 11.99999999999999822, 69.42325613327489009, -34.44570377933524696 ) ) ;
#66270 = CIRCLE ( 'NONE', #48230, 77.49900000000002365 ) ;
#66271 = CARTESIAN_POINT ( 'NONE',  ( 11.99999999999999822, 73.44644590900094272, -24.73286445877629802 ) ) ;
#66272 = CARTESIAN_POINT ( 'NONE',  ( 20.07203437053270179, -132.2214334768125354, -2.500000000000000000 ) ) ;
#66273 = DIRECTION ( 'NONE',  ( 0.000000000000000000, -0.000000000000000000, 1.000000000000000000 ) ) ;
#66274 = DIRECTION ( 'NONE',  ( -1.000000000000000000, -0.000000000000000000, -0.000000000000000000 ) ) ;
#66275 = CARTESIAN_POINT ( 'NONE',  ( -96.15314808468745866, -211.9973110713294489, 81.65239583420049030 ) ) ;
#66276 = CIRCLE ( 'NONE', #72261, 31.99999999999998579 ) ;
#66277 = CARTESIAN_POINT ( 'NONE',  ( 92.34999999999999432, 90.00000000000002842, 76.10937500173430692 ) ) ;
#66278 = EDGE_CURVE ( 'NONE', #42793, #2723, #26741, .T. ) ;
#66279 = CARTESIAN_POINT ( 'NONE',  ( 5.000000000000000000, -55.16347631943085617, 60.67117009219118273 ) ) ;
#66280 = EDGE_CURVE ( 'NONE', #54186, #73246, #31645, .T. ) ;
#66281 = DIRECTION ( 'NONE',  ( -1.000000000000000000, 0.000000000000000000, -0.000000000000000000 ) ) ;
#66282 = CARTESIAN_POINT ( 'NONE',  ( -26.29030328629083968, -123.6496510949466341, 5.500000000000000000 ) ) ;
#66283 = ORIENTED_EDGE ( 'NONE', *, *, #8854, .F. ) ;
#66284 = CARTESIAN_POINT ( 'NONE',  ( 10.00000000000000000, -35.38097989696520074, 12.42422080174625520 ) ) ;
#66285 = CARTESIAN_POINT ( 'NONE',  ( -10.00000000000000000, 0.000000000000000000, 0.000000000000000000 ) ) ;
#66286 = DIRECTION ( 'NONE',  ( -1.000000000000000000, -0.000000000000000000, 0.000000000000000000 ) ) ;
#66287 = EDGE_CURVE ( 'NONE', #991, #31033, #17532, .T. ) ;
#66288 = EDGE_CURVE ( 'NONE', #37558, #5960, #38034, .T. ) ;
#66289 = DIRECTION ( 'NONE',  ( -1.000000000000000000, 0.000000000000000000, 0.000000000000000000 ) ) ;
#66290 = VERTEX_POINT ( 'NONE', #49670 ) ;
#66291 = DIRECTION ( 'NONE',  ( -1.000000000000000000, 0.000000000000000000, 0.000000000000000000 ) ) ;
#66292 = EDGE_LOOP ( 'NONE', ( #72103, #41519, #57701, #40600 ) ) ;
#66293 = DIRECTION ( 'NONE',  ( -1.000000000000000000, -0.000000000000000000, -0.000000000000000000 ) ) ;
#66294 = ORIENTED_EDGE ( 'NONE', *, *, #44760, .T. ) ;
#66295 = EDGE_CURVE ( 'NONE', #14366, #64530, #25284, .T. ) ;
#66296 = PRESENTATION_LAYER_ASSIGNMENT (  '', '', ( #47083 ) ) ;
#66297 = CIRCLE ( 'NONE', #12244, 77.49900000000000944 ) ;
#66298 = EDGE_LOOP ( 'NONE', ( #60732, #16161, #71683 ) ) ;
#66299 = FACE_OUTER_BOUND ( 'NONE', #36243, .T. ) ;
#66300 = AXIS2_PLACEMENT_3D ( 'NONE', #42042, #25110, #13081 ) ;
#66301 = EDGE_LOOP ( 'NONE', ( #31599, #44124, #63023, #52071 ) ) ;
#66302 = EDGE_LOOP ( 'NONE', ( #63456, #65262, #54926, #4267 ) ) ;
#66303 = ORIENTED_EDGE ( 'NONE', *, *, #10532, .T. ) ;
#66304 = VERTEX_POINT ( 'NONE', #43332 ) ;
#66305 = CARTESIAN_POINT ( 'NONE',  ( -2.500000000000020428, -90.00000000000000000, -310.0000000000000000 ) ) ;
#66306 = AXIS2_PLACEMENT_3D ( 'NONE', #56363, #66165, #10112 ) ;
#66307 = VERTEX_POINT ( 'NONE', #26379 ) ;
#66308 = EDGE_CURVE ( 'NONE', #53075, #25170, #30716, .T. ) ;
#66309 = CIRCLE ( 'NONE', #7480, 31.99999999999999645 ) ;
#66310 = ORIENTED_EDGE ( 'NONE', *, *, #53073, .F. ) ;
#66311 = CARTESIAN_POINT ( 'NONE',  ( 97.30629616937498838, 88.66845928578037217, 78.00114583420049996 ) ) ;
#66312 = CARTESIAN_POINT ( 'NONE',  ( 10.00000000000000000, 10.74501242461282757, 35.92658777277515014 ) ) ;
#66313 = EDGE_CURVE ( 'NONE', #47006, #25402, #61927, .T. ) ;
#66314 = CARTESIAN_POINT ( 'NONE',  ( -92.35000000000005116, 91.52997821335253548, 87.90979166840097037 ) ) ;
#66315 = ORIENTED_EDGE ( 'NONE', *, *, #10954, .F. ) ;
#66316 = ORIENTED_EDGE ( 'NONE', *, *, #52609, .T. ) ;
#66317 = EDGE_LOOP ( 'NONE', ( #62420, #54653, #57648, #70188 ) ) ;
#66318 = CARTESIAN_POINT ( 'NONE',  ( 97.30629616937498838, 91.33154071421968467, 89.37822916753381719 ) ) ;
#66319 = CIRCLE ( 'NONE', #61544, 16.00000000000000000 ) ;
#66321 = ORIENTED_EDGE ( 'NONE', *, *, #65617, .T. ) ;
#66320 = ADVANCED_FACE ( 'NONE', ( #14726 ), #25644, .T. ) ;
#66322 = CARTESIAN_POINT ( 'NONE',  ( 97.64999999999999147, -209.9999999999999716, 74.52187500173430124 ) ) ;
#66323 = VECTOR ( 'NONE', #41172, 1000.000000000000000 ) ;
#66324 = DIRECTION ( 'NONE',  ( 0.000000000000000000, 0.000000000000000000, 1.000000000000000000 ) ) ;
#66325 = LINE ( 'NONE', #36993, #10268 ) ;
#66326 = DIRECTION ( 'NONE',  ( -1.000000000000000000, 0.000000000000000000, 0.000000000000000000 ) ) ;
#66327 = LINE ( 'NONE', #37385, #40130 ) ;
#66328 = LINE ( 'NONE', #43020, #7835 ) ;
#66329 = LINE ( 'NONE', #8053, #46844 ) ;
#66330 = CYLINDRICAL_SURFACE ( 'NONE', #38262, 31.99999999999998579 ) ;
#66331 = CARTESIAN_POINT ( 'NONE',  ( -96.32499999999996021, -207.7050326799711968, 76.00354166840097037 ) ) ;
#66332 = FACE_OUTER_BOUND ( 'NONE', #65695, .T. ) ;
#66333 = EDGE_CURVE ( 'NONE', #46613, #23253, #72593, .T. ) ;
#66334 = ORIENTED_EDGE ( 'NONE', *, *, #27157, .T. ) ;
#66335 = UNCERTAINTY_MEASURE_WITH_UNIT (LENGTH_MEASURE( 1.000000000000000082E-05 ), #47497, 'distance_accuracy_value', 'NONE');
#66337 = CARTESIAN_POINT ( 'NONE',  ( -92.69370383062502583, 88.66845928578038638, 89.27239583420048064 ) ) ;
#66336 = CARTESIAN_POINT ( 'NONE',  ( 96.15314808468748708, 91.99731107132950569, 86.25614583420048120 ) ) ;
#66338 = VERTEX_POINT ( 'NONE', #14363 ) ;
#66339 = CARTESIAN_POINT ( 'NONE',  ( 92.69370383062498320, 88.66845928578037217, 75.24947916753383481 ) ) ;
#66340 = DIRECTION ( 'NONE',  ( -1.000000000000000000, -0.000000000000000000, 0.000000000000000000 ) ) ;
#66341 = DIRECTION ( 'NONE',  ( 0.000000000000000000, -0.9781476007338043566, 0.2079116908177651712 ) ) ;
#66342 = FACE_OUTER_BOUND ( 'NONE', #46243, .T. ) ;
#66343 = DIRECTION ( 'NONE',  ( -1.000000000000000000, 0.000000000000000000, 0.000000000000000000 ) ) ;
#66344 = ADVANCED_FACE ( 'NONE', ( #43692 ), #61349, .T. ) ;
#66345 = LINE ( 'NONE', #60699, #70262 ) ;
#66346 = CARTESIAN_POINT ( 'NONE',  ( -93.67499999999998295, -212.2949673200287179, 87.67166666666666686 ) ) ;
#66347 = CARTESIAN_POINT ( 'NONE',  ( 10.00000000000000000, 0.000000000000000000, 0.000000000000000000 ) ) ;
#66348 = ORIENTED_EDGE ( 'NONE', *, *, #56377, .T. ) ;
#66349 = ORIENTED_EDGE ( 'NONE', *, *, #3779, .F. ) ;
#66350 = FACE_BOUND ( 'NONE', #8425, .T. ) ;
#66351 = FACE_OUTER_BOUND ( 'NONE', #22768, .T. ) ;
#66352 = CYLINDRICAL_SURFACE ( 'NONE', #25497, 82.00000000000000000 ) ;
#66353 = FACE_OUTER_BOUND ( 'NONE', #57532, .T. ) ;
#66354 = FACE_OUTER_BOUND ( 'NONE', #31418, .T. ) ;
#66355 = CARTESIAN_POINT ( 'NONE',  ( -96.15314808468745866, -211.9973110713294489, 75.93739583420048689 ) ) ;
#66356 = VERTEX_POINT ( 'NONE', #60611 ) ;
#66357 = CARTESIAN_POINT ( 'NONE',  ( -93.84685191531254134, 91.99731107132950569, 81.17614583420048291 ) ) ;
#66358 = CARTESIAN_POINT ( 'NONE',  ( 10.00000000000000000, 62.50884508063427347, 41.76106447765511831 ) ) ;
#66359 = DIRECTION ( 'NONE',  ( 1.000000000000000000, -0.000000000000000000, -0.000000000000000000 ) ) ;
#66360 = CIRCLE ( 'NONE', #60351, 82.00000000000000000 ) ;
#66361 = DIRECTION ( 'NONE',  ( -1.000000000000000000, 0.000000000000000000, -0.000000000000000000 ) ) ;
#66362 = DIRECTION ( 'NONE',  ( 1.000000000000000000, 0.000000000000000000, -0.000000000000000000 ) ) ;
#66363 = CARTESIAN_POINT ( 'NONE',  ( 10.00000000000000000, -32.34446384429989507, 26.79245525562703278 ) ) ;
#66364 = CARTESIAN_POINT ( 'NONE',  ( 0.000000000000000000, 0.000000000000000000, -6.000000000000001776 ) ) ;
#66365 = FACE_OUTER_BOUND ( 'NONE', #71562, .T. ) ;
#66366 = DIRECTION ( 'NONE',  ( -1.000000000000000000, 0.000000000000000000, 0.000000000000000000 ) ) ;
#66367 = DIRECTION ( 'NONE',  ( -0.000000000000000000, -0.000000000000000000, 1.000000000000000000 ) ) ;
#66368 = CIRCLE ( 'NONE', #35177, 77.49900000000000944 ) ;
#66369 =( BOUNDED_CURVE ( )  B_SPLINE_CURVE ( 2, ( #51103, #5638, #6010, #21787, #28536, #29, #28914 ),
 .UNSPECIFIED., .F., .F. ) 
 B_SPLINE_CURVE_WITH_KNOTS ( ( 3, 2, 2, 3 ),
 ( 0.8333333333333334814, 0.8402777777777779011, 0.8472222222222222099, 0.8541666666666666297 ),
 .UNSPECIFIED. ) 
 CURVE ( )  GEOMETRIC_REPRESENTATION_ITEM ( )  RATIONAL_B_SPLINE_CURVE ( ( 0.9999999999999978906, 0.8660254037844408170, 1.000000000000000000, 0.8660254037844387076, 1.000000000000000000, 0.8660254037844387076, 1.000000000000000000 ) ) 
 REPRESENTATION_ITEM ( '' )  );
#66370 = CARTESIAN_POINT ( 'NONE',  ( 96.15314808468748708, 88.00268892867053694, 81.75822916753382685 ) ) ;
#66371 = CARTESIAN_POINT ( 'NONE',  ( -92.69370383062498320, -208.6684592857803295, 82.55197916753380127 ) ) ;
#66372 = DIRECTION ( 'NONE',  ( 1.000000000000000000, 0.000000000000000000, 0.000000000000000000 ) ) ;
#66373 = ORIENTED_EDGE ( 'NONE', *, *, #2981, .T. ) ;
#66374 = DIRECTION ( 'NONE',  ( -1.000000000000000000, 0.000000000000000000, 0.000000000000000000 ) ) ;
#66375 = CARTESIAN_POINT ( 'NONE',  ( -92.34999999999999432, -208.4700217866474645, 77.03541666666666288 ) ) ;
#66376 = EDGE_CURVE ( 'NONE', #54478, #23480, #45124, .T. ) ;
#66377 = DIRECTION ( 'NONE',  ( -0.000000000000000000, -0.000000000000000000, 1.000000000000000000 ) ) ;
#66378 = AXIS2_PLACEMENT_3D ( 'NONE', #53031, #51261, #30085 ) ;
#66379 = CIRCLE ( 'NONE', #25512, 77.49900000000000944 ) ;
#66380 = EDGE_CURVE ( 'NONE', #24434, #34836, #32747, .T. ) ;
#66381 = ADVANCED_FACE ( 'NONE', ( #59872 ), #51541, .F. ) ;
#66382 = EDGE_CURVE ( 'NONE', #70074, #3369, #71504, .T. ) ;
#66383 = CARTESIAN_POINT ( 'NONE',  ( 96.15314808468750130, -211.9973110713294489, 82.86947916753379673 ) ) ;
#66384 = ORIENTED_EDGE ( 'NONE', *, *, #22404, .T. ) ;
#66385 = CARTESIAN_POINT ( 'NONE',  ( 15.00000000000000000, 5.835314593368470248, -22.81335362449854642 ) ) ;
#66386 = EDGE_LOOP ( 'NONE', ( #17481, #31912, #64403, #51312 ) ) ;
#66387 = CARTESIAN_POINT ( 'NONE',  ( 10.00000000000000000, -33.00180498840060039, 17.80606268964528027 ) ) ;
#66388 = ORIENTED_EDGE ( 'NONE', *, *, #54836, .F. ) ;
#66389 = DIRECTION ( 'NONE',  ( 0.000000000000000000, 0.000000000000000000, 1.000000000000000000 ) ) ;
#66390 = EDGE_CURVE ( 'NONE', #4731, #6415, #61715, .T. ) ;
#66391 = ORIENTED_EDGE ( 'NONE', *, *, #17580, .F. ) ;
#66392 = EDGE_CURVE ( 'NONE', #70028, #28480, #50788, .T. ) ;
#66393 = CARTESIAN_POINT ( 'NONE',  ( 97.30629616937498838, -209.9999999999999716, 79.95906250086714806 ) ) ;
#66394 = FACE_OUTER_BOUND ( 'NONE', #28009, .T. ) ;
#66395 = CARTESIAN_POINT ( 'NONE',  ( 0.000000000000000000, 16.00000000000000000, -2.500000000000000000 ) ) ;
#66396 = CARTESIAN_POINT ( 'NONE',  ( -97.44941226940133561, 89.32071446497062084, 74.93153462041256319 ) ) ;
#66397 = CARTESIAN_POINT ( 'NONE',  ( 96.15314808468748708, 91.99731107132950569, 85.77989583420048803 ) ) ;
#66398 = CARTESIAN_POINT ( 'NONE',  ( -92.35000000000003695, 90.00001154861327279, 83.41187540116096955 ) ) ;
#66399 = CARTESIAN_POINT ( 'NONE',  ( 97.64999999999999147, -209.9999999999999716, 80.79249999999998977 ) ) ;
#66400 = ORIENTED_EDGE ( 'NONE', *, *, #35957, .T. ) ;
#66401 = AXIS2_PLACEMENT_3D ( 'NONE', #42640, #8048, #2083 ) ;
#66402 = VERTEX_POINT ( 'NONE', #28229 ) ;
#66403 = ORIENTED_EDGE ( 'NONE', *, *, #6000, .F. ) ;
#66404 = VERTEX_POINT ( 'NONE', #62853 ) ;
#66405 = CARTESIAN_POINT ( 'NONE',  ( 97.65000000000000568, -211.5299782133523934, 87.08958333333333712 ) ) ;
#66406 = EDGE_CURVE ( 'NONE', #33112, #12032, #9145, .T. ) ;
#66407 = EDGE_CURVE ( 'NONE', #56025, #32525, #66795, .T. ) ;
#66408 = AXIS2_PLACEMENT_3D ( 'NONE', #9316, #71348, #25868 ) ;
#66409 = CARTESIAN_POINT ( 'NONE',  ( -96.15314808468751551, 88.00268892867056536, 83.55739583420049144 ) ) ;
#66410 = CARTESIAN_POINT ( 'NONE',  ( 6.000000000000000000, 21.60688246758586928, 79.10210256391376049 ) ) ;
#66411 = LINE ( 'NONE', #65662, #32993 ) ;
#66412 = DIRECTION ( 'NONE',  ( 1.000000000000000000, -1.047380211910311281E-14, -2.618450529775778123E-14 ) ) ;
#66413 = CARTESIAN_POINT ( 'NONE',  ( 10.00000000000000000, -25.88420570971381807, -27.13269053701123212 ) ) ;
#66414 = ORIENTED_EDGE ( 'NONE', *, *, #68791, .F. ) ;
#66415 = CARTESIAN_POINT ( 'NONE',  ( -93.67499999999998295, -212.2949673200287179, 86.48104166840096241 ) ) ;
#66416 = ORIENTED_EDGE ( 'NONE', *, *, #48450, .F. ) ;
#66417 = DIRECTION ( 'NONE',  ( -1.000000000000000000, -0.000000000000000000, 0.000000000000000000 ) ) ;
#66418 = ORIENTED_EDGE ( 'NONE', *, *, #35465, .T. ) ;
#66419 = CARTESIAN_POINT ( 'NONE',  ( -93.67500000000003979, 87.70503267997129626, 83.94104166840097037 ) ) ;
#66420 = VECTOR ( 'NONE', #31047, 1000.000000000000000 ) ;
#66421 = VERTEX_POINT ( 'NONE', #62473 ) ;
#66422 = CARTESIAN_POINT ( 'NONE',  ( 92.69370383062498320, 91.33154071421968467, 87.20864583420049598 ) ) ;
#66423 = AXIS2_PLACEMENT_3D ( 'NONE', #17348, #5348, #34634 ) ;
#66424 = CARTESIAN_POINT ( 'NONE',  ( 2.500000000000034639, 90.00000000000000000, -310.0000000000000000 ) ) ;
#66425 = LINE ( 'NONE', #18408, #46230 ) ;
#66426 = DIRECTION ( 'NONE',  ( -1.000000000000000000, -0.000000000000000000, 0.000000000000000000 ) ) ;
#66427 = DIRECTION ( 'NONE',  ( 1.000000000000000000, 0.000000000000000000, 0.000000000000000000 ) ) ;
#66428 = PLANE ( 'NONE',  #58894 ) ;
#66429 = VERTEX_POINT ( 'NONE', #45170 ) ;
#66430 = DIRECTION ( 'NONE',  ( -0.000000000000000000, -0.000000000000000000, 1.000000000000000000 ) ) ;
#66431 = LINE ( 'NONE', #72771, #67175 ) ;
#66432 = VERTEX_POINT ( 'NONE', #45555 ) ;
#66433 = ORIENTED_EDGE ( 'NONE', *, *, #9075, .T. ) ;
#66434 = DIRECTION ( 'NONE',  ( 1.000000000000000000, 0.000000000000000000, 0.000000000000000000 ) ) ;
#66435 = LINE ( 'NONE', #25462, #18009 ) ;
#66436 = LINE ( 'NONE', #19806, #66551 ) ;
#66437 = CARTESIAN_POINT ( 'NONE',  ( -97.30629616937495996, -209.9999999999999716, 85.99156250086716113 ) ) ;
#66438 = ORIENTED_EDGE ( 'NONE', *, *, #54477, .T. ) ;
#66439 = FACE_OUTER_BOUND ( 'NONE', #70557, .T. ) ;
#66440 = ORIENTED_EDGE ( 'NONE', *, *, #18565, .F. ) ;
#66441 = DIRECTION ( 'NONE',  ( 0.000000000000000000, -0.07845909572785220165, 0.9969173337331274087 ) ) ;
#66442 = FACE_BOUND ( 'NONE', #11641, .T. ) ;
#66443 = CARTESIAN_POINT ( 'NONE',  ( 93.67500000000001137, -207.7050326799711968, 82.98854166840096980 ) ) ;
#66444 = CARTESIAN_POINT ( 'NONE',  ( 97.30629616937498838, 88.66845928578035796, 77.84239583420047381 ) ) ;
#66445 = DIRECTION ( 'NONE',  ( 0.000000000000000000, 0.000000000000000000, 1.000000000000000000 ) ) ;
#66446 = CARTESIAN_POINT ( 'NONE',  ( 15.00000000000000000, -19.89357724624986545, 12.59942793731086219 ) ) ;
#66447 = DIRECTION ( 'NONE',  ( 0.000000000000000000, 0.000000000000000000, 1.000000000000000000 ) ) ;
#66448 = DIRECTION ( 'NONE',  ( 0.000000000000000000, -0.3090169943749548342, 0.9510565162951510887 ) ) ;
#66449 = DIRECTION ( 'NONE',  ( 0.000000000000000000, 0.000000000000000000, -1.000000000000000000 ) ) ;
#66450 = DIRECTION ( 'NONE',  ( -1.000000000000000000, -0.000000000000000000, -0.000000000000000000 ) ) ;
#66451 = LINE ( 'NONE', #13813, #6014 ) ;
#66452 = PRODUCT_DEFINITION_CONTEXT ( 'detailed design', #8564, 'design' ) ;
#66453 = VECTOR ( 'NONE', #21388, 1000.000000000000000 ) ;
#66454 = CARTESIAN_POINT ( 'NONE',  ( 96.32499999999998863, 87.70503267997126784, 76.95604166840095672 ) ) ;
#66455 = ORIENTED_EDGE ( 'NONE', *, *, #20965, .T. ) ;
#66456 = CARTESIAN_POINT ( 'NONE',  ( -96.15314808468752972, 91.99731107132950569, 83.18697916753382060 ) ) ;
#66457 = FACE_OUTER_BOUND ( 'NONE', #4084, .T. ) ;
#66458 = VECTOR ( 'NONE', #67210, 1000.000000000000114 ) ;
#66459 = EDGE_CURVE ( 'NONE', #35679, #17553, #36736, .T. ) ;
#66460 = ADVANCED_FACE ( 'NONE', ( #10953 ), #68094, .F. ) ;
#66461 = CARTESIAN_POINT ( 'NONE',  ( -3.000000000000000000, 24.81905959214275370, -9.408202855044498492 ) ) ;
#66462 = ORIENTED_EDGE ( 'NONE', *, *, #4294, .F. ) ;
#66463 = AXIS2_PLACEMENT_3D ( 'NONE', #57158, #10528, #62813 ) ;
#66464 = ADVANCED_FACE ( 'NONE', ( #51161 ), #16585, .T. ) ;
#66465 = DIRECTION ( 'NONE',  ( -0.000000000000000000, -0.000000000000000000, 1.000000000000000000 ) ) ;
#66466 = CARTESIAN_POINT ( 'NONE',  ( 10.00000000000000000, 2.663952781846733675, -41.91543099594814947 ) ) ;
#66467 = CARTESIAN_POINT ( 'NONE',  ( -43.60332556124591008, -133.0000000000000000, 102.9091629284897493 ) ) ;
#66468 = ADVANCED_FACE ( 'NONE', ( #38778 ), #33490, .T. ) ;
#66469 = AXIS2_PLACEMENT_3D ( 'NONE', #1392, #646, #24286 ) ;
#66470 = CARTESIAN_POINT ( 'NONE',  ( 93.67499999999999716, 87.70503267997126784, 83.20020833506764291 ) ) ;
#66471 = AXIS2_PLACEMENT_3D ( 'NONE', #49874, #32951, #37876 ) ;
#66472 = CARTESIAN_POINT ( 'NONE',  ( 97.30629616937498838, -211.3315407142195852, 78.00114583420049996 ) ) ;
#66473 = ORIENTED_EDGE ( 'NONE', *, *, #41190, .T. ) ;
#66474 = ORIENTED_EDGE ( 'NONE', *, *, #61283, .F. ) ;
#66475 = EDGE_CURVE ( 'NONE', #9910, #22755, #40389, .T. ) ;
#66476 = ADVANCED_FACE ( 'NONE', ( #21853 ), #40262, .T. ) ;
#66477 = CARTESIAN_POINT ( 'NONE',  ( 0.000000000000000000, 0.000000000000000000, 0.000000000000000000 ) ) ;
#66478 = DIRECTION ( 'NONE',  ( 0.000000000000000000, 0.5224985647159441360, 0.8526401643540951758 ) ) ;
#66479 = CARTESIAN_POINT ( 'NONE',  ( 0.000000000000000000, -40.98264845739755202, 9.188173127307159405 ) ) ;
#66480 = DIRECTION ( 'NONE',  ( -1.000000000000000000, 0.000000000000000000, -0.000000000000000000 ) ) ;
#66481 = CARTESIAN_POINT ( 'NONE',  ( 97.30629616937498838, -210.9303121318039871, 74.84209103131395580 ) ) ;
#66482 = AXIS2_PLACEMENT_3D ( 'NONE', #65124, #7599, #19970 ) ;
#66483 = ORIENTED_EDGE ( 'NONE', *, *, #476, .F. ) ;
#66484 = CYLINDRICAL_SURFACE ( 'NONE', #5914, 32.50000000000000000 ) ;
#66485 = EDGE_LOOP ( 'NONE', ( #26638, #28275, #11616, #34280 ) ) ;
#66486 = VERTEX_POINT ( 'NONE', #11672 ) ;
#66487 = DIRECTION ( 'NONE',  ( 0.000000000000000000, -0.3090169943749349613, -0.9510565162951576390 ) ) ;
#66488 = EDGE_CURVE ( 'NONE', #68607, #52228, #22229, .T. ) ;
#66489 = EDGE_CURVE ( 'NONE', #44617, #33112, #67723, .T. ) ;
#66490 = FILL_AREA_STYLE_COLOUR ( '', #2728 ) ;
#66491 = CARTESIAN_POINT ( 'NONE',  ( 10.00000000000000000, -76.41127070299280888, 12.93880638057289012 ) ) ;
#66492 = ORIENTED_EDGE ( 'NONE', *, *, #31715, .T. ) ;
#66493 = DIRECTION ( 'NONE',  ( 0.000000000000000000, -0.7604059656000227152, -0.6494480483301933171 ) ) ;
#66494 = CARTESIAN_POINT ( 'NONE',  ( 97.64999999999997726, -208.4700217866474645, 79.01979166840095559 ) ) ;
#66495 = CARTESIAN_POINT ( 'NONE',  ( 96.32499999999998863, 87.70503267997126784, 86.40166666666667084 ) ) ;
#66496 = VERTEX_POINT ( 'NONE', #56823 ) ;
#66497 = CARTESIAN_POINT ( 'NONE',  ( 20.85212586905262100, -130.9402397935870965, 5.500000000000000000 ) ) ;
#66498 = CARTESIAN_POINT ( 'NONE',  ( 96.32499999999997442, 92.29496732002878900, 80.97770833506763211 ) ) ;
#66499 = CIRCLE ( 'NONE', #17279, 82.00000000000000000 ) ;
#66500 = ORIENTED_EDGE ( 'NONE', *, *, #2438, .T. ) ;
#66501 = DIRECTION ( 'NONE',  ( 0.000000000000000000, 0.000000000000000000, 1.000000000000000000 ) ) ;
#66502 = CARTESIAN_POINT ( 'NONE',  ( -95.00000000000002842, 92.66308142843932671, 85.83281250086717762 ) ) ;
#66503 = CARTESIAN_POINT ( 'NONE',  ( 94.99999999999998579, 92.66308142843935514, 82.49906250086714010 ) ) ;
#66504 = ORIENTED_EDGE ( 'NONE', *, *, #24141, .T. ) ;
#66505 = AXIS2_PLACEMENT_3D ( 'NONE', #38430, #4610, #27513 ) ;
#66506 = DIRECTION ( 'NONE',  ( 0.000000000000000000, 0.000000000000000000, 1.000000000000000000 ) ) ;
#66507 = ORIENTED_EDGE ( 'NONE', *, *, #45923, .T. ) ;
#66508 = DIRECTION ( 'NONE',  ( 1.000000000000000000, 0.000000000000000000, 0.000000000000000000 ) ) ;
#66509 = EDGE_LOOP ( 'NONE', ( #28008, #55572 ) ) ;
#66510 = CIRCLE ( 'NONE', #40109, 15.70000000000000284 ) ;
#66511 = EDGE_LOOP ( 'NONE', ( #72224, #65966, #46652, #39097 ) ) ;
#66512 = ORIENTED_EDGE ( 'NONE', *, *, #23037, .T. ) ;
#66513 = DIRECTION ( 'NONE',  ( -0.000000000000000000, -0.000000000000000000, -1.000000000000000000 ) ) ;
#66514 = VERTEX_POINT ( 'NONE', #27861 ) ;
#66515 = DIRECTION ( 'NONE',  ( 0.000000000000000000, -0.7604059656000369261, 0.6494480483301766638 ) ) ;
#66516 = VECTOR ( 'NONE', #8966, 1000.000000000000000 ) ;
#66517 = CARTESIAN_POINT ( 'NONE',  ( 92.34999999999999432, 91.52997821335252127, 88.75645833506762017 ) ) ;
#66518 = ORIENTED_EDGE ( 'NONE', *, *, #57404, .T. ) ;
#66519 = CYLINDRICAL_SURFACE ( 'NONE', #38380, 2.649999999999985700 ) ;
#66520 = CARTESIAN_POINT ( 'NONE',  ( -92.69370383062498320, -211.3315407142195852, 81.01739583420048518 ) ) ;
#66521 = ORIENTED_EDGE ( 'NONE', *, *, #10625, .F. ) ;
#66522 = VECTOR ( 'NONE', #57307, 1000.000000000000000 ) ;
#66523 = CARTESIAN_POINT ( 'NONE',  ( 11.99999999999999822, 0.000000000000000000, 0.000000000000000000 ) ) ;
#66524 = LINE ( 'NONE', #10479, #15245 ) ;
#66525 = CARTESIAN_POINT ( 'NONE',  ( 11.99999999999999822, 21.60688246758696351, -79.10210256391344785 ) ) ;
#66526 = DIRECTION ( 'NONE',  ( 0.000000000000000000, 0.000000000000000000, 1.000000000000000000 ) ) ;
#66527 = LINE ( 'NONE', #37222, #25944 ) ;
#66528 = AXIS2_PLACEMENT_3D ( 'NONE', #46849, #41204, #12615 ) ;
#66529 = AXIS2_PLACEMENT_3D ( 'NONE', #23363, #45934, #28988 ) ;
#66530 = CYLINDRICAL_SURFACE ( 'NONE', #43360, 2.650000000000540812 ) ;
#66531 = CARTESIAN_POINT ( 'NONE',  ( 97.30629616937498838, 88.66845928578035796, 88.00239583420047040 ) ) ;
#66532 = EDGE_CURVE ( 'NONE', #57513, #47511, #50419, .T. ) ;
#66533 = CARTESIAN_POINT ( 'NONE',  ( 10.00000000000000000, 55.38113227695858143, -54.21277698773617715 ) ) ;
#66534 = DIRECTION ( 'NONE',  ( 0.000000000000000000, 0.3090169943749482839, -0.9510565162951533091 ) ) ;
#66535 = CARTESIAN_POINT ( 'NONE',  ( 96.37670920697048871, -212.2908000246596316, 75.00000000000000000 ) ) ;
#66536 = EDGE_CURVE ( 'NONE', #35321, #44003, #29536, .T. ) ;
#66537 = CARTESIAN_POINT ( 'NONE',  ( 10.00000000000000000, 0.000000000000000000, 0.000000000000000000 ) ) ;
#66538 = FACE_OUTER_BOUND ( 'NONE', #9426, .T. ) ;
#66539 = CYLINDRICAL_SURFACE ( 'NONE', #31457, 77.49899999999999523 ) ;
#66540 = EDGE_CURVE ( 'NONE', #32702, #2275, #36096, .T. ) ;
#66541 = LINE ( 'NONE', #20667, #42751 ) ;
#66542 = DIRECTION ( 'NONE',  ( -1.000000000000000000, -0.000000000000000000, 0.000000000000000000 ) ) ;
#66543 = AXIS2_PLACEMENT_3D ( 'NONE', #50864, #50105, #9901 ) ;
#66544 = EDGE_CURVE ( 'NONE', #36499, #71482, #46355, .T. ) ;
#66545 = CARTESIAN_POINT ( 'NONE',  ( 0.000000000000000000, -0.8828120875903202602, 37.48860685352291000 ) ) ;
#66546 = FACE_OUTER_BOUND ( 'NONE', #51782, .T. ) ;
#66547 = ADVANCED_FACE ( 'NONE', ( #6072 ), #13161, .T. ) ;
#66548 = DIRECTION ( 'NONE',  ( 0.000000000000000000, -0.1564344650402381132, 0.9876883405951365491 ) ) ;
#66549 = CARTESIAN_POINT ( 'NONE',  ( -92.34999999999999432, -211.5299782133524502, 88.35958333333333314 ) ) ;
#66550 = DIRECTION ( 'NONE',  ( -0.000000000000000000, -0.000000000000000000, -1.000000000000000000 ) ) ;
#66551 = VECTOR ( 'NONE', #26187, 1000.000000000000000 ) ;
#66552 = EDGE_CURVE ( 'NONE', #23772, #55755, #13914, .T. ) ;
#66553 = CARTESIAN_POINT ( 'NONE',  ( 15.00000000000000000, -23.29833615347109088, -3.418703333116486665 ) ) ;
#66554 = DIRECTION ( 'NONE',  ( -1.000000000000000000, -0.000000000000000000, -0.000000000000000000 ) ) ;
#66555 = CARTESIAN_POINT ( 'NONE',  ( 97.64999999999449187, -210.0000054026048701, 81.50687481489494246 ) ) ;
#66556 = DIRECTION ( 'NONE',  ( -1.000000000000000000, -0.000000000000000000, 0.000000000000000000 ) ) ;
#66557 = CIRCLE ( 'NONE', #57016, 31.99999999999999289 ) ;
#66558 = VERTEX_POINT ( 'NONE', #41732 ) ;
#66559 = ORIENTED_EDGE ( 'NONE', *, *, #66798, .F. ) ;
#66560 = EDGE_CURVE ( 'NONE', #63739, #25323, #27117, .T. ) ;
#66561 = DIRECTION ( 'NONE',  ( 0.000000000000000000, -0.3090169943749549453, 0.9510565162951511997 ) ) ;
#66562 = EDGE_CURVE ( 'NONE', #17707, #62140, #16349, .T. ) ;
#66563 = CARTESIAN_POINT ( 'NONE',  ( 11.99999999999999822, 0.000000000000000000, 0.000000000000000000 ) ) ;
#66564 = ORIENTED_EDGE ( 'NONE', *, *, #47311, .T. ) ;
#66565 = AXIS2_PLACEMENT_3D ( 'NONE', #32626, #15335, #31887 ) ;
#66566 = CARTESIAN_POINT ( 'NONE',  ( 92.69370383062501162, -209.9999999999999716, 80.75281250086715090 ) ) ;
#66567 = CARTESIAN_POINT ( 'NONE',  ( 96.15314808468750130, -211.9973110713294489, 83.66322916753382799 ) ) ;
#66568 = AXIS2_PLACEMENT_3D ( 'NONE', #31678, #48245, #32040 ) ;
#66569 = ORIENTED_EDGE ( 'NONE', *, *, #5057, .T. ) ;
#66570 = CARTESIAN_POINT ( 'NONE',  ( 97.30629616937498838, -209.9999999999999716, 87.57906250086715261 ) ) ;
#66571 = ORIENTED_EDGE ( 'NONE', *, *, #41400, .F. ) ;
#66572 = DIRECTION ( 'NONE',  ( -1.000000000000000000, 0.000000000000000000, 0.000000000000000000 ) ) ;
#66573 = EDGE_LOOP ( 'NONE', ( #56319, #19124, #71839, #37829 ) ) ;
#66574 = AXIS2_PLACEMENT_3D ( 'NONE', #17628, #22538, #11249 ) ;
#66575 = CARTESIAN_POINT ( 'NONE',  ( -95.00000000000002842, 87.33691857156074434, 77.89531250086714920 ) ) ;
#66576 = VERTEX_POINT ( 'NONE', #7531 ) ;
#66577 = ORIENTED_EDGE ( 'NONE', *, *, #69005, .T. ) ;
#66578 = CYLINDRICAL_SURFACE ( 'NONE', #25670, 2.649999999999985700 ) ;
#66579 = AXIS2_PLACEMENT_3D ( 'NONE', #65437, #42136, #30092 ) ;
#66580 = EDGE_LOOP ( 'NONE', ( #69537, #1178, #475, #74149 ) ) ;
#66581 = CARTESIAN_POINT ( 'NONE',  ( 10.00000000000000000, 41.81611651403867569, -3.925862922255714871 ) ) ;
#66582 = DIRECTION ( 'NONE',  ( -1.000000000000000000, 0.000000000000000000, 0.000000000000000000 ) ) ;
#66583 = ORIENTED_EDGE ( 'NONE', *, *, #37863, .F. ) ;
#66584 = FACE_OUTER_BOUND ( 'NONE', #67033, .T. ) ;
#66585 = AXIS2_PLACEMENT_3D ( 'NONE', #50371, #45500, #21805 ) ;
#66586 = ORIENTED_EDGE ( 'NONE', *, *, #10771, .F. ) ;
#66587 =( BOUNDED_CURVE ( )  B_SPLINE_CURVE ( 2, ( #8095, #25013, #47217, #47955, #18995, #41949, #2863, #64887, #65622 ),
 .UNSPECIFIED., .F., .F. ) 
 B_SPLINE_CURVE_WITH_KNOTS ( ( 3, 2, 2, 2, 3 ),
 ( 0.7620226289501886852, 0.7620226784190389235, 0.7690784439599557265, 0.7761342095008724185, 0.7831899741104385582 ),
 .UNSPECIFIED. ) 
 CURVE ( )  GEOMETRIC_REPRESENTATION_ITEM ( )  RATIONAL_B_SPLINE_CURVE ( ( 0.9999981213880371200, 0.9999990606874329391, 1.000000000000000000, 0.8660254037844387076, 1.000000000000000000, 0.8660254037844387076, 1.000000000000000000, 0.8660254037844387076, 1.000000000000000000 ) ) 
 REPRESENTATION_ITEM ( '' )  );
#66588 = CARTESIAN_POINT ( 'NONE',  ( 96.32499999999998863, -212.2949673200287179, 81.40104166840096411 ) ) ;
#66589 = VERTEX_POINT ( 'NONE', #51909 ) ;
#66590 = VERTEX_POINT ( 'NONE', #6786 ) ;
#66591 = ORIENTED_EDGE ( 'NONE', *, *, #28496, .T. ) ;
#66592 = CARTESIAN_POINT ( 'NONE',  ( 96.66078690017491226, -211.6002465100980032, 74.64190636928354650 ) ) ;
#66593 = LINE ( 'NONE', #26359, #63108 ) ;
#66594 = ORIENTED_EDGE ( 'NONE', *, *, #52266, .F. ) ;
#66595 = ORIENTED_EDGE ( 'NONE', *, *, #6248, .F. ) ;
#66596 = ORIENTED_EDGE ( 'NONE', *, *, #62343, .F. ) ;
#66597 = LINE ( 'NONE', #26364, #8468 ) ;
#66598 = DIRECTION ( 'NONE',  ( -1.000000000000000000, -0.000000000000000000, -0.000000000000000000 ) ) ;
#66599 = CARTESIAN_POINT ( 'NONE',  ( -97.30629616937501680, 88.66845928578038638, 80.32947916753381890 ) ) ;
#66600 = EDGE_CURVE ( 'NONE', #4011, #44188, #55953, .T. ) ;
#66601 = EDGE_LOOP ( 'NONE', ( #51043, #20844, #56425, #19507 ) ) ;
#66602 = CARTESIAN_POINT ( 'NONE',  ( 94.99999999999998579, 92.66308142843935514, 78.05406250086714692 ) ) ;
#66603 = ORIENTED_EDGE ( 'NONE', *, *, #70319, .T. ) ;
#66604 = LINE ( 'NONE', #15084, #2360 ) ;
#66605 = CARTESIAN_POINT ( 'NONE',  ( -92.69370383062498320, -209.9999999999999716, 89.32531250086714181 ) ) ;
#66606 = CARTESIAN_POINT ( 'NONE',  ( -7.400000000000003908, -1.056673655988042765E-14, -5.892267102755452808E-15 ) ) ;
#66607 = CARTESIAN_POINT ( 'NONE',  ( 0.000000000000000000, 0.000000000000000000, 77.49899999999999523 ) ) ;
#66608 = CARTESIAN_POINT ( 'NONE',  ( 12.00000000000000000, 14.60985201121729737, 18.46759930825687235 ) ) ;
#66609 = CARTESIAN_POINT ( 'NONE',  ( -96.15314808468747287, -208.0026889286704943, 80.64697916753381435 ) ) ;
#66610 = DIRECTION ( 'NONE',  ( 0.000000000000000000, 0.000000000000000000, -1.000000000000000000 ) ) ;
#66611 = DIRECTION ( 'NONE',  ( -1.000000000000000000, 0.000000000000000000, -0.000000000000000000 ) ) ;
#66612 = DIRECTION ( 'NONE',  ( 0.000000000000000000, 0.5224985647159441360, 0.8526401643540951758 ) ) ;
#66613 = ORIENTED_EDGE ( 'NONE', *, *, #40085, .F. ) ;
#66614 = CIRCLE ( 'NONE', #24641, 31.99999999999999289 ) ;
#66615 = ORIENTED_EDGE ( 'NONE', *, *, #1654, .T. ) ;
#66616 = CARTESIAN_POINT ( 'NONE',  ( -14.87942725330654348, -141.9795960975983178, -5.500000000000000000 ) ) ;
#66617 = EDGE_CURVE ( 'NONE', #15277, #55743, #18792, .T. ) ;
#66618 = CARTESIAN_POINT ( 'NONE',  ( 6.000000000000000000, -40.65526001592564853, -71.21200624218839437 ) ) ;
#66619 = EDGE_CURVE ( 'NONE', #28408, #54047, #69930, .T. ) ;
#66620 = DIRECTION ( 'NONE',  ( 1.000000000000000000, 0.000000000000000000, 0.000000000000000000 ) ) ;
#66621 = CARTESIAN_POINT ( 'NONE',  ( -95.00000000000002842, 87.33691857156074434, 85.35656250086714181 ) ) ;
#66622 = FACE_OUTER_BOUND ( 'NONE', #20640, .T. ) ;
#66623 = DIRECTION ( 'NONE',  ( -1.000000000000000000, 0.000000000000000000, -0.000000000000000000 ) ) ;
#66624 = AXIS2_PLACEMENT_3D ( 'NONE', #37978, #21405, #67666 ) ;
#66625 = ORIENTED_EDGE ( 'NONE', *, *, #60609, .T. ) ;
#66626 = CIRCLE ( 'NONE', #45009, 37.49900000000000233 ) ;
#66627 = CARTESIAN_POINT ( 'NONE',  ( 11.99999999999999822, 26.01480285779837232, 70.53064760720326376 ) ) ;
#66628 = EDGE_CURVE ( 'NONE', #28475, #31156, #23707, .T. ) ;
#66629 = EDGE_CURVE ( 'NONE', #31252, #72829, #23546, .T. ) ;
#66631 = CARTESIAN_POINT ( 'NONE',  ( 1.459549131277868561, -120.3460004817713411, 2.500000000000000000 ) ) ;
#66630 = AXIS2_PLACEMENT_3D ( 'NONE', #65176, #41489, #47868 ) ;
#66632 = CYLINDRICAL_SURFACE ( 'NONE', #44163, 82.00000000000000000 ) ;
#66633 = FACE_OUTER_BOUND ( 'NONE', #63757, .T. ) ;
#66634 = FACE_OUTER_BOUND ( 'NONE', #54314, .T. ) ;
#66635 = CARTESIAN_POINT ( 'NONE',  ( -97.64999999954994792, 89.99996890530464100, 88.81037122970319331 ) ) ;
#66636 = CARTESIAN_POINT ( 'NONE',  ( -96.15314808468745866, -211.9973110713294489, 82.28739583420048120 ) ) ;
#66637 = CARTESIAN_POINT ( 'NONE',  ( -97.64999999999996305, -209.9999999999999716, 86.90437500173429441 ) ) ;
#66638 = ADVANCED_FACE ( 'NONE', ( #41376 ), #24448, .T. ) ;
#66639 = DIRECTION ( 'NONE',  ( -1.000000000000000000, 0.000000000000000000, 0.000000000000000000 ) ) ;
#66640 = AXIS2_PLACEMENT_3D ( 'NONE', #11847, #50596, #67525 ) ;
#66641 = CARTESIAN_POINT ( 'NONE',  ( -10.00000000000000000, 0.000000000000000000, 0.000000000000000000 ) ) ;
#66642 = CARTESIAN_POINT ( 'NONE',  ( 10.00000000000000000, -21.40280677340345505, -36.13751322684441902 ) ) ;
#66643 = ORIENTED_EDGE ( 'NONE', *, *, #52044, .T. ) ;
#66644 = DIRECTION ( 'NONE',  ( 0.000000000000000000, 0.1045284632676448111, 0.9945218953682742891 ) ) ;
#66645 = DIRECTION ( 'NONE',  ( -1.000000000000000000, 0.000000000000000000, 0.000000000000000000 ) ) ;
#66646 = CARTESIAN_POINT ( 'NONE',  ( 97.64999999999999147, -209.9999999999999716, 79.52249999999999375 ) ) ;
#66647 = AXIS2_PLACEMENT_3D ( 'NONE', #63774, #40091, #5892 ) ;
#66648 = DIRECTION ( 'NONE',  ( 0.000000000000000000, 0.000000000000000000, -1.000000000000000000 ) ) ;
#66649 = ORIENTED_EDGE ( 'NONE', *, *, #20041, .F. ) ;
#66650 = EDGE_CURVE ( 'NONE', #7440, #46823, #15152, .T. ) ;
#66651 = CARTESIAN_POINT ( 'NONE',  ( 96.32499999999997442, 92.29496732002878900, 78.35833333333333428 ) ) ;
#66652 = FACE_OUTER_BOUND ( 'NONE', #15153, .T. ) ;
#66653 = ORIENTED_EDGE ( 'NONE', *, *, #21513, .F. ) ;
#66654 = FACE_OUTER_BOUND ( 'NONE', #7996, .T. ) ;
#66655 = CYLINDRICAL_SURFACE ( 'NONE', #37539, 31.99999999999998579 ) ;
#66656 = EDGE_CURVE ( 'NONE', #13671, #31995, #30080, .T. ) ;
#66657 = ORIENTED_EDGE ( 'NONE', *, *, #21907, .F. ) ;
#66658 = DIRECTION ( 'NONE',  ( -3.061616997868382648E-16, -1.000000000000000000, 0.000000000000000000 ) ) ;
#66659 = ORIENTED_EDGE ( 'NONE', *, *, #65149, .T. ) ;
#66660 = CARTESIAN_POINT ( 'NONE',  ( -13.05994868825747446, -139.5943292883446532, 5.500000000000000000 ) ) ;
#66661 = ORIENTED_EDGE ( 'NONE', *, *, #28342, .F. ) ;
#66662 = ORIENTED_EDGE ( 'NONE', *, *, #64171, .F. ) ;
#66663 = ORIENTED_EDGE ( 'NONE', *, *, #25650, .T. ) ;
#66664 = ORIENTED_EDGE ( 'NONE', *, *, #51288, .F. ) ;
#66665 = CARTESIAN_POINT ( 'NONE',  ( 11.99999999999999822, 2.956366410620650420, 75.11725578898469280 ) ) ;
#66666 = ORIENTED_EDGE ( 'NONE', *, *, #45798, .F. ) ;
#66667 = VERTEX_POINT ( 'NONE', #1929 ) ;
#66668 = CARTESIAN_POINT ( 'NONE',  ( 96.15314808468748708, 91.99731107132950569, 76.88989583420048746 ) ) ;
#66669 = AXIS2_PLACEMENT_3D ( 'NONE', #3887, #38453, #25037 ) ;
#66670 = LINE ( 'NONE', #61023, #40 ) ;
#66672 = CARTESIAN_POINT ( 'NONE',  ( 10.00000000000000000, 75.11764819372149304, -2.946379043146603482 ) ) ;
#66671 = VECTOR ( 'NONE', #7512, 999.9999999999998863 ) ;
#66673 = VERTEX_POINT ( 'NONE', #47743 ) ;
#66674 = ORIENTED_EDGE ( 'NONE', *, *, #18832, .T. ) ;
#66675 = ORIENTED_EDGE ( 'NONE', *, *, #57804, .T. ) ;
#66676 = CARTESIAN_POINT ( 'NONE',  ( 97.30629616937498838, 91.33154071421968467, 86.83822916753381094 ) ) ;
#66677 = ORIENTED_EDGE ( 'NONE', *, *, #49611, .T. ) ;
#66678 = AXIS2_PLACEMENT_3D ( 'NONE', #21314, #4430, #20956 ) ;
#66679 = CARTESIAN_POINT ( 'NONE',  ( 92.35000000000002274, -208.4700217866474645, 74.78645833506763552 ) ) ;
#66680 = PRODUCT_CONTEXT ( 'NONE', #9969, 'mechanical' ) ;
#66681 = CYLINDRICAL_SURFACE ( 'NONE', #595, 77.49899999999999523 ) ;
#66682 = DIRECTION ( 'NONE',  ( -1.000000000000000000, 0.000000000000000000, 0.000000000000000000 ) ) ;
#66683 = FACE_OUTER_BOUND ( 'NONE', #42443, .T. ) ;
#66684 = CARTESIAN_POINT ( 'NONE',  ( 0.000000000000000000, 22.74946021919133088, 29.81001611431016229 ) ) ;
#66685 = CIRCLE ( 'NONE', #7854, 82.00000000000000000 ) ;
#66686 = DIRECTION ( 'NONE',  ( 0.000000000000000000, 0.000000000000000000, -1.000000000000000000 ) ) ;
#66687 = DIRECTION ( 'NONE',  ( 1.000000000000000000, 0.000000000000000000, 0.000000000000000000 ) ) ;
#66688 = CARTESIAN_POINT ( 'NONE',  ( -94.99999999999997158, -206.9400435732949575, 75.31562500173430408 ) ) ;
#66689 = CARTESIAN_POINT ( 'NONE',  ( -97.30629616937501680, 90.00000000000004263, 87.89656250086714806 ) ) ;
#66690 = VERTEX_POINT ( 'NONE', #46643 ) ;
#66692 = CARTESIAN_POINT ( 'NONE',  ( -93.84685191531252713, 88.00268892867056536, 86.67947916753381321 ) ) ;
#66691 = CARTESIAN_POINT ( 'NONE',  ( 97.30629616937498838, 88.66845928578037217, 87.36739583420047950 ) ) ;
#66693 = VERTEX_POINT ( 'NONE', #12785 ) ;
#66694 = CARTESIAN_POINT ( 'NONE',  ( 97.64999999999999147, -210.0000001167898631, 84.68187499741277691 ) ) ;
#66695 = CARTESIAN_POINT ( 'NONE',  ( 92.34999999999999432, 90.00000000000002842, 82.37999999999999545 ) ) ;
#66696 = DIRECTION ( 'NONE',  ( 0.000000000000000000, 0.000000000000000000, 1.000000000000000000 ) ) ;
#66697 = CARTESIAN_POINT ( 'NONE',  ( 93.67499999999998295, 92.29496732002878900, 82.35354166840096468 ) ) ;
#66698 = AXIS2_PLACEMENT_3D ( 'NONE', #31732, #9178, #32470 ) ;
#66699 = CARTESIAN_POINT ( 'NONE',  ( -10.00000000000000000, 0.000000000000000000, 0.000000000000000000 ) ) ;
#66700 = DIRECTION ( 'NONE',  ( 1.000000000000000000, 0.000000000000000000, 0.000000000000000000 ) ) ;
#66701 = DIRECTION ( 'NONE',  ( 0.000000000000000000, -8.881784197001252323E-16, -1.000000000000000000 ) ) ;
#66702 = DIRECTION ( 'NONE',  ( 0.000000000000000000, 0.000000000000000000, 1.000000000000000000 ) ) ;
#66703 = VERTEX_POINT ( 'NONE', #12055 ) ;
#66704 = EDGE_CURVE ( 'NONE', #44128, #9413, #70657, .T. ) ;
#66705 = AXIS2_PLACEMENT_3D ( 'NONE', #65185, #1331, #24578 ) ;
#66706 = ORIENTED_EDGE ( 'NONE', *, *, #4707, .T. ) ;
#66707 = EDGE_CURVE ( 'NONE', #72132, #58797, #10332, .T. ) ;
#66708 = CARTESIAN_POINT ( 'NONE',  ( -97.65000000000001990, 88.47002178664754979, 79.89291666666666458 ) ) ;
#66709 = ADVANCED_FACE ( 'NONE', ( #1562 ), #47386, .T. ) ;
#66710 = FACE_OUTER_BOUND ( 'NONE', #17665, .T. ) ;
#66711 = CARTESIAN_POINT ( 'NONE',  ( 95.00000000000000000, -206.9400435732949575, 75.87125000000000341 ) ) ;
#66712 = CARTESIAN_POINT ( 'NONE',  ( 95.00000000000000000, -206.9400435732949575, 88.01562500173432113 ) ) ;
#66713 = CARTESIAN_POINT ( 'NONE',  ( -100.0000000000000142, 95.00000000000002842, 90.00000000000000000 ) ) ;
#66714 = DIRECTION ( 'NONE',  ( -1.000000000000000000, 0.000000000000000000, 0.000000000000000000 ) ) ;
#66715 = CARTESIAN_POINT ( 'NONE',  ( 92.35000000000002274, 88.47002178664752137, 84.33791666666667197 ) ) ;
#66716 = ORIENTED_EDGE ( 'NONE', *, *, #47975, .T. ) ;
#66717 = CARTESIAN_POINT ( 'NONE',  ( -95.00000000000002842, 92.66308142843932671, 83.13406250086714522 ) ) ;
#66718 = EDGE_CURVE ( 'NONE', #61765, #48451, #31189, .T. ) ;
#66719 = CYLINDRICAL_SURFACE ( 'NONE', #18739, 15.70000000000327312 ) ;
#66720 = DIRECTION ( 'NONE',  ( 0.000000000000000000, 0.5224985647159500202, -0.8526401643540915121 ) ) ;
#66721 = DIRECTION ( 'NONE',  ( -1.000000000000000000, 0.000000000000000000, -0.000000000000000000 ) ) ;
#66722 = CARTESIAN_POINT ( 'NONE',  ( -3.000000000000000000, -18.13022148937243472, -15.02647892043568767 ) ) ;
#66723 = FACE_OUTER_BOUND ( 'NONE', #3263, .T. ) ;
#66724 = DIRECTION ( 'NONE',  ( -1.000000000000000000, 0.000000000000000000, 0.000000000000000000 ) ) ;
#66725 = CARTESIAN_POINT ( 'NONE',  ( -97.65000000000001990, 90.00000000000004263, 90.00000000000000000 ) ) ;
#66726 = DIRECTION ( 'NONE',  ( 0.000000000000000000, 0.000000000000000000, 1.000000000000000000 ) ) ;
#66727 = EDGE_CURVE ( 'NONE', #16859, #27537, #19928, .T. ) ;
#66728 = EDGE_CURVE ( 'NONE', #55130, #56682, #66527, .T. ) ;
#66729 = CARTESIAN_POINT ( 'NONE',  ( 96.15314808468748708, 88.00268892867053694, 81.12322916753382174 ) ) ;
#66730 = ADVANCED_FACE ( 'NONE', ( #37587, #25193 ), #26658, .T. ) ;
#66731 = CARTESIAN_POINT ( 'NONE',  ( -97.30629616937497417, -211.3315407142195852, 82.23447916753383424 ) ) ;
#66732 = CARTESIAN_POINT ( 'NONE',  ( 0.000000000000000000, -63.18004540532994184, -44.88180994100446952 ) ) ;
#66733 = EDGE_LOOP ( 'NONE', ( #20168, #325, #21891, #16074 ) ) ;
#66734 = LINE ( 'NONE', #31765, #11286 ) ;
#66735 = CARTESIAN_POINT ( 'NONE',  ( -97.64999999999996305, -209.9999999999999716, 78.57000000000000739 ) ) ;
#66736 = DIRECTION ( 'NONE',  ( 1.000000000000000000, 0.000000000000000000, 0.000000000000000000 ) ) ;
#66737 = EDGE_CURVE ( 'NONE', #10962, #69749, #9004, .T. ) ;
#66738 = VECTOR ( 'NONE', #11106, 1000.000000000000000 ) ;
#66739 = CIRCLE ( 'NONE', #27108, 12.49999999999999645 ) ;
#66740 = CIRCLE ( 'NONE', #51165, 31.99999999999999645 ) ;
#66741 = CARTESIAN_POINT ( 'NONE',  ( -97.30629616937501680, 91.33154071421968467, 78.31864583420050963 ) ) ;
#66742 = CARTESIAN_POINT ( 'NONE',  ( 97.30629616937498838, -208.6684592857803011, 83.66322916753379957 ) ) ;
#66743 = ORIENTED_EDGE ( 'NONE', *, *, #30529, .T. ) ;
#66744 = EDGE_CURVE ( 'NONE', #29501, #65482, #12736, .T. ) ;
#66745 = CARTESIAN_POINT ( 'NONE',  ( 0.000000000000000000, -20.55727247249748046, 16.78983467731285018 ) ) ;
#66746 = EDGE_LOOP ( 'NONE', ( #22184, #63971, #51824, #37019 ) ) ;
#66747 = CARTESIAN_POINT ( 'NONE',  ( -3.000000000000002665, 2.353404862842836044E-15, 19.21700905503013601 ) ) ;
#66748 = ORIENTED_EDGE ( 'NONE', *, *, #21222, .T. ) ;
#66749 = AXIS2_PLACEMENT_3D ( 'NONE', #45953, #62887, #46311 ) ;
#66750 = ORIENTED_EDGE ( 'NONE', *, *, #35543, .F. ) ;
#66751 = ORIENTED_EDGE ( 'NONE', *, *, #37964, .F. ) ;
#66752 = CARTESIAN_POINT ( 'NONE',  ( 97.30629616937498838, -208.6684592857803295, 78.74197916753381321 ) ) ;
#66753 = DIRECTION ( 'NONE',  ( 0.1850432970638656582, -0.9827303690289285187, 0.000000000000000000 ) ) ;
#66754 = CARTESIAN_POINT ( 'NONE',  ( -26.53422223201112828, -120.6595836127786043, -2.500000000000000444 ) ) ;
#66755 = DIRECTION ( 'NONE',  ( 1.000000000000000000, 0.000000000000000000, 0.000000000000000000 ) ) ;
#66756 = CARTESIAN_POINT ( 'NONE',  ( 92.69370383062498320, 88.66845928578037217, 85.40947916753380298 ) ) ;
#66757 = CARTESIAN_POINT ( 'NONE',  ( 95.73180504966225612, 87.36255141571184879, 75.02735117824596500 ) ) ;
#66758 = CARTESIAN_POINT ( 'NONE',  ( 93.67500000000001137, -212.2949673200287179, 81.85083333333332689 ) ) ;
#66759 = ORIENTED_EDGE ( 'NONE', *, *, #54841, .T. ) ;
#66760 = ORIENTED_EDGE ( 'NONE', *, *, #11879, .T. ) ;
#66761 = ORIENTED_EDGE ( 'NONE', *, *, #67204, .T. ) ;
#66762 = EDGE_LOOP ( 'NONE', ( #29651, #63853, #31453, #61299 ) ) ;
#66763 = CARTESIAN_POINT ( 'NONE',  ( 0.000000000000000000, -74.65491531819111515, 23.16904090965678975 ) ) ;
#66764 = CARTESIAN_POINT ( 'NONE',  ( -97.64999999999996305, -209.9999999999999716, 85.55499999999999261 ) ) ;
#66765 = DIRECTION ( 'NONE',  ( 0.000000000000000000, 0.000000000000000000, -1.000000000000000000 ) ) ;
#66766 = FACE_OUTER_BOUND ( 'NONE', #66803, .T. ) ;
#66767 = DIRECTION ( 'NONE',  ( 0.000000000000000000, 0.9510565162951523099, 0.3090169943749516146 ) ) ;
#66768 = CARTESIAN_POINT ( 'NONE',  ( 11.99999999999999822, -16.65972982744991171, 80.28980883073751329 ) ) ;
#66769 = ORIENTED_EDGE ( 'NONE', *, *, #35882, .F. ) ;
#66770 = CARTESIAN_POINT ( 'NONE',  ( -93.67499999999998295, -207.7050326799711968, 86.69270833506763552 ) ) ;
#66771 = EDGE_LOOP ( 'NONE', ( #65554, #12274, #72640, #51026 ) ) ;
#66772 = CARTESIAN_POINT ( 'NONE',  ( 0.000000000000000000, 16.65560815589464028, -38.55633173626993226 ) ) ;
#66773 = ORIENTED_EDGE ( 'NONE', *, *, #67729, .F. ) ;
#66774 = CARTESIAN_POINT ( 'NONE',  ( -97.65000000000001990, 88.47002178664754979, 83.78229166840095843 ) ) ;
#66775 = ORIENTED_EDGE ( 'NONE', *, *, #20697, .T. ) ;
#66776 = CARTESIAN_POINT ( 'NONE',  ( 94.99999999999998579, 87.33691857156068750, 82.34031250086714238 ) ) ;
#66777 = VECTOR ( 'NONE', #69656, 1000.000000000000000 ) ;
#66778 = LINE ( 'NONE', #19794, #14197 ) ;
#66779 = DIRECTION ( 'NONE',  ( 1.000000000000000000, -7.331661483372147883E-15, -2.592266024478009537E-14 ) ) ;
#66780 = EDGE_CURVE ( 'NONE', #64543, #24878, #306, .T. ) ;
#66781 = CARTESIAN_POINT ( 'NONE',  ( 1.250000000000000000, -12.36245420541525597, -1.199999999999999956 ) ) ;
#66782 = DIRECTION ( 'NONE',  ( -1.000000000000000000, -0.000000000000000000, 0.000000000000000000 ) ) ;
#66783 = ORIENTED_EDGE ( 'NONE', *, *, #1042, .F. ) ;
#66784 = DIRECTION ( 'NONE',  ( 0.000000000000000000, 0.000000000000000000, 1.000000000000000000 ) ) ;
#66785 = CYLINDRICAL_SURFACE ( 'NONE', #68376, 77.49899999999999523 ) ;
#66786 = ORIENTED_EDGE ( 'NONE', *, *, #29457, .F. ) ;
#66787 = EDGE_CURVE ( 'NONE', #37478, #12484, #73976, .T. ) ;
#66788 = CIRCLE ( 'NONE', #3223, 77.49899999999999523 ) ;
#66789 = ORIENTED_EDGE ( 'NONE', *, *, #48207, .F. ) ;
#66790 = CIRCLE ( 'NONE', #27154, 77.49899999999999523 ) ;
#66791 = EDGE_CURVE ( 'NONE', #5740, #71004, #25551, .T. ) ;
#66792 = PRODUCT ( 'output shaft', 'output shaft', '', ( #35058 ) ) ;
#66793 = DIRECTION ( 'NONE',  ( 0.000000000000000000, 0.000000000000000000, 1.000000000000000000 ) ) ;
#66794 = VECTOR ( 'NONE', #7171, 1000.000000000000000 ) ;
#66795 = CIRCLE ( 'NONE', #45183, 31.99999999999998579 ) ;
#66796 = DIRECTION ( 'NONE',  ( -1.000000000000000000, -0.000000000000000000, 0.000000000000000000 ) ) ;
#66797 = CARTESIAN_POINT ( 'NONE',  ( -94.99999999999997158, -213.0599564267049857, 83.17374999999999829 ) ) ;
#66798 = EDGE_CURVE ( 'NONE', #7707, #15838, #13889, .T. ) ;
#66799 =( BOUNDED_CURVE ( )  B_SPLINE_CURVE ( 2, ( #72731, #4727, #44186, #11446, #34379, #3980, #55833 ),
 .UNSPECIFIED., .F., .F. ) 
 B_SPLINE_CURVE_WITH_KNOTS ( ( 3, 2, 2, 3 ),
 ( 0.4166666666666662966, 0.4236111111111106609, 0.4305555555555550806, 0.4374999999999994449 ),
 .UNSPECIFIED. ) 
 CURVE ( )  GEOMETRIC_REPRESENTATION_ITEM ( )  RATIONAL_B_SPLINE_CURVE ( ( 1.000000000000007550, 0.8660254037844311581, 1.000000000000000000, 0.8660254037844387076, 1.000000000000000000, 0.8660254037844493658, 0.9999999999999893419 ) ) 
 REPRESENTATION_ITEM ( '' )  );
#66800 = CARTESIAN_POINT ( 'NONE',  ( -94.99999999999997158, -212.6630814284392557, 83.61031250086716682 ) ) ;
#66801 = ORIENTED_EDGE ( 'NONE', *, *, #14163, .T. ) ;
#66802 = FACE_OUTER_BOUND ( 'NONE', #14193, .T. ) ;
#66803 = EDGE_LOOP ( 'NONE', ( #43221, #6144, #61775, #63337 ) ) ;
#66804 = ADVANCED_FACE ( 'NONE', ( #8643 ), #30809, .T. ) ;
#66805 = CARTESIAN_POINT ( 'NONE',  ( 10.00000000000000000, 0.000000000000000000, 0.000000000000000000 ) ) ;
#66806 = FACE_BOUND ( 'NONE', #49465, .T. ) ;
#66807 = VECTOR ( 'NONE', #54088, 1000.000000000000000 ) ;
#66808 = DIRECTION ( 'NONE',  ( -1.000000000000000000, 0.000000000000000000, 0.000000000000000000 ) ) ;
#66809 = CARTESIAN_POINT ( 'NONE',  ( 94.99999999999998579, 92.66308142843932671, 78.05406250086714692 ) ) ;
#66810 = CARTESIAN_POINT ( 'NONE',  ( -4.653126046682595884, -146.1313684676804314, 5.500000000000000000 ) ) ;
#66811 = CARTESIAN_POINT ( 'NONE',  ( 97.64999999999999147, 89.99999989488613039, 86.58687499784845443 ) ) ;
#66812 = CARTESIAN_POINT ( 'NONE',  ( 100.0000000000260343, -214.9999999999999716, -74.99999999999349143 ) ) ;
#66813 = CARTESIAN_POINT ( 'NONE',  ( 94.21072067537627959, 92.27861417635780583, 74.85481846778738202 ) ) ;
#66814 = LINE ( 'NONE', #31846, #54586 ) ;
#66815 = CARTESIAN_POINT ( 'NONE',  ( 10.00000000000000000, 2.663952781846733675, -41.91543099594814947 ) ) ;
#66816 = CARTESIAN_POINT ( 'NONE',  ( -92.69370383062498320, -210.0000000000000568, 74.79348190356851944 ) ) ;
#66817 = ADVANCED_FACE ( 'NONE', ( #8262 ), #66166, .F. ) ;
#66818 = CARTESIAN_POINT ( 'NONE',  ( 5.000000000000000000, 27.75498641678786527, -31.52238457039571173 ) ) ;
#66819 = ORIENTED_EDGE ( 'NONE', *, *, #1042, .T. ) ;
#66820 = CARTESIAN_POINT ( 'NONE',  ( -97.30629616937501680, 88.66845928578038638, 84.61572916753380014 ) ) ;
#66821 = EDGE_CURVE ( 'NONE', #44951, #70845, #59438, .T. ) ;
#66822 = EDGE_CURVE ( 'NONE', #54007, #35131, #46405, .T. ) ;
#66823 = CARTESIAN_POINT ( 'NONE',  ( 10.00000000000000000, 0.000000000000000000, 0.000000000000000000 ) ) ;
#66824 = CARTESIAN_POINT ( 'NONE',  ( 10.00000000000000000, -21.32104025579135964, 30.84782396557210760 ) ) ;
#66825 = ADVANCED_FACE ( 'NONE', ( #31926 ), #54866, .F. ) ;
#66826 = VERTEX_POINT ( 'NONE', #4130 ) ;
#66827 = CARTESIAN_POINT ( 'NONE',  ( 95.00000000000000000, -209.9999999999999716, 75.00000000000000000 ) ) ;
#66828 = CARTESIAN_POINT ( 'NONE',  ( 15.00000000000000000, -0.9646360437372099028, 23.52805723605590771 ) ) ;
#66829 = CIRCLE ( 'NONE', #30846, 12.49999999999999822 ) ;
#66830 = CYLINDRICAL_SURFACE ( 'NONE', #31192, 31.99999999999998579 ) ;
#66831 = AXIS2_PLACEMENT_3D ( 'NONE', #7943, #30864, #14692 ) ;
#66832 = DIRECTION ( 'NONE',  ( 1.000000000000000000, 0.000000000000000000, 0.000000000000000000 ) ) ;
#66833 = CARTESIAN_POINT ( 'NONE',  ( 96.15314808468748708, -208.0026889286704943, 78.15989583420049769 ) ) ;
#66834 = CIRCLE ( 'NONE', #2051, 31.99999999999998579 ) ;
#66835 = ORIENTED_EDGE ( 'NONE', *, *, #3191, .T. ) ;
#66836 = AXIS2_PLACEMENT_3D ( 'NONE', #54877, #36843, #2682 ) ;
#66837 = ORIENTED_EDGE ( 'NONE', *, *, #22395, .F. ) ;
#66838 = DIRECTION ( 'NONE',  ( -1.000000000000000000, 0.000000000000000000, 0.000000000000000000 ) ) ;
#66839 = CIRCLE ( 'NONE', #29632, 31.99999999999999645 ) ;
#66840 = DIRECTION ( 'NONE',  ( -1.000000000000000000, -0.000000000000000000, -0.000000000000000000 ) ) ;
#66841 = CYLINDRICAL_SURFACE ( 'NONE', #59256, 15.70000000000327312 ) ;
#66842 = DIRECTION ( 'NONE',  ( 0.000000000000000000, 0.2334453638558989796, 0.9723699203976782224 ) ) ;
#66843 = CARTESIAN_POINT ( 'NONE',  ( 10.00000000000000000, 28.89263327155850902, -71.91182617369157981 ) ) ;
#66844 = CARTESIAN_POINT ( 'NONE',  ( 96.15314808468748708, -208.0026889286704943, 77.52489583420047836 ) ) ;
#66845 = ORIENTED_EDGE ( 'NONE', *, *, #28802, .T. ) ;
#66846 = FACE_OUTER_BOUND ( 'NONE', #58160, .T. ) ;
#66847 = ORIENTED_EDGE ( 'NONE', *, *, #8676, .F. ) ;
#66848 = VERTEX_POINT ( 'NONE', #4880 ) ;
#66849 = CARTESIAN_POINT ( 'NONE',  ( 10.00000000000000000, 10.74501242461333028, -35.92658777277499382 ) ) ;
#66850 = CARTESIAN_POINT ( 'NONE',  ( 10.00000000000000000, 0.000000000000000000, 0.000000000000000000 ) ) ;
#66851 = EDGE_LOOP ( 'NONE', ( #36965, #12199, #27535, #72501 ) ) ;
#66852 = CARTESIAN_POINT ( 'NONE',  ( 15.00000000000000000, -18.13022148937242761, 15.02647892043569122 ) ) ;
#66853 = CARTESIAN_POINT ( 'NONE',  ( 93.67500000000001137, -207.7050326799711968, 79.81354166840095843 ) ) ;
#66854 = CARTESIAN_POINT ( 'NONE',  ( 96.32499999999998863, 87.70503267997126784, 84.49666666666666970 ) ) ;
#66855 = CIRCLE ( 'NONE', #15230, 31.99999999999999289 ) ;
#66856 = ORIENTED_EDGE ( 'NONE', *, *, #61748, .T. ) ;
#66857 = CARTESIAN_POINT ( 'NONE',  ( 0.000000000000000000, 73.73191006444572793, -14.66109333815486515 ) ) ;
#66858 = CARTESIAN_POINT ( 'NONE',  ( -92.91683521821995839, -211.0005890871206589, 74.79348190356851944 ) ) ;
#66859 = ORIENTED_EDGE ( 'NONE', *, *, #11148, .T. ) ;
#66860 = CARTESIAN_POINT ( 'NONE',  ( 93.67499999999998295, 92.29496732002878900, 84.25854166840096582 ) ) ;
#66861 = CARTESIAN_POINT ( 'NONE',  ( -97.30629616937501680, 88.66845928578038638, 83.50447916753383026 ) ) ;
#66862 = CARTESIAN_POINT ( 'NONE',  ( 93.84685191531248449, 88.00268892867053694, 81.49364583420047836 ) ) ;
#66863 = ORIENTED_EDGE ( 'NONE', *, *, #72097, .F. ) ;
#66864 = DIRECTION ( 'NONE',  ( -1.000000000000000000, 0.000000000000000000, 0.000000000000000000 ) ) ;
#66865 = ORIENTED_EDGE ( 'NONE', *, *, #74327, .F. ) ;
#66866 = CYLINDRICAL_SURFACE ( 'NONE', #3319, 82.00000000000000000 ) ;
#66867 = EDGE_LOOP ( 'NONE', ( #62507, #15252, #23859, #56061 ) ) ;
#66868 = EDGE_CURVE ( 'NONE', #1281, #73677, #61261, .T. ) ;
#66869 = ORIENTED_EDGE ( 'NONE', *, *, #47644, .F. ) ;
#66870 = CARTESIAN_POINT ( 'NONE',  ( 93.67499999999999716, 87.70503267997126784, 79.94583333333332575 ) ) ;
#66871 = EDGE_CURVE ( 'NONE', #73511, #62613, #55978, .T. ) ;
#66872 = VERTEX_POINT ( 'NONE', #68007 ) ;
#66873 = CARTESIAN_POINT ( 'NONE',  ( 3.000000000000000000, 1.467624384280029837, 2.541999999999997151 ) ) ;
#66874 = CARTESIAN_POINT ( 'NONE',  ( 94.99999999999998579, 93.05995642670504253, 88.01562500173429271 ) ) ;
#66875 = ORIENTED_EDGE ( 'NONE', *, *, #63705, .T. ) ;
#66876 = DIRECTION ( 'NONE',  ( 1.000000000000000000, 0.000000000000000000, 0.000000000000000000 ) ) ;
#66877 = CARTESIAN_POINT ( 'NONE',  ( -93.84685191531247028, -211.9973110713294489, 80.32947916753380468 ) ) ;
#66879 = VERTEX_POINT ( 'NONE', #62767 ) ;
#66878 = EDGE_CURVE ( 'NONE', #69865, #590, #31843, .T. ) ;
#66880 = DIRECTION ( 'NONE',  ( 1.000000000000000000, 0.000000000000000000, 0.000000000000000000 ) ) ;
#66881 = AXIS2_PLACEMENT_3D ( 'NONE', #20273, #70653, #36456 ) ;
#66882 = DIRECTION ( 'NONE',  ( -1.000000000000000000, 0.000000000000000000, 0.000000000000000000 ) ) ;
#66883 = CARTESIAN_POINT ( 'NONE',  ( 0.000000000000000000, 0.000000000000000000, -275.0000000000000000 ) ) ;
#66884 = CARTESIAN_POINT ( 'NONE',  ( 95.00000000000000000, -209.9999999999999716, 90.00000000000000000 ) ) ;
#66885 = AXIS2_PLACEMENT_3D ( 'NONE', #10848, #49568, #61986 ) ;
#66886 = DIRECTION ( 'NONE',  ( 0.000000000000000000, 0.000000000000000000, 1.000000000000000000 ) ) ;
#66887 = AXIS2_PLACEMENT_3D ( 'NONE', #29696, #25188, #7529 ) ;
#66888 = CARTESIAN_POINT ( 'NONE',  ( 97.30629616937498838, 88.66845928578035796, 86.73239583420047438 ) ) ;
#66889 = CIRCLE ( 'NONE', #64488, 77.49899999999999523 ) ;
#66890 = CARTESIAN_POINT ( 'NONE',  ( 0.000000000000000000, 0.000000000000000000, 0.000000000000000000 ) ) ;
#66891 = DIRECTION ( 'NONE',  ( -1.000000000000000000, -0.000000000000000000, 0.000000000000000000 ) ) ;
#66892 = CARTESIAN_POINT ( 'NONE',  ( 0.000000000000000000, -6.903761155838323837, 77.19088730480521576 ) ) ;
#66893 = EDGE_CURVE ( 'NONE', #6463, #16864, #38695, .T. ) ;
#66894 = CARTESIAN_POINT ( 'NONE',  ( 10.00000000000000000, -62.50884508063453637, 41.76106447765467777 ) ) ;
#66895 = EDGE_CURVE ( 'NONE', #32355, #35859, #32665, .T. ) ;
#66896 = DIRECTION ( 'NONE',  ( 2.603472992746261562E-14, 2.546204323184492723E-14, -1.000000000000000000 ) ) ;
#66897 = DIRECTION ( 'NONE',  ( 0.000000000000000000, -0.9238795325112822976, -0.3826834323651006620 ) ) ;
#66898 = CIRCLE ( 'NONE', #51279, 77.49900000000000944 ) ;
#66899 = CARTESIAN_POINT ( 'NONE',  ( 97.65000000000006253, -208.4700217866474929, 75.13041666666666174 ) ) ;
#66900 = DIRECTION ( 'NONE',  ( 1.000000000000000000, 0.000000000000000000, 0.000000000000000000 ) ) ;
#66901 = CARTESIAN_POINT ( 'NONE',  ( 10.00000000000000000, 55.16347631943129670, -60.67117009219074220 ) ) ;
#66902 = EDGE_CURVE ( 'NONE', #1787, #45691, #72394, .T. ) ;
#66903 = ADVANCED_FACE ( 'NONE', ( #50707 ), #28510, .F. ) ;
#66904 = CARTESIAN_POINT ( 'NONE',  ( 0.000000000000000000, 65.58780272294129077, -36.73666225445822420 ) ) ;
#66905 = PRESENTATION_LAYER_ASSIGNMENT (  '', '', ( #28528 ) ) ;
#66906 = CARTESIAN_POINT ( 'NONE',  ( -97.64999999999994884, -208.4700217866474645, 84.23208333333333542 ) ) ;
#66907 = LINE ( 'NONE', #72895, #54879 ) ;
#66908 = DIRECTION ( 'NONE',  ( 0.000000000000000000, -0.9723699203976740035, -0.2334453638559160216 ) ) ;
#66909 = CARTESIAN_POINT ( 'NONE',  ( 10.00000000000000000, -21.32104025579091910, -30.84782396557241313 ) ) ;
#66910 = DIRECTION ( 'NONE',  ( -1.000000000000000000, -0.000000000000000000, -0.000000000000000000 ) ) ;
#66911 = DIRECTION ( 'NONE',  ( 0.000000000000000000, 0.000000000000000000, 1.000000000000000000 ) ) ;
#66912 = ORIENTED_EDGE ( 'NONE', *, *, #31670, .F. ) ;
#66913 = EDGE_LOOP ( 'NONE', ( #42661, #57713, #56131, #12749 ) ) ;
#66914 = DIRECTION ( 'NONE',  ( 0.000000000000000000, 0.000000000000000000, 1.000000000000000000 ) ) ;
#66915 = CARTESIAN_POINT ( 'NONE',  ( 10.00000000000000000, -59.03961581697432592, 46.53671651293927880 ) ) ;
#66916 = EDGE_LOOP ( 'NONE', ( #45792, #23046, #5481, #10322 ) ) ;
#66917 = CARTESIAN_POINT ( 'NONE',  ( 97.30629616937498838, -211.3315407142195852, 82.28739583420048120 ) ) ;
#66918 = CARTESIAN_POINT ( 'NONE',  ( 93.84685191531251292, -211.9973110713294489, 83.55739583420049144 ) ) ;
#66919 = AXIS2_PLACEMENT_3D ( 'NONE', #55142, #3673, #9656 ) ;
#66920 = VERTEX_POINT ( 'NONE', #16129 ) ;
#66921 = CARTESIAN_POINT ( 'NONE',  ( 95.00000000000000000, -207.3369185715606307, 87.73781250086715033 ) ) ;
#66922 = CIRCLE ( 'NONE', #5781, 16.00000000000000000 ) ;
#66923 = ORIENTED_EDGE ( 'NONE', *, *, #39666, .T. ) ;
#66924 = CARTESIAN_POINT ( 'NONE',  ( 0.000000000000000000, -21.32104025579091910, -30.84782396557241313 ) ) ;
#66925 = ORIENTED_EDGE ( 'NONE', *, *, #388, .F. ) ;
#66926 = CARTESIAN_POINT ( 'NONE',  ( -95.00000000000002842, 92.66308142843932671, 76.30781250086715772 ) ) ;
#66927 = ORIENTED_EDGE ( 'NONE', *, *, #38897, .T. ) ;
#66928 = AXIS2_PLACEMENT_3D ( 'NONE', #36647, #8823, #2114 ) ;
#66929 = ORIENTED_EDGE ( 'NONE', *, *, #67635, .F. ) ;
#66930 = DIRECTION ( 'NONE',  ( 0.000000000000000000, 0.000000000000000000, -1.000000000000000000 ) ) ;
#66931 = AXIS2_PLACEMENT_3D ( 'NONE', #3224, #71601, #65618 ) ;
#66932 = VERTEX_POINT ( 'NONE', #22900 ) ;
#66933 = CARTESIAN_POINT ( 'NONE',  ( 0.000000000000000000, 10.41901085202135491, -40.68715046381917944 ) ) ;
#66934 = CYLINDRICAL_SURFACE ( 'NONE', #3261, 77.49899999999999523 ) ;
#66935 = VERTEX_POINT ( 'NONE', #33400 ) ;
#66936 = CARTESIAN_POINT ( 'NONE',  ( 10.00000000000000000, 20.41045688087824317, 72.35160999960824313 ) ) ;
#66937 = ORIENTED_EDGE ( 'NONE', *, *, #72449, .F. ) ;
#66938 = DIRECTION ( 'NONE',  ( -1.000000000000000000, -0.000000000000000000, -0.000000000000000000 ) ) ;
#66939 = PRODUCT_DEFINITION ( 'UNKNOWN', '', #71206, #25113 ) ;
#66940 = EDGE_LOOP ( 'NONE', ( #23296, #24715, #60830, #29869 ) ) ;
#66941 = ADVANCED_FACE ( 'NONE', ( #50333 ), #34163, .T. ) ;
#66942 = VERTEX_POINT ( 'NONE', #62004 ) ;
#66943 = EDGE_LOOP ( 'NONE', ( #34970, #29743, #40518, #16469 ) ) ;
#66944 = CARTESIAN_POINT ( 'NONE',  ( 97.30629616937498838, -211.3315407142195852, 75.30239583420048177 ) ) ;
#66945 = CONTEXT_DEPENDENT_SHAPE_REPRESENTATION ( #17236, #58469 ) ;
#66946 = CARTESIAN_POINT ( 'NONE',  ( 0.000000000000000000, -75.11764819372145041, -2.946379043147127064 ) ) ;
#66947 = VERTEX_POINT ( 'NONE', #15373 ) ;
#66948 = ORIENTED_EDGE ( 'NONE', *, *, #44389, .F. ) ;
#66949 = EDGE_CURVE ( 'NONE', #49570, #69413, #4234, .T. ) ;
#66950 = ORIENTED_EDGE ( 'NONE', *, *, #73580, .F. ) ;
#66951 = CARTESIAN_POINT ( 'NONE',  ( 0.000000000000000000, 6.762365576493310826, 25.66652317338401090 ) ) ;
#66952 = DIRECTION ( 'NONE',  ( 0.000000000000000000, -0.9510565162951500895, -0.3090169943749581649 ) ) ;
#66953 = AXIS2_PLACEMENT_3D ( 'NONE', #69677, #18174, #64053 ) ;
#66954 = EDGE_CURVE ( 'NONE', #73822, #30711, #39441, .T. ) ;
#66955 = CARTESIAN_POINT ( 'NONE',  ( -93.84685191531254134, 91.99731107132950569, 74.98489583420048632 ) ) ;
#66956 = ORIENTED_EDGE ( 'NONE', *, *, #1685, .T. ) ;
#66957 = CARTESIAN_POINT ( 'NONE',  ( 96.15314808468748708, 88.00268892867053694, 77.78947916753381264 ) ) ;
#66958 = CIRCLE ( 'NONE', #40568, 32.00000000000000000 ) ;
#66959 = ORIENTED_EDGE ( 'NONE', *, *, #30223, .T. ) ;
#66960 = CYLINDRICAL_SURFACE ( 'NONE', #45545, 16.00000000000000000 ) ;
#66961 = CARTESIAN_POINT ( 'NONE',  ( 10.00000000000000000, 33.17418723428307459, 17.67226234102837878 ) ) ;
#66962 = ADVANCED_FACE ( 'NONE', ( #56365 ), #10865, .F. ) ;
#66963 = DIRECTION ( 'NONE',  ( 1.000000000000000000, 1.427937372958405461E-15, 7.962523111839130290E-16 ) ) ;
#66964 = CARTESIAN_POINT ( 'NONE',  ( 5.000000000000000000, -27.75498641678720446, -31.52238457039628727 ) ) ;
#66965 = CARTESIAN_POINT ( 'NONE',  ( 10.00000000000000000, 20.40083707022987625, -72.35432306680462489 ) ) ;
#66966 = CARTESIAN_POINT ( 'NONE',  ( -93.84685191531247028, -211.9973110713294489, 80.32947916753380468 ) ) ;
#66967 = CARTESIAN_POINT ( 'NONE',  ( 0.000000000000000000, 32.34446384430010113, -26.79245525562679831 ) ) ;
#66968 = CARTESIAN_POINT ( 'NONE',  ( -2.499999999999965361, 90.00000000000000000, -90.00000000000000000 ) ) ;
#66969 = FACE_OUTER_BOUND ( 'NONE', #37246, .T. ) ;
#66970 = EDGE_LOOP ( 'NONE', ( #29947, #60229, #32337, #56801 ) ) ;
#66971 = VERTEX_POINT ( 'NONE', #61627 ) ;
#66972 = DIRECTION ( 'NONE',  ( -1.000000000000000000, -1.343011723336883198E-16, -0.000000000000000000 ) ) ;
#66973 = PLANE ( 'NONE',  #19495 ) ;
#66974 = EDGE_CURVE ( 'NONE', #19944, #28475, #41464, .T. ) ;
#66975 = CARTESIAN_POINT ( 'NONE',  ( 95.29776683160980610, -207.6384304500494409, 74.83035915144985495 ) ) ;
#66976 = EDGE_CURVE ( 'NONE', #7335, #37614, #33036, .T. ) ;
#66977 = CARTESIAN_POINT ( 'NONE',  ( -97.30629616937501680, 90.00000000000004263, 80.75281250086715090 ) ) ;
#66978 = CARTESIAN_POINT ( 'NONE',  ( 10.00000000000000000, 0.000000000000000000, 0.000000000000000000 ) ) ;
#66979 = FACE_BOUND ( 'NONE', #627, .T. ) ;
#66980 = AXIS2_PLACEMENT_3D ( 'NONE', #41691, #30402, #46237 ) ;
#66981 = ORIENTED_EDGE ( 'NONE', *, *, #15067, .T. ) ;
#66982 = DIRECTION ( 'NONE',  ( 1.000000000000000000, 0.000000000000000000, 0.000000000000000000 ) ) ;
#66983 = AXIS2_PLACEMENT_3D ( 'NONE', #34821, #38982, #40092 ) ;
#66984 = CIRCLE ( 'NONE', #67161, 42.00000000000000000 ) ;
#66985 = CARTESIAN_POINT ( 'NONE',  ( 0.000000000000000000, 0.000000000000000000, 0.000000000000000000 ) ) ;
#66986 = CARTESIAN_POINT ( 'NONE',  ( -3.000000000000000000, 22.07842321921481243, 8.187992925817422218 ) ) ;
#66987 = CIRCLE ( 'NONE', #21358, 77.49899999999999523 ) ;
#66988 = DIRECTION ( 'NONE',  ( 1.343011723336883198E-16, -1.000000000000000000, 0.000000000000000000 ) ) ;
#66989 = DIRECTION ( 'NONE',  ( 1.000000000000000000, 0.000000000000000000, -0.000000000000000000 ) ) ;
#66990 = CARTESIAN_POINT ( 'NONE',  ( -92.69370383062498320, -209.9999999999999716, 81.86406250086714920 ) ) ;
#66991 = DIRECTION ( 'NONE',  ( 0.000000000000000000, 0.000000000000000000, 1.000000000000000000 ) ) ;
#66992 = SHAPE_REPRESENTATION ( 'output shaft', ( #43395 ), #60192 ) ;
#66993 = EDGE_LOOP ( 'NONE', ( #51325, #60969, #72216, #35587 ) ) ;
#66994 = CYLINDRICAL_SURFACE ( 'NONE', #10667, 82.00000000000000000 ) ;
#66995 = DIRECTION ( 'NONE',  ( -1.000000000000000000, 7.571543891232750625E-15, 2.563413034563919882E-14 ) ) ;
#66996 = CARTESIAN_POINT ( 'NONE',  ( 10.00000000000000000, -36.88895765772628010, -6.736453364083947015 ) ) ;
#66997 = VERTEX_POINT ( 'NONE', #10483 ) ;
#66998 = DIRECTION ( 'NONE',  ( 0.8774505977381978905, 0.4796670183876304283, -0.000000000000000000 ) ) ;
#66999 = PLANE ( 'NONE',  #10158 ) ;
#67000 = AXIS2_PLACEMENT_3D ( 'NONE', #26525, #54733, #43481 ) ;
#67001 = AXIS2_PLACEMENT_3D ( 'NONE', #34090, #51378, #73938 ) ;
#67003 = DIRECTION ( 'NONE',  ( -1.000000000000000000, 0.000000000000000000, -0.000000000000000000 ) ) ;
#67002 = TOROIDAL_SURFACE ( 'NONE', #34647, 22.90000000000000213, 0.5999999999999937605 ) ;
#67004 = VERTEX_POINT ( 'NONE', #16501 ) ;
#67005 = VECTOR ( 'NONE', #48504, 1000.000000000000114 ) ;
#67006 = DIRECTION ( 'NONE',  ( 0.000000000000000000, 0.000000000000000000, 1.000000000000000000 ) ) ;
#67007 = ORIENTED_EDGE ( 'NONE', *, *, #41012, .T. ) ;
#67008 = VECTOR ( 'NONE', #45489, 1000.000000000000000 ) ;
#67009 =( BOUNDED_CURVE ( )  B_SPLINE_CURVE ( 2, ( #72988, #55718, #4235, #9115, #27129, #50059, #60636, #43716, #66637, #9480, #32404 ),
 .UNSPECIFIED., .F., .F. ) 
 B_SPLINE_CURVE_WITH_KNOTS ( ( 3, 2, 2, 2, 2, 3 ),
 ( 0.1481709449582802873, 0.1481710763592573865, 0.1552268419001741062, 0.1622826074410907982, 0.1693383729820075179, 0.1693384224428226559 ),
 .UNSPECIFIED. ) 
 CURVE ( )  GEOMETRIC_REPRESENTATION_ITEM ( )  RATIONAL_B_SPLINE_CURVE ( ( 0.9999950100198486957, 0.9999975049634587387, 1.000000000000000000, 0.8660254037844387076, 1.000000000000000000, 0.8660254037844387076, 1.000000000000000000, 0.8660254037844387076, 1.000000000000000000, 0.9999990608400038949, 0.9999981216931748129 ) ) 
 REPRESENTATION_ITEM ( '' )  );
#67010 = DIRECTION ( 'NONE',  ( 1.000000000000000000, -0.000000000000000000, -0.000000000000000000 ) ) ;
#67011 = CARTESIAN_POINT ( 'NONE',  ( 0.000000000000000000, -3.925862922256468046, 41.81611651403860463 ) ) ;
#67012 = EDGE_LOOP ( 'NONE', ( #49812, #21758, #58820, #27130 ) ) ;
#67013 = EDGE_CURVE ( 'NONE', #15750, #49569, #33791, .T. ) ;
#67014 = DIRECTION ( 'NONE',  ( -0.5200609990133016058, -0.8541291221503261033, 0.000000000000000000 ) ) ;
#67015 = ORIENTED_EDGE ( 'NONE', *, *, #41746, .T. ) ;
#67016 = FACE_OUTER_BOUND ( 'NONE', #12574, .T. ) ;
#67017 = ORIENTED_EDGE ( 'NONE', *, *, #37163, .T. ) ;
#67018 = VERTEX_POINT ( 'NONE', #24365 ) ;
#67019 = EDGE_CURVE ( 'NONE', #44110, #42446, #17614, .T. ) ;
#67020 = VERTEX_POINT ( 'NONE', #52553 ) ;
#67021 = CARTESIAN_POINT ( 'NONE',  ( -7.001685179585692254, -14.98378029539707512, -1.199999999999999956 ) ) ;
#67022 = EDGE_CURVE ( 'NONE', #32475, #4971, #46239, .T. ) ;
#67023 = ORIENTED_EDGE ( 'NONE', *, *, #54518, .F. ) ;
#67024 = ORIENTED_EDGE ( 'NONE', *, *, #55840, .T. ) ;
#67025 = CARTESIAN_POINT ( 'NONE',  ( 97.30629616937498838, 90.00000000000002842, 78.05406250086716113 ) ) ;
#67026 = DIRECTION ( 'NONE',  ( 1.000000000000000000, 0.000000000000000000, 0.000000000000000000 ) ) ;
#67027 = CIRCLE ( 'NONE', #62221, 16.00000000000000000 ) ;
#67028 = CARTESIAN_POINT ( 'NONE',  ( -10.00000000000000000, 0.000000000000000000, 0.000000000000000000 ) ) ;
#67029 = AXIS2_PLACEMENT_3D ( 'NONE', #18260, #41202, #12613 ) ;
#67030 = VERTEX_POINT ( 'NONE', #17982 ) ;
#67031 = AXIS2_PLACEMENT_3D ( 'NONE', #25396, #6624, #47219 ) ;
#67032 = EDGE_CURVE ( 'NONE', #38079, #66432, #9034, .T. ) ;
#67033 = EDGE_LOOP ( 'NONE', ( #62757, #12829, #11460, #49199 ) ) ;
#67034 = ORIENTED_EDGE ( 'NONE', *, *, #23276, .F. ) ;
#67035 = CARTESIAN_POINT ( 'NONE',  ( 93.84685191531248449, 91.99731107132950569, 87.63197916753379957 ) ) ;
#67036 = ORIENTED_EDGE ( 'NONE', *, *, #28185, .T. ) ;
#67037 = CARTESIAN_POINT ( 'NONE',  ( 92.69370383062501162, -211.3315407142195852, 84.61572916753380014 ) ) ;
#67038 = PRODUCT_CONTEXT ( 'NONE', #34457, 'mechanical' ) ;
#67039 = DIRECTION ( 'NONE',  ( -1.000000000000000000, 0.000000000000000000, 0.000000000000000000 ) ) ;
#67040 = CIRCLE ( 'NONE', #20232, 31.99999999999999289 ) ;
#67041 = FACE_OUTER_BOUND ( 'NONE', #68313, .T. ) ;
#67042 = CARTESIAN_POINT ( 'NONE',  ( -92.35000000000006537, 90.00000034979574082, 77.69687501385438111 ) ) ;
#67043 = AXIS2_PLACEMENT_3D ( 'NONE', #25673, #31675, #61376 ) ;
#67044 = CARTESIAN_POINT ( 'NONE',  ( 10.00000000000000000, 0.000000000000000000, 0.000000000000000000 ) ) ;
#67045 = CARTESIAN_POINT ( 'NONE',  ( 10.00000000000000000, 0.000000000000000000, 0.000000000000000000 ) ) ;
#67046 = CARTESIAN_POINT ( 'NONE',  ( 6.000000000000000000, -80.28980883073747066, -16.65972982745017461 ) ) ;
#67047 = CARTESIAN_POINT ( 'NONE',  ( -96.15314808468747287, -208.0026889286704943, 87.63197916753379957 ) ) ;
#67048 = CARTESIAN_POINT ( 'NONE',  ( -92.69370383062502583, 91.33154071421968467, 84.45697916753383083 ) ) ;
#67049 = ORIENTED_EDGE ( 'NONE', *, *, #36597, .T. ) ;
#67051 = CARTESIAN_POINT ( 'NONE',  ( -93.84685191531252713, 88.00268892867056536, 87.31447916753380412 ) ) ;
#67050 = CARTESIAN_POINT ( 'NONE',  ( 92.69370383062498320, 91.33154071421968467, 87.68489583420047495 ) ) ;
#67052 = EDGE_LOOP ( 'NONE', ( #68278, #66433, #24037, #13025 ) ) ;
#67053 = CARTESIAN_POINT ( 'NONE',  ( 15.00000000000000000, -22.32062822937489344, -14.36278369418800160 ) ) ;
#67054 = EDGE_CURVE ( 'NONE', #5282, #14250, #43956, .T. ) ;
#67055 = DIRECTION ( 'NONE',  ( 0.000000000000000000, -0.5877852522924797984, 0.8090169943749426773 ) ) ;
#67056 = LINE ( 'NONE', #38862, #12674 ) ;
#67057 = DIRECTION ( 'NONE',  ( -1.000000000000000000, 0.000000000000000000, -0.000000000000000000 ) ) ;
#67058 = CARTESIAN_POINT ( 'NONE',  ( 2.047646702416564768, -96.54137380445985173, 5.500000000000000000 ) ) ;
#67059 = CARTESIAN_POINT ( 'NONE',  ( 10.00000000000000000, -22.48208911017474065, -35.47612816024548721 ) ) ;
#67060 = CIRCLE ( 'NONE', #11818, 12.50000000000000000 ) ;
#67061 = PLANE ( 'NONE',  #16996 ) ;
#67062 = LINE ( 'NONE', #32474, #11998 ) ;
#67063 = VERTEX_POINT ( 'NONE', #1474 ) ;
#67064 = AXIS2_PLACEMENT_3D ( 'NONE', #32350, #55664, #4553 ) ;
#67065 = ORIENTED_EDGE ( 'NONE', *, *, #68957, .F. ) ;
#67066 = AXIS2_PLACEMENT_3D ( 'NONE', #23029, #12097, #7205 ) ;
#67067 = CIRCLE ( 'NONE', #34650, 37.49900000000001654 ) ;
#67068 = CARTESIAN_POINT ( 'NONE',  ( -97.65000000000001990, 88.47002178664754979, 81.79791666666666572 ) ) ;
#67069 = ADVANCED_FACE ( 'NONE', ( #35274 ), #58566, .F. ) ;
#67070 = CARTESIAN_POINT ( 'NONE',  ( 11.99999999999999822, 0.000000000000000000, 0.000000000000000000 ) ) ;
#67071 = EDGE_CURVE ( 'NONE', #23893, #51310, #64226, .T. ) ;
#67072 = CARTESIAN_POINT ( 'NONE',  ( 92.35000000005783249, -210.0000112241611703, 75.47473230081648410 ) ) ;
#67073 = CARTESIAN_POINT ( 'NONE',  ( 10.00000000000000178, 12.24744871391589029, 2.500000000000004441 ) ) ;
#67074 = CARTESIAN_POINT ( 'NONE',  ( 97.64999999999999147, -209.9999999999999716, 76.98250000000000171 ) ) ;
#67075 = DIRECTION ( 'NONE',  ( 0.000000000000000000, 0.000000000000000000, 1.000000000000000000 ) ) ;
#67076 = CARTESIAN_POINT ( 'NONE',  ( 10.00000000000000000, -10.96151621346461447, -35.95386929396268272 ) ) ;
#67077 = VECTOR ( 'NONE', #55461, 1000.000000000000000 ) ;
#67078 = EDGE_CURVE ( 'NONE', #13867, #16540, #46556, .T. ) ;
#67079 = ORIENTED_EDGE ( 'NONE', *, *, #22178, .F. ) ;
#67080 = CARTESIAN_POINT ( 'NONE',  ( -92.69370383062504004, 90.00000000000004263, 80.43531250086714124 ) ) ;
#67081 = PLANE ( 'NONE',  #9137 ) ;
#67082 = DIRECTION ( 'NONE',  ( 0.000000000000000000, -0.8090169943749422332, -0.5877852522924803536 ) ) ;
#67083 = CARTESIAN_POINT ( 'NONE',  ( 11.99999999999999822, 54.21277698773752007, -55.38113227695726692 ) ) ;
#67084 = CARTESIAN_POINT ( 'NONE',  ( 15.00000000000000000, 20.85821328998741109, -10.92862929874522671 ) ) ;
#67085 = FACE_OUTER_BOUND ( 'NONE', #61485, .T. ) ;
#67086 = PLANE ( 'NONE',  #69775 ) ;
#67087 = CARTESIAN_POINT ( 'NONE',  ( -235.0000123116479926, -123.0000000000000284, 2.500000000000000000 ) ) ;
#67088 = CIRCLE ( 'NONE', #62445, 16.00000000000000000 ) ;
#67089 = AXIS2_PLACEMENT_3D ( 'NONE', #15909, #15160, #62150 ) ;
#67090 = CARTESIAN_POINT ( 'NONE',  ( 92.69370383062498320, 91.33154071421968467, 80.22364583420048234 ) ) ;
#67091 = AXIS2_PLACEMENT_3D ( 'NONE', #13998, #36566, #31663 ) ;
#67092 = AXIS2_PLACEMENT_3D ( 'NONE', #66904, #15775, #20671 ) ;
#67093 = CARTESIAN_POINT ( 'NONE',  ( -92.69370383062498320, -209.9999999999999716, 83.76906250086716454 ) ) ;
#67094 = CARTESIAN_POINT ( 'NONE',  ( 97.64999999999990621, 90.00000071509185773, 85.31687502647973531 ) ) ;
#67095 = ORIENTED_EDGE ( 'NONE', *, *, #48352, .T. ) ;
#67096 = DIRECTION ( 'NONE',  ( -1.000000000000000000, 0.000000000000000000, 0.000000000000000000 ) ) ;
#67097 = CARTESIAN_POINT ( 'NONE',  ( -92.34999999999999432, -209.9999999999999716, 78.88750000000000284 ) ) ;
#67098 = FACE_OUTER_BOUND ( 'NONE', #24067, .T. ) ;
#67099 = AXIS2_PLACEMENT_3D ( 'NONE', #1572, #60172, #41743 ) ;
#67100 = VECTOR ( 'NONE', #32319, 1000.000000000000000 ) ;
#67101 = CARTESIAN_POINT ( 'NONE',  ( -95.00000000000002842, 92.66308142843932671, 77.57781250086715374 ) ) ;
#67102 = CARTESIAN_POINT ( 'NONE',  ( 93.84685191531249870, -208.0026889286704943, 84.45697916753380241 ) ) ;
#67103 = ORIENTED_EDGE ( 'NONE', *, *, #18608, .T. ) ;
#67104 = CARTESIAN_POINT ( 'NONE',  ( -95.00000000000002842, 90.00000000000004263, 90.00000000000000000 ) ) ;
#67105 = VERTEX_POINT ( 'NONE', #47298 ) ;
#67106 = LINE ( 'NONE', #32518, #48851 ) ;
#67107 = VERTEX_POINT ( 'NONE', #69844 ) ;
#67108 = AXIS2_PLACEMENT_3D ( 'NONE', #72965, #67348, #15849 ) ;
#67109 = EDGE_CURVE ( 'NONE', #1173, #30034, #29608, .T. ) ;
#67110 = DIRECTION ( 'NONE',  ( -1.000000000000000000, 0.000000000000000000, -0.000000000000000000 ) ) ;
#67111 = CIRCLE ( 'NONE', #69483, 32.00000000000000000 ) ;
#67112 = VERTEX_POINT ( 'NONE', #70203 ) ;
#67113 = VERTEX_POINT ( 'NONE', #41642 ) ;
#67114 = EDGE_CURVE ( 'NONE', #53177, #17752, #36779, .T. ) ;
#67115 = AXIS2_PLACEMENT_3D ( 'NONE', #47700, #1519, #71725 ) ;
#67116 = VECTOR ( 'NONE', #14296, 1000.000000000000000 ) ;
#67117 = CARTESIAN_POINT ( 'NONE',  ( 95.00000000000000000, -212.6630814284392557, 75.99031250086716227 ) ) ;
#67118 = EDGE_CURVE ( 'NONE', #68543, #20059, #71432, .T. ) ;
#67119 = CARTESIAN_POINT ( 'NONE',  ( 10.00000000000000000, 0.000000000000000000, 0.000000000000000000 ) ) ;
#67120 = DIRECTION ( 'NONE',  ( -1.000000000000000000, 0.000000000000000000, 0.000000000000000000 ) ) ;
#67121 = CARTESIAN_POINT ( 'NONE',  ( 0.000000000000000000, -37.22597642581161637, 5.202137450156258502 ) ) ;
#67122 = CARTESIAN_POINT ( 'NONE',  ( 97.30629616937498838, 90.00000000000002842, 86.94406250086716170 ) ) ;
#67123 = CARTESIAN_POINT ( 'NONE',  ( 92.34999999999999432, 90.00001557635631855, 80.55437446300187787 ) ) ;
#67124 = CARTESIAN_POINT ( 'NONE',  ( 95.00000000000000000, -206.9400435732949575, 77.14124999999999943 ) ) ;
#67125 = ORIENTED_EDGE ( 'NONE', *, *, #9253, .T. ) ;
#67126 = EDGE_CURVE ( 'NONE', #4935, #53602, #12698, .T. ) ;
#67127 = ORIENTED_EDGE ( 'NONE', *, *, #38896, .F. ) ;
#67128 = ORIENTED_EDGE ( 'NONE', *, *, #3147, .T. ) ;
#67129 = ORIENTED_EDGE ( 'NONE', *, *, #22178, .T. ) ;
#67130 = DIRECTION ( 'NONE',  ( 0.000000000000000000, 1.000000000000000000, 7.228014483236689653E-16 ) ) ;
#67131 = SHAPE_REPRESENTATION_RELATIONSHIP ( 'NONE' , 'NONE' ,  #23018, #74006 ) ;
#67132 = DIRECTION ( 'NONE',  ( 0.000000000000000000, -0.9238795325112821866, -0.3826834323651006065 ) ) ;
#67133 = CARTESIAN_POINT ( 'NONE',  ( -97.64999999993855795, 90.00001182123732235, 81.82400613091868991 ) ) ;
#67134 = DIRECTION ( 'NONE',  ( 1.000000000000000000, 0.000000000000000000, 0.000000000000000000 ) ) ;
#67135 = SHAPE_REPRESENTATION ( 'housing cover', ( #43395 ), #37485 ) ;
#67136 = CARTESIAN_POINT ( 'NONE',  ( -97.65000000002666525, 90.00000000000008527, -74.99999999999992895 ) ) ;
#67137 = LINE ( 'NONE', #43493, #72775 ) ;
#67138 = VERTEX_POINT ( 'NONE', #24728 ) ;
#67139 = AXIS2_PLACEMENT_3D ( 'NONE', #47455, #13238, #524 ) ;
#67140 = CARTESIAN_POINT ( 'NONE',  ( -96.32499999999996021, -212.2949673200287179, 85.10520833506762983 ) ) ;
#67141 = ORIENTED_EDGE ( 'NONE', *, *, #46529, .T. ) ;
#67142 = LINE ( 'NONE', #49840, #6221 ) ;
#67143 = ORIENTED_EDGE ( 'NONE', *, *, #44597, .T. ) ;
#67144 = CARTESIAN_POINT ( 'NONE',  ( -97.65000000000001990, 90.00000000000004263, 83.09437500173430635 ) ) ;
#67145 = VECTOR ( 'NONE', #18875, 1000.000000000000000 ) ;
#67146 = EDGE_LOOP ( 'NONE', ( #8402, #15806, #29180, #21520 ) ) ;
#67147 = CARTESIAN_POINT ( 'NONE',  ( 97.30629616937498838, 91.33154071421968467, 81.91697916753381037 ) ) ;
#67148 = EDGE_CURVE ( 'NONE', #27140, #57518, #21002, .T. ) ;
#67149 = CARTESIAN_POINT ( 'NONE',  ( -97.64999999999994884, 88.47002178664749295, 76.08291666666664810 ) ) ;
#67150 = AXIS2_PLACEMENT_3D ( 'NONE', #43385, #60301, #53905 ) ;
#67151 = CARTESIAN_POINT ( 'NONE',  ( 10.00000000000000000, -41.19522573413780009, 65.64334221924896440 ) ) ;
#67152 = AXIS2_PLACEMENT_3D ( 'NONE', #36385, #25119, #42782 ) ;
#67153 = DIRECTION ( 'NONE',  ( -1.000000000000000000, -0.000000000000000000, -0.000000000000000000 ) ) ;
#67154 = DIRECTION ( 'NONE',  ( -1.000000000000000000, 0.000000000000000000, 0.000000000000000000 ) ) ;
#67155 = CIRCLE ( 'NONE', #63578, 21.00000000000000000 ) ;
#67156 = DIRECTION ( 'NONE',  ( -1.000000000000000000, -0.000000000000000000, 0.000000000000000000 ) ) ;
#67157 = ORIENTED_EDGE ( 'NONE', *, *, #54932, .T. ) ;
#67158 = LINE ( 'NONE', #4390, #72297 ) ;
#67159 = FACE_OUTER_BOUND ( 'NONE', #37572, .T. ) ;
#67160 = EDGE_LOOP ( 'NONE', ( #71247, #9181, #52492, #10911 ) ) ;
#67161 = AXIS2_PLACEMENT_3D ( 'NONE', #28435, #51745, #23186 ) ;
#67162 = VERTEX_POINT ( 'NONE', #34524 ) ;
#67163 = ADVANCED_FACE ( 'NONE', ( #5988 ), #28894, .T. ) ;
#67164 = FACE_OUTER_BOUND ( 'NONE', #1838, .T. ) ;
#67165 = ADVANCED_FACE ( 'NONE', ( #63490 ), #11967, .F. ) ;
#67166 = CARTESIAN_POINT ( 'NONE',  ( -97.65000000000001990, 88.47002178664754979, 79.97229166840095615 ) ) ;
#67167 = CARTESIAN_POINT ( 'NONE',  ( 10.00000000000000000, 0.000000000000000000, 0.000000000000000000 ) ) ;
#67168 = CARTESIAN_POINT ( 'NONE',  ( -92.69370383062498320, -211.3315407142195852, 79.90614583420048689 ) ) ;
#67169 = ORIENTED_EDGE ( 'NONE', *, *, #2702, .T. ) ;
#67170 = DIRECTION ( 'NONE',  ( -1.000000000000000000, 0.000000000000000000, 0.000000000000000000 ) ) ;
#67171 = VERTEX_POINT ( 'NONE', #47658 ) ;
#67172 = VECTOR ( 'NONE', #35701, 1000.000000000000000 ) ;
#67173 = CYLINDRICAL_SURFACE ( 'NONE', #21045, 77.49899999999999523 ) ;
#67174 = AXIS2_PLACEMENT_3D ( 'NONE', #6228, #69000, #58828 ) ;
#67175 = VECTOR ( 'NONE', #50221, 1000.000000000000000 ) ;
#67176 = CARTESIAN_POINT ( 'NONE',  ( -7.543218489614351263, -11.91259227951415056, -1.199999999999999956 ) ) ;
#67177 = CARTESIAN_POINT ( 'NONE',  ( -92.35000000000395914, -210.0000045800647115, 76.42687486209126746 ) ) ;
#67178 = CARTESIAN_POINT ( 'NONE',  ( 97.30629616937498838, 90.00000000000002842, 77.89531250086714920 ) ) ;
#67179 = DIRECTION ( 'NONE',  ( 2.603472992746261562E-14, 2.546204323184492723E-14, -1.000000000000000000 ) ) ;
#67180 = CARTESIAN_POINT ( 'NONE',  ( 10.00000000000000000, 26.08949754953024325, 27.05870788708241648 ) ) ;
#67181 = DIRECTION ( 'NONE',  ( -1.000000000000000000, -0.000000000000000000, -0.000000000000000000 ) ) ;
#67182 = VECTOR ( 'NONE', #41515, 1000.000000000000000 ) ;
#67183 = CARTESIAN_POINT ( 'NONE',  ( 96.73972734126401463, 91.51405112163766375, 74.79348190356853365 ) ) ;
#67184 = AXIS2_PLACEMENT_3D ( 'NONE', #71794, #49979, #43632 ) ;
#67185 = DIRECTION ( 'NONE',  ( 0.000000000000000000, 0.000000000000000000, 1.000000000000000000 ) ) ;
#67186 = DIRECTION ( 'NONE',  ( -0.000000000000000000, -0.000000000000000000, 1.000000000000000000 ) ) ;
#67187 = CARTESIAN_POINT ( 'NONE',  ( 12.00000000000000000, 20.85821328998756385, 10.92862929874494249 ) ) ;
#67188 = CARTESIAN_POINT ( 'NONE',  ( 5.000000000000000000, 32.34446384430010113, -26.79245525562679831 ) ) ;
#67189 = CARTESIAN_POINT ( 'NONE',  ( -92.35000000018069954, 89.99996905681452120, 78.33187387208522523 ) ) ;
#67190 = VERTEX_POINT ( 'NONE', #64965 ) ;
#67191 = CARTESIAN_POINT ( 'NONE',  ( -96.15314808468752972, 91.99731107132950569, 84.45697916753380241 ) ) ;
#67192 = FACE_OUTER_BOUND ( 'NONE', #18974, .T. ) ;
#67193 = FACE_OUTER_BOUND ( 'NONE', #72444, .T. ) ;
#67194 = ADVANCED_FACE ( 'NONE', ( #55145 ), #70564, .T. ) ;
#67195 = ORIENTED_EDGE ( 'NONE', *, *, #24630, .T. ) ;
#67197 = CARTESIAN_POINT ( 'NONE',  ( 0.000000000000000000, -40.65526001592565564, -71.21200624218839437 ) ) ;
#67196 = AXIS2_PLACEMENT_3D ( 'NONE', #19895, #42480, #48111 ) ;
#67198 = CARTESIAN_POINT ( 'NONE',  ( -95.00000000000002842, 90.00000000000004263, 75.00000000000000000 ) ) ;
#67199 = PLANE ( 'NONE',  #43183 ) ;
#67200 = EDGE_CURVE ( 'NONE', #57844, #49855, #30603, .T. ) ;
#67201 = AXIS2_PLACEMENT_3D ( 'NONE', #30912, #59885, #4504 ) ;
#67202 = CARTESIAN_POINT ( 'NONE',  ( -92.34999999999999432, -209.9999999999999716, 84.60249999999999204 ) ) ;
#67203 = CARTESIAN_POINT ( 'NONE',  ( 96.15314808468748708, -208.0026889286704943, 80.06489583420048461 ) ) ;
#67204 = EDGE_CURVE ( 'NONE', #38641, #21124, #40226, .T. ) ;
#67205 = ORIENTED_EDGE ( 'NONE', *, *, #49327, .F. ) ;
#67206 = EDGE_CURVE ( 'NONE', #56916, #35888, #25839, .T. ) ;
#67207 = VERTEX_POINT ( 'NONE', #2209 ) ;
#67208 = CARTESIAN_POINT ( 'NONE',  ( -5.000000000000000000, -2.886751345948134428, -2.080000000000000071 ) ) ;
#67209 = DIRECTION ( 'NONE',  ( -1.000000000000000000, 0.000000000000000000, 0.000000000000000000 ) ) ;
#67210 = DIRECTION ( 'NONE',  ( 0.6064928550163524168, 0.7950889364178788110, -0.000000000000000000 ) ) ;
#67211 = CARTESIAN_POINT ( 'NONE',  ( 97.64999999999999147, -209.9999999999999716, 76.98250000000000171 ) ) ;
#67212 = CYLINDRICAL_SURFACE ( 'NONE', #23710, 16.00000000000000000 ) ;
#67213 = CARTESIAN_POINT ( 'NONE',  ( 92.69370383062501162, -208.6684592857803011, 75.77864583420048916 ) ) ;
#67214 = CIRCLE ( 'NONE', #68420, 16.00000000000000355 ) ;
#67215 = EDGE_CURVE ( 'NONE', #11203, #22660, #834, .T. ) ;
#67216 = ORIENTED_EDGE ( 'NONE', *, *, #29282, .T. ) ;
#67217 = LINE ( 'NONE', #64830, #52749 ) ;
#67218 = ORIENTED_EDGE ( 'NONE', *, *, #70852, .F. ) ;
#67219 = VERTEX_POINT ( 'NONE', #31835 ) ;
#67220 = DIRECTION ( 'NONE',  ( -1.000000000000000000, 0.000000000000000000, 0.000000000000000000 ) ) ;
#67221 = VECTOR ( 'NONE', #39230, 1000.000000000000000 ) ;
#67222 = TOROIDAL_SURFACE ( 'NONE', #46788, 13.10000000000000142, 0.5999999999999998668 ) ;
#67223 = DIRECTION ( 'NONE',  ( -1.000000000000000000, -0.000000000000000000, 0.000000000000000000 ) ) ;
#67224 = AXIS2_PLACEMENT_3D ( 'NONE', #36518, #65484, #14330 ) ;
#67225 = ORIENTED_EDGE ( 'NONE', *, *, #18099, .T. ) ;
#67226 = CARTESIAN_POINT ( 'NONE',  ( 5.000000000000000000, -51.29473840253177741, -63.97538442413482329 ) ) ;
#67227 = CARTESIAN_POINT ( 'NONE',  ( 96.32499999999998863, -212.2949673200287179, 78.86104166840097207 ) ) ;
#67229 = CIRCLE ( 'NONE', #44370, 12.49999999999999645 ) ;
#67228 = CARTESIAN_POINT ( 'NONE',  ( 92.34999999999999432, 88.47002178664753558, 80.52791666666665549 ) ) ;
#67230 = ORIENTED_EDGE ( 'NONE', *, *, #69590, .T. ) ;
#67231 = PLANE ( 'NONE',  #52747 ) ;
#67232 = ORIENTED_EDGE ( 'NONE', *, *, #30457, .T. ) ;
#67233 = CARTESIAN_POINT ( 'NONE',  ( -93.14543241548911112, -211.3788240028428618, 74.79348190356847681 ) ) ;
#67234 = EDGE_CURVE ( 'NONE', #65491, #57151, #20571, .T. ) ;
#67235 = VERTEX_POINT ( 'NONE', #14923 ) ;
#67236 = CARTESIAN_POINT ( 'NONE',  ( 96.32499999999997442, 92.29496732002878900, 84.15270833506762926 ) ) ;
#67237 =( BOUNDED_CURVE ( )  B_SPLINE_CURVE ( 2, ( #62572, #50134, #61069, #11054, #20838, #9562, #67072 ),
 .UNSPECIFIED., .F., .F. ) 
 B_SPLINE_CURVE_WITH_KNOTS ( ( 3, 2, 2, 3 ),
 ( 0.9101937466091534201, 0.9172495203147084109, 0.9243052858555913520, 0.9313609857393206903 ),
 .UNSPECIFIED. ) 
 CURVE ( )  GEOMETRIC_REPRESENTATION_ITEM ( )  RATIONAL_B_SPLINE_CURVE ( ( 1.000000000000000000, 0.8660254037844387076, 1.000000000000000000, 0.8660254037844387076, 1.000000000000000000, 0.8660266504798650455, 0.9999975066323494310 ) ) 
 REPRESENTATION_ITEM ( '' )  );
#67238 = CARTESIAN_POINT ( 'NONE',  ( -95.00000000000002842, 92.66308142843932671, 84.56281250086716739 ) ) ;
#67239 = CARTESIAN_POINT ( 'NONE',  ( 93.84685191531248449, 91.99731107132950569, 78.74197916753381321 ) ) ;
#67240 = EDGE_CURVE ( 'NONE', #26872, #34723, #33021, .T. ) ;
#67241 = VERTEX_POINT ( 'NONE', #9281 ) ;
#67242 = DIRECTION ( 'NONE',  ( -1.000000000000000000, 0.000000000000000000, -0.000000000000000000 ) ) ;
#67243 = LINE ( 'NONE', #51427, #55289 ) ;
#67244 = ORIENTED_EDGE ( 'NONE', *, *, #13418, .F. ) ;
#67245 = DIRECTION ( 'NONE',  ( -0.6516173805718079581, 0.7585478161175704948, 0.000000000000000000 ) ) ;
#67246 = EDGE_CURVE ( 'NONE', #45326, #33698, #48395, .T. ) ;
#67247 = EDGE_CURVE ( 'NONE', #13514, #10345, #19448, .T. ) ;
#67248 = CARTESIAN_POINT ( 'NONE',  ( -92.69370383062498320, -211.3315407142195852, 81.65239583420049030 ) ) ;
#67249 = ORIENTED_EDGE ( 'NONE', *, *, #20644, .F. ) ;
#67250 = ORIENTED_EDGE ( 'NONE', *, *, #68867, .F. ) ;
#67251 = CARTESIAN_POINT ( 'NONE',  ( 0.000000000000000000, 40.65526001592612459, 71.21200624218811015 ) ) ;
#67252 = ORIENTED_EDGE ( 'NONE', *, *, #18098, .T. ) ;
#67253 = EDGE_CURVE ( 'NONE', #3617, #37865, #13444, .T. ) ;
#67254 = CARTESIAN_POINT ( 'NONE',  ( 1.499592026101426168, -120.0349822133818094, 2.500000000000000000 ) ) ;
#67255 = CARTESIAN_POINT ( 'NONE',  ( 94.99999999999998579, 86.94004357329500010, 88.33312500173428816 ) ) ;
#67256 = ORIENTED_EDGE ( 'NONE', *, *, #16964, .T. ) ;
#67257 = CARTESIAN_POINT ( 'NONE',  ( -96.15314808468747287, -208.0026889286704943, 79.37697916753380412 ) ) ;
#67258 = ORIENTED_EDGE ( 'NONE', *, *, #48973, .F. ) ;
#67259 = VECTOR ( 'NONE', #74140, 1000.000000000000114 ) ;
#67260 = CARTESIAN_POINT ( 'NONE',  ( 92.34999999999999432, 91.52997821335252127, 88.75645833506762017 ) ) ;
#67261 = DIRECTION ( 'NONE',  ( -1.000000000000000000, 0.000000000000000000, -0.000000000000000000 ) ) ;
#67262 = DIRECTION ( 'NONE',  ( -0.000000000000000000, -0.000000000000000000, 1.000000000000000000 ) ) ;
#67263 = CARTESIAN_POINT ( 'NONE',  ( 0.000000000000000000, 0.000000000000000000, 0.000000000000000000 ) ) ;
#67264 = EDGE_CURVE ( 'NONE', #24766, #46530, #67864, .T. ) ;
#67265 = AXIS2_PLACEMENT_3D ( 'NONE', #1301, #69302, #12521 ) ;
#67266 = DIRECTION ( 'NONE',  ( 0.000000000000000000, 0.7604059656000276002, 0.6494480483301876550 ) ) ;
#67267 = AXIS2_PLACEMENT_3D ( 'NONE', #60081, #21680, #44252 ) ;
#67268 = DIRECTION ( 'NONE',  ( -1.000000000000000000, -0.000000000000000000, -0.000000000000000000 ) ) ;
#67270 = CARTESIAN_POINT ( 'NONE',  ( 96.15314808468748708, 91.99731107132950569, 89.43114583420047836 ) ) ;
#67269 = VECTOR ( 'NONE', #13866, 999.9999999999998863 ) ;
#67271 = FACE_OUTER_BOUND ( 'NONE', #71324, .T. ) ;
#67272 = CARTESIAN_POINT ( 'NONE',  ( 11.41210121379328335, -99.40233154247455616, 5.500000000000000000 ) ) ;
#67273 = DIRECTION ( 'NONE',  ( -1.000000000000000000, 0.000000000000000000, -0.000000000000000000 ) ) ;
#67274 = CARTESIAN_POINT ( 'NONE',  ( 19.29194287201271507, -133.5026271600380880, -2.500000000000000000 ) ) ;
#67275 = DIRECTION ( 'NONE',  ( 0.000000000000000000, 0.000000000000000000, 1.000000000000000000 ) ) ;
#67276 = FACE_OUTER_BOUND ( 'NONE', #68654, .T. ) ;
#67277 = CARTESIAN_POINT ( 'NONE',  ( 11.99999999999999822, 0.000000000000000000, 0.000000000000000000 ) ) ;
#67278 = DIRECTION ( 'NONE',  ( 1.000000000000000000, -0.000000000000000000, -0.000000000000000000 ) ) ;
#67279 = CIRCLE ( 'NONE', #93, 16.00000000000000000 ) ;
#67280 = LINE ( 'NONE', #15774, #23325 ) ;
#67281 = AXIS2_PLACEMENT_3D ( 'NONE', #36443, #2281, #59761 ) ;
#67282 = DIRECTION ( 'NONE',  ( 0.000000000000000000, 0.000000000000000000, 1.000000000000000000 ) ) ;
#67283 = CARTESIAN_POINT ( 'NONE',  ( -93.67499999999998295, -212.2949673200287179, 85.76666666666665151 ) ) ;
#67284 = AXIS2_PLACEMENT_3D ( 'NONE', #69697, #47869, #13652 ) ;
#67285 = AXIS2_PLACEMENT_3D ( 'NONE', #16622, #6103, #39561 ) ;
#67286 = DIRECTION ( 'NONE',  ( 1.000000000000000000, 0.000000000000000000, 0.000000000000000000 ) ) ;
#67287 = LINE ( 'NONE', #15784, #49147 ) ;
#67288 = DIRECTION ( 'NONE',  ( 2.603472992746261562E-14, 2.546204323184492723E-14, -1.000000000000000000 ) ) ;
#67289 = CARTESIAN_POINT ( 'NONE',  ( 97.64999999999999147, -209.9999999999999716, 77.61749999999999261 ) ) ;
#67290 = DIRECTION ( 'NONE',  ( -1.000000000000000000, 0.000000000000000000, 0.000000000000000000 ) ) ;
#67291 = EDGE_CURVE ( 'NONE', #1038, #56786, #29422, .T. ) ;
#67292 = CARTESIAN_POINT ( 'NONE',  ( 96.15314808468750130, -211.9973110713294489, 89.37822916753381719 ) ) ;
#67293 = EDGE_CURVE ( 'NONE', #14612, #23771, #40563, .T. ) ;
#67294 = ORIENTED_EDGE ( 'NONE', *, *, #55783, .F. ) ;
#67295 = EDGE_CURVE ( 'NONE', #12759, #56516, #16235, .T. ) ;
#67296 = ORIENTED_EDGE ( 'NONE', *, *, #41071, .F. ) ;
#67297 = EDGE_CURVE ( 'NONE', #51292, #63103, #36677, .T. ) ;
#67298 = DIRECTION ( 'NONE',  ( -1.000000000000000000, 0.000000000000000000, 0.000000000000000000 ) ) ;
#67299 = CARTESIAN_POINT ( 'NONE',  ( -12.49999999999999645, 0.000000000000000000, 20.00000000000000000 ) ) ;
#67300 = ORIENTED_EDGE ( 'NONE', *, *, #9193, .F. ) ;
#67301 = CARTESIAN_POINT ( 'NONE',  ( 97.30629616937498838, -211.3315407142195852, 79.11239583420046984 ) ) ;
#67302 = CARTESIAN_POINT ( 'NONE',  ( 97.30629616937498838, -211.3315407142195852, 85.62114583420047609 ) ) ;
#67303 = EDGE_LOOP ( 'NONE', ( #39552, #24538, #26335, #34768 ) ) ;
#67304 = CARTESIAN_POINT ( 'NONE',  ( 93.84685191531249870, -208.0026889286704943, 85.25072916753381946 ) ) ;
#67305 = CIRCLE ( 'NONE', #32471, 31.99999999999998579 ) ;
#67306 = ORIENTED_EDGE ( 'NONE', *, *, #14772, .F. ) ;
#67307 = DIRECTION ( 'NONE',  ( 0.000000000000000000, 0.000000000000000000, 1.000000000000000000 ) ) ;
#67308 = VERTEX_POINT ( 'NONE', #14552 ) ;
#67309 = PRESENTATION_STYLE_ASSIGNMENT (( #68052 ) ) ;
#67310 = EDGE_LOOP ( 'NONE', ( #63006, #29588, #52542, #9504 ) ) ;
#67311 = CARTESIAN_POINT ( 'NONE',  ( 0.000000000000000000, -80.28980883073769803, 16.65972982744906261 ) ) ;
#67312 = ORIENTED_EDGE ( 'NONE', *, *, #15730, .F. ) ;
#67313 = CARTESIAN_POINT ( 'NONE',  ( -10.00000000000000000, 0.000000000000000000, 0.000000000000000000 ) ) ;
#67314 = CARTESIAN_POINT ( 'NONE',  ( 93.67500000000001137, -212.2949673200287179, 88.91520833506763211 ) ) ;
#67315 = ADVANCED_FACE ( 'NONE', ( #59312 ), #7807, .T. ) ;
#67316 = ORIENTED_EDGE ( 'NONE', *, *, #20092, .F. ) ;
#67317 = DIRECTION ( 'NONE',  ( 1.000000000000000000, -0.000000000000000000, -0.000000000000000000 ) ) ;
#67318 = ORIENTED_EDGE ( 'NONE', *, *, #616, .F. ) ;
#67319 = DIRECTION ( 'NONE',  ( -1.000000000000000000, -0.000000000000000000, 0.000000000000000000 ) ) ;
#67320 = ORIENTED_EDGE ( 'NONE', *, *, #16762, .T. ) ;
#67321 = ORIENTED_EDGE ( 'NONE', *, *, #17552, .T. ) ;
#67322 = ORIENTED_EDGE ( 'NONE', *, *, #52822, .F. ) ;
#67323 = CARTESIAN_POINT ( 'NONE',  ( 10.00000000000000000, 0.000000000000000000, 0.000000000000000000 ) ) ;
#67324 = AXIS2_PLACEMENT_3D ( 'NONE', #53200, #1738, #12231 ) ;
#67325 = EDGE_CURVE ( 'NONE', #47328, #34710, #53486, .T. ) ;
#67326 = ADVANCED_FACE ( 'NONE', ( #32201 ), #55894, .F. ) ;
#67327 = DIRECTION ( 'NONE',  ( 0.000000000000000000, 0.000000000000000000, -1.000000000000000000 ) ) ;
#67328 = ORIENTED_EDGE ( 'NONE', *, *, #4074, .F. ) ;
#67329 = AXIS2_PLACEMENT_3D ( 'NONE', #33778, #27380, #55595 ) ;
#67330 = ORIENTED_EDGE ( 'NONE', *, *, #1893, .F. ) ;
#67331 = VERTEX_POINT ( 'NONE', #21289 ) ;
#67332 = CARTESIAN_POINT ( 'NONE',  ( -26.29030328629083968, -123.6496510949466341, 5.500000000000000000 ) ) ;
#67333 = VECTOR ( 'NONE', #14940, 1000.000000000000000 ) ;
#67334 = DIRECTION ( 'NONE',  ( -1.000000000000000000, 0.000000000000000000, 0.000000000000000000 ) ) ;
#67335 = CARTESIAN_POINT ( 'NONE',  ( -93.67500000000003979, 92.29496732002878900, 89.78833333333332689 ) ) ;
#67336 = ORIENTED_EDGE ( 'NONE', *, *, #16990, .T. ) ;
#67337 = CARTESIAN_POINT ( 'NONE',  ( 97.30629616937498838, 88.66845928578037217, 78.47739583420047893 ) ) ;
#67338 = ORIENTED_EDGE ( 'NONE', *, *, #57672, .T. ) ;
#67339 = CARTESIAN_POINT ( 'NONE',  ( 97.64999999981932888, 89.99996905681224746, 78.33187387208513996 ) ) ;
#67340 = CARTESIAN_POINT ( 'NONE',  ( -93.84685191531248449, -208.0026889286704943, 88.16114583420046813 ) ) ;
#67341 = ORIENTED_EDGE ( 'NONE', *, *, #3316, .F. ) ;
#67342 = CARTESIAN_POINT ( 'NONE',  ( 4.829002333675111558, -2.985476894631607259, -1.879366290983715881 ) ) ;
#67343 = CARTESIAN_POINT ( 'NONE',  ( 0.000000000000000000, -5.202137450156129717, -37.22597642581163768 ) ) ;
#67344 = CARTESIAN_POINT ( 'NONE',  ( 92.35000000019410038, 89.99998015720535705, 86.27002759516707897 ) ) ;
#67345 = CARTESIAN_POINT ( 'NONE',  ( -92.69370383062498320, -208.6684592857803295, 81.12322916753380753 ) ) ;
#67346 = CARTESIAN_POINT ( 'NONE',  ( 0.000000000000000000, 0.000000000000000000, 0.000000000000000000 ) ) ;
#67347 = CARTESIAN_POINT ( 'NONE',  ( -23.97194136764370498, -131.3950000906648938, 5.500000000000000000 ) ) ;
#67348 = DIRECTION ( 'NONE',  ( -1.000000000000000000, -0.000000000000000000, 0.000000000000000000 ) ) ;
#67349 = ORIENTED_EDGE ( 'NONE', *, *, #64410, .F. ) ;
#67350 = ORIENTED_EDGE ( 'NONE', *, *, #55264, .T. ) ;
#67351 = CYLINDRICAL_SURFACE ( 'NONE', #16832, 42.00000000000000000 ) ;
#67352 = CYLINDRICAL_SURFACE ( 'NONE', #14730, 16.00000000000000000 ) ;
#67353 = CARTESIAN_POINT ( 'NONE',  ( 95.99319914654141428, -207.8660161998918454, 74.81432998548488911 ) ) ;
#67354 = CARTESIAN_POINT ( 'NONE',  ( -92.69370383062504004, 90.00000000000004263, 80.43531250086714124 ) ) ;
#67355 = DIRECTION ( 'NONE',  ( 0.000000000000000000, 0.000000000000000000, 1.000000000000000000 ) ) ;
#67356 = FACE_OUTER_BOUND ( 'NONE', #59182, .T. ) ;
#67357 = ORIENTED_EDGE ( 'NONE', *, *, #62949, .T. ) ;
#67358 = CARTESIAN_POINT ( 'NONE',  ( 5.000000000000002665, -80.28980883073769803, 16.65972982744906261 ) ) ;
#67359 = CIRCLE ( 'NONE', #60138, 77.49899999999999523 ) ;
#67360 = VECTOR ( 'NONE', #14060, 1000.000000000000000 ) ;
#67361 = CIRCLE ( 'NONE', #33772, 31.99999999999999289 ) ;
#67362 = CARTESIAN_POINT ( 'NONE',  ( -12.00000000000000000, 0.000000000000000000, -17.30399999999999849 ) ) ;
#67363 = DIRECTION ( 'NONE',  ( 0.000000000000000000, 0.9510565162951543083, 0.3090169943749449533 ) ) ;
#67364 = FACE_OUTER_BOUND ( 'NONE', #64827, .T. ) ;
#67365 = CARTESIAN_POINT ( 'NONE',  ( 15.00000000000000000, -1.278221433540507546, -26.51162292216071492 ) ) ;
#67366 = CARTESIAN_POINT ( 'NONE',  ( -92.69370383062498320, -211.3315407142195852, 78.63614583420049087 ) ) ;
#67367 = CYLINDRICAL_SURFACE ( 'NONE', #70075, 31.99999999999998579 ) ;
#67368 = ORIENTED_EDGE ( 'NONE', *, *, #37034, .T. ) ;
#67369 = CARTESIAN_POINT ( 'NONE',  ( 11.99999999999999822, -20.41045688087772092, -72.35160999960838524 ) ) ;
#67370 = EDGE_CURVE ( 'NONE', #7767, #29135, #72263, .T. ) ;
#67371 = CARTESIAN_POINT ( 'NONE',  ( -97.65000000000001990, 90.00000000000004263, 88.73000000000000398 ) ) ;
#67372 = LINE ( 'NONE', #11336, #29758 ) ;
#67373 = ORIENTED_EDGE ( 'NONE', *, *, #41029, .T. ) ;
#67374 = DIRECTION ( 'NONE',  ( 0.000000000000000000, 0.000000000000000000, 1.000000000000000000 ) ) ;
#67376 = EDGE_CURVE ( 'NONE', #7618, #50553, #73172, .T. ) ;
#67375 = LINE ( 'NONE', #40950, #57035 ) ;
#67377 = CIRCLE ( 'NONE', #36201, 31.99999999999999289 ) ;
#67378 = CIRCLE ( 'NONE', #37409, 31.99999999999999645 ) ;
#67379 = ADVANCED_FACE ( 'NONE', ( #22428 ), #69113, .F. ) ;
#67380 = AXIS2_PLACEMENT_3D ( 'NONE', #63415, #5908, #52115 ) ;
#67381 = DIRECTION ( 'NONE',  ( 1.000000000000000000, 1.427937372958405461E-15, 7.962523111839130290E-16 ) ) ;
#67382 = VERTEX_POINT ( 'NONE', #10772 ) ;
#67383 = ADVANCED_FACE ( 'NONE', ( #44995 ), #67173, .T. ) ;
#67384 = FACE_OUTER_BOUND ( 'NONE', #38675, .T. ) ;
#67385 = ORIENTED_EDGE ( 'NONE', *, *, #65863, .F. ) ;
#67386 = ADVANCED_FACE ( 'NONE', ( #34071 ), #27691, .T. ) ;
#67387 = CARTESIAN_POINT ( 'NONE',  ( 93.84685191531249870, -208.0026889286704943, 88.26697916753380468 ) ) ;
#67388 = CARTESIAN_POINT ( 'NONE',  ( -92.35000000045951651, -209.9999506483816560, 87.22187670868756015 ) ) ;
#67389 = EDGE_LOOP ( 'NONE', ( #40227, #28862, #29483, #54901 ) ) ;
#67390 = LINE ( 'NONE', #72639, #13838 ) ;
#67391 = ORIENTED_EDGE ( 'NONE', *, *, #7819, .F. ) ;
#67392 = CARTESIAN_POINT ( 'NONE',  ( 11.99999999999999822, -14.66109333815513160, 73.73191006444567108 ) ) ;
#67393 = DIRECTION ( 'NONE',  ( -1.000000000000000000, -0.000000000000000000, 0.000000000000000000 ) ) ;
#67394 = ORIENTED_EDGE ( 'NONE', *, *, #73766, .F. ) ;
#67395 = VERTEX_POINT ( 'NONE', #50993 ) ;
#67396 = VERTEX_POINT ( 'NONE', #15675 ) ;
#67397 = DIRECTION ( 'NONE',  ( -1.000000000000000000, -0.000000000000000000, -0.000000000000000000 ) ) ;
#67398 = ADVANCED_FACE ( 'NONE', ( #68296 ), #45372, .F. ) ;
#67399 = EDGE_CURVE ( 'NONE', #53082, #50665, #5530, .T. ) ;
#67400 = ORIENTED_EDGE ( 'NONE', *, *, #63794, .F. ) ;
#67401 = PRODUCT_DEFINITION_SHAPE ( 'NONE', 'NONE',  #74344 ) ;
#67402 = EDGE_LOOP ( 'NONE', ( #32095, #30787, #21840, #45068 ) ) ;
#67403 = CARTESIAN_POINT ( 'NONE',  ( 94.99999999999998579, 87.33691857156068750, 77.89531250086714920 ) ) ;
#67404 = LINE ( 'NONE', #5389, #11951 ) ;
#67405 = LINE ( 'NONE', #50484, #44101 ) ;
#67406 = ORIENTED_EDGE ( 'NONE', *, *, #73991, .F. ) ;
#67407 = ORIENTED_EDGE ( 'NONE', *, *, #33676, .T. ) ;
#67408 = AXIS2_PLACEMENT_3D ( 'NONE', #14845, #32122, #37791 ) ;
#67409 = AXIS2_PLACEMENT_3D ( 'NONE', #9823, #32741, #49302 ) ;
#67410 = ORIENTED_EDGE ( 'NONE', *, *, #39386, .F. ) ;
#67411 = CARTESIAN_POINT ( 'NONE',  ( 97.30629616937498838, 88.66845928578037217, 88.00239583420047040 ) ) ;
#67412 = CIRCLE ( 'NONE', #10966, 31.99999999999998579 ) ;
#67413 = ORIENTED_EDGE ( 'NONE', *, *, #41582, .T. ) ;
#67414 = CARTESIAN_POINT ( 'NONE',  ( 92.69370383062501162, -209.9999999999999716, 84.56281250086713897 ) ) ;
#67415 = EDGE_CURVE ( 'NONE', #35038, #35410, #26572, .T. ) ;
#67416 = EDGE_CURVE ( 'NONE', #63089, #26612, #15100, .T. ) ;
#67417 = PRODUCT_CONTEXT ( 'NONE', #39750, 'mechanical' ) ;
#67418 = DIRECTION ( 'NONE',  ( -1.000000000000000000, -0.000000000000000000, -0.000000000000000000 ) ) ;
#67419 = DIRECTION ( 'NONE',  ( -0.000000000000000000, -0.000000000000000000, 1.000000000000000000 ) ) ;
#67420 = CARTESIAN_POINT ( 'NONE',  ( 0.000000000000000000, 0.000000000000000000, 0.000000000000000000 ) ) ;
#67421 = DIRECTION ( 'NONE',  ( 0.000000000000000000, -0.000000000000000000, 1.000000000000000000 ) ) ;
#67422 = CARTESIAN_POINT ( 'NONE',  ( 94.99999999999998579, 90.00000000000002842, 90.00000000000000000 ) ) ;
#67423 = DIRECTION ( 'NONE',  ( 0.000000000000000000, 1.000000000000000000, 3.491481338843133750E-15 ) ) ;
#67424 = CARTESIAN_POINT ( 'NONE',  ( -97.30629616937497417, -211.3315407142195852, 89.06072916753379332 ) ) ;
#67425 = CARTESIAN_POINT ( 'NONE',  ( -96.15314808468751551, 88.00268892867056536, 87.36739583420049371 ) ) ;
#67426 = VECTOR ( 'NONE', #1086, 1000.000000000000000 ) ;
#67427 = EDGE_LOOP ( 'NONE', ( #35448, #64353 ) ) ;
#67429 = CARTESIAN_POINT ( 'NONE',  ( -97.30629616937501680, 91.33154071421968467, 89.58989583420047609 ) ) ;
#67428 = CARTESIAN_POINT ( 'NONE',  ( 96.15314808468748708, 88.00268892867053694, 86.67947916753381321 ) ) ;
#67430 = ORIENTED_EDGE ( 'NONE', *, *, #60291, .T. ) ;
#67431 = CARTESIAN_POINT ( 'NONE',  ( 93.67500000000001137, -212.2949673200287179, 84.47020833506762472 ) ) ;
#67432 = CARTESIAN_POINT ( 'NONE',  ( 11.99999999999999822, 26.02418014898407961, -70.52718814184231633 ) ) ;
#67433 = CARTESIAN_POINT ( 'NONE',  ( -23.97194136764370498, -131.3950000906648938, -2.500000000000000444 ) ) ;
#67434 = DIRECTION ( 'NONE',  ( -1.000000000000000000, -0.000000000000000000, -0.000000000000000000 ) ) ;
#67435 = CARTESIAN_POINT ( 'NONE',  ( -93.84685191531248449, -208.0026889286704943, 89.43114583420047836 ) ) ;
#67436 = CARTESIAN_POINT ( 'NONE',  ( -92.34999999999999432, -209.9999999999999716, 82.06250000000000000 ) ) ;
#67437 = DIRECTION ( 'NONE',  ( 0.7533909544171997208, 0.6575728627325955200, 0.000000000000000000 ) ) ;
#67438 = AXIS2_PLACEMENT_3D ( 'NONE', #6071, #56822, #68844 ) ;
#67439 = DIRECTION ( 'NONE',  ( -1.000000000000000000, -0.000000000000000000, -0.000000000000000000 ) ) ;
#67440 = VERTEX_POINT ( 'NONE', #38227 ) ;
#67441 = AXIS2_PLACEMENT_3D ( 'NONE', #21645, #44599, #68644 ) ;
#67442 = VERTEX_POINT ( 'NONE', #61172 ) ;
#67443 = AXIS2_PLACEMENT_3D ( 'NONE', #35474, #24569, #1318 ) ;
#67444 = CARTESIAN_POINT ( 'NONE',  ( -97.65000000000001990, 91.52997821335253548, 80.42208333333331893 ) ) ;
#67445 = FACE_OUTER_BOUND ( 'NONE', #10820, .T. ) ;
#67446 = CARTESIAN_POINT ( 'NONE',  ( 0.000000000000000000, 0.000000000000000000, 0.000000000000000000 ) ) ;
#67447 = LINE ( 'NONE', #33597, #2431 ) ;
#67448 = FACE_BOUND ( 'NONE', #64220, .T. ) ;
#67449 = CARTESIAN_POINT ( 'NONE',  ( 10.00000000000000000, 51.02545421589324803, 55.20638768913779870 ) ) ;
#67450 = DIRECTION ( 'NONE',  ( -0.000000000000000000, -0.000000000000000000, 1.000000000000000000 ) ) ;
#67451 =( BOUNDED_CURVE ( )  B_SPLINE_CURVE ( 2, ( #26443, #38094, #30961, #25342, #71923, #43754, #36983 ),
 .UNSPECIFIED., .F., .F. ) 
 B_SPLINE_CURVE_WITH_KNOTS ( ( 3, 2, 2, 3 ),
 ( 0.3125000000000001665, 0.3194444444444445308, 0.3263888888888890061, 0.3333333333333333703 ),
 .UNSPECIFIED. ) 
 CURVE ( )  GEOMETRIC_REPRESENTATION_ITEM ( )  RATIONAL_B_SPLINE_CURVE ( ( 0.9999999999999967804, 0.8660254037844419273, 1.000000000000000000, 0.8660254037844387076, 1.000000000000000000, 0.8660254037844375974, 1.000000000000001110 ) ) 
 REPRESENTATION_ITEM ( '' )  );
#67452 = CARTESIAN_POINT ( 'NONE',  ( -92.34999999999999432, -208.4700217866474645, 79.57541666666666913 ) ) ;
#67453 = ORIENTED_EDGE ( 'NONE', *, *, #9748, .F. ) ;
#67454 = CARTESIAN_POINT ( 'NONE',  ( -97.30629616937501680, 88.66845928578038638, 81.44072916753381719 ) ) ;
#67455 = DIRECTION ( 'NONE',  ( 1.000000000000000000, -7.571539615859142926E-15, -2.618450529775767079E-14 ) ) ;
#67456 = DIRECTION ( 'NONE',  ( 1.000000000000000000, 0.000000000000000000, 0.000000000000000000 ) ) ;
#67457 = DIRECTION ( 'NONE',  ( 0.000000000000000000, 0.000000000000000000, 1.000000000000000000 ) ) ;
#67458 = DIRECTION ( 'NONE',  ( -1.000000000000000000, 0.000000000000000000, 0.000000000000000000 ) ) ;
#67459 = CYLINDRICAL_SURFACE ( 'NONE', #2960, 16.00000000000000000 ) ;
#67460 = DIRECTION ( 'NONE',  ( -0.000000000000000000, -0.000000000000000000, 1.000000000000000000 ) ) ;
#67461 = EDGE_CURVE ( 'NONE', #34558, #30100, #72667, .T. ) ;
#67462 = ADVANCED_FACE ( 'NONE', ( #32578 ), #55525, .T. ) ;
#67463 = ADVANCED_FACE ( 'NONE', ( #10024 ), #26937, .F. ) ;
#67464 = VECTOR ( 'NONE', #4427, 1000.000000000000114 ) ;
#67465 =( BOUNDED_CURVE ( )  B_SPLINE_CURVE ( 2, ( #9912, #4670, #73800, #33960, #27577, #50506, #21940, #56908, #15181 ),
 .UNSPECIFIED., .F., .F. ) 
 B_SPLINE_CURVE_WITH_KNOTS ( ( 3, 2, 2, 2, 3 ),
 ( 0.5715170088694363493, 0.5785727743551949409, 0.5856285398961110777, 0.5926843054370272146, 0.5926843883826560244 ),
 .UNSPECIFIED. ) 
 CURVE ( )  GEOMETRIC_REPRESENTATION_ITEM ( )  RATIONAL_B_SPLINE_CURVE ( ( 1.000000000000000000, 0.8660254037844387076, 1.000000000000000000, 0.8660254037844387076, 1.000000000000000000, 0.8660254037844387076, 1.000000000000000000, 0.9999984250316910073, 0.9999968501004118382 ) ) 
 REPRESENTATION_ITEM ( '' )  );
#67466 = CARTESIAN_POINT ( 'NONE',  ( 97.30629616937498838, 91.33154071421968467, 80.64697916753382856 ) ) ;
#67467 = EDGE_CURVE ( 'NONE', #30173, #39405, #4289, .T. ) ;
#67468 = CARTESIAN_POINT ( 'NONE',  ( -97.30629616937497417, -211.3315407142195852, 84.13947916753383538 ) ) ;
#67469 = DIRECTION ( 'NONE',  ( 0.000000000000000000, 0.000000000000000000, 1.000000000000000000 ) ) ;
#67470 = EDGE_LOOP ( 'NONE', ( #42027, #72842, #14169, #70717 ) ) ;
#67471 = DIRECTION ( 'NONE',  ( -1.000000000000000000, -0.000000000000000000, -0.000000000000000000 ) ) ;
#67472 = VECTOR ( 'NONE', #65053, 1000.000000000000000 ) ;
#67473 = CARTESIAN_POINT ( 'NONE',  ( -92.34999999999999432, -208.4700217866474645, 78.94041666666666401 ) ) ;
#67474 = DIRECTION ( 'NONE',  ( -1.000000000000000000, -0.000000000000000000, 0.000000000000000000 ) ) ;
#67475 = AXIS2_PLACEMENT_3D ( 'NONE', #26667, #10124, #62396 ) ;
#67476 = EDGE_CURVE ( 'NONE', #18206, #58103, #46299, .T. ) ;
#67477 = CARTESIAN_POINT ( 'NONE',  ( -96.15314808468751551, 88.00268892867056536, 78.47739583420049314 ) ) ;
#67478 = CARTESIAN_POINT ( 'NONE',  ( 92.69370383062501162, -209.9999999999999716, 80.75281250086715090 ) ) ;
#67479 = VERTEX_POINT ( 'NONE', #5891 ) ;
#67480 = AXIS2_PLACEMENT_3D ( 'NONE', #66699, #33584, #21943 ) ;
#67481 = DIRECTION ( 'NONE',  ( 0.000000000000000000, 0.000000000000000000, -1.000000000000000000 ) ) ;
#67482 = VERTEX_POINT ( 'NONE', #35181 ) ;
#67483 = AXIS2_PLACEMENT_3D ( 'NONE', #28762, #249, #23142 ) ;
#67484 = EDGE_CURVE ( 'NONE', #20620, #26097, #58479, .T. ) ;
#67485 = CARTESIAN_POINT ( 'NONE',  ( -96.32499999999996021, -207.7050326799711968, 76.00354166840097037 ) ) ;
#67486 = VERTEX_POINT ( 'NONE', #17156 ) ;
#67487 = AXIS2_PLACEMENT_3D ( 'NONE', #70155, #28462, #74334 ) ;
#67488 = CARTESIAN_POINT ( 'NONE',  ( -7.469491406282116941, 4.756046723998916370, -55.00000000000000000 ) ) ;
#67489 = VECTOR ( 'NONE', #12877, 1000.000000000000114 ) ;
#67490 = ORIENTED_EDGE ( 'NONE', *, *, #19345, .T. ) ;
#67491 = ORIENTED_EDGE ( 'NONE', *, *, #51464, .T. ) ;
#67492 = VERTEX_POINT ( 'NONE', #47207 ) ;
#67493 = CARTESIAN_POINT ( 'NONE',  ( 93.84685191531251292, -211.9973110713294489, 76.57239583420049200 ) ) ;
#67494 = ADVANCED_FACE ( 'NONE', ( #57753 ), #63773, .T. ) ;
#67495 = EDGE_CURVE ( 'NONE', #49393, #39290, #40451, .T. ) ;
#67496 = ORIENTED_EDGE ( 'NONE', *, *, #47466, .T. ) ;
#67497 = DIRECTION ( 'NONE',  ( -1.000000000000000000, 0.000000000000000000, -0.000000000000000000 ) ) ;
#67498 = CARTESIAN_POINT ( 'NONE',  ( 11.99999999999999822, 0.000000000000000000, 0.000000000000000000 ) ) ;
#67499 = CARTESIAN_POINT ( 'NONE',  ( 92.69370383062498320, 88.66845928578037217, 86.04447916753382231 ) ) ;
#67500 = CARTESIAN_POINT ( 'NONE',  ( 10.00000000000000000, 0.000000000000000000, 0.000000000000000000 ) ) ;
#67501 = CARTESIAN_POINT ( 'NONE',  ( 95.00000000000000000, -213.0599564267049857, 78.72875000000001933 ) ) ;
#67502 = ORIENTED_EDGE ( 'NONE', *, *, #63332, .F. ) ;
#67503 = VERTEX_POINT ( 'NONE', #41197 ) ;
#67504 = ORIENTED_EDGE ( 'NONE', *, *, #5810, .T. ) ;
#67505 = ORIENTED_EDGE ( 'NONE', *, *, #42872, .T. ) ;
#67506 = DIRECTION ( 'NONE',  ( 0.000000000000000000, 0.000000000000000000, 1.000000000000000000 ) ) ;
#67507 = FILL_AREA_STYLE_COLOUR ( '', #9936 ) ;
#67508 = DIRECTION ( 'NONE',  ( 0.000000000000000000, -0.5877852522924691403, 0.8090169943749504489 ) ) ;
#67509 = DIRECTION ( 'NONE',  ( 0.000000000000000000, 0.000000000000000000, 1.000000000000000000 ) ) ;
#67510 = LINE ( 'NONE', #73880, #28230 ) ;
#67511 = DIRECTION ( 'NONE',  ( 0.3853207896976523772, -0.9227826878668550226, 0.000000000000000000 ) ) ;
#67512 = FACE_OUTER_BOUND ( 'NONE', #43386, .T. ) ;
#67513 = EDGE_LOOP ( 'NONE', ( #39506, #66210, #20216, #68753 ) ) ;
#67514 = CARTESIAN_POINT ( 'NONE',  ( -96.32499999999996021, -207.7050326799711968, 82.35354166840096468 ) ) ;
#67515 = ORIENTED_EDGE ( 'NONE', *, *, #46196, .F. ) ;
#67516 = CARTESIAN_POINT ( 'NONE',  ( 10.00000000000000000, 0.000000000000000000, 0.000000000000000000 ) ) ;
#67517 = EDGE_LOOP ( 'NONE', ( #47994, #58940 ) ) ;
#67519 = CARTESIAN_POINT ( 'NONE',  ( -96.32500000000001705, 92.29496732002878900, 82.98854166840096980 ) ) ;
#67518 = CARTESIAN_POINT ( 'NONE',  ( 96.32499999999997442, 92.29496732002878900, 84.15270833506762926 ) ) ;
#67520 = ORIENTED_EDGE ( 'NONE', *, *, #74108, .F. ) ;
#67521 = CARTESIAN_POINT ( 'NONE',  ( 92.69370383062498320, 91.33154071421968467, 84.03364583420049883 ) ) ;
#67522 = LINE ( 'NONE', #11485, #26217 ) ;
#67523 = CARTESIAN_POINT ( 'NONE',  ( -97.64999999999996305, -211.5299782133524218, 82.51229166840094820 ) ) ;
#67524 = DIRECTION ( 'NONE',  ( 0.000000000000000000, 0.000000000000000000, 1.000000000000000000 ) ) ;
#67525 = DIRECTION ( 'NONE',  ( 0.000000000000000000, 0.000000000000000000, 1.000000000000000000 ) ) ;
#67526 = PRESENTATION_LAYER_ASSIGNMENT (  '', '', ( #1501 ) ) ;
#67527 = DIRECTION ( 'NONE',  ( -1.000000000000000000, -1.343011723336883198E-16, -0.000000000000000000 ) ) ;
#67528 = ORIENTED_EDGE ( 'NONE', *, *, #30702, .F. ) ;
#67529 = DIRECTION ( 'NONE',  ( -1.000000000000000000, -0.000000000000000000, -0.000000000000000000 ) ) ;
#67530 = CARTESIAN_POINT ( 'NONE',  ( 10.00000000000000000, 0.000000000000000000, 0.000000000000000000 ) ) ;
#67531 = DIRECTION ( 'NONE',  ( 0.000000000000000000, 1.000000000000000000, 3.491481338843133750E-15 ) ) ;
#67532 = ORIENTED_EDGE ( 'NONE', *, *, #41261, .F. ) ;
#67533 = CIRCLE ( 'NONE', #57931, 31.99999999999998579 ) ;
#67534 = ORIENTED_EDGE ( 'NONE', *, *, #51914, .F. ) ;
#67536 = EDGE_CURVE ( 'NONE', #22824, #6493, #73922, .T. ) ;
#67535 = CIRCLE ( 'NONE', #6315, 12.49999999999999822 ) ;
#67537 = CARTESIAN_POINT ( 'NONE',  ( 97.64999999999999147, -209.9999999999999716, 90.00000000000000000 ) ) ;
#67538 = DIRECTION ( 'NONE',  ( -1.000000000000000000, -0.000000000000000000, -0.000000000000000000 ) ) ;
#67539 = CARTESIAN_POINT ( 'NONE',  ( 10.00000000000000000, 0.000000000000000000, 0.000000000000000000 ) ) ;
#67540 = VECTOR ( 'NONE', #24346, 1000.000000000000000 ) ;
#67541 = CARTESIAN_POINT ( 'NONE',  ( -94.99999999999997158, -207.3369185715606307, 79.48281250086715488 ) ) ;
#67542 = ORIENTED_EDGE ( 'NONE', *, *, #28883, .F. ) ;
#67543 = CARTESIAN_POINT ( 'NONE',  ( 11.99999999999999822, 0.000000000000000000, 0.000000000000000000 ) ) ;
#67544 = ORIENTED_EDGE ( 'NONE', *, *, #38968, .F. ) ;
#67545 = CARTESIAN_POINT ( 'NONE',  ( -97.64999999953586496, -210.0000309672219601, 77.38038495123339544 ) ) ;
#67546 = AXIS2_PLACEMENT_3D ( 'NONE', #49774, #53396, #11056 ) ;
#67547 = CIRCLE ( 'NONE', #53162, 16.00000000000000000 ) ;
#67548 = FACE_BOUND ( 'NONE', #72096, .T. ) ;
#67549 = CARTESIAN_POINT ( 'NONE',  ( 10.00000000000000000, 8.830959090342393125, 74.65491531819122883 ) ) ;
#67550 = CARTESIAN_POINT ( 'NONE',  ( 97.30629616937498838, 91.33154071421968467, 76.04322916753380923 ) ) ;
#67551 = LINE ( 'NONE', #27696, #60464 ) ;
#67552 = CARTESIAN_POINT ( 'NONE',  ( 5.000000000000000000, -31.52238457039619490, 27.75498641678731104 ) ) ;
#67553 = EDGE_CURVE ( 'NONE', #65977, #27241, #30658, .T. ) ;
#67554 = FACE_OUTER_BOUND ( 'NONE', #414, .T. ) ;
#67555 = CARTESIAN_POINT ( 'NONE',  ( -90.00000000000002842, 95.00000000000002842, -79.99999999999998579 ) ) ;
#67556 = DIRECTION ( 'NONE',  ( 1.000000000000000000, 0.000000000000000000, 0.000000000000000000 ) ) ;
#67557 = ADVANCED_FACE ( 'NONE', ( #40089 ), #51356, .T. ) ;
#67558 = DIRECTION ( 'NONE',  ( 1.000000000000000000, 0.000000000000000000, 0.000000000000000000 ) ) ;
#67559 = CYLINDRICAL_SURFACE ( 'NONE', #28801, 31.99999999999998579 ) ;
#67560 = DIRECTION ( 'NONE',  ( -1.000000000000000000, -0.000000000000000000, -0.000000000000000000 ) ) ;
#67561 = EDGE_CURVE ( 'NONE', #73369, #68357, #41507, .T. ) ;
#67562 = DIRECTION ( 'NONE',  ( 0.000000000000000000, 0.000000000000000000, 1.000000000000000000 ) ) ;
#67563 = CARTESIAN_POINT ( 'NONE',  ( -93.67500000000003979, 87.70503267997129626, 78.22604166840096696 ) ) ;
#67564 = ORIENTED_EDGE ( 'NONE', *, *, #73427, .T. ) ;
#67565 = EDGE_CURVE ( 'NONE', #21247, #63634, #24280, .T. ) ;
#67566 = CARTESIAN_POINT ( 'NONE',  ( -95.00000000000002842, 87.33691857156074434, 84.08656250086714579 ) ) ;
#67567 = LINE ( 'NONE', #58841, #69571 ) ;
#67568 = CARTESIAN_POINT ( 'NONE',  ( -97.65000000000001990, 90.00000000000004263, 90.00000000000000000 ) ) ;
#67569 = VERTEX_POINT ( 'NONE', #34434 ) ;
#67570 = CARTESIAN_POINT ( 'NONE',  ( 94.99999999999998579, 90.00000000000002842, 90.00000000000000000 ) ) ;
#67571 = DIRECTION ( 'NONE',  ( 1.000000000000000000, 0.000000000000000000, 0.000000000000000000 ) ) ;
#67572 = EDGE_CURVE ( 'NONE', #72495, #2787, #60738, .T. ) ;
#67573 = DIRECTION ( 'NONE',  ( 0.000000000000000000, 0.000000000000000000, 1.000000000000000000 ) ) ;
#67574 = DIRECTION ( 'NONE',  ( -1.000000000000000000, 0.000000000000000000, 0.000000000000000000 ) ) ;
#67575 = CARTESIAN_POINT ( 'NONE',  ( 93.84685191531251292, -211.9973110713294489, 79.11239583420048405 ) ) ;
#67576 = AXIS2_PLACEMENT_3D ( 'NONE', #31712, #57318, #23117 ) ;
#67577 = ORIENTED_EDGE ( 'NONE', *, *, #64264, .T. ) ;
#67579 = ORIENTED_EDGE ( 'NONE', *, *, #16530, .T. ) ;
#67578 =( BOUNDED_CURVE ( )  B_SPLINE_CURVE ( 2, ( #7274, #35822, #7635, #64791, #1670, #63691, #24923, #70777, #35103 ),
 .UNSPECIFIED., .F., .F. ) 
 B_SPLINE_CURVE_WITH_KNOTS ( ( 3, 2, 2, 2, 3 ),
 ( 0.3386766260338262002, 0.3386767459623536425, 0.3457325115032360840, 0.3527882770441184701, 0.3598440426530883918 ),
 .UNSPECIFIED. ) 
 CURVE ( )  GEOMETRIC_REPRESENTATION_ITEM ( )  RATIONAL_B_SPLINE_CURVE ( ( 0.9999954456811690484, 0.9999977228018784858, 1.000000000000000000, 0.8660254037844387076, 1.000000000000000000, 0.8660254037844387076, 1.000000000000000000, 0.8660254037844387076, 1.000000000000000000 ) ) 
 REPRESENTATION_ITEM ( '' )  );
#67580 = EDGE_CURVE ( 'NONE', #10345, #34939, #66685, .T. ) ;
#67581 = ADVANCED_FACE ( 'NONE', ( #23905 ), #69034, .T. ) ;
#67582 = CARTESIAN_POINT ( 'NONE',  ( 96.73972734126404305, -208.4859488783623362, 74.79348190356850523 ) ) ;
#67583 = CARTESIAN_POINT ( 'NONE',  ( -92.35000000000003695, 90.00000000000004263, 90.00000000000000000 ) ) ;
#67584 = FACE_OUTER_BOUND ( 'NONE', #10536, .T. ) ;
#67585 = DIRECTION ( 'NONE',  ( -1.000000000000000000, 0.000000000000000000, 0.000000000000000000 ) ) ;
#67586 = EDGE_CURVE ( 'NONE', #60556, #62067, #49872, .T. ) ;
#67587 = DIRECTION ( 'NONE',  ( 1.000000000000000000, 0.000000000000000000, 0.000000000000000000 ) ) ;
#67588 = CARTESIAN_POINT ( 'NONE',  ( 93.67500000000001137, -207.7050326799711968, 87.35416666666665719 ) ) ;
#67589 = ORIENTED_EDGE ( 'NONE', *, *, #63025, .F. ) ;
#67590 = DIRECTION ( 'NONE',  ( 1.000000000000000000, 0.000000000000000000, 0.000000000000000000 ) ) ;
#67591 = ORIENTED_EDGE ( 'NONE', *, *, #46496, .T. ) ;
#67592 = AXIS2_PLACEMENT_3D ( 'NONE', #36749, #32206, #38233 ) ;
#67593 = ORIENTED_EDGE ( 'NONE', *, *, #27792, .F. ) ;
#67594 = LINE ( 'NONE', #27353, #28547 ) ;
#67595 = CIRCLE ( 'NONE', #35183, 37.49900000000000233 ) ;
#67596 = CARTESIAN_POINT ( 'NONE',  ( 26.50000000000000355, -120.0000000000000000, -64.00000000000000000 ) ) ;
#67597 = ORIENTED_EDGE ( 'NONE', *, *, #33870, .T. ) ;
#67598 = DIRECTION ( 'NONE',  ( 0.000000000000000000, -0.4999999999999995559, 0.8660254037844389297 ) ) ;
#67599 = CARTESIAN_POINT ( 'NONE',  ( 97.64999999999997726, -208.4700217866474645, 80.28979166840098003 ) ) ;
#67600 = CARTESIAN_POINT ( 'NONE',  ( 93.67499999999999716, 87.70503267997126784, 82.48583333333333201 ) ) ;
#67601 = ORIENTED_EDGE ( 'NONE', *, *, #18426, .F. ) ;
#67602 = CARTESIAN_POINT ( 'NONE',  ( 1.250000000000000000, -12.36245420541525597, 0.000000000000000000 ) ) ;
#67603 = EDGE_LOOP ( 'NONE', ( #3883, #63799, #52966, #8598, #70645 ) ) ;
#67604 = CARTESIAN_POINT ( 'NONE',  ( -92.34999999999999432, -208.4700217866474645, 82.82979166840095786 ) ) ;
#67605 = ORIENTED_EDGE ( 'NONE', *, *, #33731, .F. ) ;
#67606 = CARTESIAN_POINT ( 'NONE',  ( 11.99999999999999822, 0.000000000000000000, 0.000000000000000000 ) ) ;
#67607 = CARTESIAN_POINT ( 'NONE',  ( -95.00000000000002842, 92.66308142843932671, 85.19781250086714408 ) ) ;
#67608 = CARTESIAN_POINT ( 'NONE',  ( 92.69370383062498320, 88.66845928578037217, 79.53572916753380184 ) ) ;
#67609 = ORIENTED_EDGE ( 'NONE', *, *, #57075, .F. ) ;
#67610 = DIRECTION ( 'NONE',  ( 0.000000000000000000, 0.000000000000000000, 1.000000000000000000 ) ) ;
#67611 = DIRECTION ( 'NONE',  ( 0.7950889364178798102, -0.6064928550163511956, 0.000000000000000000 ) ) ;
#67612 = CARTESIAN_POINT ( 'NONE',  ( 11.99999999999999822, -41.19522573413689059, -65.64334221924951862 ) ) ;
#67613 = DIRECTION ( 'NONE',  ( 2.603472992746261562E-14, 2.546204323184492723E-14, -1.000000000000000000 ) ) ;
#67614 = EDGE_LOOP ( 'NONE', ( #14768, #25149, #55113, #44663 ) ) ;
#67615 = DIRECTION ( 'NONE',  ( 0.000000000000000000, 0.000000000000000000, 1.000000000000000000 ) ) ;
#67616 = CARTESIAN_POINT ( 'NONE',  ( -92.69370383062498320, -208.6684592857803011, 80.48822916753383083 ) ) ;
#67617 = VERTEX_POINT ( 'NONE', #51736 ) ;
#67618 = ORIENTED_EDGE ( 'NONE', *, *, #11716, .F. ) ;
#67619 = DIRECTION ( 'NONE',  ( -1.000000000000000000, 0.000000000000000000, 0.000000000000000000 ) ) ;
#67620 = ORIENTED_EDGE ( 'NONE', *, *, #38020, .T. ) ;
#67621 = CYLINDRICAL_SURFACE ( 'NONE', #59997, 2.649999999999985700 ) ;
#67622 =( REPRESENTATION_RELATIONSHIP ('NONE','NONE', #31117, #66992 ) REPRESENTATION_RELATIONSHIP_WITH_TRANSFORMATION ( #29395 )SHAPE_REPRESENTATION_RELATIONSHIP( ) );
#67623 = AXIS2_PLACEMENT_3D ( 'NONE', #69768, #45382, #11157 ) ;
#67624 = ADVANCED_FACE ( 'NONE', ( #18257 ), #280, .T. ) ;
#67625 = CARTESIAN_POINT ( 'NONE',  ( 92.34999999999990905, 88.47002178664757821, 80.52791666666665549 ) ) ;
#67626 = VERTEX_POINT ( 'NONE', #29158 ) ;
#67627 = CARTESIAN_POINT ( 'NONE',  ( -92.69370383062498320, -209.9999999999999716, 75.35531250086714294 ) ) ;
#67628 = ORIENTED_EDGE ( 'NONE', *, *, #65150, .T. ) ;
#67629 = CARTESIAN_POINT ( 'NONE',  ( -92.35000000000003695, 90.00000000000004263, 86.50750000000000739 ) ) ;
#67630 = CARTESIAN_POINT ( 'NONE',  ( 10.00000000000000000, 12.26510123303259725, 35.53030884539089840 ) ) ;
#67631 = CARTESIAN_POINT ( 'NONE',  ( 7.399999999999994138, -1.226600263951431156E-13, -12.50000000000022027 ) ) ;
#67632 = DIRECTION ( 'NONE',  ( -1.000000000000000000, 0.000000000000000000, 0.000000000000000000 ) ) ;
#67633 = AXIS2_PLACEMENT_3D ( 'NONE', #71934, #31710, #54655 ) ;
#67634 = CARTESIAN_POINT ( 'NONE',  ( -97.64999999999993463, 88.47002178664749295, 81.16291666666667481 ) ) ;
#67635 = EDGE_CURVE ( 'NONE', #11463, #48336, #17467, .T. ) ;
#67636 = VECTOR ( 'NONE', #66293, 1000.000000000000000 ) ;
#67637 = FACE_OUTER_BOUND ( 'NONE', #7863, .T. ) ;
#67638 = CARTESIAN_POINT ( 'NONE',  ( 92.69370383062498320, 90.00000000000002842, 87.73781250086713612 ) ) ;
#67639 = DIRECTION ( 'NONE',  ( 0.000000000000000000, 0.000000000000000000, 1.000000000000000000 ) ) ;
#67640 = LINE ( 'NONE', #33406, #45820 ) ;
#67641 = ADVANCED_FACE ( 'NONE', ( #40835 ), #52462, .F. ) ;
#67642 = DIRECTION ( 'NONE',  ( 0.000000000000000000, 0.000000000000000000, -1.000000000000000000 ) ) ;
#67643 = LINE ( 'NONE', #9009, #45980 ) ;
#67644 = CARTESIAN_POINT ( 'NONE',  ( 10.00000000000000000, 35.38097989696512968, 12.42422080174651100 ) ) ;
#67645 = CARTESIAN_POINT ( 'NONE',  ( 11.99999999999999822, -62.50884508063395373, -41.76106447765554464 ) ) ;
#67646 = CARTESIAN_POINT ( 'NONE',  ( 97.64999999997402824, 89.99998827382246702, 82.77687459617033028 ) ) ;
#67647 = AXIS2_PLACEMENT_3D ( 'NONE', #13576, #36145, #1249 ) ;
#67648 = CARTESIAN_POINT ( 'NONE',  ( 0.000000000000000000, 0.000000000000000000, 0.000000000000000000 ) ) ;
#67649 = CIRCLE ( 'NONE', #54436, 31.99999999999998934 ) ;
#67650 = CARTESIAN_POINT ( 'NONE',  ( 6.000000000000000000, -10.30890764327441289, 81.34940948281332851 ) ) ;
#67651 = ADVANCED_FACE ( 'NONE', ( #43441 ), #43057, .T. ) ;
#67652 = CARTESIAN_POINT ( 'NONE',  ( 10.00000000000000000, 26.02418014898310261, 70.52718814184268581 ) ) ;
#67653 = AXIS2_PLACEMENT_3D ( 'NONE', #66890, #72518, #21019 ) ;
#67654 = CARTESIAN_POINT ( 'NONE',  ( 97.64999999999999147, -209.9999999999999716, 82.06250000000000000 ) ) ;
#67655 = CIRCLE ( 'NONE', #18432, 16.00000000000000000 ) ;
#67656 = AXIS2_PLACEMENT_3D ( 'NONE', #39736, #16045, #68304 ) ;
#67657 = DIRECTION ( 'NONE',  ( -1.000000000000000000, -0.000000000000000000, -0.000000000000000000 ) ) ;
#67658 = CARTESIAN_POINT ( 'NONE',  ( -92.34999999999999432, -208.4700217866474645, 84.02041666666667652 ) ) ;
#67659 = DIRECTION ( 'NONE',  ( -0.4796670183876294291, 0.8774505977381983346, 0.000000000000000000 ) ) ;
#67660 = EDGE_CURVE ( 'NONE', #56288, #12067, #65993, .T. ) ;
#67661 = DIRECTION ( 'NONE',  ( 0.000000000000000000, 0.000000000000000000, 1.000000000000000000 ) ) ;
#67662 = ADVANCED_FACE ( 'NONE', ( #20098 ), #13719, .T. ) ;
#67663 = DIRECTION ( 'NONE',  ( 0.000000000000000000, 0.000000000000000000, 1.000000000000000000 ) ) ;
#67664 = CARTESIAN_POINT ( 'NONE',  ( 0.000000000000000000, -71.87247863392443037, 39.47590169984818687 ) ) ;
#67665 = AXIS2_PLACEMENT_3D ( 'NONE', #27001, #41437, #31260 ) ;
#67666 = DIRECTION ( 'NONE',  ( 1.000000000000000000, 0.000000000000000000, 0.000000000000000000 ) ) ;
#67667 = EDGE_CURVE ( 'NONE', #63002, #10732, #58861, .T. ) ;
#67668 = CARTESIAN_POINT ( 'NONE',  ( 96.15314808468750130, -211.9973110713294489, 87.47322916753381605 ) ) ;
#67669 = VERTEX_POINT ( 'NONE', #8086 ) ;
#67670 = ORIENTED_EDGE ( 'NONE', *, *, #8987, .T. ) ;
#67671 = ADVANCED_FACE ( 'NONE', ( #14834 ), #25389, .F. ) ;
#67672 = DIRECTION ( 'NONE',  ( 0.000000000000000000, -0.9969173337331270757, -0.07845909572785580988 ) ) ;
#67673 = ORIENTED_EDGE ( 'NONE', *, *, #32763, .T. ) ;
#67674 = AXIS2_PLACEMENT_3D ( 'NONE', #25262, #48185, #31257 ) ;
#67675 = DIRECTION ( 'NONE',  ( 0.000000000000000000, 0.1564344650402311743, -0.9876883405951377704 ) ) ;
#67676 =( BOUNDED_CURVE ( )  B_SPLINE_CURVE ( 2, ( #1792, #47606, #69070, #13016, #35950, #57790, #18293 ),
 .UNSPECIFIED., .F., .F. ) 
 B_SPLINE_CURVE_WITH_KNOTS ( ( 3, 2, 2, 3 ),
 ( 0.5833333333333329263, 0.5902777777777776791, 0.5972222222222223209, 0.6041666666666670737 ),
 .UNSPECIFIED. ) 
 CURVE ( )  GEOMETRIC_REPRESENTATION_ITEM ( )  RATIONAL_B_SPLINE_CURVE ( ( 1.000000000000008660, 0.8660254037844301589, 1.000000000000000000, 0.8660254037844387076, 1.000000000000000000, 0.8660254037844301589, 1.000000000000008660 ) ) 
 REPRESENTATION_ITEM ( '' )  );
#67677 = CARTESIAN_POINT ( 'NONE',  ( 93.84685191531249870, -208.0026889286704943, 78.74197916753381321 ) ) ;
#67678 = ORIENTED_EDGE ( 'NONE', *, *, #23673, .T. ) ;
#67679 = CARTESIAN_POINT ( 'NONE',  ( 96.15314808468750130, -211.9973110713294489, 82.39322916753381776 ) ) ;
#67680 = DIRECTION ( 'NONE',  ( -1.000000000000000000, -0.000000000000000000, 0.000000000000000000 ) ) ;
#67681 = ORIENTED_EDGE ( 'NONE', *, *, #9348, .T. ) ;
#67682 = PLANE ( 'NONE',  #65908 ) ;
#67683 = EDGE_LOOP ( 'NONE', ( #72387, #29027, #51299, #43295 ) ) ;
#67684 = CARTESIAN_POINT ( 'NONE',  ( 50.00005079999999680, 1.530808498934191521E-15, -12.50000000000000000 ) ) ;
#67685 = AXIS2_PLACEMENT_3D ( 'NONE', #48347, #8505, #31049 ) ;
#67686 = ORIENTED_EDGE ( 'NONE', *, *, #8257, .T. ) ;
#67687 = DIRECTION ( 'NONE',  ( -1.000000000000000000, -0.000000000000000000, -0.000000000000000000 ) ) ;
#67688 = VERTEX_POINT ( 'NONE', #65246 ) ;
#67689 = CARTESIAN_POINT ( 'NONE',  ( -96.32500000000001705, 87.70503267997129626, 77.40583333333331950 ) ) ;
#67690 = CARTESIAN_POINT ( 'NONE',  ( 11.99999999999999822, -8.830959090341869100, -74.65491531819127147 ) ) ;
#67691 = ORIENTED_EDGE ( 'NONE', *, *, #36598, .T. ) ;
#67692 = LINE ( 'NONE', #15434, #29810 ) ;
#67693 = AXIS2_PLACEMENT_3D ( 'NONE', #63540, #63176, #782 ) ;
#67694 = ORIENTED_EDGE ( 'NONE', *, *, #73643, .F. ) ;
#67695 = CARTESIAN_POINT ( 'NONE',  ( 5.999999999999999112, 77.16300072079698680, -27.74655509720591340 ) ) ;
#67696 = ORIENTED_EDGE ( 'NONE', *, *, #31848, .T. ) ;
#67697 = EDGE_LOOP ( 'NONE', ( #7217, #64290, #67515, #24024 ) ) ;
#67698 = VECTOR ( 'NONE', #27307, 1000.000000000000000 ) ;
#67699 = ORIENTED_EDGE ( 'NONE', *, *, #46042, .F. ) ;
#67700 = DIRECTION ( 'NONE',  ( 0.000000000000000000, 0.000000000000000000, -1.000000000000000000 ) ) ;
#67701 = AXIS2_PLACEMENT_3D ( 'NONE', #12435, #39540, #23721 ) ;
#67702 = ITEM_DEFINED_TRANSFORMATION ( 'NONE', 'NONE', #66401,  #43395 ) ;
#67703 = CARTESIAN_POINT ( 'NONE',  ( 10.00000000000000000, -25.88420570971419821, 27.13269053701087330 ) ) ;
#67704 = ORIENTED_EDGE ( 'NONE', *, *, #60031, .T. ) ;
#67705 = VERTEX_POINT ( 'NONE', #53963 ) ;
#67706 = ORIENTED_EDGE ( 'NONE', *, *, #55496, .F. ) ;
#67707 = CARTESIAN_POINT ( 'NONE',  ( 10.00000000000000000, -2.543863470247802905, -81.96053171279903893 ) ) ;
#67708 = CARTESIAN_POINT ( 'NONE',  ( -99.99999999999998579, -124.0000000000000142, -40.00000000000002132 ) ) ;
#67709 = CARTESIAN_POINT ( 'NONE',  ( -97.30629616937501680, 91.33154071421968467, 77.04864583420048518 ) ) ;
#67710 = ORIENTED_EDGE ( 'NONE', *, *, #56940, .T. ) ;
#67711 = CARTESIAN_POINT ( 'NONE',  ( 96.15314808468748708, 91.99731107132950569, 77.36614583420046642 ) ) ;
#67712 = ORIENTED_EDGE ( 'NONE', *, *, #45247, .T. ) ;
#67713 = FILL_AREA_STYLE_COLOUR ( '', #47937 ) ;
#67714 = CARTESIAN_POINT ( 'NONE',  ( -97.30629616937495996, -209.9999999999999716, 85.19781250086714408 ) ) ;
#67715 = ORIENTED_EDGE ( 'NONE', *, *, #39727, .T. ) ;
#67716 = DIRECTION ( 'NONE',  ( -1.000000000000000000, -0.000000000000000000, 0.000000000000000000 ) ) ;
#67717 = DIRECTION ( 'NONE',  ( 1.000000000000000000, 0.000000000000000000, 0.000000000000000000 ) ) ;
#67718 = DIRECTION ( 'NONE',  ( -1.000000000000000000, -0.000000000000000000, 0.000000000000000000 ) ) ;
#67719 = CARTESIAN_POINT ( 'NONE',  ( -97.30629616937497417, -208.6684592857803295, 80.69989583420046131 ) ) ;
#67720 = AXIS2_PLACEMENT_3D ( 'NONE', #29043, #41438, #17398 ) ;
#67721 = EDGE_CURVE ( 'NONE', #21877, #58950, #17526, .T. ) ;
#67722 = CARTESIAN_POINT ( 'NONE',  ( 4.999999999999999112, -36.13751322684434797, 21.40280677340357940 ) ) ;
#67723 = LINE ( 'NONE', #44427, #54775 ) ;
#67724 = DIRECTION ( 'NONE',  ( 0.000000000000000000, 0.7431448254773960205, -0.6691306063588563502 ) ) ;
#67725 = EDGE_LOOP ( 'NONE', ( #7136, #42807, #67696, #23407 ) ) ;
#67726 = EDGE_CURVE ( 'NONE', #17422, #21235, #66740, .T. ) ;
#67727 = ORIENTED_EDGE ( 'NONE', *, *, #23013, .F. ) ;
#67728 = FACE_OUTER_BOUND ( 'NONE', #24269, .T. ) ;
#67729 = EDGE_CURVE ( 'NONE', #54454, #57324, #55941, .T. ) ;
#67730 = CARTESIAN_POINT ( 'NONE',  ( 94.99999999999998579, 93.05995642670504253, 84.76125000000000398 ) ) ;
#67731 = DIRECTION ( 'NONE',  ( -1.000000000000000000, 0.000000000000000000, 0.000000000000000000 ) ) ;
#67732 = CARTESIAN_POINT ( 'NONE',  ( -92.69370383062504004, 90.00000000000004263, 82.34031250086714238 ) ) ;
#67733 = FACE_OUTER_BOUND ( 'NONE', #4723, .T. ) ;
#67734 = DIRECTION ( 'NONE',  ( 1.000000000000000000, 0.000000000000000000, 0.000000000000000000 ) ) ;
#67735 = AXIS2_PLACEMENT_3D ( 'NONE', #12691, #8162, #1100 ) ;
#67736 = EDGE_CURVE ( 'NONE', #39261, #45157, #36656, .T. ) ;
#67737 = ORIENTED_EDGE ( 'NONE', *, *, #18379, .F. ) ;
#67738 = DIRECTION ( 'NONE',  ( 1.000000000000000000, 0.000000000000000000, -0.000000000000000000 ) ) ;
#67739 = CARTESIAN_POINT ( 'NONE',  ( 10.00000000000000000, -28.89263327155797967, 71.91182617369179297 ) ) ;
#67740 = DIRECTION ( 'NONE',  ( -1.000000000000000000, 0.000000000000000000, -0.000000000000000000 ) ) ;
#67741 = DIRECTION ( 'NONE',  ( 0.000000000000000000, -0.9238795325112906243, 0.3826834323650805669 ) ) ;
#67742 = CARTESIAN_POINT ( 'NONE',  ( -92.35000000000005116, 91.52997821335254969, 89.73541666666663730 ) ) ;
#67743 = CARTESIAN_POINT ( 'NONE',  ( 92.35000000000000853, -209.9999999999999716, 88.80937500173430976 ) ) ;
#67744 = CARTESIAN_POINT ( 'NONE',  ( -93.84685191531247028, -211.9973110713294489, 79.85322916753381151 ) ) ;
#67745 = CARTESIAN_POINT ( 'NONE',  ( 0.000000000000000000, 74.65491531819118620, 23.16904090965733332 ) ) ;
#67746 = CIRCLE ( 'NONE', #42519, 31.99999999999998934 ) ;
#67747 = EDGE_LOOP ( 'NONE', ( #814, #14260, #42884, #33902 ) ) ;
#67748 = AXIS2_PLACEMENT_3D ( 'NONE', #72268, #30932, #60643 ) ;
#67749 = CYLINDRICAL_SURFACE ( 'NONE', #52682, 31.99999999999998579 ) ;
#67750 = CARTESIAN_POINT ( 'NONE',  ( -92.34999999999998010, 91.52997821335249284, 88.46541666666664128 ) ) ;
#67751 = DIRECTION ( 'NONE',  ( -1.000000000000000000, 0.000000000000000000, 0.000000000000000000 ) ) ;
#67752 = ORIENTED_EDGE ( 'NONE', *, *, #61650, .F. ) ;
#67753 = CARTESIAN_POINT ( 'NONE',  ( 0.000000000000000000, -78.73519480814971416, 22.90783923731600069 ) ) ;
#67754 = CARTESIAN_POINT ( 'NONE',  ( 0.000000000000000000, -31.47745569255189224, 68.26794271651249346 ) ) ;
#67755 = CIRCLE ( 'NONE', #36500, 31.99999999999998579 ) ;
#67756 = EDGE_CURVE ( 'NONE', #57151, #69865, #58358, .T. ) ;
#67758 = EDGE_CURVE ( 'NONE', #7618, #37316, #2855, .T. ) ;
#67757 = VECTOR ( 'NONE', #74022, 1000.000000000000000 ) ;
#67759 = UNCERTAINTY_MEASURE_WITH_UNIT (LENGTH_MEASURE( 1.000000000000000082E-05 ), #52252, 'distance_accuracy_value', 'NONE');
#67760 = DIRECTION ( 'NONE',  ( -1.000000000000000000, 0.000000000000000000, -0.000000000000000000 ) ) ;
#67761 = ORIENTED_EDGE ( 'NONE', *, *, #24701, .F. ) ;
#67762 = CARTESIAN_POINT ( 'NONE',  ( 10.00000000000000000, 36.88895765772633695, 6.736453364083687667 ) ) ;
#67763 = EDGE_CURVE ( 'NONE', #46797, #71305, #45175, .T. ) ;
#67764 = DIRECTION ( 'NONE',  ( 1.000000000000000000, 0.000000000000000000, 0.000000000000000000 ) ) ;
#67765 = VERTEX_POINT ( 'NONE', #41939 ) ;
#67766 = VECTOR ( 'NONE', #18744, 1000.000000000000000 ) ;
#67767 = CARTESIAN_POINT ( 'NONE',  ( 95.00000000000000000, -212.6630814284392557, 87.26156250086714294 ) ) ;
#67768 = CARTESIAN_POINT ( 'NONE',  ( 10.00000000000000000, -26.01480285779785362, -70.53064760720343429 ) ) ;
#67769 = ORIENTED_EDGE ( 'NONE', *, *, #41592, .T. ) ;
#67770 = VECTOR ( 'NONE', #65956, 1000.000000000000000 ) ;
#67771 = DIRECTION ( 'NONE',  ( 0.000000000000000000, 0.000000000000000000, 1.000000000000000000 ) ) ;
#67772 = EDGE_LOOP ( 'NONE', ( #64037, #73624, #2068, #52317 ) ) ;
#67773 = ORIENTED_EDGE ( 'NONE', *, *, #53002, .T. ) ;
#67774 = CARTESIAN_POINT ( 'NONE',  ( 8.700667342345820288, -98.11853780484867116, 5.500000000000000000 ) ) ;
#67775 = ORIENTED_EDGE ( 'NONE', *, *, #13475, .F. ) ;
#67776 = EDGE_LOOP ( 'NONE', ( #2925, #41549, #1962, #68569 ) ) ;
#67777 = ORIENTED_EDGE ( 'NONE', *, *, #57597, .F. ) ;
#67778 = DIRECTION ( 'NONE',  ( 1.000000000000000000, 1.427937372958405461E-15, 7.962523111839130290E-16 ) ) ;
#67779 = ORIENTED_EDGE ( 'NONE', *, *, #49463, .F. ) ;
#67780 = ORIENTED_EDGE ( 'NONE', *, *, #46764, .F. ) ;
#67781 = CARTESIAN_POINT ( 'NONE',  ( 94.99999999999998579, 92.66308142843935514, 76.94281250086714863 ) ) ;
#67782 = CARTESIAN_POINT ( 'NONE',  ( 10.00000000000000000, 74.18225833017937987, -34.94270380257560049 ) ) ;
#67783 = CYLINDRICAL_SURFACE ( 'NONE', #18921, 77.49899999999999523 ) ;
#67784 = ORIENTED_EDGE ( 'NONE', *, *, #64767, .T. ) ;
#67785 = ORIENTED_EDGE ( 'NONE', *, *, #29537, .F. ) ;
#67786 = ORIENTED_EDGE ( 'NONE', *, *, #29082, .F. ) ;
#67787 = CARTESIAN_POINT ( 'NONE',  ( 94.99999999999998579, 87.33691857156068750, 87.89656250086713385 ) ) ;
#67788 = ORIENTED_EDGE ( 'NONE', *, *, #5064, .F. ) ;
#67789 = CARTESIAN_POINT ( 'NONE',  ( 96.15314808468748708, -208.0026889286704943, 84.35114583420048007 ) ) ;
#67790 = VECTOR ( 'NONE', #18388, 1000.000000000000000 ) ;
#67791 = CARTESIAN_POINT ( 'NONE',  ( 0.000000000000000000, 0.000000000000000000, 0.000000000000000000 ) ) ;
#67792 = CARTESIAN_POINT ( 'NONE',  ( -92.34999999999999432, -209.9999999999999716, 90.00000000000000000 ) ) ;
#67793 = FACE_OUTER_BOUND ( 'NONE', #43557, .T. ) ;
#67794 = LINE ( 'NONE', #33195, #36520 ) ;
#67795 = CYLINDRICAL_SURFACE ( 'NONE', #12786, 42.00000000000000000 ) ;
#67796 = CARTESIAN_POINT ( 'NONE',  ( 10.00000000000000000, 34.44570377933598593, 69.42325613327452061 ) ) ;
#67797 = CARTESIAN_POINT ( 'NONE',  ( -3.000000000000000000, -23.29833615347104825, -3.418703333116803744 ) ) ;
#67798 = CARTESIAN_POINT ( 'NONE',  ( -97.30629616937497417, -208.6684592857803011, 88.31989583420046586 ) ) ;
#67799 = CARTESIAN_POINT ( 'NONE',  ( -95.00000000000002842, 92.66308142843932671, 87.10281250086715943 ) ) ;
#67800 = VERTEX_POINT ( 'NONE', #64874 ) ;
#67802 = CARTESIAN_POINT ( 'NONE',  ( -95.00000000000002842, 87.33691857156074434, 84.72156250086713669 ) ) ;
#67801 = CARTESIAN_POINT ( 'NONE',  ( 92.69370383062498320, 91.33154071421968467, 88.95489583420048518 ) ) ;
#67803 = ORIENTED_EDGE ( 'NONE', *, *, #48364, .T. ) ;
#67804 = CARTESIAN_POINT ( 'NONE',  ( 95.00000000000000000, -213.0599564267049857, 84.52312500173428589 ) ) ;
#67805 = CARTESIAN_POINT ( 'NONE',  ( -95.00000000000002842, 90.00000000000004263, 90.00000000000000000 ) ) ;
#67806 = CARTESIAN_POINT ( 'NONE',  ( 10.00000000000000000, -37.58145647212453611, -0.6853352020794456489 ) ) ;
#67807 = CARTESIAN_POINT ( 'NONE',  ( 11.99999999999999822, -3.894527615417340272, -81.90746397400391743 ) ) ;
#67808 = DIRECTION ( 'NONE',  ( -1.000000000000000000, -0.000000000000000000, -0.000000000000000000 ) ) ;
#67809 = DIRECTION ( 'NONE',  ( 0.000000000000000000, 0.000000000000000000, 1.000000000000000000 ) ) ;
#67810 = CARTESIAN_POINT ( 'NONE',  ( 11.99999999999999822, 73.44644590900061587, 24.73286445877730699 ) ) ;
#67811 = CARTESIAN_POINT ( 'NONE',  ( 0.000000000000000000, 22.74946021919175720, -29.81001611430984255 ) ) ;
#67812 = AXIS2_PLACEMENT_3D ( 'NONE', #71153, #54981, #26772 ) ;
#67813 = CARTESIAN_POINT ( 'NONE',  ( 11.99999999999999822, 0.000000000000000000, 0.000000000000000000 ) ) ;
#67814 = ORIENTED_EDGE ( 'NONE', *, *, #57044, .F. ) ;
#67815 = EDGE_CURVE ( 'NONE', #49448, #69189, #13355, .T. ) ;
#67816 = ORIENTED_EDGE ( 'NONE', *, *, #40892, .F. ) ;
#67817 = EDGE_CURVE ( 'NONE', #16386, #23771, #4340, .T. ) ;
#67818 = CARTESIAN_POINT ( 'NONE',  ( -97.65000000000001990, 88.47002178664754979, 83.06791666666664753 ) ) ;
#67819 = DIRECTION ( 'NONE',  ( 0.000000000000000000, 0.9876883405951372152, 0.1564344650402346160 ) ) ;
#67820 = CARTESIAN_POINT ( 'NONE',  ( -95.00000000000002842, 90.00000000000004263, 90.00000000000000000 ) ) ;
#67821 = DIRECTION ( 'NONE',  ( -1.000000000000000000, 0.000000000000000000, 0.000000000000000000 ) ) ;
#67822 = CARTESIAN_POINT ( 'NONE',  ( -11.59999999999999787, 0.000000000000000000, 40.80000000000001847 ) ) ;
#67823 = DIRECTION ( 'NONE',  ( 0.000000000000000000, 0.000000000000000000, 1.000000000000000000 ) ) ;
#67824 = FACE_OUTER_BOUND ( 'NONE', #69608, .T. ) ;
#67825 = DIRECTION ( 'NONE',  ( -1.000000000000000000, 0.000000000000000000, 0.000000000000000000 ) ) ;
#67826 = EDGE_CURVE ( 'NONE', #40774, #12733, #3165, .T. ) ;
#67827 = ORIENTED_EDGE ( 'NONE', *, *, #17676, .F. ) ;
#67828 = CARTESIAN_POINT ( 'NONE',  ( -92.69370383062504004, 90.00000000000004263, 82.97531250086714749 ) ) ;
#67829 = AXIS2_PLACEMENT_3D ( 'NONE', #58544, #58934, #71292 ) ;
#67830 = FACE_OUTER_BOUND ( 'NONE', #56797, .T. ) ;
#67831 = EDGE_CURVE ( 'NONE', #36914, #45508, #31379, .T. ) ;
#67832 = CARTESIAN_POINT ( 'NONE',  ( -23.50044424985255276, 0.001194404164626844313, -80.00000000000000000 ) ) ;
#67833 = DIRECTION ( 'NONE',  ( 0.000000000000000000, -0.1564344650402382242, 0.9876883405951366601 ) ) ;
#67834 = CARTESIAN_POINT ( 'NONE',  ( 11.99999999999999822, -49.70050353004846500, -59.46389618802017907 ) ) ;
#67835 = CARTESIAN_POINT ( 'NONE',  ( -92.35000000000003695, 90.00000000000004263, 82.06250000000000000 ) ) ;
#67836 = CYLINDRICAL_SURFACE ( 'NONE', #16613, 2.649999999999985700 ) ;
#67837 =( NAMED_UNIT ( * ) SI_UNIT ( $, .STERADIAN. ) SOLID_ANGLE_UNIT ( ) );
#67838 = ADVANCED_FACE ( 'NONE', ( #14086 ), #8467, .F. ) ;
#67839 = ADVANCED_FACE ( 'NONE', ( #49420 ), #49780, .T. ) ;
#67840 = CIRCLE ( 'NONE', #39081, 15.70000000000000284 ) ;
#67841 = CARTESIAN_POINT ( 'NONE',  ( 97.30629616937498838, 90.00000000000002842, 81.86406250086714920 ) ) ;
#67842 = CARTESIAN_POINT ( 'NONE',  ( -97.30629616937497417, -211.3315407142195852, 80.32947916753381890 ) ) ;
#67843 = FACE_OUTER_BOUND ( 'NONE', #34104, .T. ) ;
#67844 = VERTEX_POINT ( 'NONE', #10680 ) ;
#67845 = LINE ( 'NONE', #27979, #54493 ) ;
#67846 = CARTESIAN_POINT ( 'NONE',  ( -92.34999999999999432, -209.9999999999999716, 75.07749999999998636 ) ) ;
#67847 = CARTESIAN_POINT ( 'NONE',  ( 97.64999999999999147, -209.9999733970770137, 78.96687592183759818 ) ) ;
#67848 = EDGE_CURVE ( 'NONE', #58924, #39300, #4323, .T. ) ;
#67849 = EDGE_CURVE ( 'NONE', #47502, #26794, #73455, .T. ) ;
#67850 = CIRCLE ( 'NONE', #31820, 82.00000000000000000 ) ;
#67851 = CARTESIAN_POINT ( 'NONE',  ( -96.15314808468752972, 91.99731107132950569, 77.63072916753381492 ) ) ;
#67852 = CARTESIAN_POINT ( 'NONE',  ( 96.15314808468748708, -208.0026889286704943, 79.90614583420047268 ) ) ;
#67853 = VERTEX_POINT ( 'NONE', #26489 ) ;
#67854 = CYLINDRICAL_SURFACE ( 'NONE', #40676, 31.99999999999999289 ) ;
#67855 = VERTEX_POINT ( 'NONE', #55808 ) ;
#67856 = AXIS2_PLACEMENT_3D ( 'NONE', #29153, #1008, #63039 ) ;
#67857 = CARTESIAN_POINT ( 'NONE',  ( -94.99999999999997158, -206.9400435732949575, 88.01562500173432113 ) ) ;
#67858 = VECTOR ( 'NONE', #62066, 1000.000000000000000 ) ;
#67859 = ORIENTED_EDGE ( 'NONE', *, *, #33411, .F. ) ;
#67860 = CARTESIAN_POINT ( 'NONE',  ( -10.94538922500103162, 0.000000000000000000, 13.90444123027096879 ) ) ;
#67861 = VECTOR ( 'NONE', #10800, 1000.000000000000000 ) ;
#67862 = ORIENTED_EDGE ( 'NONE', *, *, #67325, .T. ) ;
#67863 = ORIENTED_EDGE ( 'NONE', *, *, #46249, .T. ) ;
#67864 = CIRCLE ( 'NONE', #39054, 16.00000000000000355 ) ;
#67865 = ORIENTED_EDGE ( 'NONE', *, *, #17994, .T. ) ;
#67866 = CARTESIAN_POINT ( 'NONE',  ( 97.30629616937498838, -211.3315407142195852, 75.46114583420049371 ) ) ;
#67867 = EDGE_LOOP ( 'NONE', ( #56736, #41546, #5937, #24490 ) ) ;
#67868 = CARTESIAN_POINT ( 'NONE',  ( 5.000000000000000000, 35.47612816024523852, 22.48208911017513145 ) ) ;
#67869 = CARTESIAN_POINT ( 'NONE',  ( -97.64999999993850111, -209.9999881787635729, 81.82400613094797848 ) ) ;
#67870 = CARTESIAN_POINT ( 'NONE',  ( 97.30629616937498838, 88.66845928578037217, 86.89114583420050053 ) ) ;
#67871 = DIRECTION ( 'NONE',  ( 0.000000000000000000, 0.000000000000000000, 1.000000000000000000 ) ) ;
#67872 = CARTESIAN_POINT ( 'NONE',  ( 97.64999999999997726, -211.5299782133524502, 76.92958333333332632 ) ) ;
#67873 = AXIS2_PLACEMENT_3D ( 'NONE', #16392, #56633, #45731 ) ;
#67874 = ORIENTED_EDGE ( 'NONE', *, *, #55756, .F. ) ;
#67875 = ORIENTED_EDGE ( 'NONE', *, *, #20097, .T. ) ;
#67876 = ORIENTED_EDGE ( 'NONE', *, *, #68586, .F. ) ;
#67877 = ORIENTED_EDGE ( 'NONE', *, *, #45504, .F. ) ;
#67878 = DIRECTION ( 'NONE',  ( 0.000000000000000000, 0.000000000000000000, 1.000000000000000000 ) ) ;
#67879 = FILL_AREA_STYLE ('',( #67507 ) ) ;
#67880 = DIRECTION ( 'NONE',  ( 0.000000000000000000, 0.3090169943749480619, -0.9510565162951533091 ) ) ;
#67881 = VECTOR ( 'NONE', #43803, 1000.000000000000000 ) ;
#67882 = CARTESIAN_POINT ( 'NONE',  ( 5.000000000000000000, -67.80270845531921964, 46.11716303203163392 ) ) ;
#67883 = FACE_OUTER_BOUND ( 'NONE', #55765, .T. ) ;
#67884 = CARTESIAN_POINT ( 'NONE',  ( -92.35000000005462084, -210.0000170173125014, 88.49187441316038871 ) ) ;
#67885 = FACE_OUTER_BOUND ( 'NONE', #34585, .T. ) ;
#67886 = EDGE_CURVE ( 'NONE', #45326, #34583, #28352, .T. ) ;
#67887 = VERTEX_POINT ( 'NONE', #44909 ) ;
#67888 = CARTESIAN_POINT ( 'NONE',  ( -93.67499999999998295, -207.7050326799711968, 84.15270833506762926 ) ) ;
#67889 = ORIENTED_EDGE ( 'NONE', *, *, #39987, .T. ) ;
#67890 = DIRECTION ( 'NONE',  ( 7.962523111839282146E-16, -1.065814103640130873E-14, -1.000000000000000000 ) ) ;
#67892 = ORIENTED_EDGE ( 'NONE', *, *, #17384, .F. ) ;
#67891 = ADVANCED_FACE ( 'NONE', ( #67830, #72698 ), #60717, .F. ) ;
#67894 = CARTESIAN_POINT ( 'NONE',  ( -95.00000000000002842, 86.94004357329504273, 78.17312500173430578 ) ) ;
#67893 = CARTESIAN_POINT ( 'NONE',  ( 96.32499999999997442, 92.29496732002878900, 83.51770833506763836 ) ) ;
#67895 =( BOUNDED_CURVE ( )  B_SPLINE_CURVE ( 2, ( #6281, #23557, #46486, #56677, #28447, #22078, #45394, #45022, #51380 ),
 .UNSPECIFIED., .F., .F. ) 
 B_SPLINE_CURVE_WITH_KNOTS ( ( 3, 2, 2, 2, 3 ),
 ( 0.6138516023186938453, 0.6209073675976484186, 0.6279631331385308046, 0.6350188986794130797, 0.6350190250571088324 ),
 .UNSPECIFIED. ) 
 CURVE ( )  GEOMETRIC_REPRESENTATION_ITEM ( )  RATIONAL_B_SPLINE_CURVE ( ( 1.000000000000000000, 0.8660254037844387076, 1.000000000000000000, 0.8660254037844387076, 1.000000000000000000, 0.8660254037844387076, 1.000000000000000000, 0.9999976003453262541, 0.9999952007766141904 ) ) 
 REPRESENTATION_ITEM ( '' )  );
#67896 = EDGE_LOOP ( 'NONE', ( #16483, #6313, #57153, #64901 ) ) ;
#67897 = CARTESIAN_POINT ( 'NONE',  ( 93.84685191531248449, 88.00268892867053694, 82.92239583420048632 ) ) ;
#67898 = CARTESIAN_POINT ( 'NONE',  ( -93.67500000000003979, 87.70503267997129626, 76.24166666666666003 ) ) ;
#67899 = DIRECTION ( 'NONE',  ( 1.343011723336883198E-16, -1.000000000000000000, 0.000000000000000000 ) ) ;
#67900 = EDGE_CURVE ( 'NONE', #49062, #36328, #50531, .T. ) ;
#67901 = LINE ( 'NONE', #16391, #6210 ) ;
#67902 = CYLINDRICAL_SURFACE ( 'NONE', #67873, 37.49900000000000233 ) ;
#67903 = LINE ( 'NONE', #39333, #61311 ) ;
#67904 = ORIENTED_EDGE ( 'NONE', *, *, #13982, .F. ) ;
#67905 = DIRECTION ( 'NONE',  ( -1.000000000000000000, -0.000000000000000000, -0.000000000000000000 ) ) ;
#67906 = DIRECTION ( 'NONE',  ( 0.8225049752423776450, 0.5687579148473765889, -0.000000000000000000 ) ) ;
#67907 = CARTESIAN_POINT ( 'NONE',  ( 10.00000000000000000, 10.74501242461333028, -35.92658777277499382 ) ) ;
#67908 = CIRCLE ( 'NONE', #27037, 37.49900000000000233 ) ;
#67909 = VERTEX_POINT ( 'NONE', #22338 ) ;
#67910 = ADVANCED_FACE ( 'NONE', ( #39264 ), #67081, .F. ) ;
#67911 = ORIENTED_EDGE ( 'NONE', *, *, #18354, .T. ) ;
#67912 = CARTESIAN_POINT ( 'NONE',  ( 95.00000000002597744, 90.00000000000007105, -75.00000000000000000 ) ) ;
#67913 = CYLINDRICAL_SURFACE ( 'NONE', #6572, 16.00000000000000000 ) ;
#67914 = CARTESIAN_POINT ( 'NONE',  ( 2.874421927457452952, -143.3717286177755739, 5.500000000000000000 ) ) ;
#67915 = CARTESIAN_POINT ( 'NONE',  ( -94.99999999999997158, -207.3369185715606307, 82.02281250086714692 ) ) ;
#67916 = ORIENTED_EDGE ( 'NONE', *, *, #45932, .F. ) ;
#67917 = ADVANCED_FACE ( 'NONE', ( #45282 ), #68203, .F. ) ;
#67918 = CARTESIAN_POINT ( 'NONE',  ( -96.15314808468751551, 88.00268892867056536, 88.47864583420047779 ) ) ;
#67919 = CIRCLE ( 'NONE', #53522, 11.59999999999999964 ) ;
#67920 = ORIENTED_EDGE ( 'NONE', *, *, #32976, .F. ) ;
#67921 = DIRECTION ( 'NONE',  ( 0.000000000000000000, 0.000000000000000000, 1.000000000000000000 ) ) ;
#67922 = AXIS2_PLACEMENT_3D ( 'NONE', #35144, #58081, #30239 ) ;
#67923 = FACE_BOUND ( 'NONE', #45888, .T. ) ;
#67924 = DIRECTION ( 'NONE',  ( -1.000000000000000000, 0.000000000000000000, 0.000000000000000000 ) ) ;
#67925 = CARTESIAN_POINT ( 'NONE',  ( 93.84685191531248449, 91.99731107132950569, 75.56697916753381605 ) ) ;
#67926 = CARTESIAN_POINT ( 'NONE',  ( -20.30386590532152979, -102.9045904027214959, 2.500000000000000000 ) ) ;
#67927 = CARTESIAN_POINT ( 'NONE',  ( 94.99999999999998579, 86.94004357329502852, 78.17312500173430578 ) ) ;
#67928 = AXIS2_PLACEMENT_3D ( 'NONE', #9658, #72786, #50614 ) ;
#67929 = CARTESIAN_POINT ( 'NONE',  ( -96.32499999999996021, -207.7050326799711968, 76.63854166840096127 ) ) ;
#67930 = CARTESIAN_POINT ( 'NONE',  ( -93.26027265873587169, -208.4859488783624215, 74.79348190356851944 ) ) ;
#67931 = EDGE_CURVE ( 'NONE', #22766, #47765, #59909, .T. ) ;
#67932 = DIRECTION ( 'NONE',  ( 0.000000000000000000, 0.000000000000000000, -1.000000000000000000 ) ) ;
#67933 = ADVANCED_FACE ( 'NONE', ( #43802 ), #66719, .F. ) ;
#67934 = CIRCLE ( 'NONE', #23545, 20.64000000000000057 ) ;
#67935 = AXIS2_PLACEMENT_3D ( 'NONE', #910, #41102, #13618 ) ;
#67936 = CARTESIAN_POINT ( 'NONE',  ( 95.00000000000000000, -206.9400435732949575, 79.12562500173429214 ) ) ;
#67937 = DIRECTION ( 'NONE',  ( -1.000000000000000000, 0.000000000000000000, -0.000000000000000000 ) ) ;
#67938 = CARTESIAN_POINT ( 'NONE',  ( -92.69370383062498320, -211.3315407142195852, 89.43114583420049257 ) ) ;
#67939 = DIRECTION ( 'NONE',  ( 0.000000000000000000, -0.8090169943749531134, 0.5877852522924653655 ) ) ;
#67940 = ORIENTED_EDGE ( 'NONE', *, *, #3664, .T. ) ;
#67941 = CARTESIAN_POINT ( 'NONE',  ( 10.00000000000000000, -76.41127070299262414, -12.93880638057396304 ) ) ;
#67942 = CARTESIAN_POINT ( 'NONE',  ( -93.84685191531254134, 91.99731107132950569, 78.63614583420047666 ) ) ;
#67943 = AXIS2_PLACEMENT_3D ( 'NONE', #29829, #36592, #70417 ) ;
#67944 = CARTESIAN_POINT ( 'NONE',  ( 97.30629616937498838, -211.3315407142195852, 89.27239583420048064 ) ) ;
#67945 = ORIENTED_EDGE ( 'NONE', *, *, #50074, .T. ) ;
#67946 = DIRECTION ( 'NONE',  ( -1.000000000000000000, 0.000000000000000000, -0.000000000000000000 ) ) ;
#67947 = PLANE ( 'NONE',  #56403 ) ;
#67948 = DIRECTION ( 'NONE',  ( 0.000000000000000000, 0.000000000000000000, 1.000000000000000000 ) ) ;
#67949 = CARTESIAN_POINT ( 'NONE',  ( -94.99999999999997158, -206.9400435732949575, 84.76125000000000398 ) ) ;
#67950 = CARTESIAN_POINT ( 'NONE',  ( 97.30629616937498838, -211.3315407142195852, 75.46114583420049371 ) ) ;
#67951 = ORIENTED_EDGE ( 'NONE', *, *, #4721, .T. ) ;
#67952 = ORIENTED_EDGE ( 'NONE', *, *, #49704, .T. ) ;
#67953 = CARTESIAN_POINT ( 'NONE',  ( 92.69370383062501162, -209.9999999999999716, 89.64281250086713726 ) ) ;
#67954 = CARTESIAN_POINT ( 'NONE',  ( 15.00000000000000000, 23.49999999999999645, 1.499999999999995337 ) ) ;
#67955 = CARTESIAN_POINT ( 'NONE',  ( -97.64999999999996305, -209.9999999999999716, 85.63437500173431260 ) ) ;
#67956 = PLANE ( 'NONE',  #32690 ) ;
#67957 = VECTOR ( 'NONE', #68924, 1000.000000000000000 ) ;
#67958 = CARTESIAN_POINT ( 'NONE',  ( 92.35000000000000853, -209.9999999999999716, 81.82437500173429612 ) ) ;
#67959 = CARTESIAN_POINT ( 'NONE',  ( 93.67500000000001137, -207.7050326799711968, 89.89416666666666345 ) ) ;
#67960 = EDGE_CURVE ( 'NONE', #20502, #58897, #3953, .T. ) ;
#67961 = ORIENTED_EDGE ( 'NONE', *, *, #51348, .T. ) ;
#67962 = CARTESIAN_POINT ( 'NONE',  ( -97.47814808468751835, 90.00000000000004263, 89.90078125043358170 ) ) ;
#67963 = VERTEX_POINT ( 'NONE', #50143 ) ;
#67964 = ORIENTED_EDGE ( 'NONE', *, *, #63403, .T. ) ;
#67965 = CARTESIAN_POINT ( 'NONE',  ( 11.99999999999999822, 0.000000000000000000, 0.000000000000000000 ) ) ;
#67966 =( NAMED_UNIT ( * ) SI_UNIT ( $, .STERADIAN. ) SOLID_ANGLE_UNIT ( ) );
#67967 = CARTESIAN_POINT ( 'NONE',  ( 0.000000000000000000, 0.000000000000000000, 0.000000000000000000 ) ) ;
#67968 = EDGE_CURVE ( 'NONE', #21517, #29541, #46348, .T. ) ;
#67969 = AXIS2_PLACEMENT_3D ( 'NONE', #56931, #8272, #32301 ) ;
#67970 = ORIENTED_EDGE ( 'NONE', *, *, #68771, .F. ) ;
#67971 = DIRECTION ( 'NONE',  ( -1.000000000000000000, 0.000000000000000000, 0.000000000000000000 ) ) ;
#67972 = CARTESIAN_POINT ( 'NONE',  ( 96.32499999999998863, -207.7050326799711968, 75.26270833506764291 ) ) ;
#67973 = CARTESIAN_POINT ( 'NONE',  ( 92.34999999999999432, 90.00000000000002842, 81.10999999999999943 ) ) ;
#67974 = ADVANCED_FACE ( 'NONE', ( #10311 ), #11417, .T. ) ;
#67975 = VERTEX_POINT ( 'NONE', #46380 ) ;
#67976 = ORIENTED_EDGE ( 'NONE', *, *, #829, .T. ) ;
#67977 = CARTESIAN_POINT ( 'NONE',  ( -92.35000000000000853, -210.0000058630848798, 82.77687479895044476 ) ) ;
#67978 = VERTEX_POINT ( 'NONE', #6891 ) ;
#67979 = AXIS2_PLACEMENT_3D ( 'NONE', #13532, #24816, #64311 ) ;
#67980 = CARTESIAN_POINT ( 'NONE',  ( 5.000000000000002665, 2.543863470249527303, -81.96053171279901051 ) ) ;
#67981 = CARTESIAN_POINT ( 'NONE',  ( -96.15314808468751551, 88.00268892867056536, 86.09739583420049769 ) ) ;
#67982 = CARTESIAN_POINT ( 'NONE',  ( 97.30629616937498838, 91.33154071421968467, 79.85322916753379729 ) ) ;
#67983 = VERTEX_POINT ( 'NONE', #23090 ) ;
#67984 = DIRECTION ( 'NONE',  ( 2.603472992746261562E-14, 2.546204323184492723E-14, -1.000000000000000000 ) ) ;
#67985 = ADVANCED_FACE ( 'NONE', ( #17072 ), #5436, .F. ) ;
#67986 = FACE_OUTER_BOUND ( 'NONE', #48976, .T. ) ;
#67987 = CARTESIAN_POINT ( 'NONE',  ( 11.99999999999999822, -77.32052557432845674, 5.256550761632577284 ) ) ;
#67988 = CARTESIAN_POINT ( 'NONE',  ( -97.64999999999986358, -208.4700217866474361, 77.88208333333332689 ) ) ;
#67989 = ORIENTED_EDGE ( 'NONE', *, *, #28854, .T. ) ;
#67990 = DIRECTION ( 'NONE',  ( 0.000000000000000000, 0.000000000000000000, -1.000000000000000000 ) ) ;
#67991 = CARTESIAN_POINT ( 'NONE',  ( -94.99999999999997158, -207.3369185715606307, 78.05406250086714692 ) ) ;
#67992 = VERTEX_POINT ( 'NONE', #23813 ) ;
#67993 = AXIS2_PLACEMENT_3D ( 'NONE', #42894, #60559, #31959 ) ;
#67994 = ORIENTED_EDGE ( 'NONE', *, *, #71768, .T. ) ;
#67995 = CARTESIAN_POINT ( 'NONE',  ( 92.52185191531251007, -209.9999999999999716, 89.90078125043358170 ) ) ;
#67996 = EDGE_LOOP ( 'NONE', ( #4541, #64098, #27588, #13354 ) ) ;
#67997 = CARTESIAN_POINT ( 'NONE',  ( -3.000000000000000000, -23.29833615347104825, -3.418703333116803744 ) ) ;
#67998 = CARTESIAN_POINT ( 'NONE',  ( 0.000000000000000000, 32.34446384430010113, -26.79245525562679831 ) ) ;
#67999 = EDGE_LOOP ( 'NONE', ( #49644, #31748, #11644, #314 ) ) ;
#68000 = CARTESIAN_POINT ( 'NONE',  ( -94.99999999999997158, -207.3369185715606307, 77.41906250086714181 ) ) ;
#68001 = ORIENTED_EDGE ( 'NONE', *, *, #16528, .F. ) ;
#68003 = EDGE_CURVE ( 'NONE', #31034, #14108, #40365, .T. ) ;
#68002 = DIRECTION ( 'NONE',  ( -0.000000000000000000, -0.000000000000000000, -1.000000000000000000 ) ) ;
#68004 = DIRECTION ( 'NONE',  ( 0.000000000000000000, 0.9510565162951523099, 0.3090169943749513926 ) ) ;
#68005 = FACE_BOUND ( 'NONE', #29215, .T. ) ;
#68006 = CYLINDRICAL_SURFACE ( 'NONE', #19480, 32.00000000000000000 ) ;
#68007 = CARTESIAN_POINT ( 'NONE',  ( 10.00000000000000000, -25.88420570971419821, 27.13269053701087330 ) ) ;
#68008 = UNCERTAINTY_MEASURE_WITH_UNIT (LENGTH_MEASURE( 1.000000000000000082E-05 ), #46513, 'distance_accuracy_value', 'NONE');
#68009 = SURFACE_SIDE_STYLE ('',( #4882 ) ) ;
#68010 = CARTESIAN_POINT ( 'NONE',  ( 92.69370383062498320, 90.00000000000002842, 83.29281250086714294 ) ) ;
#68011 = CYLINDRICAL_SURFACE ( 'NONE', #20787, 82.00000000000000000 ) ;
#68012 = CARTESIAN_POINT ( 'NONE',  ( -10.00000000000000000, 0.000000000000000000, 0.000000000000000000 ) ) ;
#68013 = CARTESIAN_POINT ( 'NONE',  ( 97.64999999999999147, -209.9999999999999716, 86.50750000000000739 ) ) ;
#68014 = LINE ( 'NONE', #16507, #62855 ) ;
#68015 = LINE ( 'NONE', #37957, #42866 ) ;
#68016 = EDGE_CURVE ( 'NONE', #30226, #35224, #40004, .T. ) ;
#68017 = CARTESIAN_POINT ( 'NONE',  ( 4.999999999999999112, -10.41901085202050581, -40.68715046381939970 ) ) ;
#68018 = FACE_OUTER_BOUND ( 'NONE', #21949, .T. ) ;
#68019 = ADVANCED_FACE ( 'NONE', ( #22721 ), #52378, .F. ) ;
#68020 = CARTESIAN_POINT ( 'NONE',  ( -92.35000000000016485, 91.52997821335260653, 75.76541666666668107 ) ) ;
#68021 = ADVANCED_FACE ( 'NONE', ( #29435 ), #927, .T. ) ;
#68022 = AXIS2_PLACEMENT_3D ( 'NONE', #26736, #55319, #33116 ) ;
#68023 = CYLINDRICAL_SURFACE ( 'NONE', #60102, 16.00000000000000000 ) ;
#68024 = DIRECTION ( 'NONE',  ( -1.000000000000000000, -0.000000000000000000, -0.000000000000000000 ) ) ;
#68025 = DIRECTION ( 'NONE',  ( 0.000000000000000000, 0.1564344650402244852, 0.9876883405951387696 ) ) ;
#68026 = DIRECTION ( 'NONE',  ( 0.000000000000000000, -0.9876883405951359940, -0.1564344650402420267 ) ) ;
#68027 = VECTOR ( 'NONE', #11613, 1000.000000000000000 ) ;
#68028 = CARTESIAN_POINT ( 'NONE',  ( -92.34999999999999432, -208.4700217866474645, 84.65541666666666742 ) ) ;
#68029 = AXIS2_PLACEMENT_3D ( 'NONE', #42730, #73135, #8526 ) ;
#68030 = DIRECTION ( 'NONE',  ( -1.000000000000000000, -0.000000000000000000, -0.000000000000000000 ) ) ;
#68031 = PRODUCT ( 'fast gear_ISO - Spur gear 2M 40T 20PA 10FW ---S40A75H50L38.0N', 'fast gear_ISO - Spur gear 2M 40T 20PA 10FW ---S40A75H50L38.0N', '', ( #39966 ) ) ;
#68032 = VECTOR ( 'NONE', #62776, 1000.000000000000114 ) ;
#68033 = VERTEX_POINT ( 'NONE', #18173 ) ;
#68034 = CARTESIAN_POINT ( 'NONE',  ( 0.000000000000000000, -12.26510123303284594, 35.53030884539080603 ) ) ;
#68035 = DIRECTION ( 'NONE',  ( -0.000000000000000000, -0.000000000000000000, 1.000000000000000000 ) ) ;
#68036 = CARTESIAN_POINT ( 'NONE',  ( 11.99999999999999822, -77.19088730480528682, 6.903761155837505825 ) ) ;
#68037 = DIRECTION ( 'NONE',  ( -1.000000000000000000, -0.000000000000000000, -0.000000000000000000 ) ) ;
#68038 = CARTESIAN_POINT ( 'NONE',  ( 95.00000000000000000, -207.3369185715606307, 85.19781250086714408 ) ) ;
#68039 = ORIENTED_EDGE ( 'NONE', *, *, #28931, .T. ) ;
#68040 = EDGE_LOOP ( 'NONE', ( #55353, #68360, #52911, #1349 ) ) ;
#68041 = DIRECTION ( 'NONE',  ( -0.6575728627325954090, 0.7533909544171998318, 0.000000000000000000 ) ) ;
#68042 = ORIENTED_EDGE ( 'NONE', *, *, #62837, .F. ) ;
#68043 = CARTESIAN_POINT ( 'NONE',  ( 5.999999999999999112, 51.29473840253317007, -63.97538442413369353 ) ) ;
#68044 = CARTESIAN_POINT ( 'NONE',  ( 97.30629616937498838, -209.9999999999999716, 79.80031250086713612 ) ) ;
#68045 = ORIENTED_EDGE ( 'NONE', *, *, #54074, .F. ) ;
#68046 = CARTESIAN_POINT ( 'NONE',  ( 93.84685191531249870, -208.0026889286704943, 83.34572916753383254 ) ) ;
#68047 = ADVANCED_FACE ( 'NONE', ( #34349 ), #45660, .T. ) ;
#68048 = VERTEX_POINT ( 'NONE', #29808 ) ;
#68049 = FACE_OUTER_BOUND ( 'NONE', #3120, .T. ) ;
#68050 = VERTEX_POINT ( 'NONE', #57290 ) ;
#68051 = VERTEX_POINT ( 'NONE', #40744 ) ;
#68052 = SURFACE_STYLE_USAGE ( .BOTH. , #56783 ) ;
#68053 = CARTESIAN_POINT ( 'NONE',  ( 15.70000000000000284, -120.0000000000000000, -85.59999999999999432 ) ) ;
#68054 = EDGE_CURVE ( 'NONE', #20087, #70347, #47578, .T. ) ;
#68055 = ORIENTED_EDGE ( 'NONE', *, *, #2771, .T. ) ;
#68056 = CARTESIAN_POINT ( 'NONE',  ( 10.00000000000000000, 54.21277698773675979, 55.38113227695801299 ) ) ;
#68057 = DIRECTION ( 'NONE',  ( -1.000000000000000000, 0.000000000000000000, 0.000000000000000000 ) ) ;
#68058 = EDGE_CURVE ( 'NONE', #8769, #37081, #71544, .T. ) ;
#68059 = ORIENTED_EDGE ( 'NONE', *, *, #66459, .F. ) ;
#68060 = FACE_OUTER_BOUND ( 'NONE', #74148, .T. ) ;
#68061 = ORIENTED_EDGE ( 'NONE', *, *, #34023, .F. ) ;
#68062 = FACE_OUTER_BOUND ( 'NONE', #41151, .T. ) ;
#68063 = CIRCLE ( 'NONE', #54861, 31.99999999999999645 ) ;
#68064 = ORIENTED_EDGE ( 'NONE', *, *, #32516, .T. ) ;
#68065 = ADVANCED_FACE ( 'NONE', ( #6175 ), #24193, .T. ) ;
#68066 = VERTEX_POINT ( 'NONE', #39637 ) ;
#68067 = VERTEX_POINT ( 'NONE', #52006 ) ;
#68068 = CARTESIAN_POINT ( 'NONE',  ( 92.69370383062501162, -209.9999999999999716, 75.67281250086713840 ) ) ;
#68069 = CONTEXT_DEPENDENT_SHAPE_REPRESENTATION ( #25359, #30866 ) ;
#68070 = DIRECTION ( 'NONE',  ( -1.000000000000000000, 0.000000000000000000, -0.000000000000000000 ) ) ;
#68071 = ORIENTED_EDGE ( 'NONE', *, *, #7634, .F. ) ;
#68072 = VERTEX_POINT ( 'NONE', #5803 ) ;
#68073 = AXIS2_PLACEMENT_3D ( 'NONE', #40206, #63889, #46219 ) ;
#68074 = ORIENTED_EDGE ( 'NONE', *, *, #30134, .F. ) ;
#68075 = AXIS2_PLACEMENT_3D ( 'NONE', #18229, #30605, #12585 ) ;
#68076 = DIRECTION ( 'NONE',  ( 0.000000000000000000, 0.000000000000000000, 1.000000000000000000 ) ) ;
#68077 = DIRECTION ( 'NONE',  ( 0.000000000000000000, 0.9876883405951383255, -0.1564344650402277048 ) ) ;
#68078 = CARTESIAN_POINT ( 'NONE',  ( -92.69370383062504004, 89.06968786819598449, 74.84209103131394158 ) ) ;
#68079 = ORIENTED_EDGE ( 'NONE', *, *, #55443, .T. ) ;
#68080 = CIRCLE ( 'NONE', #54875, 2.541999999999999815 ) ;
#68081 = ADVANCED_FACE ( 'NONE', ( #58027 ), #53529, .F. ) ;
#68082 = CARTESIAN_POINT ( 'NONE',  ( 92.69370383062498320, 90.00000000000002842, 75.03781250086713328 ) ) ;
#68083 = AXIS2_PLACEMENT_3D ( 'NONE', #473, #46300, #40660 ) ;
#68084 = ORIENTED_EDGE ( 'NONE', *, *, #22354, .F. ) ;
#68085 = CARTESIAN_POINT ( 'NONE',  ( 93.67499999999998295, 92.29496732002878900, 75.28916666666665947 ) ) ;
#68086 = CARTESIAN_POINT ( 'NONE',  ( -92.69370383062498320, -211.3315407142195852, 84.82739583420045903 ) ) ;
#68087 = ORIENTED_EDGE ( 'NONE', *, *, #53406, .F. ) ;
#68089 = EDGE_CURVE ( 'NONE', #52810, #67503, #69675, .T. ) ;
#68088 = DIRECTION ( 'NONE',  ( -1.000000000000000000, -0.000000000000000000, -0.000000000000000000 ) ) ;
#68090 = DIRECTION ( 'NONE',  ( 1.000000000000000000, 0.000000000000000000, 0.000000000000000000 ) ) ;
#68091 = CARTESIAN_POINT ( 'NONE',  ( 92.35000000000000853, -209.9999999999999716, 88.09499999999999886 ) ) ;
#68092 = CARTESIAN_POINT ( 'NONE',  ( -93.84685191531248449, -208.0026889286704943, 78.00114583420048575 ) ) ;
#68093 = LINE ( 'NONE', #4212, #49449 ) ;
#68094 = CYLINDRICAL_SURFACE ( 'NONE', #21156, 2.649999999999999467 ) ;
#68095 = CARTESIAN_POINT ( 'NONE',  ( 0.000000000000000000, 66.50666863322055633, -39.78640506895536078 ) ) ;
#68096 = AXIS2_PLACEMENT_3D ( 'NONE', #26521, #31046, #2888 ) ;
#68097 = DIRECTION ( 'NONE',  ( -0.1045284632676570929, 0.9945218953682730678, 0.000000000000000000 ) ) ;
#68098 = LINE ( 'NONE', #45558, #20744 ) ;
#68099 = CIRCLE ( 'NONE', #2072, 15.99999999999999822 ) ;
#68100 = CARTESIAN_POINT ( 'NONE',  ( 94.68886060456939902, -207.6265741463516861, 74.84415580543368662 ) ) ;
#68101 = ADVANCED_FACE ( 'NONE', ( #48135 ), #16699, .F. ) ;
#68102 = CARTESIAN_POINT ( 'NONE',  ( -96.15314808468752972, 91.99731107132950569, 81.91697916753381037 ) ) ;
#68103 = DIRECTION ( 'NONE',  ( 0.000000000000000000, 0.000000000000000000, 1.000000000000000000 ) ) ;
#68104 = CARTESIAN_POINT ( 'NONE',  ( 11.99999999999999822, 0.000000000000000000, 0.000000000000000000 ) ) ;
#68105 = EDGE_CURVE ( 'NONE', #10838, #57712, #31567, .T. ) ;
#68106 = VERTEX_POINT ( 'NONE', #3771 ) ;
#68107 = DIRECTION ( 'NONE',  ( 0.000000000000000000, 0.000000000000000000, -1.000000000000000000 ) ) ;
#68108 = CARTESIAN_POINT ( 'NONE',  ( 0.000000000000000000, 35.47612816024556537, -22.48208911017461631 ) ) ;
#68109 = DIRECTION ( 'NONE',  ( 1.000000000000000000, 1.427937372958405461E-15, 7.962523111839130290E-16 ) ) ;
#68110 = DIRECTION ( 'NONE',  ( -1.000000000000000000, 0.000000000000000000, 0.000000000000000000 ) ) ;
#68111 = DIRECTION ( 'NONE',  ( 0.000000000000000000, -0.3826834323650772363, -0.9238795325112919565 ) ) ;
#68112 = CARTESIAN_POINT ( 'NONE',  ( -93.67500000000003979, 92.29496732002878900, 87.24833333333333485 ) ) ;
#68113 = CARTESIAN_POINT ( 'NONE',  ( -97.30629616937497417, -211.3315407142195852, 78.42447916753380355 ) ) ;
#68114 = DIRECTION ( 'NONE',  ( 0.000000000000000000, -0.9723699203976740035, -0.2334453638559160216 ) ) ;
#68115 =( BOUNDED_CURVE ( )  B_SPLINE_CURVE ( 2, ( #56541, #38496, #10292, #5418, #44518, #61436, #68179 ),
 .UNSPECIFIED., .F., .F. ) 
 B_SPLINE_CURVE_WITH_KNOTS ( ( 3, 2, 2, 3 ),
 ( 0.2083333333333331483, 0.2152777777777775681, 0.2222222222222219323, 0.2291666666666663521 ),
 .UNSPECIFIED. ) 
 CURVE ( )  GEOMETRIC_REPRESENTATION_ITEM ( )  RATIONAL_B_SPLINE_CURVE ( ( 1.000000000000003775, 0.8660254037844349329, 1.000000000000000000, 0.8660254037844387076, 1.000000000000000000, 0.8660254037844445918, 0.9999999999999941158 ) ) 
 REPRESENTATION_ITEM ( '' )  );
#68116 = ORIENTED_EDGE ( 'NONE', *, *, #9582, .F. ) ;
#68117 = AXIS2_PLACEMENT_3D ( 'NONE', #7622, #73539, #5152 ) ;
#68118 = DIRECTION ( 'NONE',  ( -1.000000000000000000, -0.000000000000000000, -0.000000000000000000 ) ) ;
#68119 = CARTESIAN_POINT ( 'NONE',  ( 92.35003715139256997, 91.52999966271907795, 76.69145685134850510 ) ) ;
#68120 = CARTESIAN_POINT ( 'NONE',  ( 10.00000000000000000, 0.000000000000000000, 0.000000000000000000 ) ) ;
#68121 = CONICAL_SURFACE ( 'NONE', #9294, 5.000000000000000888, 1.047197551196596299 ) ;
#68122 = CARTESIAN_POINT ( 'NONE',  ( 92.35000000046409241, 89.99996903277681781, 77.38038495127642591 ) ) ;
#68123 = LINE ( 'NONE', #73375, #24600 ) ;
#68124 = CIRCLE ( 'NONE', #51316, 5.000000000000000888 ) ;
#68125 = LINE ( 'NONE', #16619, #70784 ) ;
#68126 = VERTEX_POINT ( 'NONE', #15391 ) ;
#68127 = DIRECTION ( 'NONE',  ( 0.000000000000000000, 0.000000000000000000, 1.000000000000000000 ) ) ;
#68128 = CARTESIAN_POINT ( 'NONE',  ( -94.95306897617113862, 87.35041560265752025, 75.00000002508417651 ) ) ;
#68129 = ORIENTED_EDGE ( 'NONE', *, *, #19751, .T. ) ;
#68130 = CARTESIAN_POINT ( 'NONE',  ( 96.15314808468748708, -208.0026889286704943, 86.89114583420047211 ) ) ;
#68131 = CARTESIAN_POINT ( 'NONE',  ( -96.32500000000001705, 92.29496732002878900, 77.82916666666665151 ) ) ;
#68132 = ORIENTED_EDGE ( 'NONE', *, *, #57472, .T. ) ;
#68133 = EDGE_CURVE ( 'NONE', #7284, #42705, #40332, .T. ) ;
#68134 = CARTESIAN_POINT ( 'NONE',  ( 10.00000000000000000, 0.000000000000000000, 0.000000000000000000 ) ) ;
#68135 = ORIENTED_EDGE ( 'NONE', *, *, #7793, .F. ) ;
#68136 = DIRECTION ( 'NONE',  ( -0.000000000000000000, 0.8660254037844368202, 0.5000000000000031086 ) ) ;
#68137 = ORIENTED_EDGE ( 'NONE', *, *, #37157, .F. ) ;
#68138 = CARTESIAN_POINT ( 'NONE',  ( 10.00000000000000000, -74.18225833017864090, -34.94270380257719211 ) ) ;
#68139 = EDGE_CURVE ( 'NONE', #11963, #66021, #66541, .T. ) ;
#68140 = VECTOR ( 'NONE', #73581, 1000.000000000000000 ) ;
#68141 = ORIENTED_EDGE ( 'NONE', *, *, #19318, .F. ) ;
#68142 = ORIENTED_EDGE ( 'NONE', *, *, #65801, .T. ) ;
#68143 = EDGE_CURVE ( 'NONE', #23740, #53644, #3272, .T. ) ;
#68144 = ADVANCED_FACE ( 'NONE', ( #43255 ), #27033, .F. ) ;
#68145 = ORIENTED_EDGE ( 'NONE', *, *, #66949, .F. ) ;
#68146 = FACE_OUTER_BOUND ( 'NONE', #70077, .T. ) ;
#68147 = AXIS2_PLACEMENT_3D ( 'NONE', #62913, #11371, #57249 ) ;
#68148 = ORIENTED_EDGE ( 'NONE', *, *, #40336, .F. ) ;
#68149 = VERTEX_POINT ( 'NONE', #9759 ) ;
#68150 = CARTESIAN_POINT ( 'NONE',  ( 97.64999999999999147, 90.00000000000002842, 87.14249999999999829 ) ) ;
#68151 = CARTESIAN_POINT ( 'NONE',  ( 10.00000000000000000, 74.65491531819105830, 8.830959090343693418 ) ) ;
#68152 = FACE_OUTER_BOUND ( 'NONE', #70047, .T. ) ;
#68153 = EDGE_LOOP ( 'NONE', ( #40510, #33099, #13485, #28996 ) ) ;
#68154 = ORIENTED_EDGE ( 'NONE', *, *, #24846, .T. ) ;
#68155 = EDGE_CURVE ( 'NONE', #55889, #18738, #49232, .T. ) ;
#68156 = ORIENTED_EDGE ( 'NONE', *, *, #17644, .T. ) ;
#68157 = CARTESIAN_POINT ( 'NONE',  ( 97.30629616937498838, 91.33154071421968467, 86.20322916753382003 ) ) ;
#68158 = VERTEX_POINT ( 'NONE', #48861 ) ;
#68159 = CARTESIAN_POINT ( 'NONE',  ( 92.69370383062501162, -211.3315407142195852, 85.25072916753379104 ) ) ;
#68160 = CARTESIAN_POINT ( 'NONE',  ( 11.99999999999999822, 0.000000000000000000, 0.000000000000000000 ) ) ;
#68161 = DIRECTION ( 'NONE',  ( -1.000000000000000000, 0.000000000000000000, 0.000000000000000000 ) ) ;
#68162 = CARTESIAN_POINT ( 'NONE',  ( -96.32500000000001705, 92.29496732002878900, 77.90854166840097150 ) ) ;
#68163 = LINE ( 'NONE', #35429, #1994 ) ;
#68164 = CARTESIAN_POINT ( 'NONE',  ( 2.949999999999999734, 3.306546357697853240E-16, -2.699999999999999734 ) ) ;
#68165 = DIRECTION ( 'NONE',  ( 0.000000000000000000, 0.9238795325112851842, 0.3826834323650938341 ) ) ;
#68166 = CARTESIAN_POINT ( 'NONE',  ( -96.15314808468747287, -208.0026889286704943, 86.36197916753381776 ) ) ;
#68167 = CARTESIAN_POINT ( 'NONE',  ( -95.00000000000002842, 87.33691857156074434, 86.78531250086716398 ) ) ;
#68168 = ORIENTED_EDGE ( 'NONE', *, *, #50263, .F. ) ;
#68169 = ADVANCED_FACE ( 'NONE', ( #31937, #42497 ), #37961, .T. ) ;
#68171 = CARTESIAN_POINT ( 'NONE',  ( -96.15314808468752972, 91.99731107132950569, 85.09197916753380753 ) ) ;
#68170 = CARTESIAN_POINT ( 'NONE',  ( 92.69370383062498320, 88.66845928578037217, 85.25072916753379104 ) ) ;
#68172 = ORIENTED_EDGE ( 'NONE', *, *, #29780, .T. ) ;
#68173 = LINE ( 'NONE', #16300, #71851 ) ;
#68174 = VECTOR ( 'NONE', #62724, 1000.000000000000000 ) ;
#68176 = EDGE_CURVE ( 'NONE', #47415, #43524, #60897, .T. ) ;
#68175 = CARTESIAN_POINT ( 'NONE',  ( 11.99999999999999822, 0.000000000000000000, 0.000000000000000000 ) ) ;
#68177 = LINE ( 'NONE', #21180, #54703 ) ;
#68178 = DIRECTION ( 'NONE',  ( 0.000000000000000000, 0.000000000000000000, 1.000000000000000000 ) ) ;
#68179 = CARTESIAN_POINT ( 'NONE',  ( -92.35000000000003695, 90.00000000000004263, 86.50750000000000739 ) ) ;
#68180 =( GEOMETRIC_REPRESENTATION_CONTEXT ( 3 ) GLOBAL_UNCERTAINTY_ASSIGNED_CONTEXT ( ( #34574 ) ) GLOBAL_UNIT_ASSIGNED_CONTEXT ( ( #70864, #30637, #52465 ) ) REPRESENTATION_CONTEXT ( 'NONE', 'WORKASPACE' ) );
#68181 = CARTESIAN_POINT ( 'NONE',  ( 16.84844760790522855, -103.5491698323862124, 5.500000000000000000 ) ) ;
#68182 = CARTESIAN_POINT ( 'NONE',  ( 0.000000000000000000, 0.000000000000000000, 0.000000000000000000 ) ) ;
#68183 = DIRECTION ( 'NONE',  ( 0.000000000000000000, -0.000000000000000000, -1.000000000000000000 ) ) ;
#68184 = EDGE_CURVE ( 'NONE', #7708, #70437, #33173, .T. ) ;
#68185 = ADVANCED_FACE ( 'NONE', ( #54513 ), #65435, .F. ) ;
#68186 = DIRECTION ( 'NONE',  ( 0.000000000000000000, 0.8910065241883688980, -0.4539904997395447506 ) ) ;
#68187 = EDGE_LOOP ( 'NONE', ( #61216, #17312, #27003, #2191 ) ) ;
#68188 = AXIS2_PLACEMENT_3D ( 'NONE', #54863, #27389, #50331 ) ;
#68189 = ORIENTED_EDGE ( 'NONE', *, *, #3686, .T. ) ;
#68190 = CIRCLE ( 'NONE', #5791, 31.99999999999998579 ) ;
#68191 = CARTESIAN_POINT ( 'NONE',  ( -92.35000000000005116, 88.47002178664754979, 79.46958333333333258 ) ) ;
#68192 = DIRECTION ( 'NONE',  ( 0.000000000000000000, 0.000000000000000000, -1.000000000000000000 ) ) ;
#68193 = EDGE_CURVE ( 'NONE', #1816, #9559, #12790, .T. ) ;
#68194 = CARTESIAN_POINT ( 'NONE',  ( -92.35000000000000853, 88.47002178664756400, 78.83458333333334167 ) ) ;
#68195 = CARTESIAN_POINT ( 'NONE',  ( -100.0000000000000142, 95.00000000000002842, 90.00000000000000000 ) ) ;
#68196 = LINE ( 'NONE', #10306, #23111 ) ;
#68197 = DIRECTION ( 'NONE',  ( -1.000000000000000000, -0.000000000000000000, -0.000000000000000000 ) ) ;
#68198 = DIRECTION ( 'NONE',  ( 0.000000000000000000, 0.000000000000000000, -1.000000000000000000 ) ) ;
#68199 = CARTESIAN_POINT ( 'NONE',  ( 10.00000000000000000, 81.50828551894225882, 8.966570791700975818 ) ) ;
#68200 = ORIENTED_EDGE ( 'NONE', *, *, #4976, .T. ) ;
#68201 = CARTESIAN_POINT ( 'NONE',  ( -97.30629616937501680, 91.33154071421968467, 78.15989583420048348 ) ) ;
#68202 = EDGE_CURVE ( 'NONE', #370, #2973, #25564, .T. ) ;
#68203 = PLANE ( 'NONE',  #37969 ) ;
#68204 = CARTESIAN_POINT ( 'NONE',  ( 0.000000000000000000, -77.16300072079641836, -27.74655509720751567 ) ) ;
#68205 = AXIS2_PLACEMENT_3D ( 'NONE', #61864, #22377, #29388 ) ;
#68206 = DIRECTION ( 'NONE',  ( 0.000000000000000000, -0.000000000000000000, 1.000000000000000000 ) ) ;
#68207 = CARTESIAN_POINT ( 'NONE',  ( -8.637688417678548447, 13.69818742750669571, -45.00000000000000000 ) ) ;
#68208 = VECTOR ( 'NONE', #36719, 1000.000000000000000 ) ;
#68209 = CARTESIAN_POINT ( 'NONE',  ( 0.000000000000000000, 0.000000000000000000, 0.000000000000000000 ) ) ;
#68210 = CARTESIAN_POINT ( 'NONE',  ( -96.15314808468745866, -211.9973110713294489, 88.63739583420048973 ) ) ;
#68211 =( NAMED_UNIT ( * ) PLANE_ANGLE_UNIT ( ) SI_UNIT ( $, .RADIAN. ) );
#68212 = VECTOR ( 'NONE', #61570, 1000.000000000000000 ) ;
#68213 = CIRCLE ( 'NONE', #41790, 31.99999999999998579 ) ;
#68214 = VECTOR ( 'NONE', #54977, 1000.000000000000000 ) ;
#68215 = CARTESIAN_POINT ( 'NONE',  ( 94.99999999999998579, 92.66308142843932671, 76.30781250086715772 ) ) ;
#68216 = CARTESIAN_POINT ( 'NONE',  ( -92.69370383062498320, -211.3315407142195852, 81.17614583420049712 ) ) ;
#68217 = CARTESIAN_POINT ( 'NONE',  ( 12.00000000000000000, -20.55727247249748402, -16.78983467731284307 ) ) ;
#68218 = ORIENTED_EDGE ( 'NONE', *, *, #32730, .T. ) ;
#68219 = CARTESIAN_POINT ( 'NONE',  ( 0.000000000000000000, 5.817072295949927426E-16, -4.750000000000000000 ) ) ;
#68220 = CARTESIAN_POINT ( 'NONE',  ( -97.64999999999994884, -208.4700217866474645, 75.34208333333333485 ) ) ;
#68221 = CARTESIAN_POINT ( 'NONE',  ( 10.00000000000000000, 12.26510123303308752, -35.53030884539072787 ) ) ;
#68222 = CARTESIAN_POINT ( 'NONE',  ( -92.69370383062505425, 91.33154071421968467, 77.47197916753381719 ) ) ;
#68223 = CARTESIAN_POINT ( 'NONE',  ( 93.84685191531251292, -211.9973110713294489, 78.95364583420047211 ) ) ;
#68224 = ORIENTED_EDGE ( 'NONE', *, *, #50828, .F. ) ;
#68225 = DIRECTION ( 'NONE',  ( 0.000000000000000000, 0.000000000000000000, 1.000000000000000000 ) ) ;
#68226 = ORIENTED_EDGE ( 'NONE', *, *, #66288, .F. ) ;
#68227 = STYLED_ITEM ( 'NONE', ( #7406 ), #62646 ) ;
#68228 = FACE_OUTER_BOUND ( 'NONE', #7792, .T. ) ;
#68229 = ORIENTED_EDGE ( 'NONE', *, *, #33439, .F. ) ;
#68230 = AXIS2_PLACEMENT_3D ( 'NONE', #73079, #44912, #10683 ) ;
#68231 = AXIS2_PLACEMENT_3D ( 'NONE', #24738, #47666, #70575 ) ;
#68232 = ADVANCED_FACE ( 'NONE', ( #48500 ), #71412, .F. ) ;
#68233 = CARTESIAN_POINT ( 'NONE',  ( 11.99999999999999822, -75.54627589209955829, 17.28742895386058009 ) ) ;
#68234 = VECTOR ( 'NONE', #3125, 1000.000000000000000 ) ;
#68235 = EDGE_CURVE ( 'NONE', #23492, #17876, #48794, .T. ) ;
#68236 = ORIENTED_EDGE ( 'NONE', *, *, #14699, .F. ) ;
#68237 = ORIENTED_EDGE ( 'NONE', *, *, #62510, .F. ) ;
#68238 = AXIS2_PLACEMENT_3D ( 'NONE', #26951, #25574, #67562 ) ;
#68240 = EDGE_CURVE ( 'NONE', #20251, #18486, #24820, .T. ) ;
#68239 = ORIENTED_EDGE ( 'NONE', *, *, #73262, .F. ) ;
#68241 = EDGE_CURVE ( 'NONE', #42731, #43669, #74017, .T. ) ;
#68242 = CARTESIAN_POINT ( 'NONE',  ( 92.69370383062501162, -211.3315407142195852, 75.88447916753382572 ) ) ;
#68243 = ORIENTED_EDGE ( 'NONE', *, *, #13917, .T. ) ;
#68244 = DIRECTION ( 'NONE',  ( 0.000000000000000000, 0.000000000000000000, -1.000000000000000000 ) ) ;
#68245 = DIRECTION ( 'NONE',  ( 0.000000000000000000, 0.000000000000000000, 1.000000000000000000 ) ) ;
#68246 = CARTESIAN_POINT ( 'NONE',  ( 93.84685191531248449, 88.00268892867053694, 84.82739583420048746 ) ) ;
#68247 = LINE ( 'NONE', #21626, #52573 ) ;
#68248 = CARTESIAN_POINT ( 'NONE',  ( 93.67500000000001137, -207.7050326799711968, 79.73416666666666686 ) ) ;
#68249 = EDGE_LOOP ( 'NONE', ( #20833, #11574, #39190, #18383 ) ) ;
#68250 = ORIENTED_EDGE ( 'NONE', *, *, #19318, .T. ) ;
#68251 = ORIENTED_EDGE ( 'NONE', *, *, #12913, .F. ) ;
#68252 = ORIENTED_EDGE ( 'NONE', *, *, #53661, .F. ) ;
#68253 = CARTESIAN_POINT ( 'NONE',  ( 11.99999999999999822, 55.38113227695858143, -54.21277698773617715 ) ) ;
#68254 = AXIS2_PLACEMENT_3D ( 'NONE', #3814, #60217, #26349 ) ;
#68255 = DIRECTION ( 'NONE',  ( -0.000000000000000000, -0.000000000000000000, 1.000000000000000000 ) ) ;
#68256 = FACE_OUTER_BOUND ( 'NONE', #68364, .T. ) ;
#68257 = CIRCLE ( 'NONE', #16616, 16.00000000000000000 ) ;
#68258 = CARTESIAN_POINT ( 'NONE',  ( -3.000000000000000000, 0.000000000000000000, 0.000000000000000000 ) ) ;
#68259 = CARTESIAN_POINT ( 'NONE',  ( 10.00000000000000000, -80.28980883073744224, -16.65972982745018882 ) ) ;
#68260 = VECTOR ( 'NONE', #68136, 999.9999999999998863 ) ;
#68261 = EDGE_CURVE ( 'NONE', #4576, #33591, #42794, .T. ) ;
#68262 = DIRECTION ( 'NONE',  ( -0.000000000000000000, -0.000000000000000000, -1.000000000000000000 ) ) ;
#68263 = ORIENTED_EDGE ( 'NONE', *, *, #58712, .T. ) ;
#68264 = CARTESIAN_POINT ( 'NONE',  ( -97.64999999999994884, -208.4700217866474645, 84.31145833506762699 ) ) ;
#68265 = ORIENTED_EDGE ( 'NONE', *, *, #29521, .T. ) ;
#68266 = DIRECTION ( 'NONE',  ( 0.000000000000000000, 0.000000000000000000, 1.000000000000000000 ) ) ;
#68267 = VERTEX_POINT ( 'NONE', #11244 ) ;
#68269 = CARTESIAN_POINT ( 'NONE',  ( -95.00000000000002842, 93.05995642670501411, 79.12562500173429214 ) ) ;
#68268 = CARTESIAN_POINT ( 'NONE',  ( 92.34999999999999432, 91.52997821335252127, 81.77145833506763495 ) ) ;
#68270 = PRESENTATION_LAYER_ASSIGNMENT (  '', '', ( #58649 ) ) ;
#68271 = VERTEX_POINT ( 'NONE', #18 ) ;
#68272 = CARTESIAN_POINT ( 'NONE',  ( 93.84685191531248449, 91.99731107132950569, 83.34572916753383254 ) ) ;
#68273 = CARTESIAN_POINT ( 'NONE',  ( -92.35000000000000853, 88.47002178664759242, 76.29458333333333542 ) ) ;
#68274 = CARTESIAN_POINT ( 'NONE',  ( -94.99999999999997158, -213.0599564267049857, 82.61812500173428475 ) ) ;
#68275 = CARTESIAN_POINT ( 'NONE',  ( 11.99999999999999822, 6.903761155837791819, 77.19088730480525840 ) ) ;
#68276 = DIRECTION ( 'NONE',  ( 1.000000000000000000, 0.000000000000000000, 0.000000000000000000 ) ) ;
#68277 = DIRECTION ( 'NONE',  ( 0.000000000000000000, 0.1045284632676558162, 0.9945218953682731788 ) ) ;
#68278 = ORIENTED_EDGE ( 'NONE', *, *, #59160, .T. ) ;
#68279 = CARTESIAN_POINT ( 'NONE',  ( 0.000000000000000000, -66.50666863321973210, -39.78640506895674633 ) ) ;
#68280 = DIRECTION ( 'NONE',  ( -1.000000000000000000, 0.000000000000000000, 0.000000000000000000 ) ) ;
#68281 = EDGE_CURVE ( 'NONE', #50461, #15716, #22415, .T. ) ;
#68282 = EDGE_CURVE ( 'NONE', #70758, #11833, #63214, .T. ) ;
#68283 = CARTESIAN_POINT ( 'NONE',  ( 11.99999999999999822, 0.000000000000000000, 0.000000000000000000 ) ) ;
#68284 = VERTEX_POINT ( 'NONE', #38707 ) ;
#68285 = ORIENTED_EDGE ( 'NONE', *, *, #24271, .F. ) ;
#68286 = CARTESIAN_POINT ( 'NONE',  ( 95.00000000000000000, -209.9999999999999716, 90.00000000000000000 ) ) ;
#68287 = DIRECTION ( 'NONE',  ( -1.000000000000000000, 0.000000000000000000, 0.000000000000000000 ) ) ;
#68288 = CARTESIAN_POINT ( 'NONE',  ( -2.499999999999970690, 73.00000000000001421, -251.7000000000000455 ) ) ;
#68289 = DIRECTION ( 'NONE',  ( 0.000000000000000000, 0.000000000000000000, 1.000000000000000000 ) ) ;
#68290 = CARTESIAN_POINT ( 'NONE',  ( -92.69370383062498320, -211.3315407142195852, 81.81114583420048803 ) ) ;
#68291 = ORIENTED_EDGE ( 'NONE', *, *, #301, .F. ) ;
#68292 = AXIS2_PLACEMENT_3D ( 'NONE', #12575, #5847, #46806 ) ;
#68293 = CARTESIAN_POINT ( 'NONE',  ( -92.69370383062502583, 88.66845928578038638, 87.36739583420047950 ) ) ;
#68294 = ORIENTED_EDGE ( 'NONE', *, *, #31789, .F. ) ;
#68295 = VECTOR ( 'NONE', #5737, 999.9999999999998863 ) ;
#68296 = FACE_OUTER_BOUND ( 'NONE', #3413, .T. ) ;
#68297 = CARTESIAN_POINT ( 'NONE',  ( -96.53982248241459274, -212.0954260604656270, 74.96680960279337569 ) ) ;
#68298 = DIRECTION ( 'NONE',  ( 0.000000000000000000, 0.000000000000000000, 1.000000000000000000 ) ) ;
#68299 = CARTESIAN_POINT ( 'NONE',  ( 92.69370383062498320, 88.66845928578035796, 76.36072916753381890 ) ) ;
#68300 = VECTOR ( 'NONE', #30837, 1000.000000000000000 ) ;
#68301 = FACE_OUTER_BOUND ( 'NONE', #25040, .T. ) ;
#68302 = CARTESIAN_POINT ( 'NONE',  ( 11.99999999999999822, -0.8261519478425843888, -77.49459641780887864 ) ) ;
#68303 = CARTESIAN_POINT ( 'NONE',  ( -93.67499999999998295, -207.7050326799711968, 78.99333333333332519 ) ) ;
#68304 = DIRECTION ( 'NONE',  ( 0.000000000000000000, -0.7431448254773862505, -0.6691306063588671194 ) ) ;
#68305 = DIRECTION ( 'NONE',  ( -1.000000000000000000, -0.000000000000000000, -0.000000000000000000 ) ) ;
#68306 = DIRECTION ( 'NONE',  ( 0.000000000000000000, 0.000000000000000000, 1.000000000000000000 ) ) ;
#68307 = FACE_OUTER_BOUND ( 'NONE', #45673, .T. ) ;
#68308 = CARTESIAN_POINT ( 'NONE',  ( 93.84685191531248449, 91.99731107132950569, 89.69572916753382685 ) ) ;
#68309 = AXIS2_PLACEMENT_3D ( 'NONE', #3207, #26096, #49026 ) ;
#68310 = DIRECTION ( 'NONE',  ( 0.000000000000000000, 0.000000000000000000, 1.000000000000000000 ) ) ;
#68311 = DIRECTION ( 'NONE',  ( -0.000000000000000000, -0.000000000000000000, 1.000000000000000000 ) ) ;
#68312 = AXIS2_PLACEMENT_3D ( 'NONE', #48965, #3145, #13147 ) ;
#68313 = EDGE_LOOP ( 'NONE', ( #61130, #57215, #29985 ) ) ;
#68314 = CARTESIAN_POINT ( 'NONE',  ( -93.09170270117147084, 88.16127723153179829, 74.99954709728268654 ) ) ;
#68315 = CARTESIAN_POINT ( 'NONE',  ( -96.15314808468752972, 91.99731107132950569, 80.64697916753381435 ) ) ;
#68316 = AXIS2_PLACEMENT_3D ( 'NONE', #15419, #66572, #45129 ) ;
#68317 = VECTOR ( 'NONE', #72264, 1000.000000000000000 ) ;
#68318 = CARTESIAN_POINT ( 'NONE',  ( 11.99999999999999822, 0.000000000000000000, 0.000000000000000000 ) ) ;
#68319 = EDGE_LOOP ( 'NONE', ( #70628, #61408, #7187, #7591 ) ) ;
#68320 = LINE ( 'NONE', #22830, #4282 ) ;
#68321 = CARTESIAN_POINT ( 'NONE',  ( 0.000000000000000000, 0.000000000000000000, 0.000000000000000000 ) ) ;
#68322 = CYLINDRICAL_SURFACE ( 'NONE', #7168, 31.99999999999999289 ) ;
#68323 = EDGE_CURVE ( 'NONE', #30043, #52162, #16143, .T. ) ;
#68324 = DIRECTION ( 'NONE',  ( -1.000000000000000000, 0.000000000000000000, 0.000000000000000000 ) ) ;
#68325 = CARTESIAN_POINT ( 'NONE',  ( 97.30629616937497417, -210.9303297190751891, 74.84209033237941355 ) ) ;
#68326 = EDGE_CURVE ( 'NONE', #11648, #26342, #66790, .T. ) ;
#68327 = VERTEX_POINT ( 'NONE', #22534 ) ;
#68328 = ORIENTED_EDGE ( 'NONE', *, *, #70774, .F. ) ;
#68329 = EDGE_CURVE ( 'NONE', #3158, #65921, #16893, .T. ) ;
#68330 = VECTOR ( 'NONE', #26724, 1000.000000000000000 ) ;
#68331 = FACE_OUTER_BOUND ( 'NONE', #27098, .T. ) ;
#68332 = CARTESIAN_POINT ( 'NONE',  ( -5.250000000000000888, -13.95926121303099343, 0.000000000000000000 ) ) ;
#68333 =( BOUNDED_SURFACE ( )  B_SPLINE_SURFACE ( 1, 2, ( 
 ( #70565, #64969, #20186, #31838, #59688, #36007, #13802, #37132, #71311, #25099, #3306, #30724, #13446, #58955, #36369, #59314, #70948, #19453, #65334, #8171, #54050, #2587, #60078, #48398, #19816, #42765, #37823, #61495, #3987, #49819, #22376, #72381, #73494, #44196, #15986, #3625, #38928, #55476, #62236, #73867, #5106, #61123, #22002, #72741, #49457, #21624, #56220, #44947, #9612, #21240, #32531, #32892, #26890, #4357, #67122, #67870, #15625, #50185, #38558, #55846, #9973, #60753, #16361, #27254, #56602, #4739, #61863, #39304, #73121, #44577, #43839, #67499, #9230, #10348, #33263, #27641, #66397, #14878, #20884, #28003, #32152, #50566, #55098, #66756, #15244, #10727, #33649, #50943, #26524, #38178, #52412, #45320, #16743, #52802, #68246, #57329, #62620, #1345, #18211, #17839, #40789, #17473, #39679, #23855, #5841, #29113, #34020, #28750, #40401, #58067, #51688, #234, #12194, #11097, #593, #23131, #6571, #63721, #46054, #52048, #69341, #23486, #69714, #963, #63350, #29475, #68983, #11815, #68625, #56968, #74240, #46799, #34770, #5478, #28376, #57706, #41152, #46418, #51306, #64092, #40039, #12566, #58430, #11456, #6214, #35135, #22763, #35504, #34389, #6924, #29846, #45698, #17109, #62997, #30958, #8040, #24590, #65570, #70432, #59183, #41885, #25340, #54643, #59934, #43003, #65940, #18938, #42629, #54286, #70071, #30588, #64829, #64454, #8421, #2458, #48635, #70816, #7309, #53909, #13306, #7672, #53536, #2075, #8784, #36606, #31335, #19681, #14038, #48266, #71176, #2810, #14421, #36239, #1705, #24957, #36980, #42270, #24237, #47893, #12925, #19313, #25701, #71555, #37369, #31700, #20052, #60308, #47163, #18573, #41514, #30229, #35860, #13674, #58813, #53170, #47529, #65199, #59555, #26441, #60666, #56128, #62143, #67025, #66311, #44105, #67403, #27164, #55383, #38837, #38092, #49367, #73403, #61776, #71921, #27547, #50482, #33181, #4644, #15530, #38469, #21529, #3538, #21158, #67781, #66668, #15154, #61405, #55757, #43390, #39214, #16268, #14787, #44490, #3902, #9888, #50094, #10627, #72300, #20798, #15903, #33553, #61022, #10257, #48992, #72651, #9522, #32444, #3173, #9147, #21913, #26803, #73022, #37735, #44859, #49727, #26065, #20437, #32070, #43752, #55007, #32805, #4270, #12752, #47348, #36060, #51222, #40978 ),
 ( #1530, #45609, #58620, #70253, #53352, #64278, #41337, #56880, #24410, #28282, #18037, #74150, #7126, #13499, #18760, #1892, #24779, #22662, #41698, #13122, #27920, #63914, #68536, #22287, #64638, #35678, #7497, #29660, #39584, #30042, #12383, #35329, #58258, #6754, #42084, #69895, #59004, #52991, #30407, #47708, #70624, #19138, #65021, #52610, #33934, #1162, #56513, #24059, #5016, #46983, #45229, #18390, #50849, #73775, #68150, #16642, #62531, #11007, #5388, #14977, #3725, #19502, #49556, #25886, #32256, #20623, #42449, #19869, #66495, #59740, #65386, #37919, #20985, #48816, #25160, #2993, #26250, #60489, #14230, #72114, #71363, #8224, #55204, #43577, #30773, #60850, #9330, #26623, #42818, #31521, #49189, #65747, #37185, #3357, #36422, #66130, #60126, #72481, #54832, #48449, #43207, #8970, #14605, #43937, #66854, #54459, #59369, #8608, #71734, #7858, #53719, #2262, #20237, #31893, #2637, #48086, #31153, #70998, #13853, #54106, #36794, #25517, #37557, #27745, #44299, #22864, #39030, #11198, #45802, #15726, #10077, #56707, #28473, #27358, #5209, #61229, #10448, #50294, #73227, #15340, #21340, #22484, #67600, #39403, #26988, #62350, #4464, #34124, #38284, #51409, #33000, #45426, #21727, #72840, #45047, #28109, #68353, #55944, #44683, #16093, #56327, #61968, #50668, #33366, #16849, #4844, #73596, #22107, #67973, #16467, #9712, #39780, #10833, #5578, #51046, #33754, #62729, #73969, #57071, #67228, #54470, #32630, #55575, #4094, #49923, #38661, #61593, #51788, #58921, #24693, #6311, #57433, #337, #23230, #58532, #63825, #64192, #23965, #13031, #1445, #68725, #40143, #1807, #17210, #29214, #11554, #63097, #41614, #41253, #12666, #40889, #34490, #47266, #52152, #52516, #5950, #46901, #18671, #24330, #12298, #52904, #697, #69444, #70169, #7029, #28859, #23588, #18310, #34873, #35598, #40506, #29954, #64553, #63453, #35970, #46156, #1070, #6667, #69089, #17574, #17947, #7411, #11927, #57808, #46518, #30326, #53270, #35236, #58169, #29573, #69809, #59654, #31061, #3639, #53637, #54745, #25437, #71654, #59283, #20150, #36708, #43491, #55111, #60767, #42364, #3273, #54019, #30690, #2910, #37472, #26162, #65302, #2557, #13773, #14138, #8137, #60040, #48365, #49099, #71277, #31437, #19781, #37089, #42729, #41998, #72025, #65663 ) ),
 .UNSPECIFIED., .F., .F., .F. ) 
 B_SPLINE_SURFACE_WITH_KNOTS ( ( 2, 2 ),
 ( 3, 2, 2, 2, 2, 2, 2, 2, 2, 2, 2, 2, 2, 2, 2, 2, 2, 2, 2, 2, 2, 2, 2, 2, 2, 2, 2, 2, 2, 2, 2, 2, 2, 2, 2, 2, 2, 2, 2, 2, 2, 2, 2, 2, 2, 2, 2, 2, 2, 2, 2, 2, 2, 2, 2, 2, 2, 2, 2, 2, 2, 2, 2, 2, 2, 2, 2, 2, 2, 2, 2, 2, 2, 2, 2, 2, 2, 2, 2, 2, 2, 2, 2, 2, 2, 2, 2, 2, 2, 2, 2, 2, 2, 2, 2, 2, 2, 2, 2, 2, 2, 2, 2, 2, 2, 2, 2, 2, 2, 2, 2, 2, 2, 2, 2, 2, 2, 2, 2, 2, 2, 2, 2, 2, 2, 2, 2, 2, 2, 2, 2, 2, 2, 2, 2, 2, 2, 2, 2, 2, 2, 2, 2, 3 ),
 ( 0.000000000000000000, 1.000000000000000000 ),
 ( 0.000000000000000000, 0.006944444444444444059, 0.01388888888888888812, 0.02083333333333333218, 0.02777777777777777624, 0.03472222222222222376, 0.04166666666666666435, 0.04861111111111111188, 0.05555555555555555247, 0.06250000000000000000, 0.06944444444444444753, 0.07638888888888889506, 0.08333333333333332871, 0.09027777777777777624, 0.09722222222222222376, 0.1041666666666666713, 0.1111111111111111049, 0.1180555555555555525, 0.1250000000000000000, 0.1319444444444444475, 0.1388888888888888951, 0.1458333333333333426, 0.1527777777777777901, 0.1597222222222222099, 0.1666666666666666574, 0.1736111111111111049, 0.1805555555555555525, 0.1875000000000000000, 0.1944444444444444475, 0.2013888888888888951, 0.2083333333333333426, 0.2152777777777777901, 0.2222222222222222099, 0.2291666666666666574, 0.2361111111111111049, 0.2430555555555555525, 0.2500000000000000000, 0.2569444444444444198, 0.2638888888888888951, 0.2708333333333333148, 0.2777777777777777901, 0.2847222222222222099, 0.2916666666666666852, 0.2986111111111111049, 0.3055555555555555802, 0.3125000000000000000, 0.3194444444444444198, 0.3263888888888888951, 0.3333333333333333148, 0.3402777777777777901, 0.3472222222222222099, 0.3541666666666666852, 0.3611111111111111049, 0.3680555555555555802, 0.3750000000000000000, 0.3819444444444444198, 0.3888888888888888951, 0.3958333333333333148, 0.4027777777777777901, 0.4097222222222222099, 0.4166666666666666852, 0.4236111111111111049, 0.4305555555555555802, 0.4375000000000000000, 0.4444444444444444198, 0.4513888888888888951, 0.4583333333333333148, 0.4652777777777777901, 0.4722222222222222099, 0.4791666666666666852, 0.4861111111111111049, 0.4930555555555555802, 0.5000000000000000000, 0.5069444444444444198, 0.5138888888888888395, 0.5208333333333333703, 0.5277777777777777901, 0.5347222222222222099, 0.5416666666666666297, 0.5486111111111111605, 0.5555555555555555802, 0.5625000000000000000, 0.5694444444444444198, 0.5763888888888888395, 0.5833333333333333703, 0.5902777777777777901, 0.5972222222222222099, 0.6041666666666666297, 0.6111111111111111605, 0.6180555555555555802, 0.6250000000000000000, 0.6319444444444444198, 0.6388888888888888395, 0.6458333333333333703, 0.6527777777777777901, 0.6597222222222222099, 0.6666666666666666297, 0.6736111111111111605, 0.6805555555555555802, 0.6875000000000000000, 0.6944444444444444198, 0.7013888888888888395, 0.7083333333333333703, 0.7152777777777777901, 0.7222222222222222099, 0.7291666666666666297, 0.7361111111111111605, 0.7430555555555555802, 0.7500000000000000000, 0.7569444444444444198, 0.7638888888888888395, 0.7708333333333333703, 0.7777777777777777901, 0.7847222222222222099, 0.7916666666666666297, 0.7986111111111111605, 0.8055555555555555802, 0.8125000000000000000, 0.8194444444444444198, 0.8263888888888888395, 0.8333333333333333703, 0.8402777777777777901, 0.8472222222222222099, 0.8541666666666666297, 0.8611111111111111605, 0.8680555555555555802, 0.8750000000000000000, 0.8819444444444444198, 0.8888888888888888395, 0.8958333333333333703, 0.9027777777777777901, 0.9097222222222222099, 0.9166666666666666297, 0.9236111111111111605, 0.9305555555555555802, 0.9375000000000000000, 0.9444444444444444198, 0.9513888888888888395, 0.9583333333333333703, 0.9652777777777777901, 0.9722222222222222099, 0.9791666666666666297, 0.9842226772312639982, 0.9940649040035766104 ),
 .UNSPECIFIED. ) 
 GEOMETRIC_REPRESENTATION_ITEM ( )  RATIONAL_B_SPLINE_SURFACE ( (
 ( 1.000000000000000000, 0.8660254037844387076, 1.000000000000000000, 0.8660254037844387076, 1.000000000000000000, 0.8660254037844387076, 1.000000000000000000, 0.8660254037844387076, 1.000000000000000000, 0.8660254037844387076, 1.000000000000000000, 0.8660254037844387076, 1.000000000000000000, 0.8660254037844387076, 1.000000000000000000, 0.8660254037844387076, 1.000000000000000000, 0.8660254037844387076, 1.000000000000000000, 0.8660254037844387076, 1.000000000000000000, 0.8660254037844387076, 1.000000000000000000, 0.8660254037844387076, 1.000000000000000000, 0.8660254037844387076, 1.000000000000000000, 0.8660254037844387076, 1.000000000000000000, 0.8660254037844387076, 1.000000000000000000, 0.8660254037844387076, 1.000000000000000000, 0.8660254037844387076, 1.000000000000000000, 0.8660254037844387076, 1.000000000000000000, 0.8660254037844387076, 1.000000000000000000, 0.8660254037844387076, 1.000000000000000000, 0.8660254037844387076, 1.000000000000000000, 0.8660254037844387076, 1.000000000000000000, 0.8660254037844387076, 1.000000000000000000, 0.8660254037844387076, 1.000000000000000000, 0.8660254037844387076, 1.000000000000000000, 0.8660254037844387076, 1.000000000000000000, 0.8660254037844387076, 1.000000000000000000, 0.8660254037844387076, 1.000000000000000000, 0.8660254037844387076, 1.000000000000000000, 0.8660254037844387076, 1.000000000000000000, 0.8660254037844387076, 1.000000000000000000, 0.8660254037844387076, 1.000000000000000000, 0.8660254037844387076, 1.000000000000000000, 0.8660254037844387076, 1.000000000000000000, 0.8660254037844387076, 1.000000000000000000, 0.8660254037844387076, 1.000000000000000000, 0.8660254037844387076, 1.000000000000000000, 0.8660254037844387076, 1.000000000000000000, 0.8660254037844387076, 1.000000000000000000, 0.8660254037844387076, 1.000000000000000000, 0.8660254037844387076, 1.000000000000000000, 0.8660254037844387076, 1.000000000000000000, 0.8660254037844387076, 1.000000000000000000, 0.8660254037844387076, 1.000000000000000000, 0.8660254037844387076, 1.000000000000000000, 0.8660254037844387076, 1.000000000000000000, 0.8660254037844387076, 1.000000000000000000, 0.8660254037844387076, 1.000000000000000000, 0.8660254037844387076, 1.000000000000000000, 0.8660254037844387076, 1.000000000000000000, 0.8660254037844387076, 1.000000000000000000, 0.8660254037844387076, 1.000000000000000000, 0.8660254037844387076, 1.000000000000000000, 0.8660254037844387076, 1.000000000000000000, 0.8660254037844387076, 1.000000000000000000, 0.8660254037844387076, 1.000000000000000000, 0.8660254037844387076, 1.000000000000000000, 0.8660254037844387076, 1.000000000000000000, 0.8660254037844387076, 1.000000000000000000, 0.8660254037844387076, 1.000000000000000000, 0.8660254037844387076, 1.000000000000000000, 0.8660254037844387076, 1.000000000000000000, 0.8660254037844387076, 1.000000000000000000, 0.8660254037844387076, 1.000000000000000000, 0.8660254037844387076, 1.000000000000000000, 0.8660254037844387076, 1.000000000000000000, 0.8660254037844387076, 1.000000000000000000, 0.8660254037844387076, 1.000000000000000000, 0.8660254037844387076, 1.000000000000000000, 0.8660254037844387076, 1.000000000000000000, 0.8660254037844387076, 1.000000000000000000, 0.8660254037844387076, 1.000000000000000000, 0.8660254037844387076, 1.000000000000000000, 0.8660254037844387076, 1.000000000000000000, 0.8660254037844387076, 1.000000000000000000, 0.8660254037844387076, 1.000000000000000000, 0.8660254037844387076, 1.000000000000000000, 0.8660254037844387076, 1.000000000000000000, 0.8660254037844387076, 1.000000000000000000, 0.8660254037844387076, 1.000000000000000000, 0.8660254037844387076, 1.000000000000000000, 0.8660254037844387076, 1.000000000000000000, 0.8660254037844387076, 1.000000000000000000, 0.8660254037844387076, 1.000000000000000000, 0.8660254037844387076, 1.000000000000000000, 0.8660254037844387076, 1.000000000000000000, 0.8660254037844387076, 1.000000000000000000, 0.8660254037844387076, 1.000000000000000000, 0.8660254037844387076, 1.000000000000000000, 0.8660254037844387076, 1.000000000000000000, 0.8660254037844387076, 1.000000000000000000, 0.8660254037844387076, 1.000000000000000000, 0.8660254037844387076, 1.000000000000000000, 0.8660254037844387076, 1.000000000000000000, 0.8660254037844387076, 1.000000000000000000, 0.8660254037844387076, 1.000000000000000000, 0.8660254037844387076, 1.000000000000000000, 0.8660254037844387076, 1.000000000000000000, 0.8660254037844387076, 1.000000000000000000, 0.8660254037844387076, 1.000000000000000000, 0.8660254037844387076, 1.000000000000000000, 0.8660254037844387076, 1.000000000000000000, 0.8660254037844387076, 1.000000000000000000, 0.8660254037844387076, 1.000000000000000000, 0.8660254037844387076, 1.000000000000000000, 0.8660254037844387076, 1.000000000000000000, 0.8660254037844387076, 1.000000000000000000, 0.8660254037844387076, 1.000000000000000000, 0.8660254037844387076, 1.000000000000000000, 0.8660254037844387076, 1.000000000000000000, 0.8660254037844387076, 1.000000000000000000, 0.8660254037844387076, 1.000000000000000000, 0.8660254037844387076, 1.000000000000000000, 0.8660254037844387076, 1.000000000000000000, 0.8660254037844387076, 1.000000000000000000, 0.8660254037844387076, 1.000000000000000000, 0.8660254037844387076, 1.000000000000000000, 0.8660254037844387076, 1.000000000000000000, 0.8660254037844387076, 1.000000000000000000, 0.8660254037844387076, 1.000000000000000000, 0.8660254037844387076, 1.000000000000000000, 0.8660254037844387076, 1.000000000000000000, 0.8660254037844387076, 1.000000000000000000, 0.8660254037844387076, 1.000000000000000000, 0.8660254037844387076, 1.000000000000000000, 0.8660254037844387076, 1.000000000000000000, 0.8660254037844387076, 1.000000000000000000, 0.8660254037844387076, 1.000000000000000000, 0.8660254037844387076, 1.000000000000000000, 0.8660254037844387076, 1.000000000000000000, 0.8660254037844387076, 1.000000000000000000, 0.8660254037844387076, 1.000000000000000000, 0.8660254037844387076, 1.000000000000000000, 0.8660254037844387076, 1.000000000000000000, 0.8660254037844387076, 1.000000000000000000, 0.8660254037844387076, 1.000000000000000000, 0.8660254037844387076, 1.000000000000000000, 0.8660254037844387076, 1.000000000000000000, 0.8660254037844387076, 1.000000000000000000, 0.8660254037844387076, 1.000000000000000000, 0.8660254037844387076, 1.000000000000000000, 0.9024577157650908177, 0.9469497795711379062, 0.9469497795711379062, 0.9469497795711379062),
 ( 1.000000000000000000, 0.8660254037844387076, 1.000000000000000000, 0.8660254037844387076, 1.000000000000000000, 0.8660254037844387076, 1.000000000000000000, 0.8660254037844387076, 1.000000000000000000, 0.8660254037844387076, 1.000000000000000000, 0.8660254037844387076, 1.000000000000000000, 0.8660254037844387076, 1.000000000000000000, 0.8660254037844387076, 1.000000000000000000, 0.8660254037844387076, 1.000000000000000000, 0.8660254037844387076, 1.000000000000000000, 0.8660254037844387076, 1.000000000000000000, 0.8660254037844387076, 1.000000000000000000, 0.8660254037844387076, 1.000000000000000000, 0.8660254037844387076, 1.000000000000000000, 0.8660254037844387076, 1.000000000000000000, 0.8660254037844387076, 1.000000000000000000, 0.8660254037844387076, 1.000000000000000000, 0.8660254037844387076, 1.000000000000000000, 0.8660254037844387076, 1.000000000000000000, 0.8660254037844387076, 1.000000000000000000, 0.8660254037844387076, 1.000000000000000000, 0.8660254037844387076, 1.000000000000000000, 0.8660254037844387076, 1.000000000000000000, 0.8660254037844387076, 1.000000000000000000, 0.8660254037844387076, 1.000000000000000000, 0.8660254037844387076, 1.000000000000000000, 0.8660254037844387076, 1.000000000000000000, 0.8660254037844387076, 1.000000000000000000, 0.8660254037844387076, 1.000000000000000000, 0.8660254037844387076, 1.000000000000000000, 0.8660254037844387076, 1.000000000000000000, 0.8660254037844387076, 1.000000000000000000, 0.8660254037844387076, 1.000000000000000000, 0.8660254037844387076, 1.000000000000000000, 0.8660254037844387076, 1.000000000000000000, 0.8660254037844387076, 1.000000000000000000, 0.8660254037844387076, 1.000000000000000000, 0.8660254037844387076, 1.000000000000000000, 0.8660254037844387076, 1.000000000000000000, 0.8660254037844387076, 1.000000000000000000, 0.8660254037844387076, 1.000000000000000000, 0.8660254037844387076, 1.000000000000000000, 0.8660254037844387076, 1.000000000000000000, 0.8660254037844387076, 1.000000000000000000, 0.8660254037844387076, 1.000000000000000000, 0.8660254037844387076, 1.000000000000000000, 0.8660254037844387076, 1.000000000000000000, 0.8660254037844387076, 1.000000000000000000, 0.8660254037844387076, 1.000000000000000000, 0.8660254037844387076, 1.000000000000000000, 0.8660254037844387076, 1.000000000000000000, 0.8660254037844387076, 1.000000000000000000, 0.8660254037844387076, 1.000000000000000000, 0.8660254037844387076, 1.000000000000000000, 0.8660254037844387076, 1.000000000000000000, 0.8660254037844387076, 1.000000000000000000, 0.8660254037844387076, 1.000000000000000000, 0.8660254037844387076, 1.000000000000000000, 0.8660254037844387076, 1.000000000000000000, 0.8660254037844387076, 1.000000000000000000, 0.8660254037844387076, 1.000000000000000000, 0.8660254037844387076, 1.000000000000000000, 0.8660254037844387076, 1.000000000000000000, 0.8660254037844387076, 1.000000000000000000, 0.8660254037844387076, 1.000000000000000000, 0.8660254037844387076, 1.000000000000000000, 0.8660254037844387076, 1.000000000000000000, 0.8660254037844387076, 1.000000000000000000, 0.8660254037844387076, 1.000000000000000000, 0.8660254037844387076, 1.000000000000000000, 0.8660254037844387076, 1.000000000000000000, 0.8660254037844387076, 1.000000000000000000, 0.8660254037844387076, 1.000000000000000000, 0.8660254037844387076, 1.000000000000000000, 0.8660254037844387076, 1.000000000000000000, 0.8660254037844387076, 1.000000000000000000, 0.8660254037844387076, 1.000000000000000000, 0.8660254037844387076, 1.000000000000000000, 0.8660254037844387076, 1.000000000000000000, 0.8660254037844387076, 1.000000000000000000, 0.8660254037844387076, 1.000000000000000000, 0.8660254037844387076, 1.000000000000000000, 0.8660254037844387076, 1.000000000000000000, 0.8660254037844387076, 1.000000000000000000, 0.8660254037844387076, 1.000000000000000000, 0.8660254037844387076, 1.000000000000000000, 0.8660254037844387076, 1.000000000000000000, 0.8660254037844387076, 1.000000000000000000, 0.8660254037844387076, 1.000000000000000000, 0.8660254037844387076, 1.000000000000000000, 0.8660254037844387076, 1.000000000000000000, 0.8660254037844387076, 1.000000000000000000, 0.8660254037844387076, 1.000000000000000000, 0.8660254037844387076, 1.000000000000000000, 0.8660254037844387076, 1.000000000000000000, 0.8660254037844387076, 1.000000000000000000, 0.8660254037844387076, 1.000000000000000000, 0.8660254037844387076, 1.000000000000000000, 0.8660254037844387076, 1.000000000000000000, 0.8660254037844387076, 1.000000000000000000, 0.8660254037844387076, 1.000000000000000000, 0.8660254037844387076, 1.000000000000000000, 0.8660254037844387076, 1.000000000000000000, 0.8660254037844387076, 1.000000000000000000, 0.8660254037844387076, 1.000000000000000000, 0.8660254037844387076, 1.000000000000000000, 0.8660254037844387076, 1.000000000000000000, 0.8660254037844387076, 1.000000000000000000, 0.8660254037844387076, 1.000000000000000000, 0.8660254037844387076, 1.000000000000000000, 0.8660254037844387076, 1.000000000000000000, 0.8660254037844387076, 1.000000000000000000, 0.8660254037844387076, 1.000000000000000000, 0.8660254037844387076, 1.000000000000000000, 0.8660254037844387076, 1.000000000000000000, 0.8660254037844387076, 1.000000000000000000, 0.8660254037844387076, 1.000000000000000000, 0.8660254037844387076, 1.000000000000000000, 0.8660254037844387076, 1.000000000000000000, 0.8660254037844387076, 1.000000000000000000, 0.8660254037844387076, 1.000000000000000000, 0.8660254037844387076, 1.000000000000000000, 0.8660254037844387076, 1.000000000000000000, 0.8660254037844387076, 1.000000000000000000, 0.8660254037844387076, 1.000000000000000000, 0.8660254037844387076, 1.000000000000000000, 0.8660254037844387076, 1.000000000000000000, 0.8660254037844387076, 1.000000000000000000, 0.8660254037844387076, 1.000000000000000000, 0.8660254037844387076, 1.000000000000000000, 0.8660254037844387076, 1.000000000000000000, 0.8660254037844387076, 1.000000000000000000, 0.8660254037844387076, 1.000000000000000000, 0.8660254037844387076, 1.000000000000000000, 0.8660254037844387076, 1.000000000000000000, 0.8660254037844387076, 1.000000000000000000, 0.8660254037844387076, 1.000000000000000000, 0.8660254037844387076, 1.000000000000000000, 0.8660254037844387076, 1.000000000000000000, 0.8660254037844387076, 1.000000000000000000, 0.8660254037844387076, 1.000000000000000000, 0.9024577157650908177, 0.9469497795711379062, 0.9469497795711379062, 0.9469497795711379062) ) ) 
 REPRESENTATION_ITEM ( '' )  SURFACE ( )  );
#68334 = PLANE ( 'NONE',  #29248 ) ;
#68335 = CARTESIAN_POINT ( 'NONE',  ( 0.000000000000000000, -17.80606268964563554, 33.00180498840040855 ) ) ;
#68336 = ADVANCED_FACE ( 'NONE', ( #73640 ), #39082, .T. ) ;
#68337 = FACE_OUTER_BOUND ( 'NONE', #18220, .T. ) ;
#68338 = CARTESIAN_POINT ( 'NONE',  ( 93.67500000000001137, -212.2949673200287179, 89.47083333333333144 ) ) ;
#68339 = VECTOR ( 'NONE', #10722, 1000.000000000000114 ) ;
#68340 = VECTOR ( 'NONE', #17629, 1000.000000000000000 ) ;
#68341 = VERTEX_POINT ( 'NONE', #10494 ) ;
#68342 = ORIENTED_EDGE ( 'NONE', *, *, #57711, .F. ) ;
#68343 = CARTESIAN_POINT ( 'NONE',  ( 15.00000000000000000, 0.000000000000000000, 0.000000000000000000 ) ) ;
#68344 = VERTEX_POINT ( 'NONE', #62779 ) ;
#68345 = VERTEX_POINT ( 'NONE', #34177 ) ;
#68346 = CARTESIAN_POINT ( 'NONE',  ( 6.000000000000000000, -22.90783923731575200, -78.73519480814978522 ) ) ;
#68347 = CIRCLE ( 'NONE', #41941, 12.49999999999999645 ) ;
#68348 = CARTESIAN_POINT ( 'NONE',  ( 10.00000000000000000, 0.000000000000000000, 0.000000000000000000 ) ) ;
#68349 = VECTOR ( 'NONE', #44742, 1000.000000000000000 ) ;
#68350 = ORIENTED_EDGE ( 'NONE', *, *, #44973, .F. ) ;
#68351 = FACE_OUTER_BOUND ( 'NONE', #1639, .T. ) ;
#68352 = CARTESIAN_POINT ( 'NONE',  ( 97.64999999999997726, -211.5299782133524502, 78.27895833506762813 ) ) ;
#68353 = CARTESIAN_POINT ( 'NONE',  ( 92.34999999999999432, 90.00000000000002842, 81.74500000000000455 ) ) ;
#68354 = EDGE_CURVE ( 'NONE', #22408, #39802, #54623, .T. ) ;
#68355 = ORIENTED_EDGE ( 'NONE', *, *, #66041, .T. ) ;
#68356 = DIRECTION ( 'NONE',  ( -0.000000000000000000, -0.000000000000000000, 1.000000000000000000 ) ) ;
#68357 = VERTEX_POINT ( 'NONE', #56376 ) ;
#68358 = EDGE_CURVE ( 'NONE', #36787, #28860, #45222, .T. ) ;
#68359 = DIRECTION ( 'NONE',  ( -0.000000000000000000, -0.000000000000000000, -1.000000000000000000 ) ) ;
#68360 = ORIENTED_EDGE ( 'NONE', *, *, #40158, .T. ) ;
#68361 = CARTESIAN_POINT ( 'NONE',  ( -97.65000000000001990, 88.47002178664754979, 88.22729166840096582 ) ) ;
#68362 = CARTESIAN_POINT ( 'NONE',  ( -97.30629616937501680, 91.33154071421968467, 82.12864583420048348 ) ) ;
#68363 = CARTESIAN_POINT ( 'NONE',  ( 96.15314808468748708, 88.00268892867053694, 77.15447916753380753 ) ) ;
#68364 = EDGE_LOOP ( 'NONE', ( #41687, #41284, #882, #19147 ) ) ;
#68365 = FACE_OUTER_BOUND ( 'NONE', #72210, .T. ) ;
#68366 = CIRCLE ( 'NONE', #46732, 31.99999999999999289 ) ;
#68367 = DIRECTION ( 'NONE',  ( -0.8571673007021122226, 1.049727191138618572E-16, 0.5150380749100542666 ) ) ;
#68368 = VECTOR ( 'NONE', #65414, 1000.000000000000000 ) ;
#68369 = CARTESIAN_POINT ( 'NONE',  ( -3.000000000000000000, 26.50000000000000000, -1.500000000000001332 ) ) ;
#68370 = DIRECTION ( 'NONE',  ( 0.000000000000000000, 0.000000000000000000, 1.000000000000000000 ) ) ;
#68371 = VERTEX_POINT ( 'NONE', #62398 ) ;
#68372 = FACE_OUTER_BOUND ( 'NONE', #39664, .T. ) ;
#68373 = CIRCLE ( 'NONE', #40728, 77.49899999999999523 ) ;
#68374 = EDGE_CURVE ( 'NONE', #6126, #21432, #5633, .T. ) ;
#68375 = EDGE_CURVE ( 'NONE', #62821, #18312, #27409, .T. ) ;
#68377 = CARTESIAN_POINT ( 'NONE',  ( -97.30629616937497417, -211.3315407142195852, 76.99572916753380980 ) ) ;
#68376 = AXIS2_PLACEMENT_3D ( 'NONE', #25819, #61159, #43514 ) ;
#68378 = VERTEX_POINT ( 'NONE', #27793 ) ;
#68379 = ORIENTED_EDGE ( 'NONE', *, *, #44659, .F. ) ;
#68380 = CARTESIAN_POINT ( 'NONE',  ( 11.99999999999999822, -22.90783923731575200, -78.73519480814978522 ) ) ;
#68381 = VECTOR ( 'NONE', #19490, 1000.000000000000000 ) ;
#68382 = AXIS2_PLACEMENT_3D ( 'NONE', #11256, #34186, #29273 ) ;
#68383 = ORIENTED_EDGE ( 'NONE', *, *, #55237, .F. ) ;
#68384 = CARTESIAN_POINT ( 'NONE',  ( 93.67499999999999716, 87.70503267997126784, 78.04083333333333883 ) ) ;
#68385 = CARTESIAN_POINT ( 'NONE',  ( 0.000000000000000000, 33.80338159004283938, 16.23288003029508886 ) ) ;
#68386 = VERTEX_POINT ( 'NONE', #15263 ) ;
#68387 = CARTESIAN_POINT ( 'NONE',  ( -92.69370383062498320, -211.3315407142195852, 77.20739583420046870 ) ) ;
#68388 = ORIENTED_EDGE ( 'NONE', *, *, #52349, .F. ) ;
#68389 = CARTESIAN_POINT ( 'NONE',  ( -97.65000000000001990, 90.00000000000004263, 76.66499999999999204 ) ) ;
#68390 = CARTESIAN_POINT ( 'NONE',  ( 0.000000000000000000, -66.50666863322028632, 39.78640506895582973 ) ) ;
#68391 = CYLINDRICAL_SURFACE ( 'NONE', #42967, 16.00000000000000000 ) ;
#68392 = CARTESIAN_POINT ( 'NONE',  ( 5.999999999999999112, 64.81221759200342092, 50.23322058963371006 ) ) ;
#68393 = DIRECTION ( 'NONE',  ( -1.000000000000000000, 0.000000000000000000, 0.000000000000000000 ) ) ;
#68394 = CARTESIAN_POINT ( 'NONE',  ( 93.84685191531248449, 91.99731107132950569, 85.09197916753380753 ) ) ;
#68395 = CARTESIAN_POINT ( 'NONE',  ( 10.00000000000000000, 37.22597642581150268, 5.202137450157037435 ) ) ;
#68396 = LINE ( 'NONE', #51452, #38607 ) ;
#68397 = DIRECTION ( 'NONE',  ( -1.000000000000000000, 0.000000000000000000, 0.000000000000000000 ) ) ;
#68398 = CARTESIAN_POINT ( 'NONE',  ( -4.999999999999999112, 0.2838785441256745923, -0.5080592402122393603 ) ) ;
#68399 = DIRECTION ( 'NONE',  ( -1.000000000000000000, 0.000000000000000000, -0.000000000000000000 ) ) ;
#68400 = CARTESIAN_POINT ( 'NONE',  ( 1.546821644788039851, 4.880444798889544522, -0.7375898304884582757 ) ) ;
#68401 = LINE ( 'NONE', #16891, #24282 ) ;
#68402 = DIRECTION ( 'NONE',  ( 0.000000000000000000, 0.8090169943749445647, 0.5877852522924770229 ) ) ;
#68403 = AXIS2_PLACEMENT_3D ( 'NONE', #33868, #6424, #56814 ) ;
#68404 = CARTESIAN_POINT ( 'NONE',  ( 10.00000000000000000, -16.45098606841149902, 33.79645857604508308 ) ) ;
#68405 = EDGE_CURVE ( 'NONE', #73333, #32813, #13961, .T. ) ;
#68406 = DIRECTION ( 'NONE',  ( 0.000000000000000000, -0.2334453638559126354, 0.9723699203976748917 ) ) ;
#68407 = AXIS2_PLACEMENT_3D ( 'NONE', #44230, #67156, #33295 ) ;
#68408 = CARTESIAN_POINT ( 'NONE',  ( -92.69370383062504004, 90.00000000000004263, 88.69031250086715090 ) ) ;
#68409 = DIRECTION ( 'NONE',  ( -1.000000000000000000, -0.000000000000000000, 0.000000000000000000 ) ) ;
#68410 = CARTESIAN_POINT ( 'NONE',  ( -92.34999999999999432, -208.4700217866474645, 83.38541666666667140 ) ) ;
#68411 = EDGE_CURVE ( 'NONE', #56682, #27079, #65664, .T. ) ;
#68412 = EDGE_CURVE ( 'NONE', #21499, #20440, #3227, .T. ) ;
#68413 = CARTESIAN_POINT ( 'NONE',  ( 2.874421927457452952, -143.3717286177755739, -5.500000000000000000 ) ) ;
#68414 = ORIENTED_EDGE ( 'NONE', *, *, #45524, .F. ) ;
#68415 = DIRECTION ( 'NONE',  ( 0.000000000000000000, 0.000000000000000000, 1.000000000000000000 ) ) ;
#68416 = CARTESIAN_POINT ( 'NONE',  ( 10.00000000000000000, -30.80686688397025108, 21.53537804866070715 ) ) ;
#68417 = FACE_OUTER_BOUND ( 'NONE', #9494, .T. ) ;
#68418 = EDGE_CURVE ( 'NONE', #65777, #17753, #4005, .T. ) ;
#68419 = DIRECTION ( 'NONE',  ( 1.000000000000000000, 0.000000000000000000, 0.000000000000000000 ) ) ;
#68420 = AXIS2_PLACEMENT_3D ( 'NONE', #41634, #40914, #70937 ) ;
#68421 = AXIS2_PLACEMENT_3D ( 'NONE', #5118, #61880, #56233 ) ;
#68422 = VECTOR ( 'NONE', #39339, 1000.000000000000000 ) ;
#68423 = CARTESIAN_POINT ( 'NONE',  ( 96.15314808468750130, -211.9973110713294489, 84.93322916753382401 ) ) ;
#68424 = VERTEX_POINT ( 'NONE', #14140 ) ;
#68425 = AXIS2_PLACEMENT_3D ( 'NONE', #9523, #14039, #59935 ) ;
#68426 = ORIENTED_EDGE ( 'NONE', *, *, #39248, .T. ) ;
#68427 = CIRCLE ( 'NONE', #17970, 37.49900000000000233 ) ;
#68428 = DIRECTION ( 'NONE',  ( -1.000000000000000000, -0.000000000000000000, 0.000000000000000000 ) ) ;
#68429 = ORIENTED_EDGE ( 'NONE', *, *, #60727, .F. ) ;
#68430 = DIRECTION ( 'NONE',  ( -1.000000000000000000, 0.000000000000000000, -0.000000000000000000 ) ) ;
#68431 = CARTESIAN_POINT ( 'NONE',  ( 93.84685191531249870, -208.0026889286704943, 79.37697916753380412 ) ) ;
#68432 = EDGE_CURVE ( 'NONE', #4640, #26852, #9988, .T. ) ;
#68433 = EDGE_LOOP ( 'NONE', ( #3088, #26396, #1103, #38376 ) ) ;
#68434 = CARTESIAN_POINT ( 'NONE',  ( 92.69370383062501162, -208.6684592857803011, 84.66864583420047552 ) ) ;
#68435 = VERTEX_POINT ( 'NONE', #32908 ) ;
#68436 = CARTESIAN_POINT ( 'NONE',  ( 93.67499999999998295, 92.29496732002878900, 80.44854166840097776 ) ) ;
#68437 = ORIENTED_EDGE ( 'NONE', *, *, #55233, .T. ) ;
#68438 = ORIENTED_EDGE ( 'NONE', *, *, #7901, .T. ) ;
#68439 = DIRECTION ( 'NONE',  ( 1.000000000000000000, 0.000000000000000000, 0.000000000000000000 ) ) ;
#68440 = VERTEX_POINT ( 'NONE', #37090 ) ;
#68441 = CARTESIAN_POINT ( 'NONE',  ( 92.35000000000002274, -208.4700217866474645, 86.21645833506764234 ) ) ;
#68442 = EDGE_CURVE ( 'NONE', #31431, #54454, #15212, .T. ) ;
#68443 = ORIENTED_EDGE ( 'NONE', *, *, #33243, .F. ) ;
#68444 = LINE ( 'NONE', #57163, #4679 ) ;
#68445 = EDGE_CURVE ( 'NONE', #42999, #34136, #31996, .T. ) ;
#68446 = ORIENTED_EDGE ( 'NONE', *, *, #28844, .F. ) ;
#68447 = CYLINDRICAL_SURFACE ( 'NONE', #66071, 31.99999999999998579 ) ;
#68448 = CIRCLE ( 'NONE', #21451, 82.00000000000000000 ) ;
#68449 = EDGE_CURVE ( 'NONE', #852, #40220, #49100, .T. ) ;
#68450 = VERTEX_POINT ( 'NONE', #66768 ) ;
#68451 = CIRCLE ( 'NONE', #2429, 31.99999999999999645 ) ;
#68452 = ORIENTED_EDGE ( 'NONE', *, *, #74059, .F. ) ;
#68453 = ORIENTED_EDGE ( 'NONE', *, *, #16810, .T. ) ;
#68454 = DIRECTION ( 'NONE',  ( -1.000000000000000000, 0.000000000000000000, 0.000000000000000000 ) ) ;
#68455 = CYLINDRICAL_SURFACE ( 'NONE', #41453, 82.00000000000000000 ) ;
#68456 = ORIENTED_EDGE ( 'NONE', *, *, #40080, .T. ) ;
#68457 = ORIENTED_EDGE ( 'NONE', *, *, #21301, .T. ) ;
#68458 = VECTOR ( 'NONE', #54503, 1000.000000000000114 ) ;
#68459 = ORIENTED_EDGE ( 'NONE', *, *, #23834, .F. ) ;
#68460 = CARTESIAN_POINT ( 'NONE',  ( 0.000000000000000000, -59.46389618801999433, 49.70050353004867816 ) ) ;
#68461 = LINE ( 'NONE', #72945, #23898 ) ;
#68462 = CARTESIAN_POINT ( 'NONE',  ( -93.84685191531254134, 91.99731107132950569, 75.61989583420049144 ) ) ;
#68463 = ORIENTED_EDGE ( 'NONE', *, *, #65275, .T. ) ;
#68464 = CARTESIAN_POINT ( 'NONE',  ( 0.000000000000000000, -64.81221759200379040, 50.23322058963324110 ) ) ;
#68465 = ORIENTED_EDGE ( 'NONE', *, *, #24514, .T. ) ;
#68466 = CARTESIAN_POINT ( 'NONE',  ( 0.000000000000000000, -24.73286445877757345, 73.44644590900053061 ) ) ;
#68467 = CARTESIAN_POINT ( 'NONE',  ( -94.99999999999997158, -212.6630814284392557, 85.99156250086714692 ) ) ;
#68468 = VERTEX_POINT ( 'NONE', #72026 ) ;
#68469 = FACE_OUTER_BOUND ( 'NONE', #19803, .T. ) ;
#68470 = CARTESIAN_POINT ( 'NONE',  ( 0.000000000000000000, 14.67089635893713684, 73.72996012237443608 ) ) ;
#68471 = CARTESIAN_POINT ( 'NONE',  ( 0.000000000000000000, 75.11764819372149304, -2.946379043146603482 ) ) ;
#68472 = CARTESIAN_POINT ( 'NONE',  ( -92.69370383062498320, -209.9999999999999716, 75.99031250086714806 ) ) ;
#68473 = CIRCLE ( 'NONE', #42059, 37.49900000000001654 ) ;
#68474 = DIRECTION ( 'NONE',  ( -1.000000000000000000, 0.000000000000000000, 0.000000000000000000 ) ) ;
#68475 = DIRECTION ( 'NONE',  ( 0.000000000000000000, 0.1564344650402243742, 0.9876883405951387696 ) ) ;
#68476 = CONICAL_SURFACE ( 'NONE', #37235, 2.649999999999999467, 1.029744258676654312 ) ;
#68477 = VECTOR ( 'NONE', #57996, 1000.000000000000000 ) ;
#68478 = CIRCLE ( 'NONE', #60063, 37.49900000000000233 ) ;
#68479 = DIRECTION ( 'NONE',  ( -1.000000000000000000, 0.000000000000000000, 0.000000000000000000 ) ) ;
#68480 = CIRCLE ( 'NONE', #24036, 31.99999999999999289 ) ;
#68481 = AXIS2_PLACEMENT_3D ( 'NONE', #32421, #61755, #55364 ) ;
#68482 = LINE ( 'NONE', #16969, #41145 ) ;
#68483 = LINE ( 'NONE', #27869, #46402 ) ;
#68484 = CARTESIAN_POINT ( 'NONE',  ( -92.69370383062502583, 91.33154071421968467, 81.12322916753382174 ) ) ;
#68485 = CARTESIAN_POINT ( 'NONE',  ( 0.000000000000000000, 81.96053171279902472, -2.543863470248670211 ) ) ;
#68486 = FACE_OUTER_BOUND ( 'NONE', #63470, .T. ) ;
#68487 = ORIENTED_EDGE ( 'NONE', *, *, #7586, .F. ) ;
#68488 = CARTESIAN_POINT ( 'NONE',  ( 10.00000000000000000, 0.000000000000000000, 0.000000000000000000 ) ) ;
#68489 = CARTESIAN_POINT ( 'NONE',  ( -10.00000000000000000, 0.000000000000000000, 0.000000000000000000 ) ) ;
#68490 = CARTESIAN_POINT ( 'NONE',  ( 93.67500000000001137, -212.2949673200287179, 86.37520833506764006 ) ) ;
#68491 = CARTESIAN_POINT ( 'NONE',  ( 95.04693102382874770, -212.6495843973424940, 75.00000002508419072 ) ) ;
#68492 = CARTESIAN_POINT ( 'NONE',  ( -20.63750000000000284, -2.946905753441389499E-14, -1.643265707204933640E-14 ) ) ;
#68493 = FACE_OUTER_BOUND ( 'NONE', #47724, .T. ) ;
#68494 = CARTESIAN_POINT ( 'NONE',  ( -94.99999999999997158, -207.3369185715606307, 79.48281250086715488 ) ) ;
#68495 = EDGE_CURVE ( 'NONE', #27109, #39671, #20539, .T. ) ;
#68496 = EDGE_CURVE ( 'NONE', #31992, #40854, #67137, .T. ) ;
#68497 = CARTESIAN_POINT ( 'NONE',  ( 11.99999999999999822, 62.20884554314020676, 46.21855187248652896 ) ) ;
#68498 = ORIENTED_EDGE ( 'NONE', *, *, #62211, .T. ) ;
#68499 = CYLINDRICAL_SURFACE ( 'NONE', #22708, 37.49900000000000233 ) ;
#68500 = LINE ( 'NONE', #39931, #50242 ) ;
#68501 = DIRECTION ( 'NONE',  ( -1.000000000000000000, -0.000000000000000000, -0.000000000000000000 ) ) ;
#68502 = EDGE_CURVE ( 'NONE', #54619, #32157, #55861, .T. ) ;
#68503 = CARTESIAN_POINT ( 'NONE',  ( 10.00000000000000000, 31.47745569255237896, -68.26794271651228030 ) ) ;
#68504 = EDGE_CURVE ( 'NONE', #29668, #60926, #74026, .T. ) ;
#68505 = CARTESIAN_POINT ( 'NONE',  ( 0.000000000000000000, -24.73286445877653961, -73.44644590900085745 ) ) ;
#68506 = AXIS2_PLACEMENT_3D ( 'NONE', #56277, #73921, #40095 ) ;
#68507 = AXIS2_PLACEMENT_3D ( 'NONE', #70928, #19430, #25451 ) ;
#68508 = CARTESIAN_POINT ( 'NONE',  ( 0.000000000000000000, -68.26794271651286294, 31.47745569255117104 ) ) ;
#68509 = ORIENTED_EDGE ( 'NONE', *, *, #25806, .T. ) ;
#68510 = CARTESIAN_POINT ( 'NONE',  ( 10.00000000000000000, 16.23288003029497162, 33.80338159004289622 ) ) ;
#68511 = DIRECTION ( 'NONE',  ( 0.000000000000000000, 0.000000000000000000, 1.000000000000000000 ) ) ;
#68512 = EDGE_LOOP ( 'NONE', ( #41716, #28132, #27898, #34765 ) ) ;
#68513 = CARTESIAN_POINT ( 'NONE',  ( 97.30629616937498838, -209.9999999999999716, 87.42031250086714067 ) ) ;
#68514 = CARTESIAN_POINT ( 'NONE',  ( 10.00000000000000000, 0.000000000000000000, 0.000000000000000000 ) ) ;
#68515 = ADVANCED_FACE ( 'NONE', ( #50200 ), #9248, .F. ) ;
#68516 = ORIENTED_EDGE ( 'NONE', *, *, #55662, .T. ) ;
#68517 = CARTESIAN_POINT ( 'NONE',  ( 0.000000000000000000, 0.000000000000000000, 0.000000000000000000 ) ) ;
#68518 = CIRCLE ( 'NONE', #16940, 82.00000000000000000 ) ;
#68519 = ORIENTED_EDGE ( 'NONE', *, *, #64451, .T. ) ;
#68520 = CARTESIAN_POINT ( 'NONE',  ( 97.65000000000000568, -211.5299782133524218, 85.26395833506762756 ) ) ;
#68521 = VERTEX_POINT ( 'NONE', #31438 ) ;
#68522 = VECTOR ( 'NONE', #24887, 1000.000000000000000 ) ;
#68523 = CARTESIAN_POINT ( 'NONE',  ( 97.65000000000000568, -211.5299782133524502, 82.00958333333333883 ) ) ;
#68524 = AXIS2_PLACEMENT_3D ( 'NONE', #65410, #43594, #59389 ) ;
#68525 = ORIENTED_EDGE ( 'NONE', *, *, #7793, .T. ) ;
#68526 = DIRECTION ( 'NONE',  ( -1.000000000000000000, 0.000000000000000000, 0.000000000000000000 ) ) ;
#68527 = ORIENTED_EDGE ( 'NONE', *, *, #42626, .T. ) ;
#68528 = CIRCLE ( 'NONE', #2510, 31.99999999999998934 ) ;
#68529 = ORIENTED_EDGE ( 'NONE', *, *, #4790, .T. ) ;
#68530 = LINE ( 'NONE', #29024, #72813 ) ;
#68531 = EDGE_CURVE ( 'NONE', #19857, #47239, #4396, .T. ) ;
#68532 = EDGE_CURVE ( 'NONE', #57658, #12172, #69211, .T. ) ;
#68533 = ORIENTED_EDGE ( 'NONE', *, *, #12632, .T. ) ;
#68534 = EDGE_CURVE ( 'NONE', #55684, #31218, #25801, .T. ) ;
#68535 = ORIENTED_EDGE ( 'NONE', *, *, #65038, .F. ) ;
#68536 = CARTESIAN_POINT ( 'NONE',  ( 93.67499999999999716, 87.70503267997126784, 88.83583333333334053 ) ) ;
#68537 = CARTESIAN_POINT ( 'NONE',  ( 0.000000000000000000, -22.64427369931191336, 30.00120703465197280 ) ) ;
#68538 = CYLINDRICAL_SURFACE ( 'NONE', #12911, 2.649999999999985700 ) ;
#68539 = ORIENTED_EDGE ( 'NONE', *, *, #51365, .F. ) ;
#68540 = ORIENTED_EDGE ( 'NONE', *, *, #68693, .F. ) ;
#68541 = ORIENTED_EDGE ( 'NONE', *, *, #37163, .F. ) ;
#68542 = CARTESIAN_POINT ( 'NONE',  ( 97.30629616937498838, 90.00000000000002842, 83.61031250086713840 ) ) ;
#68543 = VERTEX_POINT ( 'NONE', #71655 ) ;
#68544 = CARTESIAN_POINT ( 'NONE',  ( 97.30629616937498838, -208.6684592857803011, 83.66322916753379957 ) ) ;
#68545 = APPLICATION_PROTOCOL_DEFINITION ( 'draft international standard', 'automotive_design', 1998, #5718 ) ;
#68546 = FACE_OUTER_BOUND ( 'NONE', #59496, .T. ) ;
#68547 = FACE_OUTER_BOUND ( 'NONE', #9976, .T. ) ;
#68548 = DIRECTION ( 'NONE',  ( -1.000000000000000000, 0.000000000000000000, 0.000000000000000000 ) ) ;
#68549 = DIRECTION ( 'NONE',  ( 1.000000000000000000, 0.000000000000000000, 0.000000000000000000 ) ) ;
#68550 = FACE_OUTER_BOUND ( 'NONE', #5215, .T. ) ;
#68551 = CARTESIAN_POINT ( 'NONE',  ( -93.84685191531247028, -211.9973110713294489, 89.21947916753380525 ) ) ;
#68552 = CARTESIAN_POINT ( 'NONE',  ( -92.69370383062504004, 90.00000000000004263, 85.03906250086714635 ) ) ;
#68553 = EDGE_LOOP ( 'NONE', ( #54398, #15075, #66303, #31868 ) ) ;
#68555 = CARTESIAN_POINT ( 'NONE',  ( -93.84685191531252713, 88.00268892867056536, 84.13947916753380696 ) ) ;
#68554 = CARTESIAN_POINT ( 'NONE',  ( 92.69370383062498320, 88.66845928578037217, 83.98072916753380923 ) ) ;
#68556 = VERTEX_POINT ( 'NONE', #20152 ) ;
#68557 = CARTESIAN_POINT ( 'NONE',  ( -97.65000000000001990, 90.00000000000004263, 88.09499999999999886 ) ) ;
#68558 = DIRECTION ( 'NONE',  ( -1.000000000000000000, 0.000000000000000000, -0.000000000000000000 ) ) ;
#68559 = DIRECTION ( 'NONE',  ( 0.000000000000000000, -0.8526401643540859610, -0.5224985647159591240 ) ) ;
#68560 = CARTESIAN_POINT ( 'NONE',  ( -18.24502636017238899, -100.7225776329765665, 5.500000000000000000 ) ) ;
#68561 = CARTESIAN_POINT ( 'NONE',  ( -93.84685191531247028, -211.9973110713294489, 84.77447916753381207 ) ) ;
#68562 = DIRECTION ( 'NONE',  ( -1.000000000000000000, 0.000000000000000000, 0.000000000000000000 ) ) ;
#68563 = AXIS2_PLACEMENT_3D ( 'NONE', #46472, #1020, #1395 ) ;
#68564 = CIRCLE ( 'NONE', #2583, 42.00000000000000000 ) ;
#68565 = CARTESIAN_POINT ( 'NONE',  ( -97.64996030324549281, 88.46999886771563126, 88.86229325377451005 ) ) ;
#68566 = FACE_OUTER_BOUND ( 'NONE', #51681, .T. ) ;
#68567 = CIRCLE ( 'NONE', #12086, 16.00000000000000000 ) ;
#68568 = DIRECTION ( 'NONE',  ( -1.000000000000000000, 0.000000000000000000, -0.000000000000000000 ) ) ;
#68569 = ORIENTED_EDGE ( 'NONE', *, *, #40392, .F. ) ;
#68570 = ORIENTED_EDGE ( 'NONE', *, *, #5902, .F. ) ;
#68571 = CARTESIAN_POINT ( 'NONE',  ( -93.67500000000003979, 87.70503267997129626, 77.51166666666665606 ) ) ;
#68572 = CARTESIAN_POINT ( 'NONE',  ( 1.243286885786405054E-17, -120.0000000000000000, -85.60000000000000853 ) ) ;
#68573 = FACE_OUTER_BOUND ( 'NONE', #22325, .T. ) ;
#68574 = CARTESIAN_POINT ( 'NONE',  ( 0.000000000000000000, 0.000000000000000000, 125.0000000000000000 ) ) ;
#68575 = CARTESIAN_POINT ( 'NONE',  ( 97.08316478178002740, -211.0005890871205736, 74.79348190356850523 ) ) ;
#68576 = EDGE_CURVE ( 'NONE', #27263, #21733, #46949, .T. ) ;
#68577 = CARTESIAN_POINT ( 'NONE',  ( -95.00000000000002842, 86.94004357329504273, 86.42812500173430124 ) ) ;
#68578 = DIRECTION ( 'NONE',  ( 0.000000000000000000, -0.8526401643540970632, 0.5224985647159410274 ) ) ;
#68579 =( BOUNDED_CURVE ( )  B_SPLINE_CURVE ( 2, ( #19091, #2218, #60445, #60084, #8180, #8562, #31481, #2595, #13079 ),
 .UNSPECIFIED., .F., .F. ) 
 B_SPLINE_CURVE_WITH_KNOTS ( ( 3, 2, 2, 2, 3 ),
 ( 0.8255245790564514907, 0.8325803338241195561, 0.8396360993650018312, 0.8466918649058843283, 0.8466920362367552633 ),
 .UNSPECIFIED. ) 
 CURVE ( )  GEOMETRIC_REPRESENTATION_ITEM ( )  RATIONAL_B_SPLINE_CURVE ( ( 1.000000000000000000, 0.8660254037844387076, 1.000000000000000000, 0.8660254037844387076, 1.000000000000000000, 0.8660254037844387076, 1.000000000000000000, 0.9999967467762187479, 0.9999934937104295596 ) ) 
 REPRESENTATION_ITEM ( '' )  );
#68580 = VERTEX_POINT ( 'NONE', #40416 ) ;
#68581 = CARTESIAN_POINT ( 'NONE',  ( -95.00000000000002842, 92.66308142843932671, 78.68906250086713783 ) ) ;
#68582 = EDGE_CURVE ( 'NONE', #67171, #55390, #13198, .T. ) ;
#68583 = CARTESIAN_POINT ( 'NONE',  ( 4.755015822784811164, -4.336808689942017736E-16, 0.000000000000000000 ) ) ;
#68584 = AXIS2_PLACEMENT_3D ( 'NONE', #67530, #25907, #60146 ) ;
#68585 = DIRECTION ( 'NONE',  ( -1.000000000000000000, 0.000000000000000000, -0.000000000000000000 ) ) ;
#68586 = EDGE_CURVE ( 'NONE', #39686, #2485, #57345, .T. ) ;
#68587 = AXIS2_PLACEMENT_3D ( 'NONE', #56350, #50317, #44706 ) ;
#68588 = FACE_OUTER_BOUND ( 'NONE', #55968, .T. ) ;
#68589 = CARTESIAN_POINT ( 'NONE',  ( 25.81725066941077529, -113.8380548628854854, -5.500000000000000000 ) ) ;
#68590 = DIRECTION ( 'NONE',  ( -1.000000000000000000, 0.000000000000000000, 0.000000000000000000 ) ) ;
#68591 = CARTESIAN_POINT ( 'NONE',  ( -97.30629616937497417, -208.6684592857803011, 89.11364583420049712 ) ) ;
#68592 = AXIS2_PLACEMENT_3D ( 'NONE', #30738, #59705, #13083 ) ;
#68593 = ADVANCED_FACE ( 'NONE', ( #67512 ), #34035, .F. ) ;
#68594 = CARTESIAN_POINT ( 'NONE',  ( 92.69370383062498320, 91.33154071421968467, 76.41364583420049428 ) ) ;
#68595 = CARTESIAN_POINT ( 'NONE',  ( -97.30629616937497417, -208.6684592857803295, 80.22364583420048234 ) ) ;
#68596 = CARTESIAN_POINT ( 'NONE',  ( 0.000000000000000000, 14.66109333815460225, 73.73191006444577056 ) ) ;
#68597 = VERTEX_POINT ( 'NONE', #4751 ) ;
#68598 = EDGE_CURVE ( 'NONE', #27660, #27808, #57241, .T. ) ;
#68599 = CARTESIAN_POINT ( 'NONE',  ( 10.00000000000000000, 17.67226234102874116, -33.17418723428288274 ) ) ;
#68600 = CARTESIAN_POINT ( 'NONE',  ( -97.64999999999996305, -209.9999999999999716, 90.00000000000000000 ) ) ;
#68601 = CARTESIAN_POINT ( 'NONE',  ( 0.000000000000000000, 69.42325613327440692, 34.44570377933622041 ) ) ;
#68602 = DIRECTION ( 'NONE',  ( 0.000000000000000000, 0.000000000000000000, -1.000000000000000000 ) ) ;
#68603 = CARTESIAN_POINT ( 'NONE',  ( 96.15314808468748708, -208.0026889286704943, 81.17614583420048291 ) ) ;
#68604 = ORIENTED_EDGE ( 'NONE', *, *, #33775, .T. ) ;
#68605 = LINE ( 'NONE', #16726, #70700 ) ;
#68606 = EDGE_CURVE ( 'NONE', #46926, #55521, #52396, .T. ) ;
#68607 = VERTEX_POINT ( 'NONE', #63366 ) ;
#68608 = DIRECTION ( 'NONE',  ( 0.000000000000000000, 0.000000000000000000, 1.000000000000000000 ) ) ;
#68609 = ADVANCED_FACE ( 'NONE', ( #63014 ), #50960, .F. ) ;
#68610 = ORIENTED_EDGE ( 'NONE', *, *, #61387, .T. ) ;
#68611 = CIRCLE ( 'NONE', #9773, 82.00000000000000000 ) ;
#68612 = DIRECTION ( 'NONE',  ( -1.000000000000000000, -1.343011723336883198E-16, -0.000000000000000000 ) ) ;
#68613 = EDGE_CURVE ( 'NONE', #40077, #63927, #62024, .T. ) ;
#68614 = CIRCLE ( 'NONE', #62789, 11.59999999999999964 ) ;
#68615 = ORIENTED_EDGE ( 'NONE', *, *, #30213, .F. ) ;
#68616 = VERTEX_POINT ( 'NONE', #73507 ) ;
#68617 = ORIENTED_EDGE ( 'NONE', *, *, #23177, .F. ) ;
#68618 = CARTESIAN_POINT ( 'NONE',  ( 97.30629616937498838, -211.3315407142195852, 76.09614583420048461 ) ) ;
#68619 = CIRCLE ( 'NONE', #28994, 82.00000000000000000 ) ;
#68620 = EDGE_CURVE ( 'NONE', #70501, #70390, #22390, .T. ) ;
#68621 = ORIENTED_EDGE ( 'NONE', *, *, #56958, .F. ) ;
#68622 =( REPRESENTATION_RELATIONSHIP ('NONE','NONE', #31117, #33525 ) REPRESENTATION_RELATIONSHIP_WITH_TRANSFORMATION ( #62828 )SHAPE_REPRESENTATION_RELATIONSHIP( ) );
#68623 = FACE_OUTER_BOUND ( 'NONE', #27262, .T. ) ;
#68624 = ORIENTED_EDGE ( 'NONE', *, *, #47975, .F. ) ;
#68625 = CARTESIAN_POINT ( 'NONE',  ( 96.15314808468748708, 88.00268892867053694, 83.02822916753380866 ) ) ;
#68626 = CARTESIAN_POINT ( 'NONE',  ( 96.32499999999998863, -212.2949673200287179, 79.41666666666665719 ) ) ;
#68627 = ORIENTED_EDGE ( 'NONE', *, *, #20894, .T. ) ;
#68628 = EDGE_CURVE ( 'NONE', #17937, #48269, #21641, .T. ) ;
#68629 = ORIENTED_EDGE ( 'NONE', *, *, #11797, .T. ) ;
#68630 = ORIENTED_EDGE ( 'NONE', *, *, #55330, .T. ) ;
#68631 = ORIENTED_EDGE ( 'NONE', *, *, #28534, .T. ) ;
#68632 = AXIS2_PLACEMENT_3D ( 'NONE', #15566, #39617, #56913 ) ;
#68633 = CONICAL_SURFACE ( 'NONE', #42232, 2.649999999999999467, 1.029744258676654312 ) ;
#68634 = CARTESIAN_POINT ( 'NONE',  ( -92.34999999999999432, -210.0000000024460576, 75.15687493084206494 ) ) ;
#68635 = CARTESIAN_POINT ( 'NONE',  ( -2.499999999999970690, 73.00000000000001421, -204.9999999999999716 ) ) ;
#68636 = CARTESIAN_POINT ( 'NONE',  ( 57.50000000000000000, 7.347880794884118356E-15, -275.0000000000000000 ) ) ;
#68637 = VECTOR ( 'NONE', #69051, 1000.000000000000000 ) ;
#68638 = FACE_OUTER_BOUND ( 'NONE', #56349, .T. ) ;
#68639 = CARTESIAN_POINT ( 'NONE',  ( 11.99999999999999822, 50.95692526931329525, 58.39081064771768581 ) ) ;
#68640 = DIRECTION ( 'NONE',  ( 0.000000000000000000, 0.9876883405951372152, 0.1564344650402347547 ) ) ;
#68641 = ORIENTED_EDGE ( 'NONE', *, *, #43714, .T. ) ;
#68642 = CARTESIAN_POINT ( 'NONE',  ( -97.64999999999994884, -208.4700217866474645, 82.40645833506762585 ) ) ;
#68643 = ORIENTED_EDGE ( 'NONE', *, *, #17608, .F. ) ;
#68644 = DIRECTION ( 'NONE',  ( 0.000000000000000000, 0.000000000000000000, 1.000000000000000000 ) ) ;
#68645 = ORIENTED_EDGE ( 'NONE', *, *, #74018, .F. ) ;
#68647 = CARTESIAN_POINT ( 'NONE',  ( -95.00000000000002842, 86.94004357329504273, 80.71312500173431204 ) ) ;
#68646 = CARTESIAN_POINT ( 'NONE',  ( 93.67499999999999716, 87.70503267997126784, 78.12020833506763040 ) ) ;
#68648 = ORIENTED_EDGE ( 'NONE', *, *, #65617, .F. ) ;
#68649 = CARTESIAN_POINT ( 'NONE',  ( 92.69370383062498320, 91.33154071421968467, 80.22364583420048234 ) ) ;
#68650 = CARTESIAN_POINT ( 'NONE',  ( -92.34999999999999432, -209.9999999999999716, 86.50750000000000739 ) ) ;
#68651 = CARTESIAN_POINT ( 'NONE',  ( 10.00000000000000000, 17.28742895386191236, -75.54627589209927407 ) ) ;
#68652 = PLANE ( 'NONE',  #24234 ) ;
#68653 = DIRECTION ( 'NONE',  ( 0.000000000000000000, 0.000000000000000000, -1.000000000000000000 ) ) ;
#68654 = EDGE_LOOP ( 'NONE', ( #19960, #61784, #23221, #50328 ) ) ;
#68655 = CARTESIAN_POINT ( 'NONE',  ( 10.00000000000000000, 12.26510123303308752, -35.53030884539072787 ) ) ;
#68656 = DIRECTION ( 'NONE',  ( -1.000000000000000000, -0.000000000000000000, 0.000000000000000000 ) ) ;
#68657 = PLANE ( 'NONE',  #34819 ) ;
#68658 = ORIENTED_EDGE ( 'NONE', *, *, #34652, .T. ) ;
#68659 = VERTEX_POINT ( 'NONE', #45337 ) ;
#68660 = DIRECTION ( 'NONE',  ( 0.000000000000000000, 0.000000000000000000, 1.000000000000000000 ) ) ;
#68661 = DIRECTION ( 'NONE',  ( 0.000000000000000000, 0.8090169943749445647, 0.5877852522924770229 ) ) ;
#68662 = CARTESIAN_POINT ( 'NONE',  ( 10.00000000000000000, 41.81611651403861885, 3.925862922256313503 ) ) ;
#68663 = CARTESIAN_POINT ( 'NONE',  ( -97.30629616937497417, -211.3315407142195852, 82.23447916753383424 ) ) ;
#68664 = ORIENTED_EDGE ( 'NONE', *, *, #70191, .T. ) ;
#68665 = ORIENTED_EDGE ( 'NONE', *, *, #32246, .T. ) ;
#68666 =( GEOMETRIC_REPRESENTATION_CONTEXT ( 3 ) GLOBAL_UNCERTAINTY_ASSIGNED_CONTEXT ( ( #42873 ) ) GLOBAL_UNIT_ASSIGNED_CONTEXT ( ( #64632, #70993, #52237 ) ) REPRESENTATION_CONTEXT ( 'NONE', 'WORKASPACE' ) );
#68667 = AXIS2_PLACEMENT_3D ( 'NONE', #63483, #11960, #367 ) ;
#68668 = EDGE_CURVE ( 'NONE', #64530, #769, #16000, .T. ) ;
#68669 = CARTESIAN_POINT ( 'NONE',  ( 2.746707903440850533E-12, -120.0000000000000000, -70.59999999999999432 ) ) ;
#68670 = LINE ( 'NONE', #28805, #71450 ) ;
#68671 = EDGE_CURVE ( 'NONE', #52624, #23895, #24865, .T. ) ;
#68672 = VECTOR ( 'NONE', #57938, 1000.000000000000000 ) ;
#68673 = CARTESIAN_POINT ( 'NONE',  ( 10.00000000000000000, -21.32104025579135964, 30.84782396557210760 ) ) ;
#68674 = CARTESIAN_POINT ( 'NONE',  ( 92.69370383062498320, 91.33154071421968467, 74.98489583420048632 ) ) ;
#68675 = LINE ( 'NONE', #32584, #67698 ) ;
#68676 = CARTESIAN_POINT ( 'NONE',  ( 1.560000000000000053, 0.8660254037844389297, -1.500000000000000000 ) ) ;
#68677 = DIRECTION ( 'NONE',  ( 0.000000000000000000, 0.2334453638558991184, 0.9723699203976781114 ) ) ;
#68678 = CARTESIAN_POINT ( 'NONE',  ( 0.000000000000000000, 0.000000000000000000, 0.000000000000000000 ) ) ;
#68679 = EDGE_CURVE ( 'NONE', #20162, #13138, #66889, .T. ) ;
#68681 = EDGE_CURVE ( 'NONE', #7439, #2929, #52451, .T. ) ;
#68680 = DIRECTION ( 'NONE',  ( 0.000000000000000000, 0.2079116908177664758, 0.9781476007338042455 ) ) ;
#68682 = DIRECTION ( 'NONE',  ( 0.9918136447140100120, -0.1276937514489704939, 0.000000000000000000 ) ) ;
#68683 = AXIS2_PLACEMENT_3D ( 'NONE', #50956, #45333, #33277 ) ;
#68684 = CARTESIAN_POINT ( 'NONE',  ( 93.84685191531248449, 88.00268892867053694, 87.36739583420049371 ) ) ;
#68685 = CARTESIAN_POINT ( 'NONE',  ( -97.30629616937495996, -209.9999999999999716, 88.53156250086716739 ) ) ;
#68686 = CARTESIAN_POINT ( 'NONE',  ( 5.999999999999999112, 79.10210256391368944, 21.60688246758614994 ) ) ;
#68687 = ORIENTED_EDGE ( 'NONE', *, *, #63403, .F. ) ;
#68688 = LINE ( 'NONE', #45764, #22027 ) ;
#68689 = CARTESIAN_POINT ( 'NONE',  ( -97.30629616937501680, 91.33154071421968467, 78.15989583420048348 ) ) ;
#68690 = AXIS2_PLACEMENT_3D ( 'NONE', #67346, #43691, #22228 ) ;
#68691 = VECTOR ( 'NONE', #47478, 1000.000000000000000 ) ;
#68692 = VECTOR ( 'NONE', #29820, 1000.000000000000000 ) ;
#68693 = EDGE_CURVE ( 'NONE', #2465, #13867, #21209, .T. ) ;
#68694 = CARTESIAN_POINT ( 'NONE',  ( 0.000000000000000000, 35.53030884539084866, 12.26510123303271982 ) ) ;
#68695 = ORIENTED_EDGE ( 'NONE', *, *, #31668, .F. ) ;
#68696 = DIRECTION ( 'NONE',  ( 0.000000000000000000, -0.9510565162951536422, -0.3090169943749471182 ) ) ;
#68697 = DIRECTION ( 'NONE',  ( 0.000000000000000000, 1.000000000000000000, -6.938893903907229364E-16 ) ) ;
#68698 = FACE_OUTER_BOUND ( 'NONE', #9183, .T. ) ;
#68699 = ADVANCED_BREP_SHAPE_REPRESENTATION ( '', ( #12651, #43395 ), #60192 ) ;
#68700 = CARTESIAN_POINT ( 'NONE',  ( -93.67499999999998295, -207.7050326799711968, 84.70833333333332860 ) ) ;
#68701 = ADVANCED_FACE ( 'NONE', ( #67885 ), #51322, .T. ) ;
#68702 = ADVANCED_FACE ( 'NONE', ( #23501 ), #12943, .T. ) ;
#68703 = CARTESIAN_POINT ( 'NONE',  ( 92.69370383062501162, -209.9999999999999716, 76.46656250086715545 ) ) ;
#68704 = ORIENTED_EDGE ( 'NONE', *, *, #20632, .T. ) ;
#68705 = ORIENTED_EDGE ( 'NONE', *, *, #13179, .T. ) ;
#68706 = CARTESIAN_POINT ( 'NONE',  ( 93.84685191531251292, -211.9973110713294489, 85.46239583420047836 ) ) ;
#68707 = DIRECTION ( 'NONE',  ( -0.000000000000000000, -0.000000000000000000, -1.000000000000000000 ) ) ;
#68708 = EDGE_CURVE ( 'NONE', #66935, #54483, #3270, .T. ) ;
#68709 = CARTESIAN_POINT ( 'NONE',  ( 11.99999999999999822, 0.000000000000000000, 0.000000000000000000 ) ) ;
#68710 = CARTESIAN_POINT ( 'NONE',  ( 10.00000000000000000, -12.42422080174663712, 35.38097989696507994 ) ) ;
#68711 = DIRECTION ( 'NONE',  ( 0.000000000000000000, 0.000000000000000000, 1.000000000000000000 ) ) ;
#68712 = LINE ( 'NONE', #56688, #46512 ) ;
#68713 = CARTESIAN_POINT ( 'NONE',  ( 93.67500000000001137, -207.7050326799711968, 89.25916666666667254 ) ) ;
#68714 = VERTEX_POINT ( 'NONE', #29866 ) ;
#68715 =( GEOMETRIC_REPRESENTATION_CONTEXT ( 3 ) GLOBAL_UNCERTAINTY_ASSIGNED_CONTEXT ( ( #68008 ) ) GLOBAL_UNIT_ASSIGNED_CONTEXT ( ( #46513, #69804, #58915 ) ) REPRESENTATION_CONTEXT ( 'NONE', 'WORKASPACE' ) );
#68716 = CIRCLE ( 'NONE', #55507, 31.99999999999999289 ) ;
#68717 = ORIENTED_EDGE ( 'NONE', *, *, #55997, .F. ) ;
#68718 = ORIENTED_EDGE ( 'NONE', *, *, #1563, .T. ) ;
#68719 = ORIENTED_EDGE ( 'NONE', *, *, #68240, .F. ) ;
#68720 = FACE_OUTER_BOUND ( 'NONE', #12180, .T. ) ;
#68721 = AXIS2_PLACEMENT_3D ( 'NONE', #41653, #58579, #2220 ) ;
#68722 = FACE_OUTER_BOUND ( 'NONE', #24586, .T. ) ;
#68723 = CARTESIAN_POINT ( 'NONE',  ( 93.67499999999999716, 87.70503267997126784, 87.56583333333333030 ) ) ;
#68724 = CARTESIAN_POINT ( 'NONE',  ( 96.32499999999998863, -207.7050326799711968, 77.16770833506762983 ) ) ;
#68725 = CARTESIAN_POINT ( 'NONE',  ( 96.32499999999998863, 87.70503267997126784, 79.41666666666665719 ) ) ;
#68726 = ORIENTED_EDGE ( 'NONE', *, *, #1312, .T. ) ;
#68727 = CARTESIAN_POINT ( 'NONE',  ( 0.000000000000000000, 0.000000000000000000, 0.000000000000000000 ) ) ;
#68728 = CIRCLE ( 'NONE', #18314, 62.50000000000000000 ) ;
#68729 = ORIENTED_EDGE ( 'NONE', *, *, #66974, .F. ) ;
#68730 = DIRECTION ( 'NONE',  ( 0.000000000000000000, 0.9969173337331281859, -0.07845909572784168229 ) ) ;
#68731 = EDGE_LOOP ( 'NONE', ( #22801, #39197, #42100, #14481 ) ) ;
#68732 = CARTESIAN_POINT ( 'NONE',  ( 92.35000000019411459, 89.99998015682159291, 84.36502760998348549 ) ) ;
#68733 = AXIS2_PLACEMENT_3D ( 'NONE', #49119, #55131, #20556 ) ;
#68734 = CARTESIAN_POINT ( 'NONE',  ( -92.69370383062505425, 91.33154071421968467, 81.91697916753383879 ) ) ;
#68735 = CARTESIAN_POINT ( 'NONE',  ( 92.69370383062498320, 88.66845928578037217, 78.90072916753381094 ) ) ;
#68736 = ORIENTED_EDGE ( 'NONE', *, *, #47473, .T. ) ;
#68737 = DIRECTION ( 'NONE',  ( -0.000000000000000000, -0.000000000000000000, 1.000000000000000000 ) ) ;
#68738 = DIRECTION ( 'NONE',  ( -1.000000000000000000, 0.000000000000000000, 0.000000000000000000 ) ) ;
#68739 = DIRECTION ( 'NONE',  ( -1.000000000000000000, -0.000000000000000000, 0.000000000000000000 ) ) ;
#68740 = CARTESIAN_POINT ( 'NONE',  ( -92.34999999999999432, -209.9999999999999716, 77.61749999999999261 ) ) ;
#68741 = EDGE_LOOP ( 'NONE', ( #58323, #37213, #34863, #8780 ) ) ;
#68742 = CARTESIAN_POINT ( 'NONE',  ( -5.000000000000000888, -1.936377641173862463, -5.802630826755077464 ) ) ;
#68743 = VECTOR ( 'NONE', #59784, 1000.000000000000000 ) ;
#68744 = CARTESIAN_POINT ( 'NONE',  ( -92.69370383062498320, -209.9999999999999716, 78.53031250086714010 ) ) ;
#68745 = EDGE_LOOP ( 'NONE', ( #35564, #4299, #65134, #64900 ) ) ;
#68746 = ORIENTED_EDGE ( 'NONE', *, *, #29176, .F. ) ;
#68747 = FACE_BOUND ( 'NONE', #20745, .T. ) ;
#68748 = VERTEX_POINT ( 'NONE', #69359 ) ;
#68749 = CARTESIAN_POINT ( 'NONE',  ( -95.00000000000002842, 90.00000000000004263, 90.00000000000000000 ) ) ;
#68750 = DIRECTION ( 'NONE',  ( 0.000000000000000000, 0.000000000000000000, 1.000000000000000000 ) ) ;
#68751 = ORIENTED_EDGE ( 'NONE', *, *, #11148, .F. ) ;
#68752 = CARTESIAN_POINT ( 'NONE',  ( -96.15314808468747287, -208.0026889286704943, 76.20197916753380696 ) ) ;
#68753 = ORIENTED_EDGE ( 'NONE', *, *, #50238, .T. ) ;
#68754 = DIRECTION ( 'NONE',  ( -1.000000000000000000, 0.000000000000000000, -0.000000000000000000 ) ) ;
#68755 = DIRECTION ( 'NONE',  ( 0.000000000000000000, 0.000000000000000000, -1.000000000000000000 ) ) ;
#68756 = DIRECTION ( 'NONE',  ( -1.000000000000000000, 0.000000000000000000, 0.000000000000000000 ) ) ;
#68757 = CARTESIAN_POINT ( 'NONE',  ( 95.00000000000000000, -206.9400435732949575, 81.58624999999999261 ) ) ;
#68758 = ADVANCED_FACE ( 'NONE', ( #24976, #36257 ), #64845, .F. ) ;
#68759 = DIRECTION ( 'NONE',  ( -1.000000000000000000, 7.571544473058805744E-15, 2.612289469705706870E-14 ) ) ;
#68760 = ADVANCED_FACE ( 'NONE', ( #17856 ), #35518, .F. ) ;
#68761 = CARTESIAN_POINT ( 'NONE',  ( 92.35000000000000853, -208.4700217866474645, 86.21645833506764234 ) ) ;
#68762 = CARTESIAN_POINT ( 'NONE',  ( 94.99999999999998579, 92.66308142843932671, 86.30906250086714238 ) ) ;
#68763 = CARTESIAN_POINT ( 'NONE',  ( 0.000000000000000000, -46.53671651293991118, 59.03961581697383565 ) ) ;
#68764 = DIRECTION ( 'NONE',  ( -1.000000000000000000, 3.061616997868382648E-16, 0.000000000000000000 ) ) ;
#68765 = CARTESIAN_POINT ( 'NONE',  ( 12.50000000000000000, -132.5000000000000000, 40.00000000000000000 ) ) ;
#68766 = DIRECTION ( 'NONE',  ( 0.000000000000000000, 0.1564344650402243742, 0.9876883405951387696 ) ) ;
#68768 = EDGE_CURVE ( 'NONE', #28823, #32140, #32045, .T. ) ;
#68767 = CARTESIAN_POINT ( 'NONE',  ( 12.00000000000000000, 5.835314593368470248, -22.81335362449854642 ) ) ;
#68769 = CARTESIAN_POINT ( 'NONE',  ( 0.9112620892300974385, 5.247385279376962863, -1.160540885688332136 ) ) ;
#68770 = DIRECTION ( 'NONE',  ( 0.000000000000000000, 0.000000000000000000, 1.000000000000000000 ) ) ;
#68771 = EDGE_CURVE ( 'NONE', #40323, #52067, #29492, .T. ) ;
#68772 = DIRECTION ( 'NONE',  ( -1.000000000000000000, 0.000000000000000000, 0.000000000000000000 ) ) ;
#68773 = DIRECTION ( 'NONE',  ( -1.000000000000000000, 0.000000000000000000, 0.000000000000000000 ) ) ;
#68774 = EDGE_CURVE ( 'NONE', #30420, #55313, #35645, .T. ) ;
#68775 = CARTESIAN_POINT ( 'NONE',  ( -95.00000000000002842, 87.33691857156074434, 89.16656250086712987 ) ) ;
#68776 = CARTESIAN_POINT ( 'NONE',  ( -0.8815729230226008184, -93.47222532549339746, 5.500000000000000000 ) ) ;
#68777 = AXIS2_PLACEMENT_3D ( 'NONE', #37746, #54298, #71188 ) ;
#68778 = ADVANCED_FACE ( 'NONE', ( #983 ), #13688, .T. ) ;
#68779 = CIRCLE ( 'NONE', #46978, 82.00000000000000000 ) ;
#68780 = CARTESIAN_POINT ( 'NONE',  ( 94.99999999999998579, 86.94004357329502852, 85.71374999999999034 ) ) ;
#68781 = EDGE_CURVE ( 'NONE', #3354, #30420, #63738, .T. ) ;
#68782 = AXIS2_PLACEMENT_3D ( 'NONE', #74331, #67209, #5561 ) ;
#68783 =( BOUNDED_CURVE ( )  B_SPLINE_CURVE ( 2, ( #17442, #41122, #52766, #17076, #52012, #40369, #62967 ),
 .UNSPECIFIED., .F., .F. ) 
 B_SPLINE_CURVE_WITH_KNOTS ( ( 3, 2, 2, 3 ),
 ( 0.9101937466091533091, 0.9172495203147085219, 0.9243052858555913520, 0.9313609857393202462 ),
 .UNSPECIFIED. ) 
 CURVE ( )  GEOMETRIC_REPRESENTATION_ITEM ( )  RATIONAL_B_SPLINE_CURVE ( ( 1.000000000000000000, 0.8660254037844387076, 1.000000000000000000, 0.8660254037844387076, 1.000000000000000000, 0.8660266504798735943, 0.9999975066323323336 ) ) 
 REPRESENTATION_ITEM ( '' )  );
#68784 = VERTEX_POINT ( 'NONE', #18957 ) ;
#68785 = DIRECTION ( 'NONE',  ( 0.000000000000000000, -0.5877852522924797984, -0.8090169943749426773 ) ) ;
#68786 = CYLINDRICAL_SURFACE ( 'NONE', #15525, 2.649999999999999467 ) ;
#68787 = CARTESIAN_POINT ( 'NONE',  ( -0.9515373497862389396, -96.47140937769621871, -5.500000000000000000 ) ) ;
#68788 = CYLINDRICAL_SURFACE ( 'NONE', #65451, 32.00000000000000000 ) ;
#68789 = CARTESIAN_POINT ( 'NONE',  ( 10.00000000000000000, -29.81001611431024756, 22.74946021919122785 ) ) ;
#68790 = AXIS2_PLACEMENT_3D ( 'NONE', #45275, #68197, #16693 ) ;
#68791 = EDGE_CURVE ( 'NONE', #52143, #10923, #2112, .T. ) ;
#68793 = EDGE_CURVE ( 'NONE', #40041, #3329, #70830, .T. ) ;
#68792 = CIRCLE ( 'NONE', #34000, 37.49900000000000944 ) ;
#68794 = CARTESIAN_POINT ( 'NONE',  ( 96.15314808468750130, -211.9973110713294489, 84.29822916753381890 ) ) ;
#68795 = VERTEX_POINT ( 'NONE', #42288 ) ;
#68796 = VERTEX_POINT ( 'NONE', #52817 ) ;
#68797 = CARTESIAN_POINT ( 'NONE',  ( 2.874421927457452952, -143.3717286177755739, 5.500000000000000000 ) ) ;
#68798 = ORIENTED_EDGE ( 'NONE', *, *, #71795, .T. ) ;
#68799 = DIRECTION ( 'NONE',  ( 1.000000000000000000, 0.000000000000000000, 0.000000000000000000 ) ) ;
#68800 = CARTESIAN_POINT ( 'NONE',  ( 92.69370383062501162, -209.9999999999999716, 77.57781250086713953 ) ) ;
#68801 = ORIENTED_EDGE ( 'NONE', *, *, #54402, .T. ) ;
#68802 = CARTESIAN_POINT ( 'NONE',  ( 96.15314808468748708, -208.0026889286704943, 83.87489583420048689 ) ) ;
#68803 = ORIENTED_EDGE ( 'NONE', *, *, #18724, .F. ) ;
#68804 = DIRECTION ( 'NONE',  ( -0.7585478161175716050, -0.6516173805718067369, 0.000000000000000000 ) ) ;
#68805 = ORIENTED_EDGE ( 'NONE', *, *, #19913, .T. ) ;
#68806 = ORIENTED_EDGE ( 'NONE', *, *, #40850, .F. ) ;
#68807 = FACE_OUTER_BOUND ( 'NONE', #22460, .T. ) ;
#68808 = CARTESIAN_POINT ( 'NONE',  ( 92.35000000000000853, -209.9999999999999716, 80.47499999999999432 ) ) ;
#68809 = VERTEX_POINT ( 'NONE', #18592 ) ;
#68810 = CARTESIAN_POINT ( 'NONE',  ( 95.00000000000000000, -213.0599564267049857, 76.90312500173429555 ) ) ;
#68811 = CARTESIAN_POINT ( 'NONE',  ( 97.64999999999997726, -211.5299782133524502, 87.80395833506763381 ) ) ;
#68812 = ORIENTED_EDGE ( 'NONE', *, *, #70153, .T. ) ;
#68813 = FACE_OUTER_BOUND ( 'NONE', #69369, .T. ) ;
#68814 = VERTEX_POINT ( 'NONE', #59570 ) ;
#68815 = DIRECTION ( 'NONE',  ( -1.000000000000000000, 0.000000000000000000, 0.000000000000000000 ) ) ;
#68816 = EDGE_LOOP ( 'NONE', ( #12334, #31791, #13508, #55581 ) ) ;
#68817 = AXIS2_PLACEMENT_3D ( 'NONE', #3183, #66324, #37744 ) ;
#68818 = ORIENTED_EDGE ( 'NONE', *, *, #22344, .T. ) ;
#68819 = ORIENTED_EDGE ( 'NONE', *, *, #59179, .T. ) ;
#68820 = CARTESIAN_POINT ( 'NONE',  ( -92.35000000018064270, -210.0000309433161476, 78.33187387208045038 ) ) ;
#68821 = CARTESIAN_POINT ( 'NONE',  ( -5.000000000000000000, -1.096207231254244352, -0.7463930790433302986 ) ) ;
#68822 = ORIENTED_EDGE ( 'NONE', *, *, #38128, .T. ) ;
#68823 = CIRCLE ( 'NONE', #15995, 77.49899999999999523 ) ;
#68824 = VERTEX_POINT ( 'NONE', #41904 ) ;
#68826 = EDGE_CURVE ( 'NONE', #57324, #13679, #8055, .T. ) ;
#68825 = VERTEX_POINT ( 'NONE', #7327 ) ;
#68827 = CYLINDRICAL_SURFACE ( 'NONE', #60163, 2.649999999999999467 ) ;
#68828 = EDGE_CURVE ( 'NONE', #50573, #8248, #44036, .T. ) ;
#68829 = CARTESIAN_POINT ( 'NONE',  ( -92.35000000000005116, 91.52997821335253548, 86.56041666666665435 ) ) ;
#68830 = ORIENTED_EDGE ( 'NONE', *, *, #26050, .T. ) ;
#68831 = DIRECTION ( 'NONE',  ( 0.000000000000000000, 0.9135454576426055295, 0.4067366430757899387 ) ) ;
#68832 = EDGE_CURVE ( 'NONE', #33969, #73349, #10936, .T. ) ;
#68833 = VERTEX_POINT ( 'NONE', #62007 ) ;
#68834 = CARTESIAN_POINT ( 'NONE',  ( 0.000000000000000000, 6.736453364084091788, -36.88895765772625879 ) ) ;
#68835 = CARTESIAN_POINT ( 'NONE',  ( -92.69370383062498320, -211.3315407142195852, 87.36739583420047950 ) ) ;
#68836 = EDGE_LOOP ( 'NONE', ( #20507, #48214, #12363, #29885 ) ) ;
#68837 = VECTOR ( 'NONE', #46297, 1000.000000000000000 ) ;
#68838 = DIRECTION ( 'NONE',  ( 0.000000000000000000, 0.2079116908177532363, 0.9781476007338069101 ) ) ;
#68839 = CARTESIAN_POINT ( 'NONE',  ( 11.99999999999999822, 0.000000000000000000, 0.000000000000000000 ) ) ;
#68840 = CARTESIAN_POINT ( 'NONE',  ( 0.000000000000000000, 16.65972982744933972, 80.28980883073764119 ) ) ;
#68841 = CARTESIAN_POINT ( 'NONE',  ( -92.69370383062498320, -208.6684592857803295, 75.40822916753381833 ) ) ;
#68842 = EDGE_CURVE ( 'NONE', #23489, #65637, #50335, .T. ) ;
#68843 = VECTOR ( 'NONE', #37087, 1000.000000000000000 ) ;
#68844 = DIRECTION ( 'NONE',  ( 0.000000000000000000, 0.000000000000000000, 1.000000000000000000 ) ) ;
#68845 = DIRECTION ( 'NONE',  ( 0.000000000000000000, 0.000000000000000000, 1.000000000000000000 ) ) ;
#68846 = CIRCLE ( 'NONE', #62854, 31.99999999999998579 ) ;
#68847 = AXIS2_PLACEMENT_3D ( 'NONE', #16227, #52291, #63223 ) ;
#68848 = AXIS2_PLACEMENT_3D ( 'NONE', #4049, #37510, #14932 ) ;
#68849 = EDGE_CURVE ( 'NONE', #29023, #40438, #57049, .T. ) ;
#68850 = CARTESIAN_POINT ( 'NONE',  ( 10.00000000000000000, -37.58145647212453611, -0.6853352020794456489 ) ) ;
#68851 = DIRECTION ( 'NONE',  ( 0.000000000000000000, 0.000000000000000000, -1.000000000000000000 ) ) ;
#68852 = FACE_OUTER_BOUND ( 'NONE', #50772, .T. ) ;
#68853 = CARTESIAN_POINT ( 'NONE',  ( -92.69370383062504004, 90.00000000000004263, 79.16531250086714522 ) ) ;
#68854 = CARTESIAN_POINT ( 'NONE',  ( -2.499999999999968914, 79.99999999999998579, -269.9999999999999432 ) ) ;
#68855 = DIRECTION ( 'NONE',  ( -1.000000000000000000, 0.000000000000000000, 0.000000000000000000 ) ) ;
#68856 = EDGE_CURVE ( 'NONE', #49560, #31776, #36833, .T. ) ;
#68857 = EDGE_LOOP ( 'NONE', ( #51115, #61127, #11294, #18132 ) ) ;
#68858 = FACE_OUTER_BOUND ( 'NONE', #15720, .T. ) ;
#68859 = CARTESIAN_POINT ( 'NONE',  ( 0.000000000000000000, 26.01480285779837232, 70.53064760720326376 ) ) ;
#68860 = CARTESIAN_POINT ( 'NONE',  ( -20.63749999999999574, -2.946905753440916183E-14, -1.643265707205091412E-14 ) ) ;
#68861 = DIRECTION ( 'NONE',  ( -0.000000000000000000, -0.000000000000000000, 1.000000000000000000 ) ) ;
#68862 = CARTESIAN_POINT ( 'NONE',  ( -3.000000000000000000, 20.85821328998756385, -10.92862929874494959 ) ) ;
#68863 = DIRECTION ( 'NONE',  ( -1.000000000000000000, 0.000000000000000000, 0.000000000000000000 ) ) ;
#68864 = CARTESIAN_POINT ( 'NONE',  ( -97.30629616937497417, -208.6684592857803011, 75.77864583420048916 ) ) ;
#68865 = EDGE_CURVE ( 'NONE', #55001, #56348, #71652, .T. ) ;
#68866 = CARTESIAN_POINT ( 'NONE',  ( -3.000000000000000000, 5.835314593368772229, -22.81335362449846826 ) ) ;
#68867 = EDGE_CURVE ( 'NONE', #38604, #8405, #45291, .T. ) ;
#68868 = ORIENTED_EDGE ( 'NONE', *, *, #53695, .F. ) ;
#68869 = DIRECTION ( 'NONE',  ( -0.8090169943749426773, -0.5877852522924797984, 0.000000000000000000 ) ) ;
#68870 = CARTESIAN_POINT ( 'NONE',  ( 6.000000000000000000, 10.30890764327382136, 81.34940948281339956 ) ) ;
#68871 = CARTESIAN_POINT ( 'NONE',  ( 10.00000000000000000, 17.80606268964540462, 33.00180498840053644 ) ) ;
#68872 = ORIENTED_EDGE ( 'NONE', *, *, #29780, .F. ) ;
#68873 = CARTESIAN_POINT ( 'NONE',  ( -2.500000000000017319, -80.00000000000001421, -269.9999999999999432 ) ) ;
#68874 = VECTOR ( 'NONE', #63440, 1000.000000000000114 ) ;
#68875 = DIRECTION ( 'NONE',  ( 1.000000000000000000, 0.000000000000000000, 0.000000000000000000 ) ) ;
#68876 = ORIENTED_EDGE ( 'NONE', *, *, #21884, .T. ) ;
#68877 = CARTESIAN_POINT ( 'NONE',  ( 10.00000000000000000, 31.46837873495072913, -68.27212725128242710 ) ) ;
#68878 = CARTESIAN_POINT ( 'NONE',  ( -2.500000000000000000, 16.00000000000000000, 0.000000000000000000 ) ) ;
#68879 = ORIENTED_EDGE ( 'NONE', *, *, #3857, .F. ) ;
#68880 = CARTESIAN_POINT ( 'NONE',  ( 97.30629616937498838, -209.9999999999999716, 88.69031250086715090 ) ) ;
#68881 = DIRECTION ( 'NONE',  ( 1.000000000000000000, 0.000000000000000000, 0.000000000000000000 ) ) ;
#68882 = AXIS2_PLACEMENT_3D ( 'NONE', #297, #15025, #60902 ) ;
#68883 = ORIENTED_EDGE ( 'NONE', *, *, #41071, .T. ) ;
#68884 = DIRECTION ( 'NONE',  ( -1.000000000000000000, -0.000000000000000000, 0.000000000000000000 ) ) ;
#68885 = ORIENTED_EDGE ( 'NONE', *, *, #14572, .F. ) ;
#68886 = CIRCLE ( 'NONE', #5261, 11.59999999999999787 ) ;
#68887 = CARTESIAN_POINT ( 'NONE',  ( 0.000000000000000000, 50.23322058963442061, -64.81221759200289512 ) ) ;
#68888 = ORIENTED_EDGE ( 'NONE', *, *, #36061, .T. ) ;
#68889 = CIRCLE ( 'NONE', #10012, 42.00000000000000000 ) ;
#68890 = DIRECTION ( 'NONE',  ( 0.000000000000000000, 0.000000000000000000, 1.000000000000000000 ) ) ;
#68891 = VERTEX_POINT ( 'NONE', #33313 ) ;
#68892 = CARTESIAN_POINT ( 'NONE',  ( 10.00000000000000000, 22.64427369931212297, -30.00120703465181293 ) ) ;
#68893 = ORIENTED_EDGE ( 'NONE', *, *, #12450, .T. ) ;
#68894 = VERTEX_POINT ( 'NONE', #56274 ) ;
#68895 = LINE ( 'NONE', #69257, #51268 ) ;
#68896 = ADVANCED_FACE ( 'NONE', ( #23179 ), #69039, .T. ) ;
#68897 = ORIENTED_EDGE ( 'NONE', *, *, #11299, .F. ) ;
#68898 = ORIENTED_EDGE ( 'NONE', *, *, #13005, .T. ) ;
#68899 = DIRECTION ( 'NONE',  ( -7.685483754327489091E-16, -1.065814103640131188E-14, -1.000000000000000000 ) ) ;
#68900 = ORIENTED_EDGE ( 'NONE', *, *, #61306, .T. ) ;
#68901 = AXIS2_PLACEMENT_3D ( 'NONE', #11020, #69995, #29767 ) ;
#68902 = VERTEX_POINT ( 'NONE', #34438 ) ;
#68903 = CARTESIAN_POINT ( 'NONE',  ( 94.99999999999998579, 92.66308142843935514, 85.03906250086714635 ) ) ;
#68904 = EDGE_LOOP ( 'NONE', ( #55851, #22294, #13950, #33890 ) ) ;
#68905 = CARTESIAN_POINT ( 'NONE',  ( 95.00000000000000000, -207.3369185715606307, 80.59406250086715318 ) ) ;
#68906 = APPLICATION_PROTOCOL_DEFINITION ( 'draft international standard', 'automotive_design', 1998, #53241 ) ;
#68907 = DIRECTION ( 'NONE',  ( 0.000000000000000000, 0.000000000000000000, 1.000000000000000000 ) ) ;
#68908 = CARTESIAN_POINT ( 'NONE',  ( 5.000000000000000000, -32.34446384429951138, -26.79245525562750530 ) ) ;
#68909 = CARTESIAN_POINT ( 'NONE',  ( 0.000000000000000000, -8.830959090342926032, 74.65491531819115778 ) ) ;
#68910 = LINE ( 'NONE', #17399, #16399 ) ;
#68911 = ADVANCED_FACE ( 'NONE', ( #33703 ), #22054, .F. ) ;
#68912 = DIRECTION ( 'NONE',  ( -1.000000000000000000, 0.000000000000000000, 0.000000000000000000 ) ) ;
#68913 = CARTESIAN_POINT ( 'NONE',  ( 11.99999999999999822, 2.946379043146343246, 75.11764819372150725 ) ) ;
#68914 = CARTESIAN_POINT ( 'NONE',  ( -94.99999999999997158, -207.3369185715606307, 84.40406250086712703 ) ) ;
#68915 = ADVANCED_FACE ( 'NONE', ( #22814 ), #56658, .F. ) ;
#68916 = CARTESIAN_POINT ( 'NONE',  ( -92.69370383062504004, 90.00000000000004263, 81.86406250086714920 ) ) ;
#68917 = VERTEX_POINT ( 'NONE', #57019 ) ;
#68918 = VECTOR ( 'NONE', #20348, 1000.000000000000000 ) ;
#68920 = CARTESIAN_POINT ( 'NONE',  ( -92.69370383062502583, 88.66845928578038638, 86.09739583420048348 ) ) ;
#68919 = CARTESIAN_POINT ( 'NONE',  ( 97.30629616937498838, 88.66845928578037217, 84.82739583420045903 ) ) ;
#68921 = VERTEX_POINT ( 'NONE', #73919 ) ;
#68922 = DIRECTION ( 'NONE',  ( 0.000000000000000000, -0.9945218953682730678, 0.1045284632676570929 ) ) ;
#68923 = DIRECTION ( 'NONE',  ( 1.000000000000000000, 0.000000000000000000, 0.000000000000000000 ) ) ;
#68924 = DIRECTION ( 'NONE',  ( 1.000000000000000000, 1.427937372958405461E-15, 7.962523111839130290E-16 ) ) ;
#68925 = CARTESIAN_POINT ( 'NONE',  ( -5.000000000000000888, 0.9828435001097632906, -5.956909652965543422 ) ) ;
#68926 = CARTESIAN_POINT ( 'NONE',  ( -97.30629616937497417, -208.6684592857803295, 86.41489583420047893 ) ) ;
#68927 = CARTESIAN_POINT ( 'NONE',  ( -97.64999999999996305, -209.9999999999999716, 81.74500000000000455 ) ) ;
#68928 = ADVANCED_FACE ( 'NONE', ( #5526 ), #17160, .F. ) ;
#68929 = ADVANCED_FACE ( 'NONE', ( #7361 ), #24644, .T. ) ;
#68930 = DIRECTION ( 'NONE',  ( 0.000000000000000000, 0.000000000000000000, 1.000000000000000000 ) ) ;
#68931 = FACE_OUTER_BOUND ( 'NONE', #26866, .T. ) ;
#68932 = CARTESIAN_POINT ( 'NONE',  ( 97.65000000000000568, 88.47002178664753558, 89.62958333333334338 ) ) ;
#68933 = VERTEX_POINT ( 'NONE', #53222 ) ;
#68934 = VECTOR ( 'NONE', #71825, 1000.000000000000000 ) ;
#68935 = ORIENTED_EDGE ( 'NONE', *, *, #3870, .T. ) ;
#68936 = CARTESIAN_POINT ( 'NONE',  ( -95.00000000000002842, 93.05995642670501411, 79.68124999999999147 ) ) ;
#68937 = CARTESIAN_POINT ( 'NONE',  ( 97.65000000000006253, -211.5299782133524502, 88.99458333333333826 ) ) ;
#68938 = CARTESIAN_POINT ( 'NONE',  ( -42.50000000000000000, 1.702802944658382841E-15, 13.90444123027096879 ) ) ;
#68939 = DIRECTION ( 'NONE',  ( 0.000000000000000000, 0.3090169943749480619, -0.9510565162951533091 ) ) ;
#68940 = CARTESIAN_POINT ( 'NONE',  ( 11.99999999999999822, -39.78640506895651896, 66.50666863321988842 ) ) ;
#68941 = CARTESIAN_POINT ( 'NONE',  ( -20.63749999999997797, 1.882991779351789328E-13, 20.20000000000035101 ) ) ;
#68942 = VECTOR ( 'NONE', #49184, 1000.000000000000000 ) ;
#68943 = CARTESIAN_POINT ( 'NONE',  ( 0.000000000000000000, 0.000000000000000000, 0.000000000000000000 ) ) ;
#68944 = AXIS2_PLACEMENT_3D ( 'NONE', #14102, #31398, #54348 ) ;
#68945 = EDGE_CURVE ( 'NONE', #54483, #5078, #7725, .T. ) ;
#68946 = ORIENTED_EDGE ( 'NONE', *, *, #4506, .T. ) ;
#68947 = CARTESIAN_POINT ( 'NONE',  ( -95.00000000000002842, 92.66308142843932671, 76.78406250086712248 ) ) ;
#68948 = DIRECTION ( 'NONE',  ( -1.000000000000000000, 0.000000000000000000, 0.000000000000000000 ) ) ;
#68949 = VECTOR ( 'NONE', #59605, 1000.000000000000227 ) ;
#68950 = AXIS2_PLACEMENT_3D ( 'NONE', #70302, #18806, #1944 ) ;
#68951 = CARTESIAN_POINT ( 'NONE',  ( -93.33864827736697123, -211.6008015735577033, 74.79754476654878204 ) ) ;
#68952 = DIRECTION ( 'NONE',  ( -1.000000000000000000, 0.000000000000000000, -0.000000000000000000 ) ) ;
#68953 = CARTESIAN_POINT ( 'NONE',  ( -97.64999999980585699, -210.0000198431789897, 84.36502761000342332 ) ) ;
#68954 = CARTESIAN_POINT ( 'NONE',  ( 2.426025403784448642, 0.000000000000000000, 2.168404344971008868E-16 ) ) ;
#68955 = CARTESIAN_POINT ( 'NONE',  ( -96.15314808468745866, -211.9973110713294489, 89.27239583420049485 ) ) ;
#68956 = ADVANCED_FACE ( 'NONE', ( #30638 ), #30276, .T. ) ;
#68957 = EDGE_CURVE ( 'NONE', #69250, #14710, #64140, .T. ) ;
#68958 = CARTESIAN_POINT ( 'NONE',  ( 96.15314808468748708, 88.00268892867053694, 76.04322916753382344 ) ) ;
#68959 = CIRCLE ( 'NONE', #13718, 37.49900000000000944 ) ;
#68960 = CARTESIAN_POINT ( 'NONE',  ( -96.15314808468747287, -208.0026889286704943, 80.17072916753382117 ) ) ;
#68961 = DIRECTION ( 'NONE',  ( 0.000000000000000000, 0.000000000000000000, 1.000000000000000000 ) ) ;
#68962 = VERTEX_POINT ( 'NONE', #70480 ) ;
#68963 = CARTESIAN_POINT ( 'NONE',  ( 94.99999999999998579, 86.94004357329502852, 87.69812500173429726 ) ) ;
#68964 = PLANE ( 'NONE',  #61059 ) ;
#68965 = DIRECTION ( 'NONE',  ( 0.000000000000000000, -0.8910065241883722287, 0.4539904997395382003 ) ) ;
#68966 = CARTESIAN_POINT ( 'NONE',  ( -93.84685191531254134, 91.99731107132950569, 76.25489583420049655 ) ) ;
#68967 = CARTESIAN_POINT ( 'NONE',  ( 95.00000000000000000, -212.6630814284392557, 75.83156250086715033 ) ) ;
#68968 = ORIENTED_EDGE ( 'NONE', *, *, #57212, .T. ) ;
#68969 = AXIS2_PLACEMENT_3D ( 'NONE', #1467, #42025, #24356 ) ;
#68970 = DIRECTION ( 'NONE',  ( -1.000000000000000000, -0.000000000000000000, -0.000000000000000000 ) ) ;
#68971 = VERTEX_POINT ( 'NONE', #52853 ) ;
#68972 = CARTESIAN_POINT ( 'NONE',  ( -92.34999999999999432, -210.0000000334413528, 87.85687500050293863 ) ) ;
#68973 = VERTEX_POINT ( 'NONE', #18261 ) ;
#68974 = CARTESIAN_POINT ( 'NONE',  ( 10.00000000000000000, -59.46389618801928378, -49.70050353004953791 ) ) ;
#68975 = AXIS2_PLACEMENT_3D ( 'NONE', #43205, #60847, #31519 ) ;
#68976 = ORIENTED_EDGE ( 'NONE', *, *, #61794, .T. ) ;
#68977 = VERTEX_POINT ( 'NONE', #47212 ) ;
#68978 = VERTEX_POINT ( 'NONE', #12614 ) ;
#68979 = CARTESIAN_POINT ( 'NONE',  ( -94.99999999999997158, -213.0599564267049857, 77.45874999999999488 ) ) ;
#68980 = VERTEX_POINT ( 'NONE', #36660 ) ;
#68981 = AXIS2_PLACEMENT_3D ( 'NONE', #18668, #70913, #29569 ) ;
#68982 = ORIENTED_EDGE ( 'NONE', *, *, #2004, .T. ) ;
#68983 = CARTESIAN_POINT ( 'NONE',  ( 97.30629616937498838, 90.00000000000002842, 83.13406250086715943 ) ) ;
#68984 = AXIS2_PLACEMENT_3D ( 'NONE', #69234, #28628, #6460 ) ;
#68986 = CARTESIAN_POINT ( 'NONE',  ( 7.103376864691351012E-17, -120.0000000000000000, -64.00000000000000000 ) ) ;
#68985 = AXIS2_PLACEMENT_3D ( 'NONE', #23051, #29396, #12851 ) ;
#68987 = ORIENTED_EDGE ( 'NONE', *, *, #4889, .T. ) ;
#68988 = EDGE_LOOP ( 'NONE', ( #5109, #40624, #58239, #23133 ) ) ;
#68989 = EDGE_CURVE ( 'NONE', #21157, #7122, #19367, .T. ) ;
#68990 = ORIENTED_EDGE ( 'NONE', *, *, #60700, .F. ) ;
#68991 = EDGE_LOOP ( 'NONE', ( #48159, #16239, #22705, #20568 ) ) ;
#68992 = LINE ( 'NONE', #11464, #65873 ) ;
#68993 = VECTOR ( 'NONE', #28526, 1000.000000000000000 ) ;
#68994 = CARTESIAN_POINT ( 'NONE',  ( 0.000000000000000000, 0.000000000000000000, 0.000000000000000000 ) ) ;
#68995 = CARTESIAN_POINT ( 'NONE',  ( -93.67500000000003979, 87.70503267997129626, 87.67166666666666686 ) ) ;
#68996 = CARTESIAN_POINT ( 'NONE',  ( -3.000000000000000000, -25.60904388321916159, -6.976881207771517879 ) ) ;
#68997 = CYLINDRICAL_SURFACE ( 'NONE', #43465, 16.00000000000000000 ) ;
#68998 = CYLINDRICAL_SURFACE ( 'NONE', #3093, 77.49899999999999523 ) ;
#68999 = ADVANCED_FACE ( 'NONE', ( #59604 ), #35186, .F. ) ;
#69000 = DIRECTION ( 'NONE',  ( -1.000000000000000000, 0.000000000000000000, 0.000000000000000000 ) ) ;
#69001 = DIRECTION ( 'NONE',  ( -1.000000000000000000, -0.000000000000000000, 0.000000000000000000 ) ) ;
#69002 = ORIENTED_EDGE ( 'NONE', *, *, #37205, .T. ) ;
#69003 = CARTESIAN_POINT ( 'NONE',  ( -94.99999999999997158, -206.9400435732949575, 82.93562500173429441 ) ) ;
#69004 = ORIENTED_EDGE ( 'NONE', *, *, #28718, .T. ) ;
#69005 = EDGE_CURVE ( 'NONE', #10635, #24265, #58118, .T. ) ;
#69006 = DIRECTION ( 'NONE',  ( 1.000000000000000000, 1.427937372958405461E-15, 7.962523111839130290E-16 ) ) ;
#69007 = AXIS2_PLACEMENT_3D ( 'NONE', #19483, #6740, #36042 ) ;
#69008 = VERTEX_POINT ( 'NONE', #13358 ) ;
#69010 = CARTESIAN_POINT ( 'NONE',  ( -92.35000000000005116, 91.52997821335253548, 79.65479166840096070 ) ) ;
#69009 = CARTESIAN_POINT ( 'NONE',  ( 93.67499999999998295, 92.29496732002878900, 79.81354166840095843 ) ) ;
#69011 =( BOUNDED_CURVE ( )  B_SPLINE_CURVE ( 2, ( #24934, #2049, #36215, #7286, #24572, #69692, #19293 ),
 .UNSPECIFIED., .F., .F. ) 
 B_SPLINE_CURVE_WITH_KNOTS ( ( 3, 2, 2, 3 ),
 ( 0.9166666666666662966, 0.9236111111111108274, 0.9305555555555551361, 0.9374999999999995559 ),
 .UNSPECIFIED. ) 
 CURVE ( )  GEOMETRIC_REPRESENTATION_ITEM ( )  RATIONAL_B_SPLINE_CURVE ( ( 1.000000000000006439, 0.8660254037844322683, 1.000000000000000000, 0.8660254037844387076, 1.000000000000000000, 0.8660254037844472563, 0.9999999999999914513 ) ) 
 REPRESENTATION_ITEM ( '' )  );
#69012 = ORIENTED_EDGE ( 'NONE', *, *, #3954, .T. ) ;
#69013 = CARTESIAN_POINT ( 'NONE',  ( 97.30629616937498838, 90.00000000000002842, 81.22906250086715829 ) ) ;
#69014 = FACE_OUTER_BOUND ( 'NONE', #57008, .T. ) ;
#69015 = DIRECTION ( 'NONE',  ( -1.000000000000000000, 0.000000000000000000, -0.000000000000000000 ) ) ;
#69016 = AXIS2_PLACEMENT_3D ( 'NONE', #1820, #69821, #52917 ) ;
#69017 = DIRECTION ( 'NONE',  ( -0.7071067811865474617, 8.659560562354932858E-17, -0.7071067811865474617 ) ) ;
#69018 = CARTESIAN_POINT ( 'NONE',  ( 10.00000000000000000, 0.000000000000000000, 0.000000000000000000 ) ) ;
#69019 = EDGE_CURVE ( 'NONE', #35261, #50077, #2125, .T. ) ;
#69020 = ORIENTED_EDGE ( 'NONE', *, *, #389, .F. ) ;
#69021 = CARTESIAN_POINT ( 'NONE',  ( -95.00000000000002842, 93.05995642670504253, 80.31624999999999659 ) ) ;
#69022 = CARTESIAN_POINT ( 'NONE',  ( 0.000000000000000000, 2.543863470248399761, 81.96053171279903893 ) ) ;
#69023 = FACE_OUTER_BOUND ( 'NONE', #18687, .T. ) ;
#69024 = VERTEX_POINT ( 'NONE', #53967 ) ;
#69025 = VERTEX_POINT ( 'NONE', #41561 ) ;
#69026 = CYLINDRICAL_SURFACE ( 'NONE', #52847, 2.649999999999985700 ) ;
#69027 = EDGE_CURVE ( 'NONE', #57825, #55546, #2504, .T. ) ;
#69028 = DIRECTION ( 'NONE',  ( 1.000000000000000000, 0.000000000000000000, 0.000000000000000000 ) ) ;
#69029 = DIRECTION ( 'NONE',  ( 1.000000000000000000, 0.000000000000000000, 0.000000000000000000 ) ) ;
#69030 = CARTESIAN_POINT ( 'NONE',  ( -97.30629616937497417, -211.3315407142195852, 79.05947916753382287 ) ) ;
#69031 = EDGE_CURVE ( 'NONE', #27537, #31441, #12251, .T. ) ;
#69032 = VERTEX_POINT ( 'NONE', #41943 ) ;
#69033 = EDGE_CURVE ( 'NONE', #71558, #55701, #17890, .T. ) ;
#69034 = CYLINDRICAL_SURFACE ( 'NONE', #11450, 31.99999999999998579 ) ;
#69035 = EDGE_CURVE ( 'NONE', #54635, #31231, #59231, .T. ) ;
#69036 = AXIS2_PLACEMENT_3D ( 'NONE', #72752, #62633, #44210 ) ;
#69037 = DIRECTION ( 'NONE',  ( 0.000000000000000000, 0.000000000000000000, -1.000000000000000000 ) ) ;
#69038 = PLANE ( 'NONE',  #20126 ) ;
#69039 = CYLINDRICAL_SURFACE ( 'NONE', #63259, 32.00000000000000000 ) ;
#69040 = CARTESIAN_POINT ( 'NONE',  ( -2.500000000000020428, -90.00000000000000000, -310.0000000000000000 ) ) ;
#69041 = CARTESIAN_POINT ( 'NONE',  ( 10.00000000000000000, -46.21855187248673502, 62.20884554314003623 ) ) ;
#69042 = DIRECTION ( 'NONE',  ( -1.000000000000000000, 0.000000000000000000, 0.000000000000000000 ) ) ;
#69043 = CARTESIAN_POINT ( 'NONE',  ( 10.00000000000000000, 33.00180498840072829, -17.80606268964504935 ) ) ;
#69044 = CARTESIAN_POINT ( 'NONE',  ( 0.000000000000000000, -36.13751322684434797, 21.40280677340357940 ) ) ;
#69045 = LINE ( 'NONE', #16802, #2207 ) ;
#69046 = EDGE_CURVE ( 'NONE', #35350, #58563, #46469, .T. ) ;
#69047 = CIRCLE ( 'NONE', #51006, 12.75000000000265565 ) ;
#69048 = AXIS2_PLACEMENT_3D ( 'NONE', #9637, #69908, #72409 ) ;
#69049 = CARTESIAN_POINT ( 'NONE',  ( 97.30629616937498838, 91.33154071421968467, 86.36197916753383197 ) ) ;
#69050 = CARTESIAN_POINT ( 'NONE',  ( -97.30629616937497417, -208.6684592857803295, 89.74864583420048803 ) ) ;
#69051 = DIRECTION ( 'NONE',  ( 1.000000000000000000, -0.000000000000000000, -0.000000000000000000 ) ) ;
#69052 = VERTEX_POINT ( 'NONE', #63776 ) ;
#69053 = CARTESIAN_POINT ( 'NONE',  ( 95.00000000000000000, -213.0599564267049857, 83.25312500173430408 ) ) ;
#69054 = CARTESIAN_POINT ( 'NONE',  ( -95.00000000000002842, 87.33691857156074434, 79.00656250086714749 ) ) ;
#69055 = CONICAL_SURFACE ( 'NONE', #42587, 2.649999999999999467, 1.029744258676654312 ) ;
#69056 = AXIS2_PLACEMENT_3D ( 'NONE', #45087, #9746, #55610 ) ;
#69057 = CARTESIAN_POINT ( 'NONE',  ( 92.69370383062501162, -209.9999999999999716, 89.00781250086714635 ) ) ;
#69058 = ORIENTED_EDGE ( 'NONE', *, *, #16645, .T. ) ;
#69059 = DIRECTION ( 'NONE',  ( -1.000000000000000000, 0.000000000000000000, -0.000000000000000000 ) ) ;
#69060 = PLANE ( 'NONE',  #73183 ) ;
#69061 = DIRECTION ( 'NONE',  ( -1.000000000000000000, -0.000000000000000000, -0.000000000000000000 ) ) ;
#69062 = CIRCLE ( 'NONE', #31788, 12.50000000000000000 ) ;
#69063 = DIRECTION ( 'NONE',  ( -1.000000000000000000, 0.000000000000000000, 0.000000000000000000 ) ) ;
#69064 = CARTESIAN_POINT ( 'NONE',  ( 92.69370383062501162, -208.6684592857803011, 75.14364583420049826 ) ) ;
#69065 = LINE ( 'NONE', #1785, #25829 ) ;
#69066 = ORIENTED_EDGE ( 'NONE', *, *, #12947, .T. ) ;
#69067 = ORIENTED_EDGE ( 'NONE', *, *, #34645, .T. ) ;
#69068 = CARTESIAN_POINT ( 'NONE',  ( 97.30629616937498838, -211.3315407142195852, 80.54114583420049200 ) ) ;
#69069 = DIRECTION ( 'NONE',  ( 0.000000000000000000, 0.000000000000000000, 1.000000000000000000 ) ) ;
#69070 = CARTESIAN_POINT ( 'NONE',  ( 93.67499999999998295, 92.29496732002878900, 81.00416666666666288 ) ) ;
#69071 = CARTESIAN_POINT ( 'NONE',  ( 92.35000000000006537, 91.52997821335256390, 82.96208333333332519 ) ) ;
#69072 = CARTESIAN_POINT ( 'NONE',  ( 0.000000000000000000, 0.000000000000000000, 0.000000000000000000 ) ) ;
#69073 = CARTESIAN_POINT ( 'NONE',  ( 0.000000000000000000, 0.000000000000000000, 0.000000000000000000 ) ) ;
#69074 = CARTESIAN_POINT ( 'NONE',  ( 97.64999999999997726, -211.5299782133524502, 88.35958333333333314 ) ) ;
#69075 = EDGE_CURVE ( 'NONE', #41590, #36758, #52466, .T. ) ;
#69076 = ORIENTED_EDGE ( 'NONE', *, *, #68202, .T. ) ;
#69077 = ORIENTED_EDGE ( 'NONE', *, *, #2107, .F. ) ;
#69078 = VERTEX_POINT ( 'NONE', #46848 ) ;
#69079 = VERTEX_POINT ( 'NONE', #25392 ) ;
#69080 = CARTESIAN_POINT ( 'NONE',  ( 10.00000000000000000, -38.55633173626998911, -16.65560815589452304 ) ) ;
#69081 = AXIS2_PLACEMENT_3D ( 'NONE', #37748, #53550, #9162 ) ;
#69082 = EDGE_CURVE ( 'NONE', #32596, #38564, #37424, .T. ) ;
#69083 = CARTESIAN_POINT ( 'NONE',  ( -96.15314808468751551, 88.00268892867056536, 88.63739583420048973 ) ) ;
#69084 = CARTESIAN_POINT ( 'NONE',  ( 0.000000000000000000, 0.000000000000000000, -6.000000000000000000 ) ) ;
#69085 = ADVANCED_FACE ( 'NONE', ( #20103 ), #71975, .T. ) ;
#69086 = DIRECTION ( 'NONE',  ( 1.000000000000000000, 0.000000000000000000, 0.000000000000000000 ) ) ;
#69087 = CARTESIAN_POINT ( 'NONE',  ( 92.35000000000002274, -211.5299782133524502, 75.52729166840099140 ) ) ;
#69088 = EDGE_CURVE ( 'NONE', #63433, #22473, #20850, .T. ) ;
#69089 = CARTESIAN_POINT ( 'NONE',  ( 93.67499999999999716, 87.70503267997126784, 77.40583333333331950 ) ) ;
#69090 = ORIENTED_EDGE ( 'NONE', *, *, #14868, .T. ) ;
#69091 = LINE ( 'NONE', #28861, #3549 ) ;
#69092 = EDGE_LOOP ( 'NONE', ( #11801, #49203, #4086, #13830 ) ) ;
#69093 = DIRECTION ( 'NONE',  ( -1.000000000000000000, 0.000000000000000000, 0.000000000000000000 ) ) ;
#69094 = ORIENTED_EDGE ( 'NONE', *, *, #58037, .F. ) ;
#69095 = CARTESIAN_POINT ( 'NONE',  ( -97.65000000000001990, 91.52997821335253548, 88.75645833506762017 ) ) ;
#69096 = EDGE_CURVE ( 'NONE', #65189, #46694, #32119, .T. ) ;
#69097 = CARTESIAN_POINT ( 'NONE',  ( -96.15314808468751551, 88.00268892867056536, 80.38239583420048007 ) ) ;
#69098 = CIRCLE ( 'NONE', #1877, 42.00000000000000000 ) ;
#69099 = CARTESIAN_POINT ( 'NONE',  ( 94.99999999999998579, 92.66308142843935514, 89.00781250086716057 ) ) ;
#69100 = AXIS2_PLACEMENT_3D ( 'NONE', #52080, #12226, #64854 ) ;
#69101 = ORIENTED_EDGE ( 'NONE', *, *, #37594, .T. ) ;
#69102 = CARTESIAN_POINT ( 'NONE',  ( 3.000000000000000000, 0.000000000000000000, 0.000000000000000000 ) ) ;
#69103 = CARTESIAN_POINT ( 'NONE',  ( 10.00000000000000000, 0.000000000000000000, 0.000000000000000000 ) ) ;
#69104 = CARTESIAN_POINT ( 'NONE',  ( 97.64999999999999147, -209.9999999999999716, 85.87249999999998806 ) ) ;
#69105 = ADVANCED_FACE ( 'NONE', ( #14090 ), #49783, .F. ) ;
#69106 = DIRECTION ( 'NONE',  ( 0.000000000000000000, 0.7071067811865486830, -0.7071067811865464625 ) ) ;
#69107 = ORIENTED_EDGE ( 'NONE', *, *, #70158, .F. ) ;
#69108 = LINE ( 'NONE', #64208, #29099 ) ;
#69109 = VECTOR ( 'NONE', #35651, 999.9999999999998863 ) ;
#69110 = CARTESIAN_POINT ( 'NONE',  ( -92.69370383062498320, -209.9999999999999716, 77.26031250086714408 ) ) ;
#69111 = ORIENTED_EDGE ( 'NONE', *, *, #37255, .F. ) ;
#69112 = ORIENTED_EDGE ( 'NONE', *, *, #28091, .F. ) ;
#69114 = DIRECTION ( 'NONE',  ( 0.000000000000000000, -1.000000000000000000, 0.000000000000000000 ) ) ;
#69113 = CONICAL_SURFACE ( 'NONE', #61922, 14.53333333333331545, 0.3490658503988688377 ) ;
#69115 = ORIENTED_EDGE ( 'NONE', *, *, #9141, .F. ) ;
#69116 = DIRECTION ( 'NONE',  ( 1.427937372958396981E-15, -1.000000000000000000, 1.065814103640131031E-14 ) ) ;
#69117 = AXIS2_PLACEMENT_3D ( 'NONE', #69293, #63670, #19260 ) ;
#69118 = CARTESIAN_POINT ( 'NONE',  ( 92.34999999999999432, 90.00000000000002842, 80.47499999999999432 ) ) ;
#69119 = ORIENTED_EDGE ( 'NONE', *, *, #60385, .T. ) ;
#69120 = CARTESIAN_POINT ( 'NONE',  ( -96.15314808468747287, -208.0026889286704943, 75.56697916753381605 ) ) ;
#69121 = ORIENTED_EDGE ( 'NONE', *, *, #40070, .F. ) ;
#69122 = CARTESIAN_POINT ( 'NONE',  ( -92.35000000000005116, 88.47002178664754979, 76.92958333333332632 ) ) ;
#69123 = DIRECTION ( 'NONE',  ( 1.000000000000000000, -0.000000000000000000, 0.000000000000000000 ) ) ;
#69124 = EDGE_CURVE ( 'NONE', #65810, #25170, #17682, .T. ) ;
#69125 = VERTEX_POINT ( 'NONE', #72352 ) ;
#69126 = AXIS2_PLACEMENT_3D ( 'NONE', #35445, #57653, #64032 ) ;
#69127 = EDGE_LOOP ( 'NONE', ( #149, #59399 ) ) ;
#69128 = CARTESIAN_POINT ( 'NONE',  ( -10.00000000000000000, 0.000000000000000000, 0.000000000000000000 ) ) ;
#69129 = EDGE_CURVE ( 'NONE', #1781, #48167, #44158, .T. ) ;
#69130 = EDGE_CURVE ( 'NONE', #30791, #26258, #37038, .T. ) ;
#69131 = AXIS2_PLACEMENT_3D ( 'NONE', #71533, #73755, #28635 ) ;
#69132 = CARTESIAN_POINT ( 'NONE',  ( 97.64999999999324132, -209.9999940177821713, 82.14187520865721126 ) ) ;
#69133 = CARTESIAN_POINT ( 'NONE',  ( 92.69370383062498320, 90.00000000000002842, 86.46781250086714010 ) ) ;
#69134 = CYLINDRICAL_SURFACE ( 'NONE', #58044, 31.99999999999998579 ) ;
#69135 = CARTESIAN_POINT ( 'NONE',  ( 10.00000000000000000, -8.840884882374576037, -74.65374052328658649 ) ) ;
#69136 = DIRECTION ( 'NONE',  ( -1.000000000000000000, 3.061616997868382648E-16, 0.000000000000000000 ) ) ;
#69137 = CYLINDRICAL_SURFACE ( 'NONE', #26791, 2.650000000000540812 ) ;
#69138 = DIRECTION ( 'NONE',  ( 0.000000000000000000, -0.3090169943749548898, 0.9510565162951511997 ) ) ;
#69139 = CARTESIAN_POINT ( 'NONE',  ( -92.35000000000005116, 91.52997821335253548, 84.09979166840098230 ) ) ;
#69140 = DIRECTION ( 'NONE',  ( 1.000000000000000000, 0.000000000000000000, 0.000000000000000000 ) ) ;
#69141 = EDGE_CURVE ( 'NONE', #3975, #29598, #51319, .T. ) ;
#69142 = FACE_OUTER_BOUND ( 'NONE', #53691, .T. ) ;
#69143 = CARTESIAN_POINT ( 'NONE',  ( -3.000000000000000000, -22.32062822937489344, 14.36278369418800160 ) ) ;
#69144 = CARTESIAN_POINT ( 'NONE',  ( 10.00000000000000000, -35.38097989696520074, 12.42422080174625520 ) ) ;
#69145 = CARTESIAN_POINT ( 'NONE',  ( 0.000000000000000000, 5.835314593368772229, -22.81335362449846826 ) ) ;
#69146 = CARTESIAN_POINT ( 'NONE',  ( 0.000000000000000000, 20.41045688087930898, -72.35160999960793049 ) ) ;
#69147 = VERTEX_POINT ( 'NONE', #59988 ) ;
#69148 = LINE ( 'NONE', #16156, #13123 ) ;
#69149 = AXIS2_PLACEMENT_3D ( 'NONE', #24899, #47827, #70748 ) ;
#69150 = CARTESIAN_POINT ( 'NONE',  ( 5.822613034544236399, -142.8165987265839760, 5.500000000000000000 ) ) ;
#69151 = CARTESIAN_POINT ( 'NONE',  ( 10.00000000000000000, 75.11725578898467859, 2.956366410620910656 ) ) ;
#69152 = DIRECTION ( 'NONE',  ( -1.000000000000000000, 7.619177619974977057E-15, 2.612289469705706555E-14 ) ) ;
#69153 = CARTESIAN_POINT ( 'NONE',  ( 2.750000000000000000, 3.306546357697853240E-16, -2.699999999999999734 ) ) ;
#69154 = VECTOR ( 'NONE', #55855, 1000.000000000000000 ) ;
#69155 = CARTESIAN_POINT ( 'NONE',  ( 93.84685191531249870, -208.0026889286704943, 87.15572916753382060 ) ) ;
#69156 = AXIS2_PLACEMENT_3D ( 'NONE', #55550, #20961, #49529 ) ;
#69157 = ORIENTED_EDGE ( 'NONE', *, *, #8088, .F. ) ;
#69158 = VERTEX_POINT ( 'NONE', #38520 ) ;
#69159 = EDGE_LOOP ( 'NONE', ( #2243, #8706, #4742, #24623 ) ) ;
#69160 = AXIS2_PLACEMENT_3D ( 'NONE', #27590, #34341, #21192 ) ;
#69161 = LINE ( 'NONE', #68043, #7760 ) ;
#69162 = AXIS2_PLACEMENT_3D ( 'NONE', #42122, #65057, #41014 ) ;
#69163 = CARTESIAN_POINT ( 'NONE',  ( 6.000000000000000000, 16.65972982745045528, -80.28980883073738539 ) ) ;
#69164 = ORIENTED_EDGE ( 'NONE', *, *, #32684, .T. ) ;
#69165 = CARTESIAN_POINT ( 'NONE',  ( 97.30629616937498838, -211.3315407142195852, 82.44614583420049314 ) ) ;
#69166 = VERTEX_POINT ( 'NONE', #67083 ) ;
#69167 = DIRECTION ( 'NONE',  ( -1.000000000000000000, 0.000000000000000000, 0.000000000000000000 ) ) ;
#69168 = ORIENTED_EDGE ( 'NONE', *, *, #54273, .T. ) ;
#69169 = ORIENTED_EDGE ( 'NONE', *, *, #673, .T. ) ;
#69170 = DIRECTION ( 'NONE',  ( -0.000000000000000000, -0.000000000000000000, -1.000000000000000000 ) ) ;
#69171 = UNCERTAINTY_MEASURE_WITH_UNIT (LENGTH_MEASURE( 1.000000000000000082E-05 ), #57953, 'distance_accuracy_value', 'NONE');
#69172 = ADVANCED_FACE ( 'NONE', ( #21206 ), #71229, .F. ) ;
#69173 = CARTESIAN_POINT ( 'NONE',  ( 0.000000000000000000, -75.54627589209931671, -17.28742895386162814 ) ) ;
#69174 = ORIENTED_EDGE ( 'NONE', *, *, #50045, .F. ) ;
#69175 = DIRECTION ( 'NONE',  ( -0.000000000000000000, -0.000000000000000000, 1.000000000000000000 ) ) ;
#69176 = CARTESIAN_POINT ( 'NONE',  ( 92.35000000000002274, -211.5299782133524502, 88.22729166840096582 ) ) ;
#69177 = EDGE_CURVE ( 'NONE', #2347, #60338, #63319, .T. ) ;
#69178 = EDGE_CURVE ( 'NONE', #73599, #7335, #27267, .T. ) ;
#69179 = EDGE_LOOP ( 'NONE', ( #64951, #42701, #58062, #47976 ) ) ;
#69180 = DIRECTION ( 'NONE',  ( 0.000000000000000000, 0.000000000000000000, 1.000000000000000000 ) ) ;
#69181 = VERTEX_POINT ( 'NONE', #14841 ) ;
#69182 = CARTESIAN_POINT ( 'NONE',  ( 5.000000000000000888, -1.831125658499874742, -1.158123955083391943 ) ) ;
#69183 = ORIENTED_EDGE ( 'NONE', *, *, #66822, .F. ) ;
#69184 = ORIENTED_EDGE ( 'NONE', *, *, #72567, .F. ) ;
#69185 = ORIENTED_EDGE ( 'NONE', *, *, #54649, .F. ) ;
#69186 = LINE ( 'NONE', #39880, #74122 ) ;
#69187 = DIRECTION ( 'NONE',  ( 0.000000000000000000, -0.9969173337331270757, -0.07845909572785580988 ) ) ;
#69188 = VERTEX_POINT ( 'NONE', #43444 ) ;
#69189 = VERTEX_POINT ( 'NONE', #37788 ) ;
#69190 = ORIENTED_EDGE ( 'NONE', *, *, #69867, .T. ) ;
#69191 = CARTESIAN_POINT ( 'NONE',  ( 97.64999999999999147, -209.9999999999999716, 76.34749999999999659 ) ) ;
#69192 = CARTESIAN_POINT ( 'NONE',  ( 4.999999999999999112, -3.925862922256468046, 41.81611651403860463 ) ) ;
#69193 = ADVANCED_FACE ( 'NONE', ( #31383 ), #48684, .F. ) ;
#69194 = CARTESIAN_POINT ( 'NONE',  ( -95.00000000000002842, 93.05995642670501411, 87.93625000000000114 ) ) ;
#69195 = ORIENTED_EDGE ( 'NONE', *, *, #58805, .T. ) ;
#69196 = CARTESIAN_POINT ( 'NONE',  ( 97.30629616937498838, 88.66845928578037217, 75.30239583420048177 ) ) ;
#69197 = VERTEX_POINT ( 'NONE', #2860 ) ;
#69198 = CARTESIAN_POINT ( 'NONE',  ( 0.000000000000000000, 0.000000000000000000, 0.000000000000000000 ) ) ;
#69199 = CARTESIAN_POINT ( 'NONE',  ( -93.84685191531248449, -208.0026889286704943, 85.62114583420046188 ) ) ;
#69200 = ORIENTED_EDGE ( 'NONE', *, *, #51278, .F. ) ;
#69201 = DIRECTION ( 'NONE',  ( -1.000000000000000000, 0.000000000000000000, 0.000000000000000000 ) ) ;
#69202 = DIRECTION ( 'NONE',  ( -1.000000000000000000, -0.000000000000000000, 0.000000000000000000 ) ) ;
#69203 = DIRECTION ( 'NONE',  ( 0.000000000000000000, 0.000000000000000000, 1.000000000000000000 ) ) ;
#69204 = DIRECTION ( 'NONE',  ( 0.000000000000000000, 0.9876883405951372152, 0.1564344650402346160 ) ) ;
#69205 = LINE ( 'NONE', #94, #299 ) ;
#69206 = DIRECTION ( 'NONE',  ( 0.000000000000000000, 0.000000000000000000, -1.000000000000000000 ) ) ;
#69207 = ADVANCED_FACE ( 'NONE', ( #25754 ), #43060, .T. ) ;
#69208 = EDGE_CURVE ( 'NONE', #35339, #72850, #74127, .T. ) ;
#69209 = AXIS2_PLACEMENT_3D ( 'NONE', #30882, #19608, #25627 ) ;
#69210 = DIRECTION ( 'NONE',  ( -1.000000000000000000, 0.000000000000000000, 0.000000000000000000 ) ) ;
#69211 = CIRCLE ( 'NONE', #18796, 31.99999999999998224 ) ;
#69212 = DIRECTION ( 'NONE',  ( -1.000000000000000000, 0.000000000000000000, 0.000000000000000000 ) ) ;
#69213 = CARTESIAN_POINT ( 'NONE',  ( 1.560000000000000053, 1.732050807568878747, 7.017607234860990640E-28 ) ) ;
#69214 = CARTESIAN_POINT ( 'NONE',  ( -95.00000000000002842, 87.33691857156074434, 79.64156250086713840 ) ) ;
#69215 = DIRECTION ( 'NONE',  ( 0.000000000000000000, 0.9969173337331276308, 0.07845909572784864894 ) ) ;
#69216 = CARTESIAN_POINT ( 'NONE',  ( 11.99999999999999822, -72.35160999960831418, 20.41045688087797672 ) ) ;
#69217 = AXIS2_PLACEMENT_3D ( 'NONE', #42578, #65517, #13989 ) ;
#69218 = AXIS2_PLACEMENT_3D ( 'NONE', #70289, #23351, #1201 ) ;
#69219 =( BOUNDED_CURVE ( )  B_SPLINE_CURVE ( 2, ( #26318, #19933, #14668, #54527, #30838, #59807, #66555 ),
 .UNSPECIFIED., .F., .F. ) 
 B_SPLINE_CURVE_WITH_KNOTS ( ( 3, 2, 2, 3 ),
 ( 0.5080151867253829279, 0.5150708844844119616, 0.5221266500252946807, 0.5291824299508934848 ),
 .UNSPECIFIED. ) 
 CURVE ( )  GEOMETRIC_REPRESENTATION_ITEM ( )  RATIONAL_B_SPLINE_CURVE ( ( 0.9999974259464248227, 0.8660266908235904060, 1.000000000000000000, 0.8660254037844387076, 1.000000000000000000, 0.8660254037844387076, 1.000000000000000000 ) ) 
 REPRESENTATION_ITEM ( '' )  );
#69220 = ORIENTED_EDGE ( 'NONE', *, *, #44849, .F. ) ;
#69221 = CARTESIAN_POINT ( 'NONE',  ( -94.99999999999997158, -206.9400435732949575, 80.39562500173430237 ) ) ;
#69222 = LINE ( 'NONE', #48866, #10055 ) ;
#69223 = CARTESIAN_POINT ( 'NONE',  ( 10.00000000000000000, -72.35432306680498016, 20.40083707022857951 ) ) ;
#69224 = FACE_OUTER_BOUND ( 'NONE', #53296, .T. ) ;
#69225 = LINE ( 'NONE', #12074, #32147 ) ;
#69226 = CIRCLE ( 'NONE', #60844, 77.49900000000000944 ) ;
#69227 = DIRECTION ( 'NONE',  ( -0.000000000000000000, -0.000000000000000000, -1.000000000000000000 ) ) ;
#69228 = CARTESIAN_POINT ( 'NONE',  ( -94.99999999999997158, -212.6630814284392557, 75.99031250086716227 ) ) ;
#69229 = CARTESIAN_POINT ( 'NONE',  ( 6.782329983125267248, 10.49999999999999645, -105.0000000000000000 ) ) ;
#69230 = ORIENTED_EDGE ( 'NONE', *, *, #35034, .T. ) ;
#69231 = DIRECTION ( 'NONE',  ( 0.000000000000000000, -0.7071067811865536790, 0.7071067811865414665 ) ) ;
#69232 = CARTESIAN_POINT ( 'NONE',  ( 10.00000000000000000, 41.81611651403861885, 3.925862922256313503 ) ) ;
#69233 = PLANE ( 'NONE',  #39455 ) ;
#69234 = CARTESIAN_POINT ( 'NONE',  ( 95.00000000002596323, -209.9999999999999147, -74.99999999999349143 ) ) ;
#69235 = CYLINDRICAL_SURFACE ( 'NONE', #3162, 2.649999999999985700 ) ;
#69236 = ORIENTED_EDGE ( 'NONE', *, *, #31323, .F. ) ;
#69237 = PLANE ( 'NONE',  #19245 ) ;
#69238 = CARTESIAN_POINT ( 'NONE',  ( 0.000000000000000000, 33.17418723428307459, 17.67226234102837878 ) ) ;
#69239 = ORIENTED_EDGE ( 'NONE', *, *, #51187, .F. ) ;
#69240 = CARTESIAN_POINT ( 'NONE',  ( 92.69370383062501162, -209.9999999999999716, 85.83281250086714920 ) ) ;
#69241 = CARTESIAN_POINT ( 'NONE',  ( 11.99999999999999822, 18.89407956138257205, 75.16055320797038064 ) ) ;
#69242 = ORIENTED_EDGE ( 'NONE', *, *, #23834, .T. ) ;
#69243 = ADVANCED_FACE ( 'NONE', ( #5070 ), #39268, .T. ) ;
#69244 = DIRECTION ( 'NONE',  ( -1.000000000000000000, 0.000000000000000000, 0.000000000000000000 ) ) ;
#69245 = CIRCLE ( 'NONE', #46448, 16.00000000000000000 ) ;
#69246 = VERTEX_POINT ( 'NONE', #27969 ) ;
#69247 = CARTESIAN_POINT ( 'NONE',  ( 97.64999999999990621, -209.9999992849081139, 85.31687502647973531 ) ) ;
#69248 = ORIENTED_EDGE ( 'NONE', *, *, #3499, .F. ) ;
#69249 = CARTESIAN_POINT ( 'NONE',  ( -97.30629616937501680, 88.66845928578038638, 80.32947916753381890 ) ) ;
#69250 = VERTEX_POINT ( 'NONE', #68589 ) ;
#69251 = AXIS2_PLACEMENT_3D ( 'NONE', #56910, #40720, #63665 ) ;
#69252 = ADVANCED_FACE ( 'NONE', ( #74208 ), #51273, .T. ) ;
#69253 = DIRECTION ( 'NONE',  ( -1.000000000000000000, 0.000000000000000000, 0.000000000000000000 ) ) ;
#69254 = ORIENTED_EDGE ( 'NONE', *, *, #27061, .F. ) ;
#69255 = VECTOR ( 'NONE', #40803, 1000.000000000000227 ) ;
#69256 = EDGE_LOOP ( 'NONE', ( #31809, #17392, #32967, #64826 ) ) ;
#69257 = CARTESIAN_POINT ( 'NONE',  ( -3.000000000000000000, 23.50000000000000000, -1.500000000000001332 ) ) ;
#69258 = EDGE_CURVE ( 'NONE', #47069, #2989, #2153, .T. ) ;
#69259 = ORIENTED_EDGE ( 'NONE', *, *, #9260, .F. ) ;
#69260 = PRODUCT_DEFINITION_SHAPE ( 'NONE', 'NONE',  #74357 ) ;
#69261 = AXIS2_PLACEMENT_3D ( 'NONE', #74014, #41295, #29255 ) ;
#69262 = ORIENTED_EDGE ( 'NONE', *, *, #6539, .F. ) ;
#69263 = CARTESIAN_POINT ( 'NONE',  ( 0.000000000000000000, 73.73191006444572793, -14.66109333815486515 ) ) ;
#69264 = ADVANCED_FACE ( 'NONE', ( #17075 ), #62966, .F. ) ;
#69265 = VECTOR ( 'NONE', #33426, 1000.000000000000000 ) ;
#69266 = ORIENTED_EDGE ( 'NONE', *, *, #15067, .F. ) ;
#69267 = VERTEX_POINT ( 'NONE', #23094 ) ;
#69268 = CARTESIAN_POINT ( 'NONE',  ( 97.30629616937498838, 88.66845928578037217, 86.09739583420048348 ) ) ;
#69269 = ORIENTED_EDGE ( 'NONE', *, *, #69031, .T. ) ;
#69270 = CARTESIAN_POINT ( 'NONE',  ( 95.00000000000000000, -212.6630814284392557, 82.81656250086713555 ) ) ;
#69271 = FACE_OUTER_BOUND ( 'NONE', #68433, .T. ) ;
#69272 = AXIS2_PLACEMENT_3D ( 'NONE', #50649, #45407, #10430 ) ;
#69273 = DIRECTION ( 'NONE',  ( 0.000000000000000000, -0.9238795325112821866, -0.3826834323651006065 ) ) ;
#69274 = CARTESIAN_POINT ( 'NONE',  ( 15.50000000000000000, 0.000000000000000000, -4.400000000000001243 ) ) ;
#69275 = CARTESIAN_POINT ( 'NONE',  ( 10.00000000000000000, -17.80606268964563554, 33.00180498840040855 ) ) ;
#69276 = CARTESIAN_POINT ( 'NONE',  ( -10.00000000000000000, 0.000000000000000000, 0.000000000000000000 ) ) ;
#69277 = CARTESIAN_POINT ( 'NONE',  ( -3.000000000000000000, -23.29833615347104825, -3.418703333116803744 ) ) ;
#69278 = CARTESIAN_POINT ( 'NONE',  ( -94.99999999999997158, -212.6630814284392557, 82.81656250086713555 ) ) ;
#69279 = ADVANCED_FACE ( 'NONE', ( #34352 ), #4326, .F. ) ;
#69280 = AXIS2_PLACEMENT_3D ( 'NONE', #24854, #1968, #18472 ) ;
#69281 = CARTESIAN_POINT ( 'NONE',  ( -97.30629616937501680, 91.33154071421968467, 82.76364583420048859 ) ) ;
#69282 = ADVANCED_FACE ( 'NONE', ( #11420 ), #21964, .T. ) ;
#69283 = ORIENTED_EDGE ( 'NONE', *, *, #4156, .T. ) ;
#69284 = CARTESIAN_POINT ( 'NONE',  ( 96.15314808468748708, 88.00268892867053694, 83.50447916753381605 ) ) ;
#69285 = ORIENTED_EDGE ( 'NONE', *, *, #39482, .F. ) ;
#69286 = CARTESIAN_POINT ( 'NONE',  ( -96.32500000000001705, 87.70503267997129626, 78.75520833506763552 ) ) ;
#69287 = LINE ( 'NONE', #35795, #32577 ) ;
#69288 = DIRECTION ( 'NONE',  ( -0.000000000000000000, -0.000000000000000000, 1.000000000000000000 ) ) ;
#69289 = CARTESIAN_POINT ( 'NONE',  ( 10.00000000000000000, -41.81611651403864727, 3.925862922256025289 ) ) ;
#69290 = CARTESIAN_POINT ( 'NONE',  ( -93.84685191531247028, -211.9973110713294489, 86.04447916753380809 ) ) ;
#69291 = CARTESIAN_POINT ( 'NONE',  ( 10.00000000000000178, 0.000000000000000000, 0.000000000000000000 ) ) ;
#69292 = CARTESIAN_POINT ( 'NONE',  ( 10.00000000000000000, -27.05870788708213226, -26.08949754953053102 ) ) ;
#69293 = CARTESIAN_POINT ( 'NONE',  ( 11.99999999999999822, -8.840884882374576037, -74.65374052328658649 ) ) ;
#69294 = DIRECTION ( 'NONE',  ( 0.000000000000000000, 0.000000000000000000, 1.000000000000000000 ) ) ;
#69295 = ORIENTED_EDGE ( 'NONE', *, *, #2417, .F. ) ;
#69296 = EDGE_LOOP ( 'NONE', ( #21469, #67786, #60297, #53716 ) ) ;
#69297 = CARTESIAN_POINT ( 'NONE',  ( -92.35000000000003695, 90.00000000000004263, 76.34749999999999659 ) ) ;
#69298 = DIRECTION ( 'NONE',  ( -1.000000000000000000, 0.000000000000000000, 0.000000000000000000 ) ) ;
#69299 = CARTESIAN_POINT ( 'NONE',  ( -94.00680085345840098, -207.8660161998918170, 74.81432998548487490 ) ) ;
#69300 = CARTESIAN_POINT ( 'NONE',  ( 15.00000000000000000, -10.45096189432344502, -21.10159698893425784 ) ) ;
#69301 = CARTESIAN_POINT ( 'NONE',  ( 10.00000000000000000, 33.00180498840072829, -17.80606268964504935 ) ) ;
#69302 = DIRECTION ( 'NONE',  ( -1.000000000000000000, 0.000000000000000000, -0.000000000000000000 ) ) ;
#69303 = VECTOR ( 'NONE', #72867, 1000.000000000000114 ) ;
#69304 = ORIENTED_EDGE ( 'NONE', *, *, #12889, .T. ) ;
#69305 = CARTESIAN_POINT ( 'NONE',  ( -97.30629616937501680, 91.33154071421968467, 80.06489583420047040 ) ) ;
#69306 = VECTOR ( 'NONE', #52622, 1000.000000000000000 ) ;
#69307 = CARTESIAN_POINT ( 'NONE',  ( 15.00000000000000000, 0.000000000000000000, 0.000000000000000000 ) ) ;
#69308 = DIRECTION ( 'NONE',  ( -1.000000000000000000, -0.000000000000000000, 0.000000000000000000 ) ) ;
#69309 = CARTESIAN_POINT ( 'NONE',  ( 0.000000000000000000, 0.000000000000000000, 0.000000000000000000 ) ) ;
#69310 = VECTOR ( 'NONE', #49304, 1000.000000000000000 ) ;
#69311 = LINE ( 'NONE', #17797, #50071 ) ;
#69312 = DIRECTION ( 'NONE',  ( -1.000000000000000000, -0.000000000000000000, -0.000000000000000000 ) ) ;
#69313 = CARTESIAN_POINT ( 'NONE',  ( -94.99999999999997158, -207.3369185715606307, 85.19781250086714408 ) ) ;
#69314 = AXIS2_PLACEMENT_3D ( 'NONE', #57296, #10684, #5807 ) ;
#69315 = CARTESIAN_POINT ( 'NONE',  ( 93.84685191531248449, 91.99731107132950569, 76.36072916753381890 ) ) ;
#69316 = EDGE_CURVE ( 'NONE', #69892, #50077, #62120, .T. ) ;
#69317 = CARTESIAN_POINT ( 'NONE',  ( -92.69370383062498320, -209.9999999999999716, 80.59406250086715318 ) ) ;
#69318 = DIRECTION ( 'NONE',  ( -1.000000000000000000, -1.427937372958405461E-15, -7.962523111839130290E-16 ) ) ;
#69319 = ORIENTED_EDGE ( 'NONE', *, *, #34922, .F. ) ;
#69320 = CARTESIAN_POINT ( 'NONE',  ( -95.00000000000002842, 93.05995642670504253, 82.93562500173430863 ) ) ;
#69321 = CARTESIAN_POINT ( 'NONE',  ( -94.99999999999997158, -206.9400435732949575, 75.23624999999999829 ) ) ;
#69322 = DIRECTION ( 'NONE',  ( -1.000000000000000000, 0.000000000000000000, -0.000000000000000000 ) ) ;
#69323 = EDGE_CURVE ( 'NONE', #35960, #73028, #45334, .T. ) ;
#69324 = CARTESIAN_POINT ( 'NONE',  ( -97.30629616937501680, 91.33154071421968467, 75.77864583420048916 ) ) ;
#69325 = CARTESIAN_POINT ( 'NONE',  ( 97.30629616937498838, -209.9999999999999716, 78.53031250086714010 ) ) ;
#69326 = ORIENTED_EDGE ( 'NONE', *, *, #27418, .F. ) ;
#69328 = EDGE_CURVE ( 'NONE', #61245, #52121, #11778, .T. ) ;
#69327 = CIRCLE ( 'NONE', #70486, 12.50000000000022560 ) ;
#69329 = CARTESIAN_POINT ( 'NONE',  ( -97.64999999999994884, 91.52997821335257811, 75.34208333333333485 ) ) ;
#69330 = VERTEX_POINT ( 'NONE', #68953 ) ;
#69331 = CARTESIAN_POINT ( 'NONE',  ( -93.67499999999998295, -207.7050326799711968, 87.96270833506763154 ) ) ;
#69332 = VERTEX_POINT ( 'NONE', #34728 ) ;
#69333 = EDGE_CURVE ( 'NONE', #11928, #72369, #44143, .T. ) ;
#69334 = CARTESIAN_POINT ( 'NONE',  ( -93.67500000000003979, 92.29496732002878900, 79.07270833506763097 ) ) ;
#69335 = ORIENTED_EDGE ( 'NONE', *, *, #59107, .F. ) ;
#69336 = ORIENTED_EDGE ( 'NONE', *, *, #35816, .F. ) ;
#69337 = ORIENTED_EDGE ( 'NONE', *, *, #34189, .F. ) ;
#69338 = CARTESIAN_POINT ( 'NONE',  ( 0.000000000000000000, 73.72996012237440766, 14.67089635893739619 ) ) ;
#69339 = ORIENTED_EDGE ( 'NONE', *, *, #8199, .F. ) ;
#69340 = EDGE_LOOP ( 'NONE', ( #56562, #35520, #63161, #53641 ) ) ;
#69341 = CARTESIAN_POINT ( 'NONE',  ( 92.69370383062498320, 90.00000000000002842, 83.45156250086715488 ) ) ;
#69342 = ADVANCED_FACE ( 'NONE', ( #27216 ), #5439, .T. ) ;
#69343 = VECTOR ( 'NONE', #64959, 1000.000000000000000 ) ;
#69344 = LINE ( 'NONE', #58815, #3298 ) ;
#69345 = AXIS2_PLACEMENT_3D ( 'NONE', #6705, #19454, #29610 ) ;
#69346 = ORIENTED_EDGE ( 'NONE', *, *, #64751, .T. ) ;
#69347 = ORIENTED_EDGE ( 'NONE', *, *, #34921, .T. ) ;
#69348 = ORIENTED_EDGE ( 'NONE', *, *, #52362, .T. ) ;
#69349 = ORIENTED_EDGE ( 'NONE', *, *, #31789, .T. ) ;
#69350 = CARTESIAN_POINT ( 'NONE',  ( 10.00000000000000000, 37.16516213103285082, -4.992566952384588141 ) ) ;
#69351 = DIRECTION ( 'NONE',  ( 0.000000000000000000, 0.000000000000000000, 1.000000000000000000 ) ) ;
#69352 = CARTESIAN_POINT ( 'NONE',  ( 11.99999999999999822, -67.80270845531921964, 46.11716303203162681 ) ) ;
#69353 = AXIS2_PLACEMENT_3D ( 'NONE', #5609, #41551, #16499 ) ;
#69354 = FACE_OUTER_BOUND ( 'NONE', #5542, .T. ) ;
#69355 = CARTESIAN_POINT ( 'NONE',  ( 10.00000000000000000, -40.68715046381921496, -10.41901085202121457 ) ) ;
#69356 = AXIS2_PLACEMENT_3D ( 'NONE', #72984, #38797, #61736 ) ;
#69357 = CARTESIAN_POINT ( 'NONE',  ( 97.64999999954044085, -209.9999506483753180, 87.22187670868780174 ) ) ;
#69358 = FACE_OUTER_BOUND ( 'NONE', #45120, .T. ) ;
#69359 = CARTESIAN_POINT ( 'NONE',  ( 12.00000000000000000, 16.61724383029390140, 20.69703378468902955 ) ) ;
#69360 = ORIENTED_EDGE ( 'NONE', *, *, #65216, .T. ) ;
#69361 = CARTESIAN_POINT ( 'NONE',  ( -93.67499999999998295, -212.2949673200287179, 80.76604166840097321 ) ) ;
#69363 = ORIENTED_EDGE ( 'NONE', *, *, #25152, .T. ) ;
#69362 = EDGE_CURVE ( 'NONE', #13090, #15642, #56180, .T. ) ;
#69364 = FACE_OUTER_BOUND ( 'NONE', #45369, .T. ) ;
#69365 = EDGE_CURVE ( 'NONE', #1061, #25431, #38893, .T. ) ;
#69366 = EDGE_LOOP ( 'NONE', ( #20229, #27555, #45803, #69713 ) ) ;
#69368 = CARTESIAN_POINT ( 'NONE',  ( -95.00000000000002842, 86.94004357329504273, 78.80812500173429669 ) ) ;
#69367 = CARTESIAN_POINT ( 'NONE',  ( 92.34999999999999432, 88.47002178664753558, 79.97229166840095615 ) ) ;
#69370 = EDGE_CURVE ( 'NONE', #72558, #72136, #10314, .T. ) ;
#69369 = EDGE_LOOP ( 'NONE', ( #39770, #68379, #33470, #33542 ) ) ;
#69371 = CARTESIAN_POINT ( 'NONE',  ( 96.15314808468748708, 88.00268892867053694, 80.48822916753381662 ) ) ;
#69372 = CARTESIAN_POINT ( 'NONE',  ( -92.34999999999999432, -209.9999999999999716, 82.06250000000000000 ) ) ;
#69373 = CARTESIAN_POINT ( 'NONE',  ( 10.00000000000000000, 27.05870788708231700, 26.08949754953034272 ) ) ;
#69374 = CARTESIAN_POINT ( 'NONE',  ( 5.000000000000000000, -22.48208911017525580, 35.47612816024516036 ) ) ;
#69375 = DIRECTION ( 'NONE',  ( -1.000000000000000000, -0.000000000000000000, -0.000000000000000000 ) ) ;
#69376 = ORIENTED_EDGE ( 'NONE', *, *, #2865, .T. ) ;
#69377 = CARTESIAN_POINT ( 'NONE',  ( 0.000000000000000000, 31.46837873495072913, -68.27212725128242710 ) ) ;
#69378 = CYLINDRICAL_SURFACE ( 'NONE', #57632, 77.49899999999999523 ) ;
#69379 = ORIENTED_EDGE ( 'NONE', *, *, #53507, .T. ) ;
#69380 = CIRCLE ( 'NONE', #28574, 77.49899999999999523 ) ;
#69381 = ORIENTED_EDGE ( 'NONE', *, *, #54846, .T. ) ;
#69382 = AXIS2_PLACEMENT_3D ( 'NONE', #31989, #10843, #37654 ) ;
#69383 = AXIS2_PLACEMENT_3D ( 'NONE', #50931, #22367, #50175 ) ;
#69384 = DIRECTION ( 'NONE',  ( -1.000000000000000000, 0.000000000000000000, 0.000000000000000000 ) ) ;
#69385 = CYLINDRICAL_SURFACE ( 'NONE', #45055, 16.00000000000000000 ) ;
#69386 = DIRECTION ( 'NONE',  ( 0.000000000000000000, 0.000000000000000000, -1.000000000000000000 ) ) ;
#69387 = CARTESIAN_POINT ( 'NONE',  ( -92.69370383062498320, -209.9999999999999716, 76.14906250086716000 ) ) ;
#69388 = AXIS2_PLACEMENT_3D ( 'NONE', #26767, #20021, #54260 ) ;
#69389 = VERTEX_POINT ( 'NONE', #73458 ) ;
#69390 = DIRECTION ( 'NONE',  ( 0.000000000000000000, 0.000000000000000000, 1.000000000000000000 ) ) ;
#69391 = DIRECTION ( 'NONE',  ( 0.000000000000000000, -0.8910065241883626808, -0.4539904997395569075 ) ) ;
#69392 = CARTESIAN_POINT ( 'NONE',  ( 97.64999999999999147, -209.9999999999999716, 90.00000000000000000 ) ) ;
#69393 = CARTESIAN_POINT ( 'NONE',  ( 0.000000000000000000, 70.53064760720278059, 26.01480285779964774 ) ) ;
#69394 = CARTESIAN_POINT ( 'NONE',  ( -10.00000000000000000, 0.000000000000000000, 0.000000000000000000 ) ) ;
#69395 = PLANE ( 'NONE',  #43347 ) ;
#69396 = FACE_OUTER_BOUND ( 'NONE', #30047, .T. ) ;
#69397 = DIRECTION ( 'NONE',  ( 0.3420201433256714330, 4.188538737677025045E-17, -0.9396926207859073177 ) ) ;
#69398 = DIRECTION ( 'NONE',  ( -1.000000000000000000, -0.000000000000000000, 0.000000000000000000 ) ) ;
#69399 = CIRCLE ( 'NONE', #5776, 77.49900000000000944 ) ;
#69400 = CARTESIAN_POINT ( 'NONE',  ( 94.99999999999998579, 92.66308142843932671, 88.37281250086715545 ) ) ;
#69401 = AXIS2_PLACEMENT_3D ( 'NONE', #17074, #11419, #67457 ) ;
#69402 = AXIS2_PLACEMENT_3D ( 'NONE', #40849, #1023, #8097 ) ;
#69403 = DIRECTION ( 'NONE',  ( 0.000000000000000000, 0.3826834323650907810, -0.9238795325112864054 ) ) ;
#69404 = CARTESIAN_POINT ( 'NONE',  ( 11.99999999999999822, 0.000000000000000000, 0.000000000000000000 ) ) ;
#69406 = EDGE_CURVE ( 'NONE', #42737, #62456, #16702, .T. ) ;
#69405 = ORIENTED_EDGE ( 'NONE', *, *, #49069, .F. ) ;
#69407 = CARTESIAN_POINT ( 'NONE',  ( -92.69370383062504004, 90.00000000000004263, 81.07031250086714635 ) ) ;
#69408 = VECTOR ( 'NONE', #29427, 1000.000000000000000 ) ;
#69409 = AXIS2_PLACEMENT_3D ( 'NONE', #5355, #33148, #38804 ) ;
#69410 = EDGE_CURVE ( 'NONE', #72289, #25980, #11702, .T. ) ;
#69411 = CARTESIAN_POINT ( 'NONE',  ( 97.30629616937498838, -208.6684592857803011, 88.74322916753379786 ) ) ;
#69412 = EDGE_CURVE ( 'NONE', #10724, #65641, #67578, .T. ) ;
#69413 = VERTEX_POINT ( 'NONE', #46758 ) ;
#69414 = LINE ( 'NONE', #65549, #38461 ) ;
#69415 = EDGE_LOOP ( 'NONE', ( #49996, #58635, #47780, #25578 ) ) ;
#69416 = EDGE_CURVE ( 'NONE', #30664, #54778, #69680, .T. ) ;
#69417 = CYLINDRICAL_SURFACE ( 'NONE', #4569, 15.69999999999999929 ) ;
#69418 = DIRECTION ( 'NONE',  ( -1.000000000000000000, 0.000000000000000000, -0.000000000000000000 ) ) ;
#69419 = VECTOR ( 'NONE', #59837, 1000.000000000000000 ) ;
#69420 = VECTOR ( 'NONE', #55123, 1000.000000000000000 ) ;
#69421 = ORIENTED_EDGE ( 'NONE', *, *, #56112, .F. ) ;
#69422 = ORIENTED_EDGE ( 'NONE', *, *, #6000, .T. ) ;
#69423 = VECTOR ( 'NONE', #73107, 1000.000000000000000 ) ;
#69424 = CIRCLE ( 'NONE', #22638, 16.00000000000000000 ) ;
#69425 = CARTESIAN_POINT ( 'NONE',  ( 93.84685191531251292, -211.9973110713294489, 81.01739583420049939 ) ) ;
#69426 = FACE_OUTER_BOUND ( 'NONE', #53071, .T. ) ;
#69427 = DIRECTION ( 'NONE',  ( -1.000000000000000000, -0.000000000000000000, 0.000000000000000000 ) ) ;
#69428 =( GEOMETRIC_REPRESENTATION_CONTEXT ( 3 ) GLOBAL_UNCERTAINTY_ASSIGNED_CONTEXT ( ( #69171 ) ) GLOBAL_UNIT_ASSIGNED_CONTEXT ( ( #57953, #30471, #58320 ) ) REPRESENTATION_CONTEXT ( 'NONE', 'WORKASPACE' ) );
#69429 = CARTESIAN_POINT ( 'NONE',  ( 93.67499999999998295, 92.29496732002878900, 82.90916666666666401 ) ) ;
#69430 =( BOUNDED_CURVE ( )  B_SPLINE_CURVE ( 2, ( #72600, #21106, #63216, #51545, #34999, #39910, #47391, #47026, #57570 ),
 .UNSPECIFIED., .F., .F. ) 
 B_SPLINE_CURVE_WITH_KNOTS ( ( 3, 2, 2, 2, 3 ),
 ( 0.6138516023186938453, 0.6209073675976485296, 0.6279631331385309156, 0.6350188986794131907, 0.6350190250571090544 ),
 .UNSPECIFIED. ) 
 CURVE ( )  GEOMETRIC_REPRESENTATION_ITEM ( )  RATIONAL_B_SPLINE_CURVE ( ( 1.000000000000000000, 0.8660254037844387076, 1.000000000000000000, 0.8660254037844387076, 1.000000000000000000, 0.8660254037844387076, 1.000000000000000000, 0.9999976003453241447, 0.9999952007766099715 ) ) 
 REPRESENTATION_ITEM ( '' )  );
#69431 = CYLINDRICAL_SURFACE ( 'NONE', #8673, 82.00000000000000000 ) ;
#69432 = ADVANCED_FACE ( 'NONE', ( #52765 ), #41477, .T. ) ;
#69433 = DIRECTION ( 'NONE',  ( 0.000000000000000000, -0.4539904997395541875, 0.8910065241883642351 ) ) ;
#69434 = CARTESIAN_POINT ( 'NONE',  ( 97.64999999999997726, -211.5299782133524502, 84.54958333333333087 ) ) ;
#69435 = ORIENTED_EDGE ( 'NONE', *, *, #31331, .T. ) ;
#69436 = ORIENTED_EDGE ( 'NONE', *, *, #73226, .T. ) ;
#69437 = EDGE_LOOP ( 'NONE', ( #66674, #52054, #36911, #58500 ) ) ;
#69438 = EDGE_LOOP ( 'NONE', ( #55282, #17577, #44569, #11128 ) ) ;
#69439 = DIRECTION ( 'NONE',  ( 1.000000000000000000, 0.000000000000000000, 0.000000000000000000 ) ) ;
#69440 = CARTESIAN_POINT ( 'NONE',  ( -92.69370383062504004, 90.00000000000004263, 88.84906250086716284 ) ) ;
#69441 = DIRECTION ( 'NONE',  ( -1.000000000000000000, -0.000000000000000000, 0.000000000000000000 ) ) ;
#69442 = DIRECTION ( 'NONE',  ( 1.000000000000000000, 0.000000000000000000, 0.000000000000000000 ) ) ;
#69443 = CARTESIAN_POINT ( 'NONE',  ( 97.64999999999999147, -209.9999999999999716, 77.06187500173429328 ) ) ;
#69444 = CARTESIAN_POINT ( 'NONE',  ( 97.64999999999999147, 90.00000000000002842, 78.25249999999999773 ) ) ;
#69445 = ORIENTED_EDGE ( 'NONE', *, *, #39683, .T. ) ;
#69446 = CARTESIAN_POINT ( 'NONE',  ( -92.34999999999999432, -211.5299782133524502, 88.43895833506762472 ) ) ;
#69447 = ORIENTED_EDGE ( 'NONE', *, *, #1499, .F. ) ;
#69448 = ADVANCED_FACE ( 'NONE', ( #58777 ), #46384, .F. ) ;
#69449 = CARTESIAN_POINT ( 'NONE',  ( 0.000000000000000000, -10.96151621346514382, 35.95386929396252640 ) ) ;
#69450 = EDGE_CURVE ( 'NONE', #22476, #24772, #6898, .T. ) ;
#69451 = ORIENTED_EDGE ( 'NONE', *, *, #18930, .F. ) ;
#69452 = CARTESIAN_POINT ( 'NONE',  ( -96.32500000000001705, 87.70503267997129626, 88.28020833506764120 ) ) ;
#69453 = CARTESIAN_POINT ( 'NONE',  ( -95.00000000000002842, 92.66308142843932671, 82.02281250086714692 ) ) ;
#69454 = VECTOR ( 'NONE', #6660, 1000.000000000000000 ) ;
#69455 = CARTESIAN_POINT ( 'NONE',  ( 93.84685191531248449, 88.00268892867053694, 76.41364583420048007 ) ) ;
#69456 = ORIENTED_EDGE ( 'NONE', *, *, #43202, .T. ) ;
#69457 = DIRECTION ( 'NONE',  ( -1.000000000000000000, -0.000000000000000000, -0.000000000000000000 ) ) ;
#69458 = AXIS2_PLACEMENT_3D ( 'NONE', #12529, #29077, #24921 ) ;
#69459 = VECTOR ( 'NONE', #64146, 1000.000000000000000 ) ;
#69460 = CYLINDRICAL_SURFACE ( 'NONE', #25411, 2.649999999999985700 ) ;
#69461 = FACE_OUTER_BOUND ( 'NONE', #26569, .T. ) ;
#69462 = CARTESIAN_POINT ( 'NONE',  ( -92.69370383062504004, 90.27617560457107970, 74.79348190356851944 ) ) ;
#69463 = ORIENTED_EDGE ( 'NONE', *, *, #4864, .T. ) ;
#69464 = DIRECTION ( 'NONE',  ( 0.000000000000000000, 0.5877852522924743583, -0.8090169943749465631 ) ) ;
#69465 = CARTESIAN_POINT ( 'NONE',  ( -93.84685191531247028, -211.9973110713294489, 76.51947916753380241 ) ) ;
#69466 = VERTEX_POINT ( 'NONE', #6536 ) ;
#69467 = AXIS2_PLACEMENT_3D ( 'NONE', #51548, #12064, #12430 ) ;
#69468 = ORIENTED_EDGE ( 'NONE', *, *, #44051, .T. ) ;
#69469 = VECTOR ( 'NONE', #49608, 1000.000000000000000 ) ;
#69470 = FACE_OUTER_BOUND ( 'NONE', #7208, .T. ) ;
#69471 = VERTEX_POINT ( 'NONE', #561 ) ;
#69472 = CARTESIAN_POINT ( 'NONE',  ( 11.99999999999999822, 0.000000000000000000, 0.000000000000000000 ) ) ;
#69473 = CARTESIAN_POINT ( 'NONE',  ( 0.000000000000000000, 51.03279382321166224, -55.19960302592011914 ) ) ;
#69474 = ORIENTED_EDGE ( 'NONE', *, *, #34539, .F. ) ;
#69475 = CARTESIAN_POINT ( 'NONE',  ( -93.84685191531247028, -211.9973110713294489, 87.47322916753381605 ) ) ;
#69476 = ORIENTED_EDGE ( 'NONE', *, *, #61024, .F. ) ;
#69477 = CARTESIAN_POINT ( 'NONE',  ( 0.000000000000000000, 0.8261519478441983200, -77.49459641780885022 ) ) ;
#69478 = DIRECTION ( 'NONE',  ( 0.000000000000000000, 0.000000000000000000, 1.000000000000000000 ) ) ;
#69479 = ORIENTED_EDGE ( 'NONE', *, *, #42717, .T. ) ;
#69480 = VECTOR ( 'NONE', #70405, 1000.000000000000000 ) ;
#69481 = VERTEX_POINT ( 'NONE', #13273 ) ;
#69482 = DIRECTION ( 'NONE',  ( -1.000000000000000000, 0.000000000000000000, 0.000000000000000000 ) ) ;
#69483 = AXIS2_PLACEMENT_3D ( 'NONE', #17295, #63547, #63182 ) ;
#69484 = CARTESIAN_POINT ( 'NONE',  ( 0.000000000000000000, -33.71516098798685590, -74.74816331893465815 ) ) ;
#69485 = CARTESIAN_POINT ( 'NONE',  ( 92.69370383062498320, 88.66845928578035796, 84.61572916753380014 ) ) ;
#69486 = CARTESIAN_POINT ( 'NONE',  ( -10.00000000000000000, 0.000000000000000000, 0.000000000000000000 ) ) ;
#69487 = LINE ( 'NONE', #46199, #28987 ) ;
#69488 = CARTESIAN_POINT ( 'NONE',  ( 10.00000000000000000, 75.54627589209970040, -17.28742895386005785 ) ) ;
#69489 = TOROIDAL_SURFACE ( 'NONE', #37066, 18.00000000000000000, 3.300000000000000266 ) ;
#69490 = DIRECTION ( 'NONE',  ( -0.000000000000000000, 0.9945218953682731788, 0.1045284632676559550 ) ) ;
#69491 = AXIS2_PLACEMENT_3D ( 'NONE', #38433, #4613, #32773 ) ;
#69492 = PLANE ( 'NONE',  #50025 ) ;
#69493 = DIRECTION ( 'NONE',  ( -1.000000000000000000, 0.000000000000000000, 0.000000000000000000 ) ) ;
#69494 = CARTESIAN_POINT ( 'NONE',  ( -3.000000000000000000, 22.07842321921481243, 8.187992925817422218 ) ) ;
#69495 = EDGE_CURVE ( 'NONE', #24664, #66054, #64419, .T. ) ;
#69496 = DIRECTION ( 'NONE',  ( 0.000000000000000000, 0.000000000000000000, 1.000000000000000000 ) ) ;
#69497 = EDGE_CURVE ( 'NONE', #29066, #21068, #19279, .T. ) ;
#69498 = DIRECTION ( 'NONE',  ( -1.000000000000000000, 7.571544473058805744E-15, 2.612289469705706870E-14 ) ) ;
#69499 = CARTESIAN_POINT ( 'NONE',  ( -96.15314808468751551, 88.00268892867056536, 89.11364583420048291 ) ) ;
#69500 = CYLINDRICAL_SURFACE ( 'NONE', #55070, 77.49899999999999523 ) ;
#69501 = EDGE_CURVE ( 'NONE', #49856, #63817, #18177, .T. ) ;
#69502 = EDGE_CURVE ( 'NONE', #30226, #17504, #52011, .T. ) ;
#69503 = CIRCLE ( 'NONE', #1124, 31.99999999999999289 ) ;
#69504 = FACE_OUTER_BOUND ( 'NONE', #61005, .T. ) ;
#69505 = VERTEX_POINT ( 'NONE', #12894 ) ;
#69506 = AXIS2_PLACEMENT_3D ( 'NONE', #49754, #56150, #32832 ) ;
#69507 = FACE_OUTER_BOUND ( 'NONE', #22563, .T. ) ;
#69508 = CYLINDRICAL_SURFACE ( 'NONE', #29874, 31.99999999999998579 ) ;
#69509 = AXIS2_PLACEMENT_3D ( 'NONE', #22759, #33259, #3983 ) ;
#69510 = CARTESIAN_POINT ( 'NONE',  ( -12.50000000000000000, -132.5000000000000000, -40.00000000000000000 ) ) ;
#69511 = EDGE_CURVE ( 'NONE', #37081, #8769, #11655, .T. ) ;
#69512 = CARTESIAN_POINT ( 'NONE',  ( 10.00000000000000000, 80.28980883073779751, -16.65972982744850839 ) ) ;
#69513 = CARTESIAN_POINT ( 'NONE',  ( 96.15314808468748708, -208.0026889286704943, 84.50989583420049200 ) ) ;
#69514 = CIRCLE ( 'NONE', #70736, 31.99999999999998579 ) ;
#69515 = ORIENTED_EDGE ( 'NONE', *, *, #48781, .F. ) ;
#69516 = ORIENTED_EDGE ( 'NONE', *, *, #9400, .T. ) ;
#69517 = CARTESIAN_POINT ( 'NONE',  ( 50.00005079999999680, 0.000000000000000000, 0.000000000000000000 ) ) ;
#69518 = VERTEX_POINT ( 'NONE', #23454 ) ;
#69519 = EDGE_CURVE ( 'NONE', #27817, #70179, #69311, .T. ) ;
#69520 = LINE ( 'NONE', #58602, #10125 ) ;
#69521 = CARTESIAN_POINT ( 'NONE',  ( -21.33958957442910886, -129.9559990355020034, -2.500000000000000000 ) ) ;
#69523 = ORIENTED_EDGE ( 'NONE', *, *, #28774, .F. ) ;
#69522 = EDGE_CURVE ( 'NONE', #1800, #23675, #30189, .T. ) ;
#69524 = CARTESIAN_POINT ( 'NONE',  ( 96.15314808468748708, -208.0026889286704943, 80.69989583420047552 ) ) ;
#69525 = VECTOR ( 'NONE', #44997, 1000.000000000000114 ) ;
#69526 = AXIS2_PLACEMENT_3D ( 'NONE', #25677, #66645, #15127 ) ;
#69527 = ORIENTED_EDGE ( 'NONE', *, *, #1576, .F. ) ;
#69528 = CARTESIAN_POINT ( 'NONE',  ( 97.64999999999999147, 90.00000000000002842, 79.52249999999999375 ) ) ;
#69529 = VERTEX_POINT ( 'NONE', #58397 ) ;
#69530 = EDGE_CURVE ( 'NONE', #39290, #4576, #3326, .T. ) ;
#69531 = ADVANCED_FACE ( 'NONE', ( #70036 ), #35467, .F. ) ;
#69532 = ORIENTED_EDGE ( 'NONE', *, *, #30466, .F. ) ;
#69533 = CARTESIAN_POINT ( 'NONE',  ( 10.00000000000000000, -5.202137450156655518, 37.22597642581156663 ) ) ;
#69534 = AXIS2_PLACEMENT_3D ( 'NONE', #66084, #14553, #42032 ) ;
#69535 = CARTESIAN_POINT ( 'NONE',  ( 10.00000000000000000, -37.48860685352290290, -0.8828120875904512665 ) ) ;
#69536 = VECTOR ( 'NONE', #14596, 1000.000000000000000 ) ;
#69537 = ORIENTED_EDGE ( 'NONE', *, *, #9865, .F. ) ;
#69538 = CARTESIAN_POINT ( 'NONE',  ( 18.80329974962065265, -105.8248132807389084, 5.500000000000000000 ) ) ;
#69539 = CARTESIAN_POINT ( 'NONE',  ( 97.64999999999997726, -208.4700217866474645, 87.90979166840095615 ) ) ;
#69540 = AXIS2_PLACEMENT_3D ( 'NONE', #64338, #30468, #58318 ) ;
#69541 = ORIENTED_EDGE ( 'NONE', *, *, #8196, .T. ) ;
#69542 = DIRECTION ( 'NONE',  ( 1.000000000000000000, 0.000000000000000000, 0.000000000000000000 ) ) ;
#69543 = EDGE_CURVE ( 'NONE', #24805, #2169, #60268, .T. ) ;
#69544 = ORIENTED_EDGE ( 'NONE', *, *, #36408, .F. ) ;
#69545 = CARTESIAN_POINT ( 'NONE',  ( 11.99999999999999822, 0.000000000000000000, 0.000000000000000000 ) ) ;
#69546 = ORIENTED_EDGE ( 'NONE', *, *, #48566, .T. ) ;
#69547 = CARTESIAN_POINT ( 'NONE',  ( 94.99999999999998579, 86.94004357329500010, 85.15812500173430521 ) ) ;
#69548 = EDGE_CURVE ( 'NONE', #71438, #4362, #8749, .T. ) ;
#69549 = ORIENTED_EDGE ( 'NONE', *, *, #42139, .F. ) ;
#69550 = ORIENTED_EDGE ( 'NONE', *, *, #40648, .T. ) ;
#69551 = CARTESIAN_POINT ( 'NONE',  ( -93.67499999999998295, -212.2949673200287179, 78.22604166840096696 ) ) ;
#69552 = DIRECTION ( 'NONE',  ( -1.000000000000000000, -0.000000000000000000, 0.000000000000000000 ) ) ;
#69553 = ORIENTED_EDGE ( 'NONE', *, *, #18737, .T. ) ;
#69554 = ORIENTED_EDGE ( 'NONE', *, *, #36742, .T. ) ;
#69555 = ORIENTED_EDGE ( 'NONE', *, *, #42130, .F. ) ;
#69556 = CARTESIAN_POINT ( 'NONE',  ( 97.64999999999999147, 90.00000015433757028, 79.60187500750917877 ) ) ;
#69557 = DIRECTION ( 'NONE',  ( 0.000000000000000000, 0.000000000000000000, 1.000000000000000000 ) ) ;
#69558 = CARTESIAN_POINT ( 'NONE',  ( -92.35000000000005116, 91.52997821335253548, 88.46541666666665549 ) ) ;
#69559 = ORIENTED_EDGE ( 'NONE', *, *, #14772, .T. ) ;
#69560 = CARTESIAN_POINT ( 'NONE',  ( 97.30629616937498838, 90.00000000000002842, 75.35531250086714294 ) ) ;
#69561 = ORIENTED_EDGE ( 'NONE', *, *, #29930, .F. ) ;
#69562 = DIRECTION ( 'NONE',  ( -0.3311129884571281101, -0.9435911131814402886, 0.000000000000000000 ) ) ;
#69563 = CARTESIAN_POINT ( 'NONE',  ( -96.15314808468747287, -208.0026889286704943, 84.45697916753380241 ) ) ;
#69564 = EDGE_LOOP ( 'NONE', ( #40796, #61814, #6751, #52932 ) ) ;
#69565 = CIRCLE ( 'NONE', #56378, 0.5999999999999928724 ) ;
#69566 = DIRECTION ( 'NONE',  ( 7.962523111838990267E-16, 1.065814103640131188E-14, 1.000000000000000000 ) ) ;
#69567 = CYLINDRICAL_SURFACE ( 'NONE', #17625, 77.49899999999999523 ) ;
#69568 = CARTESIAN_POINT ( 'NONE',  ( 97.64999999999999147, 90.00000000000002842, 81.42749999999999488 ) ) ;
#69569 = CARTESIAN_POINT ( 'NONE',  ( -94.99999999999997158, -212.6630814284392557, 77.73656250086713726 ) ) ;
#69570 = CIRCLE ( 'NONE', #1198, 31.99999999999999289 ) ;
#69571 = VECTOR ( 'NONE', #30987, 1000.000000000000000 ) ;
#69572 = AXIS2_PLACEMENT_3D ( 'NONE', #25636, #42203, #42565 ) ;
#69573 = DIRECTION ( 'NONE',  ( -1.000000000000000000, 0.000000000000000000, 0.000000000000000000 ) ) ;
#69574 = DIRECTION ( 'NONE',  ( 1.000000000000000000, 0.000000000000000000, 0.000000000000000000 ) ) ;
#69575 = FACE_OUTER_BOUND ( 'NONE', #41241, .T. ) ;
#69576 = DIRECTION ( 'NONE',  ( 1.000000000000000000, 0.000000000000000000, 0.000000000000000000 ) ) ;
#69577 = DIRECTION ( 'NONE',  ( 0.4279312458753000703, 0.9038112904824842087, -0.000000000000000000 ) ) ;
#69578 = DIRECTION ( 'NONE',  ( -1.000000000000000000, -0.000000000000000000, -0.000000000000000000 ) ) ;
#69579 = CARTESIAN_POINT ( 'NONE',  ( -92.69370383062502583, 88.66845928578038638, 78.47739583420047893 ) ) ;
#69580 = CARTESIAN_POINT ( 'NONE',  ( 0.000000000000000000, 0.000000000000000000, 0.000000000000000000 ) ) ;
#69581 = DIRECTION ( 'NONE',  ( 0.000000000000000000, -0.2079116908177664758, 0.9781476007338042455 ) ) ;
#69582 = ORIENTED_EDGE ( 'NONE', *, *, #59794, .F. ) ;
#69583 = LINE ( 'NONE', #63961, #35229 ) ;
#69584 = VECTOR ( 'NONE', #38684, 1000.000000000000114 ) ;
#69585 = ADVANCED_FACE ( 'NONE', ( #66634 ), #19644, .F. ) ;
#69586 = CARTESIAN_POINT ( 'NONE',  ( 96.32499999999998863, -207.7050326799711968, 89.23270833506762756 ) ) ;
#69587 = CARTESIAN_POINT ( 'NONE',  ( 10.00000000000000000, -35.92658777277517856, 10.74501242461269257 ) ) ;
#69588 = CIRCLE ( 'NONE', #39595, 82.00000000000000000 ) ;
#69589 = DIRECTION ( 'NONE',  ( -1.000000000000000000, 0.000000000000000000, 0.000000000000000000 ) ) ;
#69590 = EDGE_CURVE ( 'NONE', #17276, #43589, #71752, .T. ) ;
#69591 = PLANE ( 'NONE',  #74192 ) ;
#69592 = DIRECTION ( 'NONE',  ( 0.000000000000000000, 0.000000000000000000, -1.000000000000000000 ) ) ;
#69593 = CARTESIAN_POINT ( 'NONE',  ( -94.99999999999997158, -212.6630814284392557, 76.62531250086715318 ) ) ;
#69594 = VECTOR ( 'NONE', #60668, 1000.000000000000000 ) ;
#69595 = ADVANCED_FACE ( 'NONE', ( #20757 ), #20010, .F. ) ;
#69596 = VECTOR ( 'NONE', #1865, 1000.000000000000000 ) ;
#69597 = ADVANCED_FACE ( 'NONE', ( #43352 ), #2776, .F. ) ;
#69598 = FACE_OUTER_BOUND ( 'NONE', #36088, .T. ) ;
#69599 = VERTEX_POINT ( 'NONE', #43711 ) ;
#69600 = FACE_OUTER_BOUND ( 'NONE', #36638, .T. ) ;
#69601 = CARTESIAN_POINT ( 'NONE',  ( 10.00000000000000000, 73.44644590900061587, 24.73286445877730699 ) ) ;
#69602 = CYLINDRICAL_SURFACE ( 'NONE', #38250, 77.49899999999999523 ) ;
#69603 = CARTESIAN_POINT ( 'NONE',  ( 5.000000000000000000, 39.04073710021344112, 15.48615015657596850 ) ) ;
#69604 = CYLINDRICAL_SURFACE ( 'NONE', #24714, 20.99999999999999645 ) ;
#69605 = EDGE_CURVE ( 'NONE', #57518, #27140, #18954, .T. ) ;
#69606 = EDGE_LOOP ( 'NONE', ( #39917, #41272 ) ) ;
#69607 = CYLINDRICAL_SURFACE ( 'NONE', #43267, 42.00000000000000000 ) ;
#69608 = EDGE_LOOP ( 'NONE', ( #5376, #42072 ) ) ;
#69609 = AXIS2_PLACEMENT_3D ( 'NONE', #13013, #43093, #61398 ) ;
#69610 = CARTESIAN_POINT ( 'NONE',  ( 92.69370383062501162, -211.3315407142195852, 83.98072916753380923 ) ) ;
#69611 = CARTESIAN_POINT ( 'NONE',  ( 11.99999999999999822, 44.88180994100466847, -63.18004540532978552 ) ) ;
#69612 = ORIENTED_EDGE ( 'NONE', *, *, #15255, .F. ) ;
#69613 = AXIS2_PLACEMENT_3D ( 'NONE', #16303, #5044, #26832 ) ;
#69614 = DIRECTION ( 'NONE',  ( 0.000000000000000000, 0.000000000000000000, 1.000000000000000000 ) ) ;
#69615 = CIRCLE ( 'NONE', #55234, 37.49900000000000233 ) ;
#69616 = ORIENTED_EDGE ( 'NONE', *, *, #54069, .T. ) ;
#69617 = DIRECTION ( 'NONE',  ( -1.000000000000000000, 0.000000000000000000, 0.000000000000000000 ) ) ;
#69618 = ORIENTED_EDGE ( 'NONE', *, *, #9417, .T. ) ;
#69619 = ADVANCED_FACE ( 'NONE', ( #59516 ), #14382, .T. ) ;
#69620 = EDGE_CURVE ( 'NONE', #6205, #3158, #48951, .T. ) ;
#69621 = CARTESIAN_POINT ( 'NONE',  ( -97.30629616937501680, 88.66845928578038638, 79.05947916753382287 ) ) ;
#69622 = ORIENTED_EDGE ( 'NONE', *, *, #18105, .F. ) ;
#69623 = ORIENTED_EDGE ( 'NONE', *, *, #20173, .T. ) ;
#69624 = CIRCLE ( 'NONE', #7211, 12.83284365640956182 ) ;
#69625 = ORIENTED_EDGE ( 'NONE', *, *, #664, .F. ) ;
#69626 = FACE_OUTER_BOUND ( 'NONE', #3911, .T. ) ;
#69627 = DIRECTION ( 'NONE',  ( -0.000000000000000000, -0.000000000000000000, -1.000000000000000000 ) ) ;
#69628 = VERTEX_POINT ( 'NONE', #8003 ) ;
#69629 = DIRECTION ( 'NONE',  ( 0.000000000000000000, 0.000000000000000000, 1.000000000000000000 ) ) ;
#69630 = ORIENTED_EDGE ( 'NONE', *, *, #51533, .F. ) ;
#69631 = CARTESIAN_POINT ( 'NONE',  ( 93.67500000000001137, -212.2949673200287179, 80.66020833506763665 ) ) ;
#69632 = ORIENTED_EDGE ( 'NONE', *, *, #33959, .T. ) ;
#69633 = AXIS2_PLACEMENT_3D ( 'NONE', #24720, #58190, #6691 ) ;
#69634 = ORIENTED_EDGE ( 'NONE', *, *, #18280, .T. ) ;
#69635 = ORIENTED_EDGE ( 'NONE', *, *, #4954, .T. ) ;
#69636 = VECTOR ( 'NONE', #70577, 1000.000000000000000 ) ;
#69637 = CARTESIAN_POINT ( 'NONE',  ( 93.84685191531249870, -208.0026889286704943, 81.28197916753380525 ) ) ;
#69638 = APPLICATION_PROTOCOL_DEFINITION ( 'draft international standard', 'automotive_design', 1998, #70024 ) ;
#69639 = CARTESIAN_POINT ( 'NONE',  ( 10.00000000000000000, -15.33399622253540251, 80.55351364060582853 ) ) ;
#69640 = CARTESIAN_POINT ( 'NONE',  ( -96.32500000000001705, 87.70503267997129626, 84.39083333333333314 ) ) ;
#69641 = CARTESIAN_POINT ( 'NONE',  ( 97.64999999999997726, -208.4700217866474929, 78.94041666666664980 ) ) ;
#69642 = DIRECTION ( 'NONE',  ( -2.628368902995175337E-16, -1.000000000000000000, 0.000000000000000000 ) ) ;
#69643 = CARTESIAN_POINT ( 'NONE',  ( -97.64999999999997726, 88.47002178664750716, 79.25791666666667368 ) ) ;
#69644 = AXIS2_PLACEMENT_3D ( 'NONE', #56036, #4555, #32353 ) ;
#69645 = DIRECTION ( 'NONE',  ( 0.6691306063588671194, -0.7431448254773862505, 0.000000000000000000 ) ) ;
#69646 = AXIS2_PLACEMENT_3D ( 'NONE', #44835, #61388, #27141 ) ;
#69647 = CARTESIAN_POINT ( 'NONE',  ( -96.15314808468745866, -211.9973110713294489, 85.30364583420046642 ) ) ;
#69648 = CARTESIAN_POINT ( 'NONE',  ( -92.69370383062504004, 90.00000000000004263, 83.76906250086716454 ) ) ;
#69649 = EDGE_LOOP ( 'NONE', ( #1329, #52537, #45531, #35599 ) ) ;
#69650 = CARTESIAN_POINT ( 'NONE',  ( 97.30629616937498838, 88.66845928578037217, 83.55739583420047722 ) ) ;
#69651 =( BOUNDED_CURVE ( )  B_SPLINE_CURVE ( 2, ( #68091, #11310, #17327, #28226, #62850, #41010, #449 ),
 .UNSPECIFIED., .F., .F. ) 
 B_SPLINE_CURVE_WITH_KNOTS ( ( 3, 2, 2, 3 ),
 ( 0.1250000000000002220, 0.1319444444444446418, 0.1388888888888890338, 0.1458333333333334536 ),
 .UNSPECIFIED. ) 
 CURVE ( )  GEOMETRIC_REPRESENTATION_ITEM ( )  RATIONAL_B_SPLINE_CURVE ( ( 0.9999999999999956701, 0.8660254037844430375, 1.000000000000000000, 0.8660254037844387076, 1.000000000000000000, 0.8660254037844365982, 1.000000000000002220 ) ) 
 REPRESENTATION_ITEM ( '' )  );
#69652 = ORIENTED_EDGE ( 'NONE', *, *, #66544, .F. ) ;
#69653 = PLANE ( 'NONE',  #1193 ) ;
#69654 = CARTESIAN_POINT ( 'NONE',  ( -3.000000000000000000, 16.83928648764945279, -16.46020748918028076 ) ) ;
#69655 = DIRECTION ( 'NONE',  ( 0.000000000000000000, 0.000000000000000000, 1.000000000000000000 ) ) ;
#69656 = DIRECTION ( 'NONE',  ( 2.603472992746261562E-14, 2.546204323184492723E-14, -1.000000000000000000 ) ) ;
#69657 = CARTESIAN_POINT ( 'NONE',  ( 93.67499999999998295, 92.29496732002878900, 87.35416666666665719 ) ) ;
#69658 = CARTESIAN_POINT ( 'NONE',  ( -97.30629616937495996, -209.9999999999999716, 85.19781250086714408 ) ) ;
#69659 = LINE ( 'NONE', #29788, #47489 ) ;
#69660 = DIRECTION ( 'NONE',  ( 0.000000000000000000, 0.000000000000000000, 1.000000000000000000 ) ) ;
#69661 = DIRECTION ( 'NONE',  ( 0.000000000000000000, 0.000000000000000000, -1.000000000000000000 ) ) ;
#69662 = CIRCLE ( 'NONE', #24050, 31.99999999999998579 ) ;
#69663 = CARTESIAN_POINT ( 'NONE',  ( 97.64999999999999147, -209.9999999999999716, 90.00000000000000000 ) ) ;
#69664 = ORIENTED_EDGE ( 'NONE', *, *, #44379, .F. ) ;
#69665 = VERTEX_POINT ( 'NONE', #25304 ) ;
#69666 = CARTESIAN_POINT ( 'NONE',  ( -96.32500000000001705, 87.70503267997129626, 76.77083333333332860 ) ) ;
#69667 = LINE ( 'NONE', #17426, #18698 ) ;
#69668 = CARTESIAN_POINT ( 'NONE',  ( -92.69370383062504004, 90.00000000000004263, 88.69031250086715090 ) ) ;
#69669 = DIRECTION ( 'NONE',  ( 1.000000000000000000, 0.000000000000000000, 0.000000000000000000 ) ) ;
#69670 = DIRECTION ( 'NONE',  ( -0.9227826878668540234, -0.3853207896976547642, 0.000000000000000000 ) ) ;
#69671 = LINE ( 'NONE', #35095, #37327 ) ;
#69672 = DIRECTION ( 'NONE',  ( -1.000000000000000000, 0.000000000000000000, 0.000000000000000000 ) ) ;
#69673 = ORIENTED_EDGE ( 'NONE', *, *, #39953, .F. ) ;
#69674 = CARTESIAN_POINT ( 'NONE',  ( -92.69370383062502583, 88.66845928578038638, 79.11239583420046984 ) ) ;
#69675 = LINE ( 'NONE', #12525, #33127 ) ;
#69676 = EDGE_CURVE ( 'NONE', #47732, #65728, #63421, .T. ) ;
#69677 = CARTESIAN_POINT ( 'NONE',  ( 26.00000000000000355, 0.000000000000000000, 0.000000000000000000 ) ) ;
#69678 = CARTESIAN_POINT ( 'NONE',  ( 11.99999999999999822, 75.11764819372149304, -2.946379043146603482 ) ) ;
#69679 = EDGE_CURVE ( 'NONE', #41287, #25052, #51377, .T. ) ;
#69680 = LINE ( 'NONE', #6895, #35696 ) ;
#69681 = VECTOR ( 'NONE', #65759, 1000.000000000000000 ) ;
#69682 = CARTESIAN_POINT ( 'NONE',  ( 0.000000000000000000, 37.58145647212453611, 0.6853352020791767529 ) ) ;
#69683 = CARTESIAN_POINT ( 'NONE',  ( -92.69370383062498320, -208.6684592857803011, 85.09197916753380753 ) ) ;
#69684 = EDGE_CURVE ( 'NONE', #38198, #45762, #68190, .T. ) ;
#69685 = CARTESIAN_POINT ( 'NONE',  ( 0.000000000000000000, 20.85821328998756385, -10.92862929874494959 ) ) ;
#69686 = EDGE_CURVE ( 'NONE', #18187, #22980, #15114, .T. ) ;
#69687 = CARTESIAN_POINT ( 'NONE',  ( 94.99999999999998579, 87.33691857156068750, 75.99031250086716227 ) ) ;
#69688 = CARTESIAN_POINT ( 'NONE',  ( -92.69370383062498320, -209.9999999999999716, 78.05406250086716113 ) ) ;
#69689 = CARTESIAN_POINT ( 'NONE',  ( -10.00000000000000000, 0.000000000000000000, 0.000000000000000000 ) ) ;
#69690 = ORIENTED_EDGE ( 'NONE', *, *, #45708, .F. ) ;
#69691 = CARTESIAN_POINT ( 'NONE',  ( 11.99999999999999822, -20.41045688087876897, 72.35160999960810102 ) ) ;
#69692 = CARTESIAN_POINT ( 'NONE',  ( 97.64999999999989200, 91.52997821335259232, 75.76541666666668107 ) ) ;
#69693 = FACE_OUTER_BOUND ( 'NONE', #31240, .T. ) ;
#69694 = VECTOR ( 'NONE', #22913, 1000.000000000000000 ) ;
#69695 = VECTOR ( 'NONE', #18413, 1000.000000000000000 ) ;
#69696 = AXIS2_PLACEMENT_3D ( 'NONE', #41861, #31683, #3148 ) ;
#69697 = CARTESIAN_POINT ( 'NONE',  ( 0.000000000000000000, -0.8299999999999999600, 0.000000000000000000 ) ) ;
#69699 = EDGE_CURVE ( 'NONE', #13774, #2617, #34908, .T. ) ;
#69698 = CARTESIAN_POINT ( 'NONE',  ( 97.30629616937498838, -211.3315407142195852, 78.47739583420047893 ) ) ;
#69700 = ORIENTED_EDGE ( 'NONE', *, *, #50607, .F. ) ;
#69701 = ADVANCED_FACE ( 'NONE', ( #67364 ), #62492, .T. ) ;
#69702 = EDGE_LOOP ( 'NONE', ( #26127, #26882, #70436, #509 ) ) ;
#69703 = DIRECTION ( 'NONE',  ( -1.000000000000000000, -0.000000000000000000, -0.000000000000000000 ) ) ;
#69704 = ORIENTED_EDGE ( 'NONE', *, *, #52022, .T. ) ;
#69705 = FACE_OUTER_BOUND ( 'NONE', #49736, .T. ) ;
#69706 = ADVANCED_FACE ( 'NONE', ( #16602 ), #44816, .T. ) ;
#69707 = EDGE_CURVE ( 'NONE', #25328, #17282, #63363, .T. ) ;
#69708 = ORIENTED_EDGE ( 'NONE', *, *, #10864, .F. ) ;
#69709 = ORIENTED_EDGE ( 'NONE', *, *, #71051, .F. ) ;
#69710 = VERTEX_POINT ( 'NONE', #51180 ) ;
#69711 = DIRECTION ( 'NONE',  ( -1.000000000000000000, -0.000000000000000000, 0.000000000000000000 ) ) ;
#69712 = ORIENTED_EDGE ( 'NONE', *, *, #3529, .T. ) ;
#69713 = ORIENTED_EDGE ( 'NONE', *, *, #19924, .T. ) ;
#69714 = CARTESIAN_POINT ( 'NONE',  ( 93.84685191531248449, 91.99731107132950569, 83.34572916753383254 ) ) ;
#69715 = CARTESIAN_POINT ( 'NONE',  ( -97.65000000000001990, 90.00000000000004263, 81.18937500173430521 ) ) ;
#69716 = DIRECTION ( 'NONE',  ( -1.000000000000000000, 7.571539615859142926E-15, 2.592266024478009537E-14 ) ) ;
#69717 = ORIENTED_EDGE ( 'NONE', *, *, #41079, .F. ) ;
#69718 = EDGE_LOOP ( 'NONE', ( #45697, #22876, #7781, #68529 ) ) ;
#69719 = AXIS2_PLACEMENT_3D ( 'NONE', #36291, #18264, #35189 ) ;
#69720 = ORIENTED_EDGE ( 'NONE', *, *, #65546, .F. ) ;
#69721 = VERTEX_POINT ( 'NONE', #21488 ) ;
#69722 = DIRECTION ( 'NONE',  ( -0.000000000000000000, 0.000000000000000000, -1.000000000000000000 ) ) ;
#69723 = ORIENTED_EDGE ( 'NONE', *, *, #9224, .F. ) ;
#69724 = DIRECTION ( 'NONE',  ( 2.775557561562891351E-17, 0.000000000000000000, -1.000000000000000000 ) ) ;
#69725 = CARTESIAN_POINT ( 'NONE',  ( -97.64999999999996305, -209.9999999999999716, 75.47437500173430180 ) ) ;
#69726 = DIRECTION ( 'NONE',  ( 0.000000000000000000, 0.5224985647159499091, -0.8526401643540916231 ) ) ;
#69727 = CARTESIAN_POINT ( 'NONE',  ( 10.00000000000000000, -37.58145647212453611, -0.6853352020794456489 ) ) ;
#69728 = DIRECTION ( 'NONE',  ( -1.000000000000000000, 0.000000000000000000, -0.000000000000000000 ) ) ;
#69729 = CARTESIAN_POINT ( 'NONE',  ( 11.99999999999999822, -8.966570791700153364, -81.50828551894235829 ) ) ;
#69730 = CARTESIAN_POINT ( 'NONE',  ( -92.34999999999999432, -211.5299782133524502, 77.64395833506762301 ) ) ;
#69731 = ORIENTED_EDGE ( 'NONE', *, *, #14839, .F. ) ;
#69732 = DIRECTION ( 'NONE',  ( -1.000000000000000000, 0.000000000000000000, 0.000000000000000000 ) ) ;
#69733 = VERTEX_POINT ( 'NONE', #38427 ) ;
#69735 = CARTESIAN_POINT ( 'NONE',  ( -95.00000000000002842, 86.94004357329504273, 77.53812500173428646 ) ) ;
#69734 = CARTESIAN_POINT ( 'NONE',  ( 92.34999999999999432, 90.00000000000002842, 79.91937500173429498 ) ) ;
#69736 = VERTEX_POINT ( 'NONE', #62871 ) ;
#69737 = CARTESIAN_POINT ( 'NONE',  ( 96.15314808468748708, 91.99731107132950569, 78.79489583420048859 ) ) ;
#69738 = CARTESIAN_POINT ( 'NONE',  ( 0.000000000000000000, -80.55351364060599906, 15.33399622253456585 ) ) ;
#69739 = CARTESIAN_POINT ( 'NONE',  ( 0.000000000000000000, -62.50329211542407393, -41.76937507738853839 ) ) ;
#69740 = CARTESIAN_POINT ( 'NONE',  ( -96.32500000000001705, 92.29496732002878900, 86.79854166840097207 ) ) ;
#69741 = AXIS2_PLACEMENT_3D ( 'NONE', #53029, #24451, #70290 ) ;
#69742 = DIRECTION ( 'NONE',  ( 0.000000000000000000, 0.1564344650402244019, 0.9876883405951387696 ) ) ;
#69743 = ORIENTED_EDGE ( 'NONE', *, *, #73152, .T. ) ;
#69744 = DIRECTION ( 'NONE',  ( 0.000000000000000000, 1.000000000000000000, 7.228014483236689653E-16 ) ) ;
#69745 = CIRCLE ( 'NONE', #32539, 15.99999999999999467 ) ;
#69746 = DIRECTION ( 'NONE',  ( -1.000000000000000000, 0.000000000000000000, -0.000000000000000000 ) ) ;
#69747 = ORIENTED_EDGE ( 'NONE', *, *, #19184, .T. ) ;
#69748 = VECTOR ( 'NONE', #40247, 1000.000000000000000 ) ;
#69749 = VERTEX_POINT ( 'NONE', #61367 ) ;
#69750 = EDGE_CURVE ( 'NONE', #49474, #29034, #15359, .T. ) ;
#69751 = CIRCLE ( 'NONE', #10935, 19.05560546998412974 ) ;
#69752 = ADVANCED_FACE ( 'NONE', ( #50804 ), #45569, .T. ) ;
#69753 = EDGE_CURVE ( 'NONE', #14449, #44034, #65765, .T. ) ;
#69754 = CARTESIAN_POINT ( 'NONE',  ( -0.9112620892301054321, -5.247385279376963751, -1.160540885688338131 ) ) ;
#69755 = CARTESIAN_POINT ( 'NONE',  ( 10.00000000000000000, -21.40280677340345505, -36.13751322684441902 ) ) ;
#69756 = CARTESIAN_POINT ( 'NONE',  ( -96.15314808468745866, -211.9973110713294489, 76.57239583420049200 ) ) ;
#69757 = ORIENTED_EDGE ( 'NONE', *, *, #37718, .F. ) ;
#69758 = EDGE_CURVE ( 'NONE', #13671, #68033, #28617, .T. ) ;
#69759 = DIRECTION ( 'NONE',  ( -1.000000000000000000, 0.000000000000000000, 0.000000000000000000 ) ) ;
#69760 = CARTESIAN_POINT ( 'NONE',  ( 11.99999999999999822, 59.03342792756328095, -46.54456581323744757 ) ) ;
#69761 = DIRECTION ( 'NONE',  ( 0.000000000000000000, 0.000000000000000000, -1.000000000000000000 ) ) ;
#69762 = EDGE_CURVE ( 'NONE', #31095, #420, #4606, .T. ) ;
#69763 = CARTESIAN_POINT ( 'NONE',  ( -3.000000000000000000, -11.95096189432312350, -23.69967320028773372 ) ) ;
#69764 = CYLINDRICAL_SURFACE ( 'NONE', #66528, 77.49899999999999523 ) ;
#69765 = DIRECTION ( 'NONE',  ( 0.000000000000000000, 0.5877852522924685852, 0.8090169943749508930 ) ) ;
#69766 = CARTESIAN_POINT ( 'NONE',  ( 10.00000000000000000, 0.000000000000000000, 0.000000000000000000 ) ) ;
#69767 = CYLINDRICAL_SURFACE ( 'NONE', #36399, 82.00000000000000000 ) ;
#69768 = CARTESIAN_POINT ( 'NONE',  ( 0.000000000000000000, 0.000000000000000000, 0.000000000000000000 ) ) ;
#69769 = LINE ( 'NONE', #47956, #69459 ) ;
#69770 = EDGE_CURVE ( 'NONE', #8982, #68341, #39370, .T. ) ;
#69771 = CARTESIAN_POINT ( 'NONE',  ( 97.30629616937498838, 90.00000000000002842, 88.84906250086716284 ) ) ;
#69772 = CARTESIAN_POINT ( 'NONE',  ( -94.99999999999997158, -212.6630814284392557, 88.05531250086714579 ) ) ;
#69773 = CARTESIAN_POINT ( 'NONE',  ( 96.32499999999997442, 92.29496732002878900, 79.07270833506763097 ) ) ;
#69774 = EDGE_LOOP ( 'NONE', ( #41539, #35069, #41974, #16085 ) ) ;
#69775 = AXIS2_PLACEMENT_3D ( 'NONE', #2509, #37427, #15213 ) ;
#69776 = CARTESIAN_POINT ( 'NONE',  ( 97.64999999989935020, -209.9999769027737671, 83.41187580057901130 ) ) ;
#69777 = CARTESIAN_POINT ( 'NONE',  ( -93.67499999999998295, -207.7050326799711968, 82.16833333333332234 ) ) ;
#69778 = CARTESIAN_POINT ( 'NONE',  ( -93.84685191531254134, 91.99731107132950569, 77.36614583420046642 ) ) ;
#69780 = EDGE_CURVE ( 'NONE', #53082, #63185, #29151, .T. ) ;
#69779 = CARTESIAN_POINT ( 'NONE',  ( 97.30629616937498838, -211.3315407142195852, 87.36739583420047950 ) ) ;
#69781 = ADVANCED_FACE ( 'NONE', ( #27123 ), #50056, .T. ) ;
#69782 = ORIENTED_EDGE ( 'NONE', *, *, #24809, .F. ) ;
#69783 = CARTESIAN_POINT ( 'NONE',  ( 95.00000000000000000, -206.9400435732949575, 87.30124999999999602 ) ) ;
#69784 = ORIENTED_EDGE ( 'NONE', *, *, #32978, .T. ) ;
#69785 = CIRCLE ( 'NONE', #68632, 16.00000000000000000 ) ;
#69786 = DIRECTION ( 'NONE',  ( 0.000000000000000000, 0.000000000000000000, -1.000000000000000000 ) ) ;
#69788 = PLANE ( 'NONE',  #64263 ) ;
#69787 = AXIS2_PLACEMENT_3D ( 'NONE', #37859, #68183, #66434 ) ;
#69789 = ORIENTED_EDGE ( 'NONE', *, *, #20864, .F. ) ;
#69790 = AXIS2_PLACEMENT_3D ( 'NONE', #61184, #10040, #8932 ) ;
#69791 = ORIENTED_EDGE ( 'NONE', *, *, #57126, .T. ) ;
#69792 = CARTESIAN_POINT ( 'NONE',  ( 95.00000000000000000, -212.6630814284392557, 82.97531250086714749 ) ) ;
#69793 = CARTESIAN_POINT ( 'NONE',  ( 22.94323693612312809, -114.6983135802921083, 5.500000000000000000 ) ) ;
#69794 = DIRECTION ( 'NONE',  ( 0.000000000000000000, 0.000000000000000000, 1.000000000000000000 ) ) ;
#69795 = CARTESIAN_POINT ( 'NONE',  ( 0.000000000000000000, 68.67312586195046720, -35.91791733033404199 ) ) ;
#69796 = DIRECTION ( 'NONE',  ( -1.000000000000000000, 0.000000000000000000, 0.000000000000000000 ) ) ;
#69797 = CARTESIAN_POINT ( 'NONE',  ( -6.782329983125270800, 10.49999999999999467, -125.0000000000000000 ) ) ;
#69798 = CARTESIAN_POINT ( 'NONE',  ( 96.32499999999998863, -212.2949673200287179, 86.40166666666667084 ) ) ;
#69799 = ORIENTED_EDGE ( 'NONE', *, *, #72700, .T. ) ;
#69800 = ORIENTED_EDGE ( 'NONE', *, *, #47644, .T. ) ;
#69801 = ORIENTED_EDGE ( 'NONE', *, *, #71131, .F. ) ;
#69802 = VERTEX_POINT ( 'NONE', #50442 ) ;
#69803 = DIRECTION ( 'NONE',  ( -0.7071067811865336949, 8.659560562355101724E-17, -0.7071067811865613395 ) ) ;
#69804 =( NAMED_UNIT ( * ) PLANE_ANGLE_UNIT ( ) SI_UNIT ( $, .RADIAN. ) );
#69805 = CARTESIAN_POINT ( 'NONE',  ( -93.84685191531252713, 88.00268892867056536, 86.20322916753382003 ) ) ;
#69806 = DIRECTION ( 'NONE',  ( -1.000000000000000000, 0.000000000000000000, -0.000000000000000000 ) ) ;
#69807 = CARTESIAN_POINT ( 'NONE',  ( -1.029419772574582836, -121.0910063848724718, 2.500000000000000000 ) ) ;
#69808 = CARTESIAN_POINT ( 'NONE',  ( 92.35000000000000853, -209.9999999999999716, 74.83937500173429669 ) ) ;
#69809 = CARTESIAN_POINT ( 'NONE',  ( 93.67499999999999716, 87.70503267997126784, 76.77083333333332860 ) ) ;
#69810 = VERTEX_POINT ( 'NONE', #10585 ) ;
#69811 = CARTESIAN_POINT ( 'NONE',  ( -97.64999999999996305, -209.9999999999999716, 88.17437500173430465 ) ) ;
#69812 = EDGE_CURVE ( 'NONE', #63658, #15051, #56086, .T. ) ;
#69813 = VERTEX_POINT ( 'NONE', #62104 ) ;
#69814 = CARTESIAN_POINT ( 'NONE',  ( 0.000000000000000000, 0.000000000000000000, -270.0000000000000000 ) ) ;
#69815 = ORIENTED_EDGE ( 'NONE', *, *, #65710, .T. ) ;
#69816 = CARTESIAN_POINT ( 'NONE',  ( 93.67499999999999716, 87.70503267997126784, 84.47020833506762472 ) ) ;
#69817 = CARTESIAN_POINT ( 'NONE',  ( 96.66077099052519372, 88.39973697852393286, 74.64190534806806454 ) ) ;
#69818 = VERTEX_POINT ( 'NONE', #73733 ) ;
#69819 = DIRECTION ( 'NONE',  ( 0.000000000000000000, 0.000000000000000000, 1.000000000000000000 ) ) ;
#69820 = LINE ( 'NONE', #70545, #67426 ) ;
#69821 = DIRECTION ( 'NONE',  ( -0.000000000000000000, -0.000000000000000000, 1.000000000000000000 ) ) ;
#69822 = AXIS2_PLACEMENT_3D ( 'NONE', #72958, #67716, #73710 ) ;
#69823 = FACE_OUTER_BOUND ( 'NONE', #48828, .T. ) ;
#69824 = ORIENTED_EDGE ( 'NONE', *, *, #66392, .T. ) ;
#69825 = DIRECTION ( 'NONE',  ( -1.000000000000000000, 0.000000000000000000, 0.000000000000000000 ) ) ;
#69826 = DIRECTION ( 'NONE',  ( -7.616308197390131428E-15, 1.000000000000000000, -2.546204323184492723E-14 ) ) ;
#69827 = ORIENTED_EDGE ( 'NONE', *, *, #6967, .T. ) ;
#69828 = CIRCLE ( 'NONE', #31403, 31.99999999999999289 ) ;
#69829 = ORIENTED_EDGE ( 'NONE', *, *, #5639, .F. ) ;
#69830 = ADVANCED_FACE ( 'NONE', ( #6804 ), #24468, .T. ) ;
#69831 = PLANE ( 'NONE',  #53010 ) ;
#69832 = ADVANCED_FACE ( 'NONE', ( #29717 ), #40546, .T. ) ;
#69833 = AXIS2_PLACEMENT_3D ( 'NONE', #29967, #42007, #7424 ) ;
#69834 = CARTESIAN_POINT ( 'NONE',  ( 0.000000000000000000, 23.16143007188532366, -73.95703589263949596 ) ) ;
#69835 = CARTESIAN_POINT ( 'NONE',  ( -92.35000000000005116, 91.52997821335253548, 75.20979166840096752 ) ) ;
#69836 = EDGE_LOOP ( 'NONE', ( #24323, #24761, #18752, #49650 ) ) ;
#69837 = CARTESIAN_POINT ( 'NONE',  ( -96.15314808468747287, -208.0026889286704943, 89.06072916753382174 ) ) ;
#69838 = ORIENTED_EDGE ( 'NONE', *, *, #21038, .T. ) ;
#69839 = CARTESIAN_POINT ( 'NONE',  ( 10.00000000000000000, 0.000000000000000000, 0.000000000000000000 ) ) ;
#69840 = ORIENTED_EDGE ( 'NONE', *, *, #26837, .T. ) ;
#69841 = EDGE_CURVE ( 'NONE', #66019, #68825, #53785, .T. ) ;
#69842 = ADVANCED_FACE ( 'NONE', ( #18448 ), #35730, .T. ) ;
#69843 = ORIENTED_EDGE ( 'NONE', *, *, #10166, .F. ) ;
#69844 = CARTESIAN_POINT ( 'NONE',  ( -23.50044424985128089, 0.001194404165009976208, -49.00000000000061107 ) ) ;
#69845 = AXIS2_PLACEMENT_3D ( 'NONE', #38579, #55495, #21258 ) ;
#69846 =( NAMED_UNIT ( * ) PLANE_ANGLE_UNIT ( ) SI_UNIT ( $, .RADIAN. ) );
#69847 = CARTESIAN_POINT ( 'NONE',  ( 92.69370383062498320, 91.33154071421968467, 80.06489583420047040 ) ) ;
#69848 = FACE_OUTER_BOUND ( 'NONE', #30798, .T. ) ;
#69849 = VECTOR ( 'NONE', #17446, 1000.000000000000000 ) ;
#69850 = CARTESIAN_POINT ( 'NONE',  ( -2.500000000000016431, -76.29999999999999716, -255.0000000000000000 ) ) ;
#69851 = CARTESIAN_POINT ( 'NONE',  ( -92.35000000000003695, 90.00000000000004263, 85.23749999999999716 ) ) ;
#69852 = DIRECTION ( 'NONE',  ( -1.000000000000000000, 0.000000000000000000, 0.000000000000000000 ) ) ;
#69853 = LINE ( 'NONE', #34917, #9206 ) ;
#69854 = LINE ( 'NONE', #19093, #65931 ) ;
#69855 = CARTESIAN_POINT ( 'NONE',  ( 0.000000000000000000, 26.50000000000000000, -1.500000000000001332 ) ) ;
#69856 =( BOUNDED_CURVE ( )  B_SPLINE_CURVE ( 2, ( #41639, #48391, #58948, #53297, #47655, #70559, #7801 ),
 .UNSPECIFIED., .F., .F. ) 
 B_SPLINE_CURVE_WITH_KNOTS ( ( 3, 2, 2, 3 ),
 ( 0.4791666666666668517, 0.4861111111111112160, 0.4930555555555556357, 0.5000000000000000000 ),
 .UNSPECIFIED. ) 
 CURVE ( )  GEOMETRIC_REPRESENTATION_ITEM ( )  RATIONAL_B_SPLINE_CURVE ( ( 0.9999999999999967804, 0.8660254037844419273, 1.000000000000000000, 0.8660254037844387076, 1.000000000000000000, 0.8660254037844387076, 1.000000000000000000 ) ) 
 REPRESENTATION_ITEM ( '' )  );
#69857 = EDGE_CURVE ( 'NONE', #26897, #56328, #69225, .T. ) ;
#69858 = CARTESIAN_POINT ( 'NONE',  ( -235.0000123116479926, -117.0000000000000142, 2.500000000000000000 ) ) ;
#69859 = PLANE ( 'NONE',  #58972 ) ;
#69860 = CARTESIAN_POINT ( 'NONE',  ( -92.69370383062504004, 90.00000000000004263, 85.51531250086713953 ) ) ;
#69861 = CARTESIAN_POINT ( 'NONE',  ( 0.000000000000000000, 0.000000000000000000, 125.0000000000000000 ) ) ;
#69863 = ADVANCED_FACE ( 'NONE', ( #58681 ), #69591, .F. ) ;
#69862 = DIRECTION ( 'NONE',  ( -0.000000000000000000, -0.000000000000000000, 1.000000000000000000 ) ) ;
#69864 = PRODUCT_DEFINITION_SHAPE ( 'NONE', 'NONE',  #74366 ) ;
#69865 = VERTEX_POINT ( 'NONE', #36114 ) ;
#69866 = CARTESIAN_POINT ( 'NONE',  ( 0.000000000000000000, -74.18225833017913828, 34.94270380257611208 ) ) ;
#69867 = EDGE_CURVE ( 'NONE', #1870, #66997, #6938, .T. ) ;
#69868 = CARTESIAN_POINT ( 'NONE',  ( 93.67499999999998295, 92.29496732002878900, 85.44916666666665606 ) ) ;
#69869 = CARTESIAN_POINT ( 'NONE',  ( 96.32499999999997442, 92.29496732002878900, 77.08833333333332405 ) ) ;
#69870 = AXIS2_PLACEMENT_3D ( 'NONE', #66523, #37582, #60518 ) ;
#69871 = DIRECTION ( 'NONE',  ( 1.390371824233641368E-16, -1.000000000000000000, 0.000000000000000000 ) ) ;
#69872 = CARTESIAN_POINT ( 'NONE',  ( 92.69370383062501162, -209.9999999999999716, 81.54656250086715374 ) ) ;
#69873 = AXIS2_PLACEMENT_3D ( 'NONE', #6357, #40193, #29257 ) ;
#69874 = ORIENTED_EDGE ( 'NONE', *, *, #47381, .T. ) ;
#69875 = ORIENTED_EDGE ( 'NONE', *, *, #28494, .F. ) ;
#69876 = CARTESIAN_POINT ( 'NONE',  ( 11.99999999999999822, 46.53671651293948486, 59.03961581697416250 ) ) ;
#69877 = ORIENTED_EDGE ( 'NONE', *, *, #46316, .F. ) ;
#69878 = CARTESIAN_POINT ( 'NONE',  ( 0.000000000000000000, -1.467624384280027838, 2.542000000000001592 ) ) ;
#69879 = CIRCLE ( 'NONE', #39915, 12.49999999999999645 ) ;
#69880 = CARTESIAN_POINT ( 'NONE',  ( 11.99999999999999822, 0.000000000000000000, 0.000000000000000000 ) ) ;
#69881 = EDGE_LOOP ( 'NONE', ( #31486, #1453, #49106, #4597 ) ) ;
#69882 = CARTESIAN_POINT ( 'NONE',  ( 93.84685191531249870, -208.0026889286704943, 78.26572916753382003 ) ) ;
#69883 = ORIENTED_EDGE ( 'NONE', *, *, #69953, .F. ) ;
#69884 = DIRECTION ( 'NONE',  ( -1.000000000000000000, -0.000000000000000000, 0.000000000000000000 ) ) ;
#69885 = ORIENTED_EDGE ( 'NONE', *, *, #44168, .F. ) ;
#69886 = CIRCLE ( 'NONE', #29104, 31.99999999999999289 ) ;
#69887 = ORIENTED_EDGE ( 'NONE', *, *, #62590, .F. ) ;
#69888 = DIRECTION ( 'NONE',  ( 0.000000000000000000, 0.000000000000000000, -1.000000000000000000 ) ) ;
#69889 = AXIS2_PLACEMENT_3D ( 'NONE', #37390, #48287, #71944 ) ;
#69890 = SURFACE_STYLE_USAGE ( .BOTH. , #12747 ) ;
#69891 = CARTESIAN_POINT ( 'NONE',  ( 11.99999999999999822, -55.20638768913724448, -51.02545421589383068 ) ) ;
#69892 = VERTEX_POINT ( 'NONE', #52296 ) ;
#69893 = CARTESIAN_POINT ( 'NONE',  ( 0.000000000000000000, -120.0000000000000000, 5.500000000000000000 ) ) ;
#69894 = CARTESIAN_POINT ( 'NONE',  ( 92.35000000000002274, -208.4700217866474645, 87.48645833506763836 ) ) ;
#69895 = CARTESIAN_POINT ( 'NONE',  ( 92.34999999999999432, 88.47002178664753558, 88.14791666666666003 ) ) ;
#69896 = ORIENTED_EDGE ( 'NONE', *, *, #66878, .F. ) ;
#69897 = DIRECTION ( 'NONE',  ( -1.000000000000000000, 0.000000000000000000, 0.000000000000000000 ) ) ;
#69898 = CARTESIAN_POINT ( 'NONE',  ( 10.00000000000000000, 68.67312586195046720, -35.91791733033402068 ) ) ;
#69899 = ADVANCED_FACE ( 'NONE', ( #23724 ), #24832, .T. ) ;
#69900 = ORIENTED_EDGE ( 'NONE', *, *, #30615, .F. ) ;
#69901 = ORIENTED_EDGE ( 'NONE', *, *, #65178, .F. ) ;
#69902 = DIRECTION ( 'NONE',  ( 0.000000000000000000, 0.000000000000000000, 1.000000000000000000 ) ) ;
#69903 = ORIENTED_EDGE ( 'NONE', *, *, #26337, .F. ) ;
#69904 = CARTESIAN_POINT ( 'NONE',  ( 92.34999999999999432, 90.00000000000002842, 85.63437500173431260 ) ) ;
#69905 = VERTEX_POINT ( 'NONE', #1581 ) ;
#69906 = VERTEX_POINT ( 'NONE', #1218 ) ;
#69907 = CARTESIAN_POINT ( 'NONE',  ( -2.499999999999965361, 90.00000000000000000, -90.00000000000000000 ) ) ;
#69908 = DIRECTION ( 'NONE',  ( -1.000000000000000000, 0.000000000000000000, 0.000000000000000000 ) ) ;
#69910 = EDGE_CURVE ( 'NONE', #29541, #21517, #59760, .T. ) ;
#69909 = ORIENTED_EDGE ( 'NONE', *, *, #57724, .F. ) ;
#69911 = ORIENTED_EDGE ( 'NONE', *, *, #42130, .T. ) ;
#69912 = ORIENTED_EDGE ( 'NONE', *, *, #65946, .F. ) ;
#69913 = CARTESIAN_POINT ( 'NONE',  ( 0.000000000000000000, 2.663952781846149254, 41.91543099594818500 ) ) ;
#69914 = EDGE_CURVE ( 'NONE', #66826, #71364, #17712, .T. ) ;
#69915 = LINE ( 'NONE', #53014, #20490 ) ;
#69916 = CARTESIAN_POINT ( 'NONE',  ( -97.65000000000001990, 90.00000000000004263, 87.45999999999999375 ) ) ;
#69917 = EDGE_LOOP ( 'NONE', ( #38594, #4725, #27542, #16935 ) ) ;
#69918 = CARTESIAN_POINT ( 'NONE',  ( 10.00000000000000000, 0.000000000000000000, 0.000000000000000000 ) ) ;
#69919 = CARTESIAN_POINT ( 'NONE',  ( 6.377742925735834234, -145.7647898336708181, -5.500000000000000000 ) ) ;
#69920 = VERTEX_POINT ( 'NONE', #470 ) ;
#69921 = CARTESIAN_POINT ( 'NONE',  ( 0.000000000000000000, -46.21855187248673502, 62.20884554314003623 ) ) ;
#69922 = CARTESIAN_POINT ( 'NONE',  ( -97.30629616937497417, -208.6684592857803011, 83.87489583420047268 ) ) ;
#69923 = ORIENTED_EDGE ( 'NONE', *, *, #30282, .T. ) ;
#69924 = CARTESIAN_POINT ( 'NONE',  ( 10.00000000000000000, -72.35432306680498016, 20.40083707022857951 ) ) ;
#69925 = CYLINDRICAL_SURFACE ( 'NONE', #9194, 82.00000000000000000 ) ;
#69926 = FACE_OUTER_BOUND ( 'NONE', #1234, .T. ) ;
#69927 = CARTESIAN_POINT ( 'NONE',  ( -96.15314808468745866, -211.9973110713294489, 75.77864583420047495 ) ) ;
#69928 = EDGE_CURVE ( 'NONE', #45497, #30067, #26293, .T. ) ;
#69929 = COLOUR_RGB ( '', 0.09019608, 0.27058824, 0.51372549) ;
#69930 = LINE ( 'NONE', #29698, #35559 ) ;
#69931 = CARTESIAN_POINT ( 'NONE',  ( 11.99999999999999822, -68.26794271651286294, 31.47745569255117104 ) ) ;
#69932 = CARTESIAN_POINT ( 'NONE',  ( 1.560000000000000053, -1.732050807568877859, -1.752539433813135784E-17 ) ) ;
#69933 = CARTESIAN_POINT ( 'NONE',  ( 10.00000000000000000, 0.000000000000000000, 0.000000000000000000 ) ) ;
#69934 = DIRECTION ( 'NONE',  ( 1.000000000000000000, 0.000000000000000000, 0.000000000000000000 ) ) ;
#69935 = VECTOR ( 'NONE', #54687, 1000.000000000000000 ) ;
#69936 = CARTESIAN_POINT ( 'NONE',  ( -92.69370383062502583, 91.33154071421968467, 79.21822916753380639 ) ) ;
#69937 = CARTESIAN_POINT ( 'NONE',  ( 0.000000000000000000, 33.17418723428307459, 17.67226234102837878 ) ) ;
#69938 = CARTESIAN_POINT ( 'NONE',  ( -3.000000000000000000, 0.000000000000000000, 0.000000000000000000 ) ) ;
#69939 = ADVANCED_FACE ( 'NONE', ( #34633 ), #35381, .T. ) ;
#69940 = CIRCLE ( 'NONE', #53103, 31.99999999999998224 ) ;
#69941 = EDGE_CURVE ( 'NONE', #6579, #64110, #20129, .T. ) ;
#69942 = DIRECTION ( 'NONE',  ( 0.000000000000000000, 0.000000000000000000, 1.000000000000000000 ) ) ;
#69943 = CIRCLE ( 'NONE', #67546, 5.000000000000000888 ) ;
#69944 = EDGE_CURVE ( 'NONE', #10200, #45901, #63601, .T. ) ;
#69945 = CARTESIAN_POINT ( 'NONE',  ( -5.000000000000000000, 2.886751345948137981, -5.553418012614792509 ) ) ;
#69946 = DIRECTION ( 'NONE',  ( -1.000000000000000000, 0.000000000000000000, 0.000000000000000000 ) ) ;
#69947 = VECTOR ( 'NONE', #11675, 999.9999999999998863 ) ;
#69948 = DIRECTION ( 'NONE',  ( -1.000000000000000000, 0.000000000000000000, 0.000000000000000000 ) ) ;
#69949 = DIRECTION ( 'NONE',  ( 0.000000000000000000, -0.9876883405951393247, 0.1564344650402205161 ) ) ;
#69950 = CARTESIAN_POINT ( 'NONE',  ( -96.32500000000001705, 92.29496732002878900, 87.43354166840096298 ) ) ;
#69951 = CARTESIAN_POINT ( 'NONE',  ( -94.99999999999997158, -212.6630814284392557, 77.26031250086714408 ) ) ;
#69952 = DIRECTION ( 'NONE',  ( -1.000000000000000000, 0.000000000000000000, 0.000000000000000000 ) ) ;
#69953 = EDGE_CURVE ( 'NONE', #34322, #70614, #16605, .T. ) ;
#69954 = EDGE_LOOP ( 'NONE', ( #26324, #37984, #6049, #60661 ) ) ;
#69955 = LINE ( 'NONE', #65452, #10721 ) ;
#69956 = CARTESIAN_POINT ( 'NONE',  ( -11.99999999999999645, 0.000000000000000000, 0.000000000000000000 ) ) ;
#69957 = CARTESIAN_POINT ( 'NONE',  ( -3.000000000000002665, 0.000000000000000000, 0.000000000000000000 ) ) ;
#69958 = CARTESIAN_POINT ( 'NONE',  ( 5.000000000000002665, -29.01471420065507090, -76.69515212746047439 ) ) ;
#69959 = CYLINDRICAL_SURFACE ( 'NONE', #16341, 21.00000000000000000 ) ;
#69960 = ORIENTED_EDGE ( 'NONE', *, *, #21387, .F. ) ;
#69961 = DIRECTION ( 'NONE',  ( 0.000000000000000000, 0.000000000000000000, -1.000000000000000000 ) ) ;
#69962 = CARTESIAN_POINT ( 'NONE',  ( 10.00000000000000000, 16.45098606841173705, -33.79645857604496229 ) ) ;
#69963 = ORIENTED_EDGE ( 'NONE', *, *, #7067, .F. ) ;
#69964 = CARTESIAN_POINT ( 'NONE',  ( 93.84685191531249870, -208.0026889286704943, 85.72697916753379843 ) ) ;
#69965 = DIRECTION ( 'NONE',  ( -1.000000000000000000, 3.061616997868382648E-16, 0.000000000000000000 ) ) ;
#69966 = EDGE_LOOP ( 'NONE', ( #72085, #49397, #3178, #19216, #50765, #3645, #38886, #69456, #23972, #1368, #46695, #26588 ) ) ;
#69967 = CARTESIAN_POINT ( 'NONE',  ( 95.00000000000000000, -207.3369185715606307, 89.00781250086716057 ) ) ;
#69968 = PRODUCT_DEFINITION_FORMATION_WITH_SPECIFIED_SOURCE ( 'ANY', '', #27159, .NOT_KNOWN. ) ;
#69969 = EDGE_LOOP ( 'NONE', ( #1708, #71793, #40397, #6776 ) ) ;
#69970 = DIRECTION ( 'NONE',  ( -1.000000000000000000, -0.000000000000000000, -0.000000000000000000 ) ) ;
#69971 = ORIENTED_EDGE ( 'NONE', *, *, #6451, .T. ) ;
#69972 = CARTESIAN_POINT ( 'NONE',  ( -93.84685191531252713, 88.00268892867056536, 81.12322916753382174 ) ) ;
#69973 = AXIS2_PLACEMENT_3D ( 'NONE', #48978, #14404, #2799 ) ;
#69974 = ORIENTED_EDGE ( 'NONE', *, *, #45943, .T. ) ;
#69975 = ORIENTED_EDGE ( 'NONE', *, *, #49957, .T. ) ;
#69976 = FACE_OUTER_BOUND ( 'NONE', #39059, .T. ) ;
#69977 =( BOUNDED_CURVE ( )  B_SPLINE_CURVE ( 2, ( #46350, #52724, #70360, #58360, #46722, #70739, #23781 ),
 .UNSPECIFIED., .F., .F. ) 
 B_SPLINE_CURVE_WITH_KNOTS ( ( 3, 2, 2, 3 ),
 ( 0.4791666666666668517, 0.4861111111111112160, 0.4930555555555556357, 0.5000000000000000000 ),
 .UNSPECIFIED. ) 
 CURVE ( )  GEOMETRIC_REPRESENTATION_ITEM ( )  RATIONAL_B_SPLINE_CURVE ( ( 0.9999999999999967804, 0.8660254037844419273, 1.000000000000000000, 0.8660254037844387076, 1.000000000000000000, 0.8660254037844387076, 1.000000000000000000 ) ) 
 REPRESENTATION_ITEM ( '' )  );
#69978 = ORIENTED_EDGE ( 'NONE', *, *, #68016, .F. ) ;
#69979 = CARTESIAN_POINT ( 'NONE',  ( 5.000000000000002665, -2.886751345948134873, -5.553418012614792509 ) ) ;
#69980 = DIRECTION ( 'NONE',  ( 1.000000000000000000, 0.000000000000000000, 0.000000000000000000 ) ) ;
#69981 = ORIENTED_EDGE ( 'NONE', *, *, #27333, .F. ) ;
#69982 = CARTESIAN_POINT ( 'NONE',  ( -10.00000000000000000, 0.000000000000000000, 0.000000000000000000 ) ) ;
#69983 = ORIENTED_EDGE ( 'NONE', *, *, #58220, .T. ) ;
#69984 = CARTESIAN_POINT ( 'NONE',  ( 11.99999999999999822, -50.95692526931372157, 58.39081064771733054 ) ) ;
#69985 = ORIENTED_EDGE ( 'NONE', *, *, #22323, .T. ) ;
#69986 = EDGE_CURVE ( 'NONE', #46835, #40961, #71418, .T. ) ;
#69987 = EDGE_CURVE ( 'NONE', #34202, #34378, #47838, .T. ) ;
#69988 = ORIENTED_EDGE ( 'NONE', *, *, #2782, .F. ) ;
#69989 = VECTOR ( 'NONE', #9007, 1000.000000000000000 ) ;
#69990 = ORIENTED_EDGE ( 'NONE', *, *, #58583, .T. ) ;
#69991 = CARTESIAN_POINT ( 'NONE',  ( 92.69370383062501162, -209.9999999999999716, 83.29281250086714294 ) ) ;
#69992 = AXIS2_PLACEMENT_3D ( 'NONE', #29254, #28518, #11973 ) ;
#69993 = DIRECTION ( 'NONE',  ( -1.000000000000000000, 0.000000000000000000, 0.000000000000000000 ) ) ;
#69994 = EDGE_CURVE ( 'NONE', #73774, #29448, #25027, .T. ) ;
#69995 = DIRECTION ( 'NONE',  ( -1.000000000000000000, 0.000000000000000000, 0.000000000000000000 ) ) ;
#69996 = DIRECTION ( 'NONE',  ( -1.000000000000000000, 0.000000000000000000, 0.000000000000000000 ) ) ;
#69997 = CARTESIAN_POINT ( 'NONE',  ( 2.499999999999984457, -73.00000000000001421, -255.0000000000000000 ) ) ;
#69998 = DIRECTION ( 'NONE',  ( 0.000000000000000000, 0.9238795325112877377, -0.3826834323650873948 ) ) ;
#69999 = EDGE_CURVE ( 'NONE', #16263, #4375, #49007, .T. ) ;
#70000 = DIRECTION ( 'NONE',  ( -1.000000000000000000, 0.000000000000000000, 0.000000000000000000 ) ) ;
#70001 = CARTESIAN_POINT ( 'NONE',  ( -97.30629616937495996, -209.9999999999999716, 83.92781250086714806 ) ) ;
#70002 = CARTESIAN_POINT ( 'NONE',  ( -95.00000000000002842, 87.33691857156074434, 82.34031250086714238 ) ) ;
#70003 = ORIENTED_EDGE ( 'NONE', *, *, #64960, .T. ) ;
#70004 = CARTESIAN_POINT ( 'NONE',  ( 94.99999999999998579, 87.33691857156068750, 81.54656250086715374 ) ) ;
#70005 = EDGE_CURVE ( 'NONE', #28647, #10445, #44250, .T. ) ;
#70006 = ORIENTED_EDGE ( 'NONE', *, *, #19196, .T. ) ;
#70007 = DIRECTION ( 'NONE',  ( -0.9848077530122080203, -0.1736481776669309696, 0.000000000000000000 ) ) ;
#70008 = LINE ( 'NONE', #19619, #46774 ) ;
#70009 = CARTESIAN_POINT ( 'NONE',  ( 0.000000000000000000, -120.0000000000000000, -2.500000000000000000 ) ) ;
#70010 = DIRECTION ( 'NONE',  ( -1.000000000000000000, 0.000000000000000000, 0.000000000000000000 ) ) ;
#70011 = CYLINDRICAL_SURFACE ( 'NONE', #17630, 31.99999999999999289 ) ;
#70012 = CARTESIAN_POINT ( 'NONE',  ( -96.15314808468745866, -211.9973110713294489, 85.30364583420046642 ) ) ;
#70013 = DIRECTION ( 'NONE',  ( 0.000000000000000000, 0.000000000000000000, 1.000000000000000000 ) ) ;
#70014 = CARTESIAN_POINT ( 'NONE',  ( 23.11608002360578240, -124.4885236261218182, 5.500000000000000000 ) ) ;
#70015 = CARTESIAN_POINT ( 'NONE',  ( -2.981742216678212820, 0.000000000000000000, -15.39727592608509177 ) ) ;
#70016 = CARTESIAN_POINT ( 'NONE',  ( 97.64999999999999147, -209.9999999999999716, 84.60249999999999204 ) ) ;
#70017 = ORIENTED_EDGE ( 'NONE', *, *, #45772, .T. ) ;
#70018 = EDGE_LOOP ( 'NONE', ( #5232, #64269, #33358, #52628 ) ) ;
#70019 = CARTESIAN_POINT ( 'NONE',  ( 12.00000000000000000, -22.67460108101782978, -6.353146135317906840 ) ) ;
#70020 = DIRECTION ( 'NONE',  ( 0.000000000000000000, 0.000000000000000000, 1.000000000000000000 ) ) ;
#70021 = CARTESIAN_POINT ( 'NONE',  ( -95.00000000000002842, 87.33691857156074434, 87.89656250086713385 ) ) ;
#70022 = LINE ( 'NONE', #68938, #69408 ) ;
#70023 = DIRECTION ( 'NONE',  ( -0.000000000000000000, -0.000000000000000000, -1.000000000000000000 ) ) ;
#70024 = APPLICATION_CONTEXT ( 'automotive_design' ) ;
#70025 = AXIS2_PLACEMENT_3D ( 'NONE', #32952, #15683, #14934 ) ;
#70026 = LINE ( 'NONE', #68941, #60142 ) ;
#70027 = CARTESIAN_POINT ( 'NONE',  ( 0.000000000000000000, -2.946379043145784582, -75.11764819372150725 ) ) ;
#70028 = VERTEX_POINT ( 'NONE', #27318 ) ;
#70029 = CARTESIAN_POINT ( 'NONE',  ( -96.15314808468752972, 91.99731107132950569, 76.20197916753380696 ) ) ;
#70030 = ORIENTED_EDGE ( 'NONE', *, *, #62508, .T. ) ;
#70031 = ADVANCED_FACE ( 'NONE', ( #38995 ), #7911, .T. ) ;
#70032 = ADVANCED_FACE ( 'NONE', ( #33324 ), #19556, .T. ) ;
#70033 = CARTESIAN_POINT ( 'NONE',  ( 92.48632958231168288, -210.0000000000000284, 74.91808492278046572 ) ) ;
#70034 = CIRCLE ( 'NONE', #37635, 77.49899999999999523 ) ;
#70035 = DIRECTION ( 'NONE',  ( 0.000000000000000000, -0.9876883405951358830, -0.1564344650402421932 ) ) ;
#70036 = FACE_OUTER_BOUND ( 'NONE', #60409, .T. ) ;
#70037 = DIRECTION ( 'NONE',  ( -1.000000000000000000, 0.000000000000000000, -0.000000000000000000 ) ) ;
#70038 = CARTESIAN_POINT ( 'NONE',  ( -92.69370383062498320, -208.6684592857803011, 85.72697916753381264 ) ) ;
#70039 =( NAMED_UNIT ( * ) PLANE_ANGLE_UNIT ( ) SI_UNIT ( $, .RADIAN. ) );
#70040 = CARTESIAN_POINT ( 'NONE',  ( 15.00000000000000000, 14.60985201121729737, 18.46759930825687235 ) ) ;
#70041 = EDGE_CURVE ( 'NONE', #3791, #7308, #65073, .T. ) ;
#70042 = CIRCLE ( 'NONE', #56812, 31.99999999999998224 ) ;
#70043 = AXIS2_PLACEMENT_3D ( 'NONE', #7552, #48507, #25939 ) ;
#70044 = CARTESIAN_POINT ( 'NONE',  ( 96.15314808468748708, 88.00268892867053694, 75.40822916753381833 ) ) ;
#70045 = CARTESIAN_POINT ( 'NONE',  ( -96.15314808468747287, -208.0026889286704943, 75.09072916753380866 ) ) ;
#70046 = DIRECTION ( 'NONE',  ( 0.000000000000000000, -0.5877852522924624790, -0.8090169943749553338 ) ) ;
#70047 = EDGE_LOOP ( 'NONE', ( #62803, #912, #29288, #1239 ) ) ;
#70048 = DIRECTION ( 'NONE',  ( -1.000000000000000000, -0.000000000000000000, -0.000000000000000000 ) ) ;
#70049 = CYLINDRICAL_SURFACE ( 'NONE', #34644, 82.00000000000000000 ) ;
#70050 = DIRECTION ( 'NONE',  ( 1.000000000000000000, 0.000000000000000000, 0.000000000000000000 ) ) ;
#70051 = VECTOR ( 'NONE', #67179, 1000.000000000000000 ) ;
#70052 = AXIS2_PLACEMENT_3D ( 'NONE', #60898, #9016, #4142 ) ;
#70053 = AXIS2_PLACEMENT_3D ( 'NONE', #3683, #49514, #32587 ) ;
#70054 = CARTESIAN_POINT ( 'NONE',  ( -93.84685191531254134, 91.99731107132950569, 74.98489583420048632 ) ) ;
#70055 = CARTESIAN_POINT ( 'NONE',  ( 97.30629616937498838, -211.3315407142195852, 76.57239583420046358 ) ) ;
#70056 = VERTEX_POINT ( 'NONE', #10039 ) ;
#70057 = DIRECTION ( 'NONE',  ( 0.000000000000000000, 0.000000000000000000, 1.000000000000000000 ) ) ;
#70058 = ORIENTED_EDGE ( 'NONE', *, *, #47709, .F. ) ;
#70059 = DIRECTION ( 'NONE',  ( 1.000000000000000000, 0.000000000000000000, 0.000000000000000000 ) ) ;
#70060 = VERTEX_POINT ( 'NONE', #44643 ) ;
#70061 = CIRCLE ( 'NONE', #12434, 77.49900000000000944 ) ;
#70062 = CARTESIAN_POINT ( 'NONE',  ( -92.35000000000547971, -210.0000054026037049, 81.50687481489497088 ) ) ;
#70063 = ORIENTED_EDGE ( 'NONE', *, *, #46316, .T. ) ;
#70064 = ORIENTED_EDGE ( 'NONE', *, *, #69416, .T. ) ;
#70065 = VERTEX_POINT ( 'NONE', #72800 ) ;
#70066 = CARTESIAN_POINT ( 'NONE',  ( 92.35000000021534561, -209.9999789922616458, 79.91868729553134187 ) ) ;
#70067 = VERTEX_POINT ( 'NONE', #14290 ) ;
#70068 = CIRCLE ( 'NONE', #60493, 31.99999999999999289 ) ;
#70069 = ORIENTED_EDGE ( 'NONE', *, *, #26567, .T. ) ;
#70070 =( BOUNDED_CURVE ( )  B_SPLINE_CURVE ( 2, ( #23158, #62652, #38961, #5504, #17503, #4768, #22791 ),
 .UNSPECIFIED., .F., .F. ) 
 B_SPLINE_CURVE_WITH_KNOTS ( ( 3, 2, 2, 3 ),
 ( 0.5080151867253831499, 0.5150708844844119616, 0.5221266500252946807, 0.5291824299508944840 ),
 .UNSPECIFIED. ) 
 CURVE ( )  GEOMETRIC_REPRESENTATION_ITEM ( )  RATIONAL_B_SPLINE_CURVE ( ( 0.9999974259464162740, 0.8660266908235946248, 1.000000000000000000, 0.8660254037844387076, 1.000000000000000000, 0.8660254037844387076, 1.000000000000000000 ) ) 
 REPRESENTATION_ITEM ( '' )  );
#70071 = CARTESIAN_POINT ( 'NONE',  ( 92.69370383062498320, 91.33154071421968467, 80.85864583420048746 ) ) ;
#70072 = LINE ( 'NONE', #18575, #67182 ) ;
#70073 = LINE ( 'NONE', #12571, #59678 ) ;
#70074 = VERTEX_POINT ( 'NONE', #50251 ) ;
#70075 = AXIS2_PLACEMENT_3D ( 'NONE', #49689, #61739, #21123 ) ;
#70076 = EDGE_LOOP ( 'NONE', ( #30140, #15237, #29228, #56733 ) ) ;
#70077 = EDGE_LOOP ( 'NONE', ( #45140, #54927, #22585, #21724 ) ) ;
#70078 = CARTESIAN_POINT ( 'NONE',  ( 22.94323693612312809, -114.6983135802921083, 5.500000000000000000 ) ) ;
#70079 = ORIENTED_EDGE ( 'NONE', *, *, #11426, .F. ) ;
#70080 = CIRCLE ( 'NONE', #67685, 21.00000000000000000 ) ;
#70081 = DIRECTION ( 'NONE',  ( -1.000000000000000000, 0.000000000000000000, 0.000000000000000000 ) ) ;
#70082 = EDGE_CURVE ( 'NONE', #65052, #33844, #36997, .T. ) ;
#70083 = CARTESIAN_POINT ( 'NONE',  ( -2.459674775249774736, -1.719108899120391569E-13, -15.80000000000028670 ) ) ;
#70084 = DIRECTION ( 'NONE',  ( 0.000000000000000000, -0.4539904997395351471, -0.8910065241883737830 ) ) ;
#70085 = DIRECTION ( 'NONE',  ( 0.000000000000000000, 0.1564344650402312020, -0.9876883405951376593 ) ) ;
#70086 = CYLINDRICAL_SURFACE ( 'NONE', #8362, 12.50000000000000000 ) ;
#70087 = DIRECTION ( 'NONE',  ( -1.000000000000000000, -0.000000000000000000, 0.000000000000000000 ) ) ;
#70088 = ADVANCED_FACE ( 'NONE', ( #38623 ), #30830, .T. ) ;
#70089 = CARTESIAN_POINT ( 'NONE',  ( -92.34999999999999432, -208.4700217866474645, 78.38479166840096468 ) ) ;
#70090 = EDGE_LOOP ( 'NONE', ( #57061, #30319, #35746, #61062 ) ) ;
#70091 = CARTESIAN_POINT ( 'NONE',  ( -100.0000000000260485, 95.00000000000001421, -65.00000000000001421 ) ) ;
#70092 = ORIENTED_EDGE ( 'NONE', *, *, #6547, .T. ) ;
#70094 = CARTESIAN_POINT ( 'NONE',  ( -93.67500000000003979, 92.29496732002878900, 75.26270833506764291 ) ) ;
#70093 = CARTESIAN_POINT ( 'NONE',  ( 97.64999999999997726, 88.47002178664753558, 80.81895833506764859 ) ) ;
#70095 = EDGE_CURVE ( 'NONE', #35854, #23517, #60181, .T. ) ;
#70096 = ORIENTED_EDGE ( 'NONE', *, *, #36227, .T. ) ;
#70097 = CARTESIAN_POINT ( 'NONE',  ( 96.15314808468748708, 91.99731107132950569, 80.69989583420047552 ) ) ;
#70098 = AXIS2_PLACEMENT_3D ( 'NONE', #56944, #5452, #40019 ) ;
#70099 = LINE ( 'NONE', #18600, #44566 ) ;
#70100 = DIRECTION ( 'NONE',  ( -1.000000000000000000, 0.000000000000000000, 0.000000000000000000 ) ) ;
#70101 = CARTESIAN_POINT ( 'NONE',  ( -10.00000000000000000, 0.000000000000000000, 0.000000000000000000 ) ) ;
#70102 = CARTESIAN_POINT ( 'NONE',  ( -1.233757462863590115, -120.8531368722710795, 2.500000000000000000 ) ) ;
#70103 = ORIENTED_EDGE ( 'NONE', *, *, #19503, .T. ) ;
#70105 = CARTESIAN_POINT ( 'NONE',  ( 0.000000000000000000, 0.000000000000000000, -5.624496230895140947 ) ) ;
#70104 = VECTOR ( 'NONE', #11422, 1000.000000000000114 ) ;
#70106 = VECTOR ( 'NONE', #43624, 1000.000000000000000 ) ;
#70107 = CARTESIAN_POINT ( 'NONE',  ( -0.8192951148925873284, 5.300482436767278926, -5.801655677627841179 ) ) ;
#70108 = VERTEX_POINT ( 'NONE', #13548 ) ;
#70109 = ORIENTED_EDGE ( 'NONE', *, *, #58078, .T. ) ;
#70110 = EDGE_CURVE ( 'NONE', #57325, #50561, #58616, .T. ) ;
#70111 = EDGE_CURVE ( 'NONE', #65017, #51207, #62323, .T. ) ;
#70112 = CYLINDRICAL_SURFACE ( 'NONE', #8113, 31.99999999999998579 ) ;
#70113 = DIRECTION ( 'NONE',  ( 0.000000000000000000, 0.000000000000000000, 1.000000000000000000 ) ) ;
#70114 = DIRECTION ( 'NONE',  ( 0.000000000000000000, 0.000000000000000000, -1.000000000000000000 ) ) ;
#70115 = CARTESIAN_POINT ( 'NONE',  ( -97.30629616937497417, -208.6684592857803011, 77.68364583420047609 ) ) ;
#70116 = ORIENTED_EDGE ( 'NONE', *, *, #27410, .F. ) ;
#70117 = AXIS2_PLACEMENT_3D ( 'NONE', #38849, #51234, #55771 ) ;
#70118 = CARTESIAN_POINT ( 'NONE',  ( 5.000000000000000000, -27.74655509720725988, 77.16300072079653205 ) ) ;
#70119 = EDGE_CURVE ( 'NONE', #12142, #34299, #32594, .T. ) ;
#70120 = ADVANCED_FACE ( 'NONE', ( #44260 ), #15685, .T. ) ;
#70121 = LINE ( 'NONE', #47943, #45088 ) ;
#70122 = CARTESIAN_POINT ( 'NONE',  ( 5.999999999999999112, 21.60688246758697062, -79.10210256391344785 ) ) ;
#70123 = CARTESIAN_POINT ( 'NONE',  ( 11.99999999999999822, -73.44644590900077219, 24.73286445877677764 ) ) ;
#70124 = CARTESIAN_POINT ( 'NONE',  ( 0.000000000000000000, -72.35160999960801576, -20.41045688087902121 ) ) ;
#70125 = DIRECTION ( 'NONE',  ( 0.000000000000000000, 0.000000000000000000, 1.000000000000000000 ) ) ;
#70126 = DIRECTION ( 'NONE',  ( 0.7585478161175723821, 0.6516173805718057377, 0.000000000000000000 ) ) ;
#70127 = DIRECTION ( 'NONE',  ( -1.000000000000000000, 0.000000000000000000, 0.000000000000000000 ) ) ;
#70128 = CARTESIAN_POINT ( 'NONE',  ( -97.64999999999986358, -211.5299782133524502, 76.08291666666664810 ) ) ;
#70129 = LINE ( 'NONE', #63783, #65816 ) ;
#70130 = VECTOR ( 'NONE', #72780, 1000.000000000000114 ) ;
#70131 = CARTESIAN_POINT ( 'NONE',  ( 93.84685191531248449, 88.00268892867053694, 88.00239583420048461 ) ) ;
#70132 = CARTESIAN_POINT ( 'NONE',  ( -97.30629616937497417, -211.3315407142195852, 85.40947916753381719 ) ) ;
#70133 = CARTESIAN_POINT ( 'NONE',  ( 92.35000000007821086, 90.00001303125209517, 79.28395951162845279 ) ) ;
#70134 = ORIENTED_EDGE ( 'NONE', *, *, #60885, .F. ) ;
#70135 = CARTESIAN_POINT ( 'NONE',  ( 93.67500000000001137, -212.2949673200287179, 83.20020833506764291 ) ) ;
#70136 = CARTESIAN_POINT ( 'NONE',  ( -94.99999999999997158, -213.0599564267049857, 82.53874999999999318 ) ) ;
#70137 = CARTESIAN_POINT ( 'NONE',  ( -92.69370383062505425, 91.33154071421968467, 76.04322916753380923 ) ) ;
#70138 = AXIS2_PLACEMENT_3D ( 'NONE', #69893, #41696, #47706 ) ;
#70139 = CARTESIAN_POINT ( 'NONE',  ( 95.00000000000000000, -207.3369185715606307, 88.84906250086713442 ) ) ;
#70140 = ORIENTED_EDGE ( 'NONE', *, *, #58458, .F. ) ;
#70141 = ORIENTED_EDGE ( 'NONE', *, *, #31977, .F. ) ;
#70142 = CIRCLE ( 'NONE', #66565, 16.00000000000000000 ) ;
#70143 = VECTOR ( 'NONE', #58321, 1000.000000000000000 ) ;
#70144 = ORIENTED_EDGE ( 'NONE', *, *, #7414, .F. ) ;
#70145 = DIRECTION ( 'NONE',  ( 0.000000000000000000, 0.8910065241883657894, 0.4539904997395509678 ) ) ;
#70146 = CONICAL_SURFACE ( 'NONE', #5361, 62.50000000000000000, 0.7853981633974497223 ) ;
#70147 = FACE_OUTER_BOUND ( 'NONE', #63859, .T. ) ;
#70148 = ORIENTED_EDGE ( 'NONE', *, *, #35715, .F. ) ;
#70149 = ORIENTED_EDGE ( 'NONE', *, *, #71380, .T. ) ;
#70150 = CARTESIAN_POINT ( 'NONE',  ( 93.84685191531251292, -211.9973110713294489, 81.65239583420049030 ) ) ;
#70151 = CARTESIAN_POINT ( 'NONE',  ( 10.00000000000000000, 0.000000000000000000, 0.000000000000000000 ) ) ;
#70152 = DIRECTION ( 'NONE',  ( 1.000000000000000000, 0.000000000000000000, 0.000000000000000000 ) ) ;
#70153 = EDGE_CURVE ( 'NONE', #51981, #18300, #26200, .T. ) ;
#70154 = FACE_OUTER_BOUND ( 'NONE', #64158, .T. ) ;
#70155 = CARTESIAN_POINT ( 'NONE',  ( 0.000000000000000000, -41.76937507738745836, -62.50329211542482710 ) ) ;
#70156 = DIRECTION ( 'NONE',  ( 0.000000000000000000, 0.000000000000000000, 1.000000000000000000 ) ) ;
#70157 = CARTESIAN_POINT ( 'NONE',  ( 92.35000000000002274, -211.5299782133524502, 84.33791666666667197 ) ) ;
#70158 = EDGE_CURVE ( 'NONE', #48627, #60292, #294, .T. ) ;
#70159 = ORIENTED_EDGE ( 'NONE', *, *, #17879, .F. ) ;
#70160 = VERTEX_POINT ( 'NONE', #39365 ) ;
#70161 = ORIENTED_EDGE ( 'NONE', *, *, #4948, .T. ) ;
#70162 = EDGE_LOOP ( 'NONE', ( #31249, #14901, #39019, #2031 ) ) ;
#70163 = CARTESIAN_POINT ( 'NONE',  ( 99.99999999999998579, 80.00000000000000000, -90.00000000000000000 ) ) ;
#70164 = CARTESIAN_POINT ( 'NONE',  ( -97.30629616937501680, 91.33154071421968467, 89.11364583420049712 ) ) ;
#70165 = EDGE_CURVE ( 'NONE', #28591, #20602, #22626, .T. ) ;
#70166 = DIRECTION ( 'NONE',  ( 0.000000000000000000, 0.000000000000000000, 1.000000000000000000 ) ) ;
#70167 = CARTESIAN_POINT ( 'NONE',  ( 97.64999999999999147, -209.9999999999999716, 78.33187500173430351 ) ) ;
#70168 = CARTESIAN_POINT ( 'NONE',  ( 92.69370383062501162, -209.9999999999999716, 87.73781250086713612 ) ) ;
#70169 = CARTESIAN_POINT ( 'NONE',  ( 97.64999999999997726, 88.47002178664753558, 78.19958333333332234 ) ) ;
#70171 = VERTEX_POINT ( 'NONE', #28818 ) ;
#70170 = EDGE_CURVE ( 'NONE', #23048, #50573, #64634, .T. ) ;
#70172 = CARTESIAN_POINT ( 'NONE',  ( -97.64999999999994884, -208.4700217866474645, 88.75645833506762017 ) ) ;
#70173 = ORIENTED_EDGE ( 'NONE', *, *, #27075, .T. ) ;
#70174 = CARTESIAN_POINT ( 'NONE',  ( 95.00000000000000000, -213.0599564267049857, 79.99874999999998693 ) ) ;
#70175 = EDGE_LOOP ( 'NONE', ( #67803, #15729, #65033, #72292 ) ) ;
#70176 = CARTESIAN_POINT ( 'NONE',  ( -97.65000000000001990, 91.52997821335253548, 86.21645833506764234 ) ) ;
#70177 = EDGE_CURVE ( 'NONE', #36328, #44183, #34834, .T. ) ;
#70178 = CARTESIAN_POINT ( 'NONE',  ( 93.84685191531248449, 91.99731107132950569, 75.56697916753381605 ) ) ;
#70179 = VERTEX_POINT ( 'NONE', #51747 ) ;
#70180 = CARTESIAN_POINT ( 'NONE',  ( 20.85212586905261745, -130.9402397935870965, -2.500000000000000000 ) ) ;
#70181 = DIRECTION ( 'NONE',  ( 0.000000000000000000, 0.000000000000000000, 1.000000000000000000 ) ) ;
#70182 = DIRECTION ( 'NONE',  ( -1.000000000000000000, 0.000000000000000000, -0.000000000000000000 ) ) ;
#70183 = DIRECTION ( 'NONE',  ( 1.000000000000000000, 0.000000000000000000, 0.000000000000000000 ) ) ;
#70184 = VERTEX_POINT ( 'NONE', #23188 ) ;
#70185 = CARTESIAN_POINT ( 'NONE',  ( -7.469491406282117829, 4.756046723998917258, -64.01812422950395387 ) ) ;
#70186 = CARTESIAN_POINT ( 'NONE',  ( -96.32500000000001705, 92.29496732002878900, 81.71854166840095957 ) ) ;
#70187 = AXIS2_PLACEMENT_3D ( 'NONE', #57431, #45424, #33752 ) ;
#70188 = ORIENTED_EDGE ( 'NONE', *, *, #32172, .F. ) ;
#70189 = ORIENTED_EDGE ( 'NONE', *, *, #235, .F. ) ;
#70190 = DIRECTION ( 'NONE',  ( -1.000000000000000000, 0.000000000000000000, 0.000000000000000000 ) ) ;
#70191 = EDGE_CURVE ( 'NONE', #41093, #47282, #32205, .T. ) ;
#70192 = ADVANCED_FACE ( 'NONE', ( #5907 ), #58127, .T. ) ;
#70193 = DIRECTION ( 'NONE',  ( 1.000000000000000000, 0.000000000000000000, 0.000000000000000000 ) ) ;
#70194 = DIRECTION ( 'NONE',  ( 1.000000000000000000, 0.000000000000000000, 0.000000000000000000 ) ) ;
#70195 = ORIENTED_EDGE ( 'NONE', *, *, #48352, .F. ) ;
#70196 = CARTESIAN_POINT ( 'NONE',  ( -94.99999999999997158, -207.3369185715606307, 89.00781250086716057 ) ) ;
#70197 = VERTEX_POINT ( 'NONE', #40464 ) ;
#70198 = CIRCLE ( 'NONE', #61849, 82.00000000000000000 ) ;
#70199 = CARTESIAN_POINT ( 'NONE',  ( 94.99999999999998579, 90.00000000000002842, 90.00000000000000000 ) ) ;
#70200 = CIRCLE ( 'NONE', #25934, 31.99999999999998579 ) ;
#70201 = ORIENTED_EDGE ( 'NONE', *, *, #3990, .F. ) ;
#70202 = ORIENTED_EDGE ( 'NONE', *, *, #40937, .F. ) ;
#70203 = CARTESIAN_POINT ( 'NONE',  ( 0.000000000000000000, 37.58145647212453611, 16.68533520207917675 ) ) ;
#70204 = CIRCLE ( 'NONE', #65405, 16.00000000000000000 ) ;
#70205 = CARTESIAN_POINT ( 'NONE',  ( 0.000000000000000000, -18.89407956138204980, -75.16055320797050854 ) ) ;
#70206 = CARTESIAN_POINT ( 'NONE',  ( 96.15314808468748708, 91.99731107132950569, 81.81114583420047381 ) ) ;
#70207 = DIRECTION ( 'NONE',  ( 0.000000000000000000, 0.000000000000000000, 1.000000000000000000 ) ) ;
#70208 = DIRECTION ( 'NONE',  ( 0.000000000000000000, 0.000000000000000000, 1.000000000000000000 ) ) ;
#70209 = CARTESIAN_POINT ( 'NONE',  ( -92.35000000000003695, 90.00000000000004263, 80.79249999999998977 ) ) ;
#70210 = CARTESIAN_POINT ( 'NONE',  ( 0.000000000000000000, -25.88420570971419821, 27.13269053701087330 ) ) ;
#70211 = DIRECTION ( 'NONE',  ( 0.000000000000000000, 0.000000000000000000, 1.000000000000000000 ) ) ;
#70212 = DIRECTION ( 'NONE',  ( 0.000000000000000000, 0.1564344650402312298, -0.9876883405951375483 ) ) ;
#70213 = CARTESIAN_POINT ( 'NONE',  ( 97.65000000000006253, 88.47002178664756400, 83.91458333333333997 ) ) ;
#70214 = FACE_OUTER_BOUND ( 'NONE', #26131, .T. ) ;
#70215 = AXIS2_PLACEMENT_3D ( 'NONE', #13701, #24989, #41545 ) ;
#70216 = FACE_OUTER_BOUND ( 'NONE', #18618, .T. ) ;
#70217 = CARTESIAN_POINT ( 'NONE',  ( -92.69370383062505425, 91.33154071421968467, 84.93322916753379559 ) ) ;
#70218 = LINE ( 'NONE', #20203, #11914 ) ;
#70219 = AXIS2_PLACEMENT_3D ( 'NONE', #45285, #23814, #40005 ) ;
#70220 = CYLINDRICAL_SURFACE ( 'NONE', #18029, 2.649999999999985700 ) ;
#70221 = ORIENTED_EDGE ( 'NONE', *, *, #20605, .F. ) ;
#70222 = DIRECTION ( 'NONE',  ( -1.000000000000000000, -0.000000000000000000, 0.000000000000000000 ) ) ;
#70223 = DIRECTION ( 'NONE',  ( 1.000000000000000000, -0.000000000000000000, -0.000000000000000000 ) ) ;
#70224 = DIRECTION ( 'NONE',  ( 0.000000000000000000, 0.000000000000000000, 1.000000000000000000 ) ) ;
#70225 = ADVANCED_FACE ( 'NONE', ( #63414 ), #40852, .T. ) ;
#70226 = LINE ( 'NONE', #64613, #15208 ) ;
#70227 = AXIS2_PLACEMENT_3D ( 'NONE', #44592, #33663, #38941 ) ;
#70228 = CARTESIAN_POINT ( 'NONE',  ( 95.00000000000000000, -212.6630814284392557, 81.70531250086715147 ) ) ;
#70229 = ORIENTED_EDGE ( 'NONE', *, *, #68826, .F. ) ;
#70230 = EDGE_CURVE ( 'NONE', #2928, #42628, #21448, .T. ) ;
#70231 = ORIENTED_EDGE ( 'NONE', *, *, #59933, .F. ) ;
#70232 = EDGE_CURVE ( 'NONE', #21904, #66208, #19010, .T. ) ;
#70233 = DIRECTION ( 'NONE',  ( -1.000000000000000000, 0.000000000000000000, 0.000000000000000000 ) ) ;
#70234 = EDGE_LOOP ( 'NONE', ( #41226, #26895, #19596, #20989 ) ) ;
#70235 = CARTESIAN_POINT ( 'NONE',  ( 0.000000000000000000, -14.54903810567645372, -22.19967320028775504 ) ) ;
#70236 = DIRECTION ( 'NONE',  ( -1.000000000000000000, 0.000000000000000000, 0.000000000000000000 ) ) ;
#70237 = VECTOR ( 'NONE', #64166, 1000.000000000000000 ) ;
#70238 = VERTEX_POINT ( 'NONE', #55350 ) ;
#70239 = AXIS2_PLACEMENT_3D ( 'NONE', #14706, #49287, #43674 ) ;
#70240 = CARTESIAN_POINT ( 'NONE',  ( 96.15314808468750130, -211.9973110713294489, 77.94822916753382458 ) ) ;
#70241 = EDGE_CURVE ( 'NONE', #56774, #72774, #30974, .T. ) ;
#70242 = VERTEX_POINT ( 'NONE', #54259 ) ;
#70243 = FACE_OUTER_BOUND ( 'NONE', #73488, .T. ) ;
#70244 = ORIENTED_EDGE ( 'NONE', *, *, #15956, .T. ) ;
#70245 = CIRCLE ( 'NONE', #34257, 31.99999999999999289 ) ;
#70246 = ORIENTED_EDGE ( 'NONE', *, *, #73424, .T. ) ;
#70247 = CARTESIAN_POINT ( 'NONE',  ( 25.44550000000002399, 0.000000000000000000, 0.000000000000000000 ) ) ;
#70248 =( NAMED_UNIT ( * ) PLANE_ANGLE_UNIT ( ) SI_UNIT ( $, .RADIAN. ) );
#70249 = VECTOR ( 'NONE', #69482, 1000.000000000000000 ) ;
#70250 = VERTEX_POINT ( 'NONE', #20764 ) ;
#70251 = CARTESIAN_POINT ( 'NONE',  ( -97.65000000000001990, 90.00000000000004263, 84.28499999999999659 ) ) ;
#70252 = CARTESIAN_POINT ( 'NONE',  ( 92.35000000000000853, -209.9999999999999716, 83.09437500173430635 ) ) ;
#70253 = CARTESIAN_POINT ( 'NONE',  ( 94.99999999999998579, 93.05995642670504253, 89.84125000000000227 ) ) ;
#70254 = ORIENTED_EDGE ( 'NONE', *, *, #16722, .T. ) ;
#70255 = DIRECTION ( 'NONE',  ( 0.000000000000000000, 0.07845909572784530439, -0.9969173337331279638 ) ) ;
#70256 = LINE ( 'NONE', #36797, #15282 ) ;
#70257 = VERTEX_POINT ( 'NONE', #9486 ) ;
#70258 = VERTEX_POINT ( 'NONE', #9117 ) ;
#70259 = CARTESIAN_POINT ( 'NONE',  ( 5.000000000000000000, 6.074766241781102566E-16, -0.5080592402122449114 ) ) ;
#70260 = EDGE_CURVE ( 'NONE', #688, #66304, #5836, .T. ) ;
#70261 = ORIENTED_EDGE ( 'NONE', *, *, #60446, .F. ) ;
#70262 = VECTOR ( 'NONE', #15185, 1000.000000000000000 ) ;
#70263 = CARTESIAN_POINT ( 'NONE',  ( 93.67499999999999716, 87.70503267997126784, 85.74020833506763495 ) ) ;
#70264 = EDGE_LOOP ( 'NONE', ( #18839, #2462, #50792, #36987 ) ) ;
#70265 = DIRECTION ( 'NONE',  ( 0.000000000000000000, 0.000000000000000000, 1.000000000000000000 ) ) ;
#70266 = CARTESIAN_POINT ( 'NONE',  ( 5.000000000000002665, -8.966570791700153364, -81.50828551894237251 ) ) ;
#70267 = ORIENTED_EDGE ( 'NONE', *, *, #36314, .F. ) ;
#70268 = EDGE_LOOP ( 'NONE', ( #33186, #70229, #52865, #4756 ) ) ;
#70269 = CIRCLE ( 'NONE', #47494, 82.00000000000000000 ) ;
#70270 = VERTEX_POINT ( 'NONE', #21127 ) ;
#70271 = CARTESIAN_POINT ( 'NONE',  ( 10.00000000000000000, 81.90746397400394585, -3.894527615416976118 ) ) ;
#70272 = CARTESIAN_POINT ( 'NONE',  ( 92.34999999999999432, 90.00000000000002842, 81.74500000000000455 ) ) ;
#70273 = CARTESIAN_POINT ( 'NONE',  ( -96.32500000000001705, 92.29496732002878900, 86.71916666666666629 ) ) ;
#70274 = EDGE_CURVE ( 'NONE', #52806, #74080, #59903, .T. ) ;
#70275 = ORIENTED_EDGE ( 'NONE', *, *, #73513, .T. ) ;
#70276 = EDGE_CURVE ( 'NONE', #51144, #62438, #65914, .T. ) ;
#70277 = CARTESIAN_POINT ( 'NONE',  ( -12.40464318976454727, 10.41032311384371845, -55.00000000000000000 ) ) ;
#70278 =( BOUNDED_CURVE ( )  B_SPLINE_CURVE ( 2, ( #43582, #73231, #42821, #61235, #66498, #27362, #14980 ),
 .UNSPECIFIED., .F., .T. ) 
 B_SPLINE_CURVE_WITH_KNOTS ( ( 3, 2, 2, 3 ),
 ( 0.5503499107226623721, 0.5574054777297072771, 0.5644612432705895522, 0.5715170088666294834 ),
 .UNSPECIFIED. ) 
 CURVE ( )  GEOMETRIC_REPRESENTATION_ITEM ( )  RATIONAL_B_SPLINE_CURVE ( ( 0.9999924607068793048, 0.8660291735370716504, 1.000000000000000000, 0.8660254037844387076, 1.000000000000000000, 0.8660254037844387076, 1.000000000000000000 ) ) 
 REPRESENTATION_ITEM ( '' )  );
#70279 = DIRECTION ( 'NONE',  ( -0.000000000000000000, -0.9135454576426004225, -0.4067366430758009854 ) ) ;
#70280 = ORIENTED_EDGE ( 'NONE', *, *, #50123, .T. ) ;
#70281 = CARTESIAN_POINT ( 'NONE',  ( 10.00000000000000000, 37.58145647212455032, -0.6853352020786441789 ) ) ;
#70282 = CARTESIAN_POINT ( 'NONE',  ( -97.30629616937495996, -209.9999999999999716, 82.02281250086714692 ) ) ;
#70283 = ORIENTED_EDGE ( 'NONE', *, *, #38868, .F. ) ;
#70284 = EDGE_CURVE ( 'NONE', #42522, #61695, #32409, .T. ) ;
#70285 = DIRECTION ( 'NONE',  ( -1.000000000000000000, 0.000000000000000000, 0.000000000000000000 ) ) ;
#70286 = CARTESIAN_POINT ( 'NONE',  ( -3.000000000000000000, -22.67460108101783334, 6.353146135317912169 ) ) ;
#70287 = CARTESIAN_POINT ( 'NONE',  ( 96.32499999999997442, 92.29496732002878900, 89.23270833506762756 ) ) ;
#70288 = FACE_OUTER_BOUND ( 'NONE', #27234, .T. ) ;
#70289 = CARTESIAN_POINT ( 'NONE',  ( 10.00000000000000000, 0.000000000000000000, 0.000000000000000000 ) ) ;
#70290 = DIRECTION ( 'NONE',  ( 0.000000000000000000, 0.000000000000000000, 1.000000000000000000 ) ) ;
#70291 = DIRECTION ( 'NONE',  ( -1.000000000000000000, -0.000000000000000000, -0.000000000000000000 ) ) ;
#70292 = LINE ( 'NONE', #18797, #20741 ) ;
#70293 = DIRECTION ( 'NONE',  ( -0.000000000000000000, 0.4999999999999919509, 0.8660254037844432595 ) ) ;
#70294 = CARTESIAN_POINT ( 'NONE',  ( 50.00005079999999680, 0.000000000000000000, 12.50000000000000000 ) ) ;
#70295 = CARTESIAN_POINT ( 'NONE',  ( -97.30629616937501680, 88.66845928578038638, 78.26572916753380582 ) ) ;
#70296 = FACE_OUTER_BOUND ( 'NONE', #6566, .T. ) ;
#70297 = DIRECTION ( 'NONE',  ( 0.000000000000000000, 0.000000000000000000, 1.000000000000000000 ) ) ;
#70298 =( BOUNDED_CURVE ( )  B_SPLINE_CURVE ( 2, ( #45564, #62487, #5709, #6085, #22995, #62865, #63594, #57577, #28985 ),
 .UNSPECIFIED., .F., .F. ) 
 B_SPLINE_CURVE_WITH_KNOTS ( ( 3, 2, 2, 2, 3 ),
 ( 0.6561861948910822084, 0.6632419608429419577, 0.6702977263838236777, 0.6773534919247052866, 0.6773535682752295228 ),
 .UNSPECIFIED. ) 
 CURVE ( )  GEOMETRIC_REPRESENTATION_ITEM ( )  RATIONAL_B_SPLINE_CURVE ( ( 1.000000000000000000, 0.8660254037844387076, 1.000000000000000000, 0.8660254037844387076, 1.000000000000000000, 0.8660254037844387076, 1.000000000000000000, 0.9999985502592750874, 0.9999971005499255217 ) ) 
 REPRESENTATION_ITEM ( '' )  );
#70299 = VECTOR ( 'NONE', #51716, 1000.000000000000000 ) ;
#70300 = DIRECTION ( 'NONE',  ( 0.000000000000000000, -0.5224985647159381408, -0.8526401643540988395 ) ) ;
#70302 = CARTESIAN_POINT ( 'NONE',  ( -8.000000000000007105, -1.142349898368590025E-14, -6.370018489464426943E-15 ) ) ;
#70301 = VECTOR ( 'NONE', #14047, 1000.000000000000000 ) ;
#70303 = DIRECTION ( 'NONE',  ( 1.000000000000000000, 0.000000000000000000, 0.000000000000000000 ) ) ;
#70304 = CARTESIAN_POINT ( 'NONE',  ( 10.00000000000000000, -41.76106447765533147, 62.50884508063410294 ) ) ;
#70305 = CARTESIAN_POINT ( 'NONE',  ( 97.65000000000000568, -211.5299782133524218, 75.10395833506764518 ) ) ;
#70306 = AXIS2_PLACEMENT_3D ( 'NONE', #4068, #35745, #13558 ) ;
#70307 = DIRECTION ( 'NONE',  ( 2.603472992746261562E-14, 2.546204323184492723E-14, -1.000000000000000000 ) ) ;
#70308 = CARTESIAN_POINT ( 'NONE',  ( -95.73425683495054272, -214.0859151322042067, 74.64692065633565221 ) ) ;
#70309 = AXIS2_PLACEMENT_3D ( 'NONE', #12245, #45749, #35913 ) ;
#70310 = DIRECTION ( 'NONE',  ( 1.000000000000000000, 0.000000000000000000, 0.000000000000000000 ) ) ;
#70311 = AXIS2_PLACEMENT_3D ( 'NONE', #42666, #14824, #48303 ) ;
#70312 = AXIS2_PLACEMENT_3D ( 'NONE', #30169, #6515, #70753 ) ;
#70313 = VERTEX_POINT ( 'NONE', #26033 ) ;
#70314 = DIRECTION ( 'NONE',  ( 1.000000000000000000, 0.000000000000000000, 0.000000000000000000 ) ) ;
#70315 = DIRECTION ( 'NONE',  ( 1.000000000000000000, 0.000000000000000000, 0.000000000000000000 ) ) ;
#70316 = DIRECTION ( 'NONE',  ( 1.000000000000000000, 0.000000000000000000, 0.000000000000000000 ) ) ;
#70317 = LINE ( 'NONE', #18822, #46228 ) ;
#70318 = EDGE_CURVE ( 'NONE', #15051, #30682, #61040, .T. ) ;
#70319 = EDGE_CURVE ( 'NONE', #46797, #5511, #38060, .T. ) ;
#70320 = CYLINDRICAL_SURFACE ( 'NONE', #35548, 77.49899999999999523 ) ;
#70321 = ORIENTED_EDGE ( 'NONE', *, *, #62402, .T. ) ;
#70323 = ADVANCED_FACE ( 'NONE', ( #48608 ), #48961, .T. ) ;
#70322 = CARTESIAN_POINT ( 'NONE',  ( 10.00000000000000000, 0.000000000000000000, 0.000000000000000000 ) ) ;
#70324 = DIRECTION ( 'NONE',  ( 0.6516173805718078471, -0.7585478161175706058, 0.000000000000000000 ) ) ;
#70325 = ORIENTED_EDGE ( 'NONE', *, *, #61110, .F. ) ;
#70326 = CARTESIAN_POINT ( 'NONE',  ( 92.69370383062501162, -209.9999999999999716, 84.56281250086713897 ) ) ;
#70327 = CARTESIAN_POINT ( 'NONE',  ( 97.30629616937498838, -208.6684592857803295, 88.90197916753382401 ) ) ;
#70328 = VERTEX_POINT ( 'NONE', #60989 ) ;
#70329 = CARTESIAN_POINT ( 'NONE',  ( 93.84685191531251292, -211.9973110713294489, 88.63739583420048973 ) ) ;
#70330 = ADVANCED_FACE ( 'NONE', ( #42602 ), #71521, .T. ) ;
#70331 = ORIENTED_EDGE ( 'NONE', *, *, #72209, .F. ) ;
#70332 = LINE ( 'NONE', #2712, #62310 ) ;
#70333 = ORIENTED_EDGE ( 'NONE', *, *, #18182, .T. ) ;
#70334 = CARTESIAN_POINT ( 'NONE',  ( -97.30629616937501680, 91.33154071421968467, 81.49364583420047836 ) ) ;
#70335 = ORIENTED_EDGE ( 'NONE', *, *, #35573, .T. ) ;
#70336 = ORIENTED_EDGE ( 'NONE', *, *, #43832, .F. ) ;
#70337 = CARTESIAN_POINT ( 'NONE',  ( -97.64999999999996305, -211.5299782133524218, 87.59229166840096070 ) ) ;
#70338 = ORIENTED_EDGE ( 'NONE', *, *, #18724, .T. ) ;
#70339 = DIRECTION ( 'NONE',  ( -1.000000000000000000, 0.000000000000000000, 0.000000000000000000 ) ) ;
#70340 = ORIENTED_EDGE ( 'NONE', *, *, #32053, .F. ) ;
#70341 = CYLINDRICAL_SURFACE ( 'NONE', #14196, 42.00000000000000000 ) ;
#70342 = EDGE_CURVE ( 'NONE', #42429, #63620, #15123, .T. ) ;
#70343 = VERTEX_POINT ( 'NONE', #71892 ) ;
#70344 = DIRECTION ( 'NONE',  ( 0.000000000000000000, 0.000000000000000000, -1.000000000000000000 ) ) ;
#70345 = EDGE_CURVE ( 'NONE', #9142, #29501, #70620, .T. ) ;
#70346 = VECTOR ( 'NONE', #56539, 1000.000000000000000 ) ;
#70347 = VERTEX_POINT ( 'NONE', #37708 ) ;
#70348 = ORIENTED_EDGE ( 'NONE', *, *, #8663, .F. ) ;
#70349 = ORIENTED_EDGE ( 'NONE', *, *, #65557, .F. ) ;
#70350 = CARTESIAN_POINT ( 'NONE',  ( 92.69370383062501162, -208.6684592857803011, 81.33489583420048064 ) ) ;
#70351 = CARTESIAN_POINT ( 'NONE',  ( 10.00000000000000000, -16.23288003029473359, -33.80338159004301701 ) ) ;
#70352 = ITEM_DEFINED_TRANSFORMATION ( 'NONE', 'NONE', #35204,  #43395 ) ;
#70353 = CARTESIAN_POINT ( 'NONE',  ( 10.00000000000000000, 24.73286445877808148, -73.44644590900034586 ) ) ;
#70354 = CARTESIAN_POINT ( 'NONE',  ( -3.000000000000000000, 14.60985201121729737, -18.46759930825687945 ) ) ;
#70355 = CIRCLE ( 'NONE', #21148, 82.00000000000000000 ) ;
#70356 = DIRECTION ( 'NONE',  ( 0.000000000000000000, -0.5877852522924624790, -0.8090169943749550008 ) ) ;
#70357 = DIRECTION ( 'NONE',  ( -1.000000000000000000, -0.000000000000000000, -0.000000000000000000 ) ) ;
#70358 = VECTOR ( 'NONE', #65613, 1000.000000000000000 ) ;
#70359 = DIRECTION ( 'NONE',  ( -1.000000000000000000, 0.000000000000000000, -0.000000000000000000 ) ) ;
#70360 = CARTESIAN_POINT ( 'NONE',  ( -93.67500000000003979, 87.70503267997129626, 82.59166666666665435 ) ) ;
#70361 = CARTESIAN_POINT ( 'NONE',  ( -97.30629616937497417, -208.6684592857803011, 84.50989583420046358 ) ) ;
#70362 = CARTESIAN_POINT ( 'NONE',  ( -92.69370383062502583, 88.66845928578038638, 83.71614583420050337 ) ) ;
#70363 = EDGE_CURVE ( 'NONE', #67004, #54905, #8175, .T. ) ;
#70364 = VERTEX_POINT ( 'NONE', #60640 ) ;
#70365 = EDGE_CURVE ( 'NONE', #41070, #729, #38232, .T. ) ;
#70366 = AXIS2_PLACEMENT_3D ( 'NONE', #36552, #59504, #2402 ) ;
#70367 = CARTESIAN_POINT ( 'NONE',  ( 97.30629616937498838, 88.66845928578037217, 81.65239583420049030 ) ) ;
#70368 = VECTOR ( 'NONE', #55236, 1000.000000000000000 ) ;
#70369 = EDGE_LOOP ( 'NONE', ( #34899, #71988, #43595, #70755 ) ) ;
#70370 = CARTESIAN_POINT ( 'NONE',  ( 5.000000000000000000, 15.48615015657581750, 39.04073710021349797 ) ) ;
#70371 = CARTESIAN_POINT ( 'NONE',  ( -97.64999999999996305, -209.9999999999999716, 90.00000000000000000 ) ) ;
#70372 = DIRECTION ( 'NONE',  ( 0.000000000000000000, 0.000000000000000000, 1.000000000000000000 ) ) ;
#70373 = CARTESIAN_POINT ( 'NONE',  ( 0.000000000000000000, -59.75363087400113926, 56.15606465354937882 ) ) ;
#70374 = CARTESIAN_POINT ( 'NONE',  ( -12.75044424985336633, 0.001194404164724885897, -70.59999999999966747 ) ) ;
#70375 = CARTESIAN_POINT ( 'NONE',  ( -92.69370383062498320, -209.9999999999999716, 82.34031250086714238 ) ) ;
#70376 = LINE ( 'NONE', #58009, #33075 ) ;
#70377 = DIRECTION ( 'NONE',  ( -1.000000000000000000, -0.000000000000000000, 0.000000000000000000 ) ) ;
#70378 = LINE ( 'NONE', #18517, #63166 ) ;
#70379 = DIRECTION ( 'NONE',  ( -1.000000000000000000, 0.000000000000000000, 0.000000000000000000 ) ) ;
#70380 = ORIENTED_EDGE ( 'NONE', *, *, #46631, .T. ) ;
#70381 =( GEOMETRIC_REPRESENTATION_CONTEXT ( 3 ) GLOBAL_UNCERTAINTY_ASSIGNED_CONTEXT ( ( #48137 ) ) GLOBAL_UNIT_ASSIGNED_CONTEXT ( ( #12455, #35028, #854 ) ) REPRESENTATION_CONTEXT ( 'NONE', 'WORKASPACE' ) );
#70382 = ORIENTED_EDGE ( 'NONE', *, *, #7128, .T. ) ;
#70383 = CARTESIAN_POINT ( 'NONE',  ( 0.000000000000000000, -1.467624384280032501, -2.541999999999998039 ) ) ;
#70384 = CARTESIAN_POINT ( 'NONE',  ( -92.34999999999996589, -211.5299782133524502, 78.83458333333334167 ) ) ;
#70385 = CARTESIAN_POINT ( 'NONE',  ( -92.69370383062502583, 88.66845928578038638, 88.00239583420047040 ) ) ;
#70386 = CARTESIAN_POINT ( 'NONE',  ( -2.977765906491215642, 0.000000000000000000, -15.39727592589476579 ) ) ;
#70387 = CARTESIAN_POINT ( 'NONE',  ( 10.00000000000000000, -22.64427369931191336, 30.00120703465197280 ) ) ;
#70388 = CARTESIAN_POINT ( 'NONE',  ( 92.35000000000002274, -210.0000092897486468, 78.01437532303467037 ) ) ;
#70389 = CARTESIAN_POINT ( 'NONE',  ( 10.00000000000000000, 37.48860685352291000, -0.8828120875901940279 ) ) ;
#70390 = VERTEX_POINT ( 'NONE', #65538 ) ;
#70391 = CARTESIAN_POINT ( 'NONE',  ( -97.30629616937501680, 90.00000000000004263, 75.03781250086713328 ) ) ;
#70392 = DIRECTION ( 'NONE',  ( -1.000000000000000000, 1.047380211910311281E-14, 2.618450529775778123E-14 ) ) ;
#70393 = CARTESIAN_POINT ( 'NONE',  ( -3.000000000000000000, 5.835314593368477354, 22.81335362449854642 ) ) ;
#70394 = DIRECTION ( 'NONE',  ( -0.000000000000000000, -0.000000000000000000, 1.000000000000000000 ) ) ;
#70395 = CARTESIAN_POINT ( 'NONE',  ( 10.00000000000000000, 0.000000000000000000, 0.000000000000000000 ) ) ;
#70396 = CARTESIAN_POINT ( 'NONE',  ( -92.69370383062498320, -209.9999999999999716, 87.57906250086715261 ) ) ;
#70397 = DIRECTION ( 'NONE',  ( 0.000000000000000000, 0.8090169943749446757, 0.5877852522924769119 ) ) ;
#70398 = AXIS2_PLACEMENT_3D ( 'NONE', #57558, #6067, #46272 ) ;
#70399 = DIRECTION ( 'NONE',  ( -1.000000000000000000, 0.000000000000000000, -0.000000000000000000 ) ) ;
#70400 = ADVANCED_FACE ( 'NONE', ( #14008 ), #36954, .T. ) ;
#70401 = CARTESIAN_POINT ( 'NONE',  ( -97.30629616937497417, -211.3315407142195852, 76.51947916753381662 ) ) ;
#70402 = DIRECTION ( 'NONE',  ( 0.000000000000000000, 0.000000000000000000, -1.000000000000000000 ) ) ;
#70403 = VERTEX_POINT ( 'NONE', #56846 ) ;
#70404 = FACE_OUTER_BOUND ( 'NONE', #35682, .T. ) ;
#70405 = DIRECTION ( 'NONE',  ( -0.000000000000000000, -0.000000000000000000, -1.000000000000000000 ) ) ;
#70406 = DIRECTION ( 'NONE',  ( -1.000000000000000000, 0.000000000000000000, 0.000000000000000000 ) ) ;
#70407 = ADVANCED_FACE ( 'NONE', ( #74120 ), #28625, .F. ) ;
#70408 = CIRCLE ( 'NONE', #38014, 0.5000000000000004441 ) ;
#70409 = VECTOR ( 'NONE', #28017, 1000.000000000000000 ) ;
#70410 = EDGE_CURVE ( 'NONE', #10633, #41779, #62112, .T. ) ;
#70411 =( BOUNDED_CURVE ( )  B_SPLINE_CURVE ( 2, ( #62902, #39946, #28644, #39574, #51210, #51584, #22651, #62135, #11358 ),
 .UNSPECIFIED., .F., .T. ) 
 B_SPLINE_CURVE_WITH_KNOTS ( ( 3, 2, 2, 2, 3 ),
 ( 0.6138516023217082118, 0.6209073676006977571, 0.6279631331416146711, 0.6350188986825316961, 0.6350190250602294473 ),
 .UNSPECIFIED. ) 
 CURVE ( )  GEOMETRIC_REPRESENTATION_ITEM ( )  RATIONAL_B_SPLINE_CURVE ( ( 1.000000000000000000, 0.8660254037844387076, 1.000000000000000000, 0.8660254037844387076, 1.000000000000000000, 0.8660254037844387076, 1.000000000000000000, 0.9999976003452877293, 0.9999952007765371409 ) ) 
 REPRESENTATION_ITEM ( '' )  );
#70412 = DIRECTION ( 'NONE',  ( -1.000000000000000000, -0.000000000000000000, 0.000000000000000000 ) ) ;
#70413 = CARTESIAN_POINT ( 'NONE',  ( 92.69370383062501162, -208.6684592857803011, 76.25489583420049655 ) ) ;
#70414 = VERTEX_POINT ( 'NONE', #39179 ) ;
#70415 = CIRCLE ( 'NONE', #35603, 31.99999999999999645 ) ;
#70416 = CARTESIAN_POINT ( 'NONE',  ( -3.000000000000000000, 6.762365576493643893, -25.66652317338391853 ) ) ;
#70417 = DIRECTION ( 'NONE',  ( -0.9997280174009349762, 0.02332147558787671729, 0.000000000000000000 ) ) ;
#70418 = VERTEX_POINT ( 'NONE', #57217 ) ;
#70419 = LINE ( 'NONE', #52403, #51952 ) ;
#70420 = ORIENTED_EDGE ( 'NONE', *, *, #20392, .T. ) ;
#70421 = EDGE_CURVE ( 'NONE', #29098, #5845, #45945, .T. ) ;
#70422 = DIRECTION ( 'NONE',  ( -1.000000000000000000, 0.000000000000000000, -0.000000000000000000 ) ) ;
#70423 = CIRCLE ( 'NONE', #58423, 31.99999999999998934 ) ;
#70424 = VERTEX_POINT ( 'NONE', #17355 ) ;
#70425 = ORIENTED_EDGE ( 'NONE', *, *, #70082, .F. ) ;
#70426 = VERTEX_POINT ( 'NONE', #16992 ) ;
#70427 = DIRECTION ( 'NONE',  ( 0.000000000000000000, 0.000000000000000000, 1.000000000000000000 ) ) ;
#70428 = AXIS2_PLACEMENT_3D ( 'NONE', #68134, #46687, #62896 ) ;
#70429 = EDGE_LOOP ( 'NONE', ( #41263, #56991, #9051, #36138 ) ) ;
#70430 = EDGE_CURVE ( 'NONE', #62638, #5972, #23011, .T. ) ;
#70431 = ORIENTED_EDGE ( 'NONE', *, *, #48970, .T. ) ;
#70432 = CARTESIAN_POINT ( 'NONE',  ( 93.84685191531248449, 91.99731107132950569, 81.44072916753381719 ) ) ;
#70433 = CARTESIAN_POINT ( 'NONE',  ( 0.000000000000000000, -21.60688246758530084, -79.10210256391388839 ) ) ;
#70434 = EDGE_CURVE ( 'NONE', #42545, #32709, #28717, .T. ) ;
#70435 = CARTESIAN_POINT ( 'NONE',  ( 94.15631797925327362, -214.6948328857846207, 74.84535815546847459 ) ) ;
#70436 = ORIENTED_EDGE ( 'NONE', *, *, #66390, .T. ) ;
#70437 = VERTEX_POINT ( 'NONE', #39554 ) ;
#70438 = ORIENTED_EDGE ( 'NONE', *, *, #33896, .F. ) ;
#70439 = DIRECTION ( 'NONE',  ( 0.000000000000000000, 0.000000000000000000, -1.000000000000000000 ) ) ;
#70441 = ORIENTED_EDGE ( 'NONE', *, *, #35828, .F. ) ;
#70440 = EDGE_CURVE ( 'NONE', #40781, #33089, #4985, .T. ) ;
#70442 = ADVANCED_FACE ( 'NONE', ( #16242 ), #34641, .T. ) ;
#70443 = VECTOR ( 'NONE', #20990, 1000.000000000000000 ) ;
#70444 = DIRECTION ( 'NONE',  ( -1.000000000000000000, -0.000000000000000000, -0.000000000000000000 ) ) ;
#70445 = CARTESIAN_POINT ( 'NONE',  ( -93.26027265873601380, 91.51405112163766375, 74.79348190356853365 ) ) ;
#70446 = PLANE ( 'NONE',  #26786 ) ;
#70447 = DIRECTION ( 'NONE',  ( 1.000000000000000000, 0.000000000000000000, 0.000000000000000000 ) ) ;
#70448 = CARTESIAN_POINT ( 'NONE',  ( -97.65000000000009095, 88.47002178664760663, 77.98791666666667766 ) ) ;
#70449 = CARTESIAN_POINT ( 'NONE',  ( 0.000000000000000000, 0.000000000000000000, -20.00000000000000000 ) ) ;
#70450 = CARTESIAN_POINT ( 'NONE',  ( -96.32499999999996021, -212.2949673200287179, 80.02520833506763154 ) ) ;
#70451 = LINE ( 'NONE', #70832, #33895 ) ;
#70452 = EDGE_CURVE ( 'NONE', #60230, #54767, #64728, .T. ) ;
#70454 = CARTESIAN_POINT ( 'NONE',  ( -95.00000000000002842, 86.94004357329504273, 74.99812500173430863 ) ) ;
#70453 = CARTESIAN_POINT ( 'NONE',  ( 92.34999999999999432, 91.52997821335252127, 74.78645833506763552 ) ) ;
#70455 = VERTEX_POINT ( 'NONE', #33904 ) ;
#70456 = CARTESIAN_POINT ( 'NONE',  ( 94.99999999999998579, 92.66308142843935514, 77.57781250086715374 ) ) ;
#70457 = VECTOR ( 'NONE', #28141, 1000.000000000000000 ) ;
#70458 = CARTESIAN_POINT ( 'NONE',  ( 6.377742925735834234, -145.7647898336708181, 5.500000000000000000 ) ) ;
#70459 = CARTESIAN_POINT ( 'NONE',  ( 0.000000000000000000, -54.21277698773636899, -55.38113227695839669 ) ) ;
#70460 = CARTESIAN_POINT ( 'NONE',  ( 0.000000000000000000, -26.08949754953005495, -27.05870788708258701 ) ) ;
#70461 = CARTESIAN_POINT ( 'NONE',  ( 15.00000000000000000, 23.49999999999999645, 1.499999999999995337 ) ) ;
#70462 =( GEOMETRIC_REPRESENTATION_CONTEXT ( 3 ) GLOBAL_UNCERTAINTY_ASSIGNED_CONTEXT ( ( #51874 ) ) GLOBAL_UNIT_ASSIGNED_CONTEXT ( ( #64731, #1616, #41789 ) ) REPRESENTATION_CONTEXT ( 'NONE', 'WORKASPACE' ) );
#70463 = EDGE_CURVE ( 'NONE', #69471, #2166, #18613, .T. ) ;
#70464 = DIRECTION ( 'NONE',  ( 1.000000000000000000, -0.000000000000000000, -0.000000000000000000 ) ) ;
#70465 = VERTEX_POINT ( 'NONE', #27518 ) ;
#70466 = PLANE ( 'NONE',  #64986 ) ;
#70467 = DIRECTION ( 'NONE',  ( -0.000000000000000000, -0.000000000000000000, 1.000000000000000000 ) ) ;
#70468 = EDGE_LOOP ( 'NONE', ( #41783, #27774, #66101, #53450 ) ) ;
#70469 = VECTOR ( 'NONE', #63943, 1000.000000000000000 ) ;
#70470 = ORIENTED_EDGE ( 'NONE', *, *, #45154, .T. ) ;
#70471 = AXIS2_PLACEMENT_3D ( 'NONE', #1391, #65252, #42318 ) ;
#70472 = FACE_OUTER_BOUND ( 'NONE', #47431, .T. ) ;
#70473 = CARTESIAN_POINT ( 'NONE',  ( 12.74955575014744547, 0.001194404164628405998, -85.60000000000000853 ) ) ;
#70474 = DIRECTION ( 'NONE',  ( -1.000000000000000000, 0.000000000000000000, -0.000000000000000000 ) ) ;
#70475 = CARTESIAN_POINT ( 'NONE',  ( -97.30629616937497417, -208.6684592857803011, 78.95364583420048632 ) ) ;
#70476 = EDGE_LOOP ( 'NONE', ( #19954, #44006, #47571, #49258 ) ) ;
#70477 = DIRECTION ( 'NONE',  ( 1.000000000000000000, 0.000000000000000000, 0.000000000000000000 ) ) ;
#70478 = DIRECTION ( 'NONE',  ( -1.000000000000000000, 0.000000000000000000, 0.000000000000000000 ) ) ;
#70479 = CIRCLE ( 'NONE', #47688, 37.49900000000000944 ) ;
#70480 = CARTESIAN_POINT ( 'NONE',  ( 0.000000000000000000, 22.74946021919133088, 29.81001611431016229 ) ) ;
#70481 = PLANE ( 'NONE',  #24449 ) ;
#70482 = DIRECTION ( 'NONE',  ( 1.000000000000000000, 0.000000000000000000, 0.000000000000000000 ) ) ;
#70483 = DIRECTION ( 'NONE',  ( 0.000000000000000000, 0.000000000000000000, 1.000000000000000000 ) ) ;
#70484 = CARTESIAN_POINT ( 'NONE',  ( -4.653126046682595884, -146.1313684676804314, 5.500000000000000000 ) ) ;
#70485 = CARTESIAN_POINT ( 'NONE',  ( 10.00000000000000000, 0.000000000000000000, 0.000000000000000000 ) ) ;
#70486 = AXIS2_PLACEMENT_3D ( 'NONE', #65202, #60310, #37737 ) ;
#70487 = CARTESIAN_POINT ( 'NONE',  ( 9.984461079971730157, -95.40710393340120277, 5.500000000000000000 ) ) ;
#70488 = CARTESIAN_POINT ( 'NONE',  ( 97.30629616937498838, 91.33154071421968467, 83.82197916753382572 ) ) ;
#70489 = CARTESIAN_POINT ( 'NONE',  ( -92.69370383062498320, -208.6684592857803295, 85.72697916753381264 ) ) ;
#70490 = LINE ( 'NONE', #42328, #51830 ) ;
#70491 = EDGE_LOOP ( 'NONE', ( #17981, #51735 ) ) ;
#70492 = CARTESIAN_POINT ( 'NONE',  ( -3.000000000000000000, 16.83928648764945279, -16.46020748918028076 ) ) ;
#70493 = CARTESIAN_POINT ( 'NONE',  ( -94.99999999999997158, -213.0599564267049857, 81.90374999999998806 ) ) ;
#70494 = EDGE_CURVE ( 'NONE', #60846, #55130, #68500, .T. ) ;
#70495 = CARTESIAN_POINT ( 'NONE',  ( -96.15314808468751551, 88.00268892867056536, 75.77864583420047495 ) ) ;
#70496 = EDGE_CURVE ( 'NONE', #35203, #23253, #10226, .T. ) ;
#70497 = EDGE_CURVE ( 'NONE', #46890, #35626, #15474, .T. ) ;
#70498 = EDGE_CURVE ( 'NONE', #143, #34944, #31086, .T. ) ;
#70499 = CARTESIAN_POINT ( 'NONE',  ( 92.69370383062501162, -211.3315407142195852, 85.88572916753382458 ) ) ;
#70500 = ORIENTED_EDGE ( 'NONE', *, *, #24111, .T. ) ;
#70501 = VERTEX_POINT ( 'NONE', #7559 ) ;
#70502 =( BOUNDED_CURVE ( )  B_SPLINE_CURVE ( 2, ( #33162, #50463, #61008, #44471, #22273, #9128, #56111 ),
 .UNSPECIFIED., .F., .F. ) 
 B_SPLINE_CURVE_WITH_KNOTS ( ( 3, 2, 2, 3 ),
 ( 0.2499999999999995837, 0.2569444444444442532, 0.2638888888888890061, 0.2708333333333337034 ),
 .UNSPECIFIED. ) 
 CURVE ( )  GEOMETRIC_REPRESENTATION_ITEM ( )  RATIONAL_B_SPLINE_CURVE ( ( 1.000000000000007994, 0.8660254037844307140, 1.000000000000000000, 0.8660254037844387076, 1.000000000000000000, 0.8660254037844311581, 1.000000000000007550 ) ) 
 REPRESENTATION_ITEM ( '' )  );
#70503 = AXIS2_PLACEMENT_3D ( 'NONE', #40223, #9794, #49999 ) ;
#70504 = VERTEX_POINT ( 'NONE', #41042 ) ;
#70505 = CIRCLE ( 'NONE', #38120, 82.00000000000000000 ) ;
#70506 = CARTESIAN_POINT ( 'NONE',  ( -3.000000000000000000, 26.50000000000000355, 1.500000000000000000 ) ) ;
#70507 = CARTESIAN_POINT ( 'NONE',  ( 11.99999999999999822, 81.96053171279901051, 2.543863470248673764 ) ) ;
#70508 = AXIS2_PLACEMENT_3D ( 'NONE', #56741, #29888, #22141 ) ;
#70509 = VERTEX_POINT ( 'NONE', #47048 ) ;
#70510 = AXIS2_PLACEMENT_3D ( 'NONE', #66722, #38144, #32863 ) ;
#70511 = ORIENTED_EDGE ( 'NONE', *, *, #22395, .T. ) ;
#70512 = EDGE_CURVE ( 'NONE', #55045, #55663, #1957, .T. ) ;
#70513 = DIRECTION ( 'NONE',  ( -0.000000000000000000, -0.000000000000000000, -1.000000000000000000 ) ) ;
#70514 = CARTESIAN_POINT ( 'NONE',  ( 96.15314808468748708, -208.0026889286704943, 83.23989583420049598 ) ) ;
#70515 = DIRECTION ( 'NONE',  ( -1.000000000000000000, -0.000000000000000000, 0.000000000000000000 ) ) ;
#70516 = DIRECTION ( 'NONE',  ( -1.000000000000000000, 0.000000000000000000, -0.000000000000000000 ) ) ;
#70517 = FACE_OUTER_BOUND ( 'NONE', #56954, .T. ) ;
#70518 = DIRECTION ( 'NONE',  ( 1.000000000000000000, 0.000000000000000000, 0.000000000000000000 ) ) ;
#70519 = CARTESIAN_POINT ( 'NONE',  ( 10.00000000000000000, 77.32052557432841411, 5.256550761633138613 ) ) ;
#70520 = CARTESIAN_POINT ( 'NONE',  ( 92.35000000000002274, -208.4700217866474645, 84.23208333333333542 ) ) ;
#70521 = ORIENTED_EDGE ( 'NONE', *, *, #65059, .T. ) ;
#70522 = ORIENTED_EDGE ( 'NONE', *, *, #9224, .T. ) ;
#70523 = ORIENTED_EDGE ( 'NONE', *, *, #45143, .T. ) ;
#70524 = VERTEX_POINT ( 'NONE', #47768 ) ;
#70525 = DIRECTION ( 'NONE',  ( 0.000000000000000000, 0.9510565162951523099, 0.3090169943749513926 ) ) ;
#70526 = EDGE_CURVE ( 'NONE', #56117, #55837, #19044, .T. ) ;
#70527 = ADVANCED_FACE ( 'NONE', ( #47410 ), #7051, .F. ) ;
#70528 = AXIS2_PLACEMENT_3D ( 'NONE', #63257, #68526, #45601 ) ;
#70529 = CARTESIAN_POINT ( 'NONE',  ( -96.15314808468752972, 91.99731107132950569, 87.15572916753382060 ) ) ;
#70531 = B_SPLINE_CURVE_WITH_KNOTS ( 'NONE', 3,
 ( #15459, #38403, #56818, #15842 ),
 .UNSPECIFIED., .F., .F.,
 ( 4, 4 ),
 ( 2.446487931514401995E-06, 1.000000000000000000 ),
 .UNSPECIFIED. ) ;
#70530 = CARTESIAN_POINT ( 'NONE',  ( 0.000000000000000000, -9.188173127307001309, -40.98264845739759465 ) ) ;
#70532 = CARTESIAN_POINT ( 'NONE',  ( -93.67500000000003979, 87.70503267997129626, 83.86166666666666458 ) ) ;
#70533 = CARTESIAN_POINT ( 'NONE',  ( 93.84685191531249870, -208.0026889286704943, 88.26697916753380468 ) ) ;
#70534 = CARTESIAN_POINT ( 'NONE',  ( -95.00000000002617639, -209.9999999999999432, -64.99999999999349143 ) ) ;
#70535 = AXIS2_PLACEMENT_3D ( 'NONE', #59143, #24920, #19641 ) ;
#70536 = VERTEX_POINT ( 'NONE', #69232 ) ;
#70537 = CARTESIAN_POINT ( 'NONE',  ( -2.459674775249762302, 2.117821873984080520E-13, 20.20000000000035456 ) ) ;
#70538 = ORIENTED_EDGE ( 'NONE', *, *, #21222, .F. ) ;
#70539 = CYLINDRICAL_SURFACE ( 'NONE', #27822, 31.99999999999999289 ) ;
#70540 = ORIENTED_EDGE ( 'NONE', *, *, #64926, .T. ) ;
#70541 = CARTESIAN_POINT ( 'NONE',  ( -96.32500000000001705, 87.70503267997129626, 87.64520833506762187 ) ) ;
#70542 = CARTESIAN_POINT ( 'NONE',  ( 92.69370383062498320, 91.33154071421968467, 89.11364583420049712 ) ) ;
#70543 = EDGE_LOOP ( 'NONE', ( #21804, #32991, #62179, #60648 ) ) ;
#70544 = DIRECTION ( 'NONE',  ( -1.000000000000000000, 0.000000000000000000, 0.000000000000000000 ) ) ;
#70545 = CARTESIAN_POINT ( 'NONE',  ( 92.35000000000000853, -209.9999999999999716, 89.90078125043358170 ) ) ;
#70546 = CARTESIAN_POINT ( 'NONE',  ( 7.103376864691351012E-17, -120.0000000000000000, -64.00000000000000000 ) ) ;
#70547 = CARTESIAN_POINT ( 'NONE',  ( 11.99999999999999822, -75.54627589209955829, 17.28742895386058009 ) ) ;
#70548 = ORIENTED_EDGE ( 'NONE', *, *, #8755, .T. ) ;
#70549 = CARTESIAN_POINT ( 'NONE',  ( 0.8192951148925871063, -5.300482436767286920, -5.801655677627835850 ) ) ;
#70550 = DIRECTION ( 'NONE',  ( 0.000000000000000000, 0.000000000000000000, 1.000000000000000000 ) ) ;
#70551 = EDGE_LOOP ( 'NONE', ( #26711, #790, #70815, #9059 ) ) ;
#70552 = ORIENTED_EDGE ( 'NONE', *, *, #38041, .T. ) ;
#70553 = DIRECTION ( 'NONE',  ( -1.000000000000000000, -0.000000000000000000, -0.000000000000000000 ) ) ;
#70554 = DIRECTION ( 'NONE',  ( 0.000000000000000000, 0.000000000000000000, 1.000000000000000000 ) ) ;
#70555 = DIRECTION ( 'NONE',  ( 0.000000000000000000, 0.000000000000000000, -1.000000000000000000 ) ) ;
#70556 = CARTESIAN_POINT ( 'NONE',  ( -94.99999999999997158, -207.3369185715606307, 86.46781250086716852 ) ) ;
#70557 = EDGE_LOOP ( 'NONE', ( #70333, #68525, #51870, #21303 ) ) ;
#70558 = VECTOR ( 'NONE', #3352, 1000.000000000000000 ) ;
#70559 = CARTESIAN_POINT ( 'NONE',  ( -97.64999999999996305, -211.5299782133524218, 82.43291666666665662 ) ) ;
#70560 = EDGE_LOOP ( 'NONE', ( #1811, #1599, #73063, #36411 ) ) ;
#70561 = AXIS2_PLACEMENT_3D ( 'NONE', #45376, #5894, #68298 ) ;
#70562 = VECTOR ( 'NONE', #59611, 1000.000000000000000 ) ;
#70563 = ORIENTED_EDGE ( 'NONE', *, *, #65447, .T. ) ;
#70564 = CYLINDRICAL_SURFACE ( 'NONE', #72616, 37.49900000000000233 ) ;
#70565 = CARTESIAN_POINT ( 'NONE',  ( 92.69370383062498320, 90.00000000000002842, 89.80156250086714920 ) ) ;
#70566 = AXIS2_PLACEMENT_3D ( 'NONE', #44146, #38131, #45272 ) ;
#70567 = CARTESIAN_POINT ( 'NONE',  ( 2.047646702416564324, -96.54137380445985173, -2.500000000000000000 ) ) ;
#70568 = CARTESIAN_POINT ( 'NONE',  ( 97.30629616937498838, 91.33154071421968467, 81.75822916753381264 ) ) ;
#70569 = AXIS2_PLACEMENT_3D ( 'NONE', #22623, #33898, #56839 ) ;
#70570 = CARTESIAN_POINT ( 'NONE',  ( 11.99999999999999822, 0.000000000000000000, 0.000000000000000000 ) ) ;
#70571 = LINE ( 'NONE', #13451, #4973 ) ;
#70572 = DIRECTION ( 'NONE',  ( 1.000000000000000000, 0.000000000000000000, 0.000000000000000000 ) ) ;
#70573 = FACE_OUTER_BOUND ( 'NONE', #60659, .T. ) ;
#70574 = DIRECTION ( 'NONE',  ( 0.000000000000000000, 0.2334453638558990629, 0.9723699203976782224 ) ) ;
#70575 = DIRECTION ( 'NONE',  ( 1.000000000000000000, 0.000000000000000000, 0.000000000000000000 ) ) ;
#70576 = DIRECTION ( 'NONE',  ( 1.000000000000000000, 6.951859121168206841E-17, -0.000000000000000000 ) ) ;
#70577 = DIRECTION ( 'NONE',  ( 0.000000000000000000, -0.8660254037844421493, -0.4999999999999939493 ) ) ;
#70578 = EDGE_CURVE ( 'NONE', #11224, #13197, #1226, .T. ) ;
#70579 = DIRECTION ( 'NONE',  ( 1.000000000000000000, 0.000000000000000000, 0.000000000000000000 ) ) ;
#70580 = EDGE_LOOP ( 'NONE', ( #12972, #40682, #62426, #19004 ) ) ;
#70581 = EDGE_CURVE ( 'NONE', #54849, #60507, #43082, .T. ) ;
#70582 = CARTESIAN_POINT ( 'NONE',  ( -92.69370383062504004, 90.00000000000004263, 86.15031250086714465 ) ) ;
#70583 = FACE_OUTER_BOUND ( 'NONE', #56777, .T. ) ;
#70584 = CIRCLE ( 'NONE', #62194, 77.49899999999999523 ) ;
#70585 = EDGE_CURVE ( 'NONE', #40286, #50011, #28670, .T. ) ;
#70586 = AXIS2_PLACEMENT_3D ( 'NONE', #34137, #5961, #51800 ) ;
#70587 = VECTOR ( 'NONE', #23121, 999.9999999999998863 ) ;
#70588 = CIRCLE ( 'NONE', #42990, 42.00000000000000000 ) ;
#70589 = EDGE_CURVE ( 'NONE', #50488, #65810, #23377, .T. ) ;
#70590 = DIRECTION ( 'NONE',  ( 0.000000000000000000, 1.000000000000000000, 7.228014483236689653E-16 ) ) ;
#70591 = EDGE_LOOP ( 'NONE', ( #4918, #18522, #9992, #50842 ) ) ;
#70592 = EDGE_CURVE ( 'NONE', #54635, #33655, #3479, .T. ) ;
#70593 = CARTESIAN_POINT ( 'NONE',  ( 0.000000000000000000, 23.50000000000000000, 1.499999999999997780 ) ) ;
#70594 = PLANE ( 'NONE',  #34828 ) ;
#70595 = CARTESIAN_POINT ( 'NONE',  ( 10.00000000000000000, -77.19088730480518734, -6.903761155838607166 ) ) ;
#70596 = LINE ( 'NONE', #43827, #28409 ) ;
#70597 = CARTESIAN_POINT ( 'NONE',  ( 96.15314808468748708, -208.0026889286704943, 83.23989583420049598 ) ) ;
#70598 = VERTEX_POINT ( 'NONE', #18100 ) ;
#70599 = ORIENTED_EDGE ( 'NONE', *, *, #23505, .F. ) ;
#70600 = EDGE_CURVE ( 'NONE', #38085, #18829, #46663, .T. ) ;
#70601 = ADVANCED_FACE ( 'NONE', ( #35390 ), #40708, .F. ) ;
#70602 = CARTESIAN_POINT ( 'NONE',  ( 0.000000000000000000, -41.19522573413780009, 65.64334221924896440 ) ) ;
#70603 = ORIENTED_EDGE ( 'NONE', *, *, #62909, .F. ) ;
#70604 = CARTESIAN_POINT ( 'NONE',  ( -12.40464318976454905, 10.41032311384371845, -64.01812422950393966 ) ) ;
#70605 = CARTESIAN_POINT ( 'NONE',  ( 92.69370383062501162, -209.9999999999999716, 75.67281250086713840 ) ) ;
#70606 = VECTOR ( 'NONE', #62244, 1000.000000000000000 ) ;
#70607 = ORIENTED_EDGE ( 'NONE', *, *, #74295, .T. ) ;
#70608 = CARTESIAN_POINT ( 'NONE',  ( 97.30629616937498838, -211.3315407142195852, 79.90614583420048689 ) ) ;
#70609 = VECTOR ( 'NONE', #25007, 1000.000000000000000 ) ;
#70610 = CIRCLE ( 'NONE', #21404, 31.99999999999998934 ) ;
#70611 = ORIENTED_EDGE ( 'NONE', *, *, #18307, .T. ) ;
#70612 = CARTESIAN_POINT ( 'NONE',  ( 0.000000000000000000, -51.02545421589285723, -55.20638768913812555 ) ) ;
#70613 = ORIENTED_EDGE ( 'NONE', *, *, #63837, .F. ) ;
#70614 = VERTEX_POINT ( 'NONE', #7189 ) ;
#70615 = DIRECTION ( 'NONE',  ( 0.000000000000000000, -0.5224985647159559043, 0.8526401643540879594 ) ) ;
#70616 = EDGE_CURVE ( 'NONE', #41879, #23150, #56275, .T. ) ;
#70617 = ADVANCED_FACE ( 'NONE', ( #18819 ), #6456, .T. ) ;
#70618 = AXIS2_PLACEMENT_3D ( 'NONE', #20000, #30542, #36931 ) ;
#70619 = CARTESIAN_POINT ( 'NONE',  ( 0.000000000000000000, 26.02418014898407961, -70.52718814184231633 ) ) ;
#70620 = CIRCLE ( 'NONE', #65819, 31.99999999999998224 ) ;
#70621 = EDGE_LOOP ( 'NONE', ( #34561, #53917, #13940, #11500 ) ) ;
#70622 = CARTESIAN_POINT ( 'NONE',  ( 24.95699195200416654, -110.9640411295978595, 5.500000000000000000 ) ) ;
#70623 = CARTESIAN_POINT ( 'NONE',  ( 95.00000000000000000, -206.9400435732949575, 84.84062500173429555 ) ) ;
#70624 = CARTESIAN_POINT ( 'NONE',  ( 96.32499999999997442, 92.29496732002878900, 87.88333333333332575 ) ) ;
#70625 = ORIENTED_EDGE ( 'NONE', *, *, #48473, .F. ) ;
#70626 = LINE ( 'NONE', #7499, #2333 ) ;
#70627 = DIRECTION ( 'NONE',  ( 0.5687579148473752566, -0.8225049752423786442, 0.000000000000000000 ) ) ;
#70628 = ORIENTED_EDGE ( 'NONE', *, *, #20184, .F. ) ;
#70629 = VERTEX_POINT ( 'NONE', #848 ) ;
#70630 = CARTESIAN_POINT ( 'NONE',  ( -97.30629616937501680, 88.66845928578038638, 89.21947916753381946 ) ) ;
#70631 = CARTESIAN_POINT ( 'NONE',  ( 96.15314808468748708, 88.00268892867053694, 85.40947916753380298 ) ) ;
#70632 = ORIENTED_EDGE ( 'NONE', *, *, #7147, .T. ) ;
#70633 = CARTESIAN_POINT ( 'NONE',  ( 92.34999999999999432, 88.47002178664753558, 86.95729166840096980 ) ) ;
#70634 = AXIS2_PLACEMENT_3D ( 'NONE', #66000, #49051, #60722 ) ;
#70635 = VERTEX_POINT ( 'NONE', #46667 ) ;
#70636 = FACE_BOUND ( 'NONE', #70369, .T. ) ;
#70637 = CARTESIAN_POINT ( 'NONE',  ( -92.35000000000003695, 89.99999998014077107, 85.95187500101400246 ) ) ;
#70638 = ORIENTED_EDGE ( 'NONE', *, *, #66308, .F. ) ;
#70639 = ORIENTED_EDGE ( 'NONE', *, *, #21709, .T. ) ;
#70640 = ORIENTED_EDGE ( 'NONE', *, *, #66195, .F. ) ;
#70641 = CARTESIAN_POINT ( 'NONE',  ( -100.0000000000260485, 95.00000000000001421, 75.00000000000001421 ) ) ;
#70642 = CYLINDRICAL_SURFACE ( 'NONE', #36100, 82.00000000000000000 ) ;
#70643 = VECTOR ( 'NONE', #38994, 1000.000000000000000 ) ;
#70644 = CARTESIAN_POINT ( 'NONE',  ( -95.00000000000002842, 93.05995642670501411, 84.12625000000001307 ) ) ;
#70645 = ORIENTED_EDGE ( 'NONE', *, *, #17051, .T. ) ;
#70646 = CARTESIAN_POINT ( 'NONE',  ( 10.00000000000000000, 3.925862922256160736, 41.81611651403863306 ) ) ;
#70647 = DIRECTION ( 'NONE',  ( -1.000000000000000000, 0.000000000000000000, -0.000000000000000000 ) ) ;
#70648 = VERTEX_POINT ( 'NONE', #69601 ) ;
#70649 = DIRECTION ( 'NONE',  ( 3.061616997868382648E-16, 1.000000000000000000, -0.000000000000000000 ) ) ;
#70650 = CARTESIAN_POINT ( 'NONE',  ( -94.99999999999997158, -212.6630814284392557, 82.18156250086714465 ) ) ;
#70651 = VERTEX_POINT ( 'NONE', #13190 ) ;
#70652 = CARTESIAN_POINT ( 'NONE',  ( 10.00000000000000178, 1.530808498934191521E-15, -12.50000000000000000 ) ) ;
#70653 = DIRECTION ( 'NONE',  ( -1.000000000000000000, 0.000000000000000000, 0.000000000000000000 ) ) ;
#70654 = CARTESIAN_POINT ( 'NONE',  ( 11.99999999999999822, 76.69515212746057387, -29.01471420065479379 ) ) ;
#70655 = DIRECTION ( 'NONE',  ( -1.000000000000000000, -0.000000000000000000, -0.000000000000000000 ) ) ;
#70656 = EDGE_CURVE ( 'NONE', #60846, #61246, #64339, .T. ) ;
#70657 = LINE ( 'NONE', #46276, #772 ) ;
#70658 = CARTESIAN_POINT ( 'NONE',  ( 5.000000000000000000, 26.79245525562714292, 32.34446384429980981 ) ) ;
#70659 = EDGE_CURVE ( 'NONE', #30548, #11576, #7921, .T. ) ;
#70660 = CARTESIAN_POINT ( 'NONE',  ( 11.99999999999999822, 75.11764819372149304, -2.946379043146603482 ) ) ;
#70661 = DIRECTION ( 'NONE',  ( -1.000000000000000000, -0.000000000000000000, -0.000000000000000000 ) ) ;
#70662 = EDGE_CURVE ( 'NONE', #72362, #63075, #3783, .T. ) ;
#70663 = CARTESIAN_POINT ( 'NONE',  ( 0.000000000000000000, 80.55351364060589958, 15.33399622253511829 ) ) ;
#70664 = VECTOR ( 'NONE', #2537, 1000.000000000000227 ) ;
#70665 = CARTESIAN_POINT ( 'NONE',  ( -96.15314808468752972, 91.99731107132950569, 75.56697916753381605 ) ) ;
#70666 = DIRECTION ( 'NONE',  ( -1.000000000000000000, 0.000000000000000000, -0.000000000000000000 ) ) ;
#70667 = CARTESIAN_POINT ( 'NONE',  ( 92.35000000000005116, 88.47002178664747873, 76.08291666666664810 ) ) ;
#70668 = ADVANCED_FACE ( 'NONE', ( #48879 ), #42887, .T. ) ;
#70669 = AXIS2_PLACEMENT_3D ( 'NONE', #65948, #37378, #14427 ) ;
#70670 = CARTESIAN_POINT ( 'NONE',  ( 0.000000000000000000, 71.27951684758026829, 30.41916302227139113 ) ) ;
#70671 = CIRCLE ( 'NONE', #62285, 16.00000000000000000 ) ;
#70672 = EDGE_CURVE ( 'NONE', #38741, #38823, #20307, .T. ) ;
#70673 = DIRECTION ( 'NONE',  ( -1.000000000000000000, -4.476705744456277943E-17, 0.000000000000000000 ) ) ;
#70674 = LINE ( 'NONE', #52663, #3445 ) ;
#70676 = AXIS2_PLACEMENT_3D ( 'NONE', #25561, #12795, #42864 ) ;
#70675 = CARTESIAN_POINT ( 'NONE',  ( 10.00000000000000000, 8.840884882376133902, -74.65374052328640175 ) ) ;
#70677 = DIRECTION ( 'NONE',  ( -1.000000000000000000, 0.000000000000000000, 0.000000000000000000 ) ) ;
#70678 = DIRECTION ( 'NONE',  ( -1.000000000000000000, -0.000000000000000000, -0.000000000000000000 ) ) ;
#70679 = CARTESIAN_POINT ( 'NONE',  ( -94.99999999999997158, -213.0599564267049857, 86.98374999999998636 ) ) ;
#70680 = CARTESIAN_POINT ( 'NONE',  ( -1.250000000000002442, -12.36245420541525242, -1.199999999999999956 ) ) ;
#70681 = ORIENTED_EDGE ( 'NONE', *, *, #38875, .T. ) ;
#70682 = EDGE_CURVE ( 'NONE', #18846, #42329, #19932, .T. ) ;
#70683 = DIRECTION ( 'NONE',  ( -1.000000000000000000, 0.000000000000000000, 0.000000000000000000 ) ) ;
#70684 = CARTESIAN_POINT ( 'NONE',  ( -2.500000000000015543, -73.00000000000001421, -251.7000000000000455 ) ) ;
#70686 = FACE_OUTER_BOUND ( 'NONE', #14011, .T. ) ;
#70685 = CIRCLE ( 'NONE', #10711, 31.99999999999998579 ) ;
#70687 = FACE_OUTER_BOUND ( 'NONE', #23748, .T. ) ;
#70688 = VECTOR ( 'NONE', #28965, 1000.000000000000000 ) ;
#70689 = AXIS2_PLACEMENT_3D ( 'NONE', #54899, #43639, #66561 ) ;
#70690 = AXIS2_PLACEMENT_3D ( 'NONE', #25519, #31157, #54108 ) ;
#70692 = DIRECTION ( 'NONE',  ( 0.000000000000000000, 0.000000000000000000, 1.000000000000000000 ) ) ;
#70691 = CIRCLE ( 'NONE', #15491, 37.49900000000000944 ) ;
#70693 = EDGE_LOOP ( 'NONE', ( #34676, #37341, #20096, #23399, #54978, #51593 ) ) ;
#70694 = CIRCLE ( 'NONE', #16688, 82.00000000000000000 ) ;
#70695 = ADVANCED_FACE ( 'NONE', ( #54526 ), #72537, .T. ) ;
#70696 = LINE ( 'NONE', #59440, #14302 ) ;
#70697 = EDGE_CURVE ( 'NONE', #47426, #27953, #33990, .T. ) ;
#70698 = LINE ( 'NONE', #48158, #22368 ) ;
#70699 = EDGE_LOOP ( 'NONE', ( #46400, #30963, #65080, #69119 ) ) ;
#70700 = VECTOR ( 'NONE', #56586, 1000.000000000000000 ) ;
#70701 = CARTESIAN_POINT ( 'NONE',  ( 92.69370383062501162, -208.6684592857803295, 84.50989583420049200 ) ) ;
#70702 = CARTESIAN_POINT ( 'NONE',  ( 93.84685191531251292, -211.9973110713294489, 89.27239583420049485 ) ) ;
#70703 = ADVANCED_FACE ( 'NONE', ( #14297 ), #2326, .F. ) ;
#70704 = ORIENTED_EDGE ( 'NONE', *, *, #15200, .T. ) ;
#70705 = CARTESIAN_POINT ( 'NONE',  ( -7.499999999999973355, 62.04836822995428491, -189.9999999999999147 ) ) ;
#70706 = ORIENTED_EDGE ( 'NONE', *, *, #6284, .F. ) ;
#70707 = FACE_BOUND ( 'NONE', #22504, .T. ) ;
#70708 = ORIENTED_EDGE ( 'NONE', *, *, #18191, .F. ) ;
#70709 = CARTESIAN_POINT ( 'NONE',  ( -92.69370383062502583, 88.66845928578038638, 81.81114583420048803 ) ) ;
#70710 = ORIENTED_EDGE ( 'NONE', *, *, #67495, .F. ) ;
#70711 = ORIENTED_EDGE ( 'NONE', *, *, #40648, .F. ) ;
#70712 = CARTESIAN_POINT ( 'NONE',  ( -97.64999999999997726, -209.9999719686937567, 87.53937403222815306 ) ) ;
#70713 = ORIENTED_EDGE ( 'NONE', *, *, #4900, .F. ) ;
#70714 = FACE_OUTER_BOUND ( 'NONE', #13707, .T. ) ;
#70715 = CYLINDRICAL_SURFACE ( 'NONE', #28452, 31.99999999999999289 ) ;
#70716 = AXIS2_PLACEMENT_3D ( 'NONE', #12493, #35431, #24163 ) ;
#70717 = ORIENTED_EDGE ( 'NONE', *, *, #2107, .T. ) ;
#70718 = DIRECTION ( 'NONE',  ( 1.000000000000000000, 0.000000000000000000, 0.000000000000000000 ) ) ;
#70719 = EDGE_LOOP ( 'NONE', ( #13708, #28189, #47738, #49733 ) ) ;
#70720 =( BOUNDED_CURVE ( )  B_SPLINE_CURVE ( 2, ( #28449, #22080, #11169, #45774, #28826, #39753, #62704 ),
 .UNSPECIFIED., .F., .F. ) 
 B_SPLINE_CURVE_WITH_KNOTS ( ( 3, 2, 2, 3 ),
 ( 0.4374999999999994449, 0.4444444444444441422, 0.4513888888888888951, 0.4583333333333335924 ),
 .UNSPECIFIED. ) 
 CURVE ( )  GEOMETRIC_REPRESENTATION_ITEM ( )  RATIONAL_B_SPLINE_CURVE ( ( 1.000000000000010658, 0.8660254037844280495, 1.000000000000000000, 0.8660254037844387076, 1.000000000000000000, 0.8660254037844333785, 1.000000000000005329 ) ) 
 REPRESENTATION_ITEM ( '' )  );
#70721 = CARTESIAN_POINT ( 'NONE',  ( 0.000000000000000000, 0.000000000000000000, 0.000000000000000000 ) ) ;
#70722 = VECTOR ( 'NONE', #28221, 1000.000000000000114 ) ;
#70723 = CIRCLE ( 'NONE', #69509, 77.49899999999999523 ) ;
#70724 = VERTEX_POINT ( 'NONE', #54168 ) ;
#70725 = CIRCLE ( 'NONE', #14334, 37.49900000000000944 ) ;
#70726 = CIRCLE ( 'NONE', #6100, 31.99999999999998934 ) ;
#70727 = ORIENTED_EDGE ( 'NONE', *, *, #62325, .F. ) ;
#70728 = EDGE_LOOP ( 'NONE', ( #26338, #40212, #63939, #50933 ) ) ;
#70729 = CARTESIAN_POINT ( 'NONE',  ( 97.30629616937498838, -208.6684592857803011, 79.85322916753379729 ) ) ;
#70730 = CARTESIAN_POINT ( 'NONE',  ( 11.99999999999999822, -70.53064760720297954, -26.01480285779911839 ) ) ;
#70731 = CONTEXT_DEPENDENT_SHAPE_REPRESENTATION ( #32591, #69260 ) ;
#70732 = DIRECTION ( 'NONE',  ( -0.000000000000000000, -0.000000000000000000, 1.000000000000000000 ) ) ;
#70733 = ORIENTED_EDGE ( 'NONE', *, *, #52375, .T. ) ;
#70734 = DIRECTION ( 'NONE',  ( 0.000000000000000000, 0.9969173337331281859, -0.07845909572784182107 ) ) ;
#70735 = FACE_OUTER_BOUND ( 'NONE', #7859, .T. ) ;
#70736 = AXIS2_PLACEMENT_3D ( 'NONE', #55634, #34187, #30 ) ;
#70737 = DIRECTION ( 'NONE',  ( -1.000000000000000000, -0.000000000000000000, -0.000000000000000000 ) ) ;
#70738 = LINE ( 'NONE', #18867, #22858 ) ;
#70739 = CARTESIAN_POINT ( 'NONE',  ( -97.65000000000001990, 88.47002178664754979, 82.43291666666665662 ) ) ;
#70740 = CARTESIAN_POINT ( 'NONE',  ( -97.30629616937495996, -209.9999999999999716, 80.11781250086713158 ) ) ;
#70741 = CARTESIAN_POINT ( 'NONE',  ( -97.30629616937501680, 88.66845928578038638, 79.69447916753381378 ) ) ;
#70742 = EDGE_CURVE ( 'NONE', #9345, #60145, #23850, .T. ) ;
#70743 = ORIENTED_EDGE ( 'NONE', *, *, #30691, .T. ) ;
#70744 = CARTESIAN_POINT ( 'NONE',  ( 96.15314808468748708, 91.99731107132950569, 81.81114583420047381 ) ) ;
#70745 = ORIENTED_EDGE ( 'NONE', *, *, #29923, .T. ) ;
#70746 = DIRECTION ( 'NONE',  ( 0.3853207896976547087, -0.9227826878668540234, 0.000000000000000000 ) ) ;
#70747 = CARTESIAN_POINT ( 'NONE',  ( 10.00000000000000000, -66.50666863321973210, -39.78640506895676765 ) ) ;
#70748 = DIRECTION ( 'NONE',  ( 0.000000000000000000, 0.9510565162951539753, -0.3090169943749460635 ) ) ;
#70749 = LINE ( 'NONE', #53841, #65660 ) ;
#70750 = CARTESIAN_POINT ( 'NONE',  ( -92.69370383062498320, -208.6684592857803295, 83.66322916753381378 ) ) ;
#70751 = AXIS2_PLACEMENT_3D ( 'NONE', #19892, #10102, #33026 ) ;
#70752 = CARTESIAN_POINT ( 'NONE',  ( -1.250000000000002442, -12.36245420541525242, -1.199999999999999956 ) ) ;
#70753 = DIRECTION ( 'NONE',  ( 0.000000000000000000, -0.000000000000000000, 1.000000000000000000 ) ) ;
#70754 = DIRECTION ( 'NONE',  ( 0.000000000000000000, -0.6691306063588569053, -0.7431448254773954654 ) ) ;
#70755 = ORIENTED_EDGE ( 'NONE', *, *, #59013, .F. ) ;
#70756 = AXIS2_PLACEMENT_3D ( 'NONE', #50581, #73506, #11110 ) ;
#70757 = VECTOR ( 'NONE', #2179, 1000.000000000000000 ) ;
#70758 = VERTEX_POINT ( 'NONE', #48513 ) ;
#70759 = CARTESIAN_POINT ( 'NONE',  ( 0.000000000000000000, 46.53671651294032330, -59.03961581697353012 ) ) ;
#70760 = EDGE_CURVE ( 'NONE', #35754, #63709, #72172, .T. ) ;
#70761 = CONICAL_SURFACE ( 'NONE', #5975, 2.055000000000000160, 0.7853981633974479459 ) ;
#70762 = VECTOR ( 'NONE', #20679, 1000.000000000000000 ) ;
#70763 = CARTESIAN_POINT ( 'NONE',  ( 2.047646702416564768, -96.54137380445985173, 5.500000000000000000 ) ) ;
#70764 = ADVANCED_FACE ( 'NONE', ( #8670 ), #55265, .F. ) ;
#70765 = CARTESIAN_POINT ( 'NONE',  ( -3.000000000000000000, 18.84667830672605859, -18.68964196561243796 ) ) ;
#70766 = CARTESIAN_POINT ( 'NONE',  ( -97.30629616937501680, 90.00000000000004263, 85.83281250086714920 ) ) ;
#70767 = FACE_OUTER_BOUND ( 'NONE', #27954, .T. ) ;
#70768 = CARTESIAN_POINT ( 'NONE',  ( 23.49955575014745435, 0.001194404164629722436, -64.00000000000000000 ) ) ;
#70769 = LINE ( 'NONE', #33041, #3788 ) ;
#70770 = CARTESIAN_POINT ( 'NONE',  ( 10.00000000000000000, 0.000000000000000000, 77.49899999999999523 ) ) ;
#70771 = VERTEX_POINT ( 'NONE', #31582 ) ;
#70772 = CARTESIAN_POINT ( 'NONE',  ( -97.30629616937501680, 90.00000000000004263, 76.30781250086714351 ) ) ;
#70773 = EDGE_CURVE ( 'NONE', #52874, #33020, #37617, .T. ) ;
#70774 = EDGE_CURVE ( 'NONE', #61501, #51075, #71796, .T. ) ;
#70775 = LINE ( 'NONE', #65527, #38149 ) ;
#70776 = DIRECTION ( 'NONE',  ( -1.000000000000000000, -0.000000000000000000, 0.000000000000000000 ) ) ;
#70777 = CARTESIAN_POINT ( 'NONE',  ( 97.65000000000000568, -208.4700217866474645, 84.09979166840098230 ) ) ;
#70778 = CARTESIAN_POINT ( 'NONE',  ( -97.64999999992174651, -209.9999869687493685, 79.28395951166956479 ) ) ;
#70779 = CARTESIAN_POINT ( 'NONE',  ( -96.15314808468747287, -208.0026889286704943, 85.25072916753381946 ) ) ;
#70780 = LINE ( 'NONE', #7639, #59309 ) ;
#70781 = AXIS2_PLACEMENT_3D ( 'NONE', #8636, #41724, #65418 ) ;
#70782 = EDGE_CURVE ( 'NONE', #19667, #31764, #22680, .T. ) ;
#70783 = LINE ( 'NONE', #60276, #7007 ) ;
#70784 = VECTOR ( 'NONE', #67003, 1000.000000000000000 ) ;
#70785 = CARTESIAN_POINT ( 'NONE',  ( -93.84685191531248449, -208.0026889286704943, 76.88989583420048746 ) ) ;
#70786 = CARTESIAN_POINT ( 'NONE',  ( 11.99999999999999822, 0.000000000000000000, 0.000000000000000000 ) ) ;
#70787 = ORIENTED_EDGE ( 'NONE', *, *, #34712, .T. ) ;
#70788 = CYLINDRICAL_SURFACE ( 'NONE', #6529, 77.49899999999999523 ) ;
#70789 = LINE ( 'NONE', #1683, #59889 ) ;
#70790 = CIRCLE ( 'NONE', #47995, 23.50000000000489919 ) ;
#70791 = CARTESIAN_POINT ( 'NONE',  ( 10.00000000000000000, 0.000000000000000000, 0.000000000000000000 ) ) ;
#70792 = CIRCLE ( 'NONE', #35966, 15.99999999999999822 ) ;
#70793 = CYLINDRICAL_SURFACE ( 'NONE', #44484, 31.99999999999999289 ) ;
#70794 = CARTESIAN_POINT ( 'NONE',  ( 92.69370383062501162, -209.9999999999999716, 87.26156250086715715 ) ) ;
#70795 = ORIENTED_EDGE ( 'NONE', *, *, #16105, .F. ) ;
#70796 = EDGE_CURVE ( 'NONE', #32443, #38641, #20680, .T. ) ;
#70797 = EDGE_CURVE ( 'NONE', #37666, #14575, #48150, .T. ) ;
#70798 = EDGE_CURVE ( 'NONE', #10460, #72940, #28171, .T. ) ;
#70799 = CARTESIAN_POINT ( 'NONE',  ( 0.000000000000000000, 0.000000000000000000, 0.000000000000000000 ) ) ;
#70800 = ORIENTED_EDGE ( 'NONE', *, *, #46700, .F. ) ;
#70801 = CARTESIAN_POINT ( 'NONE',  ( -15.70000000000000284, -120.0000000000000000, -85.59999999999999432 ) ) ;
#70802 = EDGE_CURVE ( 'NONE', #11565, #47064, #9463, .T. ) ;
#70803 = VERTEX_POINT ( 'NONE', #27802 ) ;
#70804 = AXIS2_PLACEMENT_3D ( 'NONE', #52175, #58944, #70554 ) ;
#70805 = DIRECTION ( 'NONE',  ( -1.000000000000000000, 0.000000000000000000, -0.000000000000000000 ) ) ;
#70806 = VECTOR ( 'NONE', #57119, 1000.000000000000000 ) ;
#70807 = AXIS2_PLACEMENT_3D ( 'NONE', #7687, #19330, #13687 ) ;
#70808 = EDGE_LOOP ( 'NONE', ( #39144, #46964, #68641, #51300 ) ) ;
#70809 = ORIENTED_EDGE ( 'NONE', *, *, #31632, .T. ) ;
#70810 = VECTOR ( 'NONE', #14698, 1000.000000000000000 ) ;
#70811 = EDGE_LOOP ( 'NONE', ( #60871, #484, #73709, #67505 ) ) ;
#70812 = CIRCLE ( 'NONE', #42, 32.00000000000000000 ) ;
#70813 = DIRECTION ( 'NONE',  ( 0.000000000000000000, -0.9510565162951543083, -0.3090169943749448977 ) ) ;
#70814 = ORIENTED_EDGE ( 'NONE', *, *, #751, .F. ) ;
#70815 = ORIENTED_EDGE ( 'NONE', *, *, #58984, .F. ) ;
#70816 = CARTESIAN_POINT ( 'NONE',  ( 96.15314808468748708, 88.00268892867053694, 80.48822916753381662 ) ) ;
#70817 = CARTESIAN_POINT ( 'NONE',  ( 10.00000000000000000, 0.000000000000000000, 0.000000000000000000 ) ) ;
#70818 = CARTESIAN_POINT ( 'NONE',  ( -93.67500000000003979, 92.29496732002878900, 87.96270833506763154 ) ) ;
#70819 = VERTEX_POINT ( 'NONE', #57131 ) ;
#70820 = ORIENTED_EDGE ( 'NONE', *, *, #1764, .F. ) ;
#70821 = ORIENTED_EDGE ( 'NONE', *, *, #13487, .T. ) ;
#70822 = PLANE ( 'NONE',  #70669 ) ;
#70823 = VERTEX_POINT ( 'NONE', #10895 ) ;
#70824 = CARTESIAN_POINT ( 'NONE',  ( 0.000000000000000000, -120.0000000000000000, 99.99999999999957367 ) ) ;
#70825 = CARTESIAN_POINT ( 'NONE',  ( 5.000000000000002665, -74.18225833017913828, 34.94270380257611919 ) ) ;
#70826 = CARTESIAN_POINT ( 'NONE',  ( -96.90895014231846005, 91.56137061862953885, 74.88237134757150670 ) ) ;
#70827 = CARTESIAN_POINT ( 'NONE',  ( 92.34999999999999432, 90.00000000000002842, 78.01437500173430806 ) ) ;
#70828 = CARTESIAN_POINT ( 'NONE',  ( 0.000000000000000000, 0.000000000000000000, 0.000000000000000000 ) ) ;
#70829 = DIRECTION ( 'NONE',  ( 1.000000000000000000, 0.000000000000000000, 0.000000000000000000 ) ) ;
#70830 = LINE ( 'NONE', #2090, #9245 ) ;
#70831 = CARTESIAN_POINT ( 'NONE',  ( -92.34999999999999432, -209.9999999999999716, 78.96687500173429441 ) ) ;
#70832 = CARTESIAN_POINT ( 'NONE',  ( 15.00000000000000000, -19.89357724624986545, 12.59942793731086219 ) ) ;
#70833 = EDGE_CURVE ( 'NONE', #64655, #42450, #73656, .T. ) ;
#70835 = CARTESIAN_POINT ( 'NONE',  ( -93.67500000000003979, 92.29496732002878900, 76.53270833506762472 ) ) ;
#70834 = CARTESIAN_POINT ( 'NONE',  ( 92.34999999999999432, 88.47002178664753558, 76.79729166840095900 ) ) ;
#70836 = VECTOR ( 'NONE', #29019, 1000.000000000000000 ) ;
#70837 = VERTEX_POINT ( 'NONE', #16910 ) ;
#70838 = CARTESIAN_POINT ( 'NONE',  ( 93.84685191531248449, 88.00268892867053694, 75.30239583420048177 ) ) ;
#70839 = CARTESIAN_POINT ( 'NONE',  ( 96.32499999999997442, 92.29496732002878900, 82.16833333333332234 ) ) ;
#70840 = CARTESIAN_POINT ( 'NONE',  ( -4.653126046682595884, -146.1313684676804314, 5.500000000000000000 ) ) ;
#70841 = LINE ( 'NONE', #2100, #51538 ) ;
#70842 = EDGE_CURVE ( 'NONE', #60472, #43729, #19067, .T. ) ;
#70843 = LINE ( 'NONE', #20467, #62685 ) ;
#70844 = CARTESIAN_POINT ( 'NONE',  ( 5.000000000000002665, -39.47590169984897557, 71.87247863392401825 ) ) ;
#70845 = VERTEX_POINT ( 'NONE', #4150 ) ;
#70846 = DIRECTION ( 'NONE',  ( -1.000000000000000000, 0.000000000000000000, 0.000000000000000000 ) ) ;
#70847 = DIRECTION ( 'NONE',  ( -1.000000000000000000, -0.000000000000000000, -0.000000000000000000 ) ) ;
#70848 = ORIENTED_EDGE ( 'NONE', *, *, #49233, .F. ) ;
#70849 = EDGE_CURVE ( 'NONE', #20435, #28882, #61653, .T. ) ;
#70850 = VERTEX_POINT ( 'NONE', #11257 ) ;
#70851 = CIRCLE ( 'NONE', #36025, 82.00000000000000000 ) ;
#70852 = EDGE_CURVE ( 'NONE', #73325, #1386, #33816, .T. ) ;
#70853 = FACE_OUTER_BOUND ( 'NONE', #73127, .T. ) ;
#70854 = CYLINDRICAL_SURFACE ( 'NONE', #64584, 12.50000000000000000 ) ;
#70855 = LINE ( 'NONE', #26481, #56762 ) ;
#70856 = CYLINDRICAL_SURFACE ( 'NONE', #62748, 20.20000000000036522 ) ;
#70857 = CARTESIAN_POINT ( 'NONE',  ( -92.35000000000007958, -208.4700217866474077, 75.76541666666668107 ) ) ;
#70858 = CARTESIAN_POINT ( 'NONE',  ( -97.30629616937497417, -211.3315407142195852, 75.88447916753382572 ) ) ;
#70859 = ORIENTED_EDGE ( 'NONE', *, *, #62424, .T. ) ;
#70860 = CIRCLE ( 'NONE', #10883, 31.99999999999997868 ) ;
#70861 = EDGE_CURVE ( 'NONE', #53187, #59102, #4524, .T. ) ;
#70862 = DIRECTION ( 'NONE',  ( -1.000000000000000000, -0.000000000000000000, 0.000000000000000000 ) ) ;
#70863 = DIRECTION ( 'NONE',  ( 1.000000000000000000, -0.000000000000000000, 0.000000000000000000 ) ) ;
#70864 =( LENGTH_UNIT ( ) NAMED_UNIT ( * ) SI_UNIT ( .MILLI., .METRE. ) );
#70865 = DIRECTION ( 'NONE',  ( -1.000000000000000000, -0.000000000000000000, 0.000000000000000000 ) ) ;
#70866 = DIRECTION ( 'NONE',  ( -0.000000000000000000, 0.000000000000000000, 1.000000000000000000 ) ) ;
#70867 = CARTESIAN_POINT ( 'NONE',  ( 10.00000000000000000, -37.01155633439063308, 6.555932627142289526 ) ) ;
#70868 = DIRECTION ( 'NONE',  ( -1.000000000000000000, -0.000000000000000000, -0.000000000000000000 ) ) ;
#70869 = VECTOR ( 'NONE', #28565, 1000.000000000000000 ) ;
#70870 = CARTESIAN_POINT ( 'NONE',  ( -97.64999999996706492, -209.9999916046304520, 84.99910573338409847 ) ) ;
#70871 = CIRCLE ( 'NONE', #30024, 12.50000000000000000 ) ;
#70872 = FACE_OUTER_BOUND ( 'NONE', #63924, .T. ) ;
#70873 = CARTESIAN_POINT ( 'NONE',  ( 0.000000000000000000, 0.000000000000000000, 0.000000000000000000 ) ) ;
#70874 = ADVANCED_FACE ( 'NONE', ( #33430 ), #68786, .F. ) ;
#70875 = EDGE_CURVE ( 'NONE', #56348, #68435, #16523, .T. ) ;
#70876 = CARTESIAN_POINT ( 'NONE',  ( 92.69370383062498320, 91.33154071421968467, 84.66864583420047552 ) ) ;
#70877 = CARTESIAN_POINT ( 'NONE',  ( -96.15314808468745866, -211.9973110713294489, 87.36739583420049371 ) ) ;
#70878 = DIRECTION ( 'NONE',  ( -1.000000000000000000, 0.000000000000000000, 0.000000000000000000 ) ) ;
#70879 = ORIENTED_EDGE ( 'NONE', *, *, #56467, .T. ) ;
#70880 = DIRECTION ( 'NONE',  ( -1.000000000000000000, -0.000000000000000000, -0.000000000000000000 ) ) ;
#70881 = CARTESIAN_POINT ( 'NONE',  ( -96.32499999999996021, -207.7050326799711968, 80.36916666666665776 ) ) ;
#70882 = CARTESIAN_POINT ( 'NONE',  ( -95.00000000000002842, 87.33691857156074434, 75.83156250086715033 ) ) ;
#70883 = EDGE_CURVE ( 'NONE', #36601, #46616, #39843, .T. ) ;
#70884 = CARTESIAN_POINT ( 'NONE',  ( 96.15314808468748708, -208.0026889286704943, 85.62114583420046188 ) ) ;
#70885 = EDGE_LOOP ( 'NONE', ( #48889, #6576, #54735, #17818 ) ) ;
#70886 = EDGE_CURVE ( 'NONE', #71645, #9962, #5270, .T. ) ;
#70887 = CARTESIAN_POINT ( 'NONE',  ( 0.000000000000000000, 0.000000000000000000, 0.000000000000000000 ) ) ;
#70888 = ORIENTED_EDGE ( 'NONE', *, *, #12068, .F. ) ;
#70889 = VERTEX_POINT ( 'NONE', #27046 ) ;
#70890 = EDGE_CURVE ( 'NONE', #67705, #14575, #56323, .T. ) ;
#70891 = CIRCLE ( 'NONE', #56485, 77.49900000000000944 ) ;
#70892 = FACE_OUTER_BOUND ( 'NONE', #14909, .T. ) ;
#70893 = PLANE ( 'NONE',  #24651 ) ;
#70894 = VECTOR ( 'NONE', #64026, 1000.000000000000000 ) ;
#70895 = ORIENTED_EDGE ( 'NONE', *, *, #12913, .T. ) ;
#70896 = DIRECTION ( 'NONE',  ( 0.000000000000000000, 0.000000000000000000, 1.000000000000000000 ) ) ;
#70897 = CARTESIAN_POINT ( 'NONE',  ( 95.00000000000000000, -212.6630814284392557, 79.80031250086715033 ) ) ;
#70898 = DIRECTION ( 'NONE',  ( 1.000000000000000000, 0.000000000000000000, 0.000000000000000000 ) ) ;
#70899 = CARTESIAN_POINT ( 'NONE',  ( 4.999999999999999112, 9.188173127307898369, -40.98264845739739570 ) ) ;
#70900 = CARTESIAN_POINT ( 'NONE',  ( 92.34999999999995168, -211.5299782133524502, 80.52791666666665549 ) ) ;
#70901 = LINE ( 'NONE', #1793, #19492 ) ;
#70902 = LINE ( 'NONE', #54367, #27336 ) ;
#70903 = CARTESIAN_POINT ( 'NONE',  ( 93.67500000000001137, -212.2949673200287179, 86.29583333333333428 ) ) ;
#70904 = VECTOR ( 'NONE', #11232, 1000.000000000000000 ) ;
#70905 = ORIENTED_EDGE ( 'NONE', *, *, #12964, .F. ) ;
#70906 = ORIENTED_EDGE ( 'NONE', *, *, #14243, .T. ) ;
#70907 = VERTEX_POINT ( 'NONE', #62794 ) ;
#70908 = VERTEX_POINT ( 'NONE', #27421 ) ;
#70909 = CARTESIAN_POINT ( 'NONE',  ( 10.00000000000000000, 0.000000000000000000, 0.000000000000000000 ) ) ;
#70910 = VECTOR ( 'NONE', #47559, 1000.000000000000000 ) ;
#70911 = CIRCLE ( 'NONE', #38518, 82.00000000000000000 ) ;
#70912 = CARTESIAN_POINT ( 'NONE',  ( -95.00000000000002842, 87.33691857156074434, 82.97531250086716170 ) ) ;
#70913 = DIRECTION ( 'NONE',  ( -1.000000000000000000, 0.000000000000000000, -0.000000000000000000 ) ) ;
#70914 = AXIS2_PLACEMENT_3D ( 'NONE', #23279, #46209, #68406 ) ;
#70915 = DIRECTION ( 'NONE',  ( 0.000000000000000000, 0.000000000000000000, 1.000000000000000000 ) ) ;
#70916 = DIRECTION ( 'NONE',  ( -1.000000000000000000, 0.000000000000000000, -0.000000000000000000 ) ) ;
#70917 = VERTEX_POINT ( 'NONE', #50358 ) ;
#70918 = CARTESIAN_POINT ( 'NONE',  ( -93.67499999999998295, -207.7050326799711968, 88.59770833506763665 ) ) ;
#70919 = ORIENTED_EDGE ( 'NONE', *, *, #57960, .F. ) ;
#70920 = FACE_OUTER_BOUND ( 'NONE', #35019, .T. ) ;
#70921 = EDGE_LOOP ( 'NONE', ( #69463, #54844, #984, #73618 ) ) ;
#70922 = CARTESIAN_POINT ( 'NONE',  ( -92.35000000000005116, 91.52997821335253548, 84.73479166840097321 ) ) ;
#70923 = CARTESIAN_POINT ( 'NONE',  ( 92.69370383062498320, 90.00000000000002842, 86.62656250086715204 ) ) ;
#70924 = CARTESIAN_POINT ( 'NONE',  ( 11.99999999999999822, -73.44644590900043113, -24.73286445877782924 ) ) ;
#70925 = DIRECTION ( 'NONE',  ( -0.7950889364178796992, 0.6064928550163511956, 0.000000000000000000 ) ) ;
#70926 = DIRECTION ( 'NONE',  ( 0.000000000000000000, 0.000000000000000000, -1.000000000000000000 ) ) ;
#70927 = EDGE_CURVE ( 'NONE', #4461, #43683, #50290, .T. ) ;
#70928 = CARTESIAN_POINT ( 'NONE',  ( 10.00000000000000000, 0.000000000000000000, 0.000000000000000000 ) ) ;
#70929 = ORIENTED_EDGE ( 'NONE', *, *, #72115, .T. ) ;
#70930 = CARTESIAN_POINT ( 'NONE',  ( 0.000000000000000000, -76.66974797899844418, 11.30684508768314522 ) ) ;
#70931 = CARTESIAN_POINT ( 'NONE',  ( -7.499999999999973355, 62.04836822995428491, -269.9999999999999432 ) ) ;
#70932 = ORIENTED_EDGE ( 'NONE', *, *, #40686, .T. ) ;
#70933 = ADVANCED_FACE ( 'NONE', ( #38721 ), #10138, .T. ) ;
#70934 = VERTEX_POINT ( 'NONE', #51474 ) ;
#70935 = CARTESIAN_POINT ( 'NONE',  ( 92.34999999999999432, 90.00000000000002842, 78.64937500173429896 ) ) ;
#70936 = EDGE_CURVE ( 'NONE', #59759, #39476, #69514, .T. ) ;
#70937 = DIRECTION ( 'NONE',  ( 0.000000000000000000, -0.1564344650402170189, -0.9876883405951399908 ) ) ;
#70938 = CARTESIAN_POINT ( 'NONE',  ( -97.65000000000001990, 89.99998767024830215, 75.47437542817787914 ) ) ;
#70939 = CARTESIAN_POINT ( 'NONE',  ( -92.69370383062498320, -208.6684592857803011, 86.99697916753382287 ) ) ;
#70940 = VERTEX_POINT ( 'NONE', #22927 ) ;
#70941 = CARTESIAN_POINT ( 'NONE',  ( -14.87942725330654348, -141.9795960975983178, 5.500000000000000000 ) ) ;
#70942 = VERTEX_POINT ( 'NONE', #45862 ) ;
#70943 = ORIENTED_EDGE ( 'NONE', *, *, #72943, .T. ) ;
#70944 = CIRCLE ( 'NONE', #25345, 82.00000000000000000 ) ;
#70945 = AXIS2_PLACEMENT_3D ( 'NONE', #56152, #11037, #67055 ) ;
#70946 = CARTESIAN_POINT ( 'NONE',  ( 10.00000000000000000, 18.89407956138256139, 75.16055320797038064 ) ) ;
#70947 = AXIS2_PLACEMENT_3D ( 'NONE', #45655, #55803, #9930 ) ;
#70948 = CARTESIAN_POINT ( 'NONE',  ( 96.15314808468748708, 91.99731107132950569, 88.95489583420049939 ) ) ;
#70949 = CARTESIAN_POINT ( 'NONE',  ( 22.08297821871651934, -111.8242998470044540, 2.500000000000000000 ) ) ;
#70950 = CARTESIAN_POINT ( 'NONE',  ( 92.69370383062498320, 90.00000000000002842, 82.65781250086713783 ) ) ;
#70951 = CARTESIAN_POINT ( 'NONE',  ( -15.70000000000041140, -119.9999999999998721, -74.99999999999958789 ) ) ;
#70952 = LINE ( 'NONE', #36011, #27763 ) ;
#70953 = CARTESIAN_POINT ( 'NONE',  ( 10.00000000000000000, -35.91791733033525702, 68.67312586194982771 ) ) ;
#70954 = CARTESIAN_POINT ( 'NONE',  ( -92.35000000053409508, 90.00005320149026034, 78.96687695417308817 ) ) ;
#70955 = CYLINDRICAL_SURFACE ( 'NONE', #11220, 42.00000000000000000 ) ;
#70956 = CYLINDRICAL_SURFACE ( 'NONE', #21351, 0.5000000000000004441 ) ;
#70957 = DIRECTION ( 'NONE',  ( 0.000000000000000000, 0.000000000000000000, 1.000000000000000000 ) ) ;
#70958 =( BOUNDED_CURVE ( )  B_SPLINE_CURVE ( 2, ( #72329, #64856, #24987, #32100, #48295, #59207, #71581 ),
 .UNSPECIFIED., .F., .F. ) 
 B_SPLINE_CURVE_WITH_KNOTS ( ( 3, 2, 2, 3 ),
 ( 0.7831899741065915244, 0.7902457405788252398, 0.7973015061197076259, 0.8043570860654229993 ),
 .UNSPECIFIED. ) 
 CURVE ( )  GEOMETRIC_REPRESENTATION_ITEM ( )  RATIONAL_B_SPLINE_CURVE ( ( 1.000000000000000000, 0.8660254037844387076, 1.000000000000000000, 0.8660254037844387076, 1.000000000000000000, 0.8660289278581059236, 0.9999929520380603787 ) ) 
 REPRESENTATION_ITEM ( '' )  );
#70959 = CYLINDRICAL_SURFACE ( 'NONE', #25208, 16.00000000000000355 ) ;
#70960 = PRODUCT_DEFINITION_CONTEXT ( 'detailed design', #66202, 'design' ) ;
#70961 = PRESENTATION_LAYER_ASSIGNMENT (  '', '', ( #61378 ) ) ;
#70962 = CARTESIAN_POINT ( 'NONE',  ( -3.000000000000000000, -10.45096189432314837, -21.10159698893440350 ) ) ;
#70963 = VERTEX_POINT ( 'NONE', #72898 ) ;
#70964 = CARTESIAN_POINT ( 'NONE',  ( -92.69370383062504004, 90.00000000000004263, 87.42031250086714067 ) ) ;
#70965 = AXIS2_PLACEMENT_3D ( 'NONE', #54588, #60248, #8727 ) ;
#70966 = EDGE_CURVE ( 'NONE', #27457, #5237, #41944, .T. ) ;
#70967 = EDGE_CURVE ( 'NONE', #9139, #61669, #73161, .T. ) ;
#70968 = CARTESIAN_POINT ( 'NONE',  ( -94.99999999999997158, -209.9999999999999716, 90.00000000000000000 ) ) ;
#70969 = CIRCLE ( 'NONE', #39760, 31.99999999999998934 ) ;
#70970 = CARTESIAN_POINT ( 'NONE',  ( -97.65000000002611102, 89.99999999999995737, -65.00000000000007105 ) ) ;
#70971 = EDGE_CURVE ( 'NONE', #53879, #35308, #53968, .T. ) ;
#70972 = VERTEX_POINT ( 'NONE', #1130 ) ;
#70973 = AXIS2_PLACEMENT_3D ( 'NONE', #49975, #14663, #8666 ) ;
#70974 = DIRECTION ( 'NONE',  ( 0.1276937514489679681, 0.9918136447140103451, 0.000000000000000000 ) ) ;
#70975 = LINE ( 'NONE', #52212, #50368 ) ;
#70976 = DIRECTION ( 'NONE',  ( 1.000000000000000000, 0.000000000000000000, 0.000000000000000000 ) ) ;
#70977 = CARTESIAN_POINT ( 'NONE',  ( 92.69370383062501162, -208.6684592857803011, 80.85864583420048746 ) ) ;
#70978 = ORIENTED_EDGE ( 'NONE', *, *, #61713, .T. ) ;
#70979 = ORIENTED_EDGE ( 'NONE', *, *, #49325, .T. ) ;
#70980 = CARTESIAN_POINT ( 'NONE',  ( -5.000000000000000000, -2.886751345948133540, -6.000000000000000000 ) ) ;
#70981 = VERTEX_POINT ( 'NONE', #40203 ) ;
#70982 = DIRECTION ( 'NONE',  ( -1.000000000000000000, 0.000000000000000000, 0.000000000000000000 ) ) ;
#70983 = DIRECTION ( 'NONE',  ( -1.000000000000000000, 0.000000000000000000, -0.000000000000000000 ) ) ;
#70984 = ORIENTED_EDGE ( 'NONE', *, *, #17143, .T. ) ;
#70985 = CARTESIAN_POINT ( 'NONE',  ( 95.00000000000000000, -212.6630814284392557, 81.07031250086716057 ) ) ;
#70986 = VECTOR ( 'NONE', #35074, 1000.000000000000000 ) ;
#70987 = VERTEX_POINT ( 'NONE', #58595 ) ;
#70988 = DIRECTION ( 'NONE',  ( 1.000000000000000000, 0.000000000000000000, 0.000000000000000000 ) ) ;
#70989 = VERTEX_POINT ( 'NONE', #53329 ) ;
#70990 = AXIS2_PLACEMENT_3D ( 'NONE', #69135, #51087, #45469 ) ;
#70991 = ORIENTED_EDGE ( 'NONE', *, *, #52432, .T. ) ;
#70992 = FACE_OUTER_BOUND ( 'NONE', #19407, .T. ) ;
#70993 =( NAMED_UNIT ( * ) PLANE_ANGLE_UNIT ( ) SI_UNIT ( $, .RADIAN. ) );
#70994 = LINE ( 'NONE', #8219, #41341 ) ;
#70995 = VERTEX_POINT ( 'NONE', #1866 ) ;
#70996 = DIRECTION ( 'NONE',  ( -1.000000000000000000, -0.000000000000000000, 0.000000000000000000 ) ) ;
#70997 = CARTESIAN_POINT ( 'NONE',  ( 92.35000000000002274, -208.4700217866474645, 83.04145833506763097 ) ) ;
#70998 = CARTESIAN_POINT ( 'NONE',  ( 94.99999999999998579, 86.94004357329500010, 83.80875000000000341 ) ) ;
#70999 = B_SPLINE_CURVE_WITH_KNOTS ( 'NONE', 1,
 ( #22844, #67953 ),
 .UNSPECIFIED., .F., .F.,
 ( 2, 2 ),
 ( 0.000000000000000000, 1.000000000000000000 ),
 .UNSPECIFIED. ) ;
#71000 = VERTEX_POINT ( 'NONE', #28915 ) ;
#71001 = FACE_OUTER_BOUND ( 'NONE', #71834, .T. ) ;
#71002 = CIRCLE ( 'NONE', #36193, 16.00000000000000000 ) ;
#71003 = LINE ( 'NONE', #152, #16518 ) ;
#71004 = VERTEX_POINT ( 'NONE', #12723 ) ;
#71005 = ORIENTED_EDGE ( 'NONE', *, *, #68668, .F. ) ;
#71006 = CARTESIAN_POINT ( 'NONE',  ( -95.00000000000002842, 87.33691857156074434, 87.42031250086715488 ) ) ;
#71007 = CARTESIAN_POINT ( 'NONE',  ( 94.99999999999998579, 87.33691857156068750, 80.91156250086714863 ) ) ;
#71008 = ORIENTED_EDGE ( 'NONE', *, *, #29269, .F. ) ;
#71009 = CARTESIAN_POINT ( 'NONE',  ( 93.67499999999999716, 87.70503267997126784, 87.64520833506762187 ) ) ;
#71010 = EDGE_CURVE ( 'NONE', #34381, #50235, #29274, .T. ) ;
#71011 = ORIENTED_EDGE ( 'NONE', *, *, #28074, .T. ) ;
#71012 = FACE_BOUND ( 'NONE', #22742, .T. ) ;
#71013 = AXIS2_PLACEMENT_3D ( 'NONE', #68182, #56546, #66701 ) ;
#71014 = VERTEX_POINT ( 'NONE', #34551 ) ;
#71015 = AXIS2_PLACEMENT_3D ( 'NONE', #69814, #18316, #1812 ) ;
#71016 = ORIENTED_EDGE ( 'NONE', *, *, #25114, .F. ) ;
#71017 = ADVANCED_FACE ( 'NONE', ( #69507 ), #57866, .T. ) ;
#71018 = ORIENTED_EDGE ( 'NONE', *, *, #46944, .F. ) ;
#71019 = DIRECTION ( 'NONE',  ( 0.000000000000000000, 1.000000000000000000, 1.445602896647339410E-16 ) ) ;
#71020 = AXIS2_PLACEMENT_3D ( 'NONE', #52864, #53975, #7370 ) ;
#71021 = CARTESIAN_POINT ( 'NONE',  ( 10.00000000000000000, 0.000000000000000000, 0.000000000000000000 ) ) ;
#71022 = EDGE_CURVE ( 'NONE', #1974, #45793, #17891, .T. ) ;
#71023 = CARTESIAN_POINT ( 'NONE',  ( -93.67500000000003979, 92.29496732002878900, 85.34333333333333371 ) ) ;
#71024 = ORIENTED_EDGE ( 'NONE', *, *, #66406, .T. ) ;
#71025 = CARTESIAN_POINT ( 'NONE',  ( 12.00000000000000000, 16.83928648764922542, -16.46020748918050458 ) ) ;
#71026 = CARTESIAN_POINT ( 'NONE',  ( 10.00000000000000000, 0.000000000000000000, 0.000000000000000000 ) ) ;
#71027 = ORIENTED_EDGE ( 'NONE', *, *, #55184, .T. ) ;
#71028 = CARTESIAN_POINT ( 'NONE',  ( 15.00000000000000000, 22.07842321921480888, -8.187992925817425771 ) ) ;
#71029 = CARTESIAN_POINT ( 'NONE',  ( -96.15314808468745866, -211.9973110713294489, 82.76364583420047438 ) ) ;
#71031 = ORIENTED_EDGE ( 'NONE', *, *, #42049, .F. ) ;
#71030 = EDGE_CURVE ( 'NONE', #3728, #68597, #41309, .T. ) ;
#71032 = CARTESIAN_POINT ( 'NONE',  ( 3.429551818649054340, -146.3199197248623875, 5.500000000000000000 ) ) ;
#71033 = CARTESIAN_POINT ( 'NONE',  ( 10.00000000000000000, 77.16300072079661732, 27.74655509720697921 ) ) ;
#71034 = FACE_OUTER_BOUND ( 'NONE', #19472, .T. ) ;
#71035 = DIRECTION ( 'NONE',  ( -1.000000000000000000, 0.000000000000000000, 0.000000000000000000 ) ) ;
#71036 = EDGE_CURVE ( 'NONE', #64851, #34378, #19117, .T. ) ;
#71037 = DIRECTION ( 'NONE',  ( 1.000000000000000000, 0.000000000000000000, 0.000000000000000000 ) ) ;
#71038 = CARTESIAN_POINT ( 'NONE',  ( -14.87942725330654348, -141.9795960975983178, 5.500000000000000000 ) ) ;
#71039 = DIRECTION ( 'NONE',  ( -1.000000000000000000, -0.000000000000000000, -0.000000000000000000 ) ) ;
#71040 = ADVANCED_FACE ( 'NONE', ( #24389 ), #18732, .T. ) ;
#71041 = DIRECTION ( 'NONE',  ( 0.000000000000000000, 0.8526401643540935105, -0.5224985647159468005 ) ) ;
#71042 = EDGE_CURVE ( 'NONE', #73588, #17434, #47949, .T. ) ;
#71043 = CARTESIAN_POINT ( 'NONE',  ( -92.69370383062502583, 91.33154071421968467, 76.67822916753378593 ) ) ;
#71044 = CYLINDRICAL_SURFACE ( 'NONE', #21470, 31.99999999999998579 ) ;
#71045 = LINE ( 'NONE', #8271, #24229 ) ;
#71046 = DIRECTION ( 'NONE',  ( 7.962523111838990267E-16, 1.065814103640131188E-14, 1.000000000000000000 ) ) ;
#71047 = DIRECTION ( 'NONE',  ( 0.000000000000000000, 0.000000000000000000, 1.000000000000000000 ) ) ;
#71048 = VECTOR ( 'NONE', #58656, 1000.000000000000000 ) ;
#71049 = FACE_OUTER_BOUND ( 'NONE', #58832, .T. ) ;
#71050 = EDGE_CURVE ( 'NONE', #30425, #41023, #38340, .T. ) ;
#71051 = EDGE_CURVE ( 'NONE', #32190, #6126, #59927, .T. ) ;
#71052 = CARTESIAN_POINT ( 'NONE',  ( 96.90829729882861443, 88.16127723153182671, 74.99954709728268654 ) ) ;
#71053 = DIRECTION ( 'NONE',  ( 0.000000000000000000, -0.6494480483301739993, -0.7604059656000392575 ) ) ;
#71054 = AXIS2_PLACEMENT_3D ( 'NONE', #42496, #19183, #70297 ) ;
#71055 = CARTESIAN_POINT ( 'NONE',  ( 11.99999999999999822, -62.20884554313985149, -46.21855187248698371 ) ) ;
#71056 = CARTESIAN_POINT ( 'NONE',  ( -97.64999999999996305, -209.9999999999999716, 87.45999999999999375 ) ) ;
#71057 = DIRECTION ( 'NONE',  ( -0.9781476007338042455, -0.2079116908177664758, 0.000000000000000000 ) ) ;
#71058 = AXIS2_PLACEMENT_3D ( 'NONE', #44957, #38571, #55857 ) ;
#71059 = ORIENTED_EDGE ( 'NONE', *, *, #50656, .F. ) ;
#71060 = CARTESIAN_POINT ( 'NONE',  ( -10.94538922500103162, 0.000000000000000000, 0.000000000000000000 ) ) ;
#71061 = DIRECTION ( 'NONE',  ( -1.000000000000000000, -0.000000000000000000, 0.000000000000000000 ) ) ;
#71062 = CARTESIAN_POINT ( 'NONE',  ( 0.000000000000000000, 22.90783923731741112, -78.73519480814930205 ) ) ;
#71063 = PLANE ( 'NONE',  #54537 ) ;
#71064 = AXIS2_PLACEMENT_3D ( 'NONE', #10952, #33877, #57189 ) ;
#71065 = AXIS2_PLACEMENT_3D ( 'NONE', #32913, #63018, #257 ) ;
#71066 = ORIENTED_EDGE ( 'NONE', *, *, #73213, .T. ) ;
#71067 = CARTESIAN_POINT ( 'NONE',  ( 0.000000000000000000, 0.000000000000000000, 0.000000000000000000 ) ) ;
#71068 = CARTESIAN_POINT ( 'NONE',  ( 11.99999999999999822, -36.72794159290197769, -65.59268652807249111 ) ) ;
#71069 = ORIENTED_EDGE ( 'NONE', *, *, #70966, .T. ) ;
#71070 = CARTESIAN_POINT ( 'NONE',  ( 93.84685191531249870, -208.0026889286704943, 82.55197916753380127 ) ) ;
#71071 = CARTESIAN_POINT ( 'NONE',  ( 97.30629616937498838, -209.9999999999999716, 88.21406250086714351 ) ) ;
#71072 = ORIENTED_EDGE ( 'NONE', *, *, #22132, .T. ) ;
#71073 = CARTESIAN_POINT ( 'NONE',  ( 92.69370383062501162, -209.9999999999999716, 88.53156250086716739 ) ) ;
#71074 = EDGE_LOOP ( 'NONE', ( #57367, #62281, #64532, #14613 ) ) ;
#71075 = DIRECTION ( 'NONE',  ( -1.000000000000000000, -0.000000000000000000, -0.000000000000000000 ) ) ;
#71076 = VERTEX_POINT ( 'NONE', #69150 ) ;
#71077 = CARTESIAN_POINT ( 'NONE',  ( -92.69370383062504004, 90.00000000000004263, 76.14906250086716000 ) ) ;
#71078 = VERTEX_POINT ( 'NONE', #17638 ) ;
#71079 = VERTEX_POINT ( 'NONE', #40953 ) ;
#71080 = DIRECTION ( 'NONE',  ( -1.000000000000000000, 0.000000000000000000, 0.000000000000000000 ) ) ;
#71081 = ADVANCED_FACE ( 'NONE', ( #46579 ), #40570, .T. ) ;
#71082 = ORIENTED_EDGE ( 'NONE', *, *, #39739, .F. ) ;
#71083 = CARTESIAN_POINT ( 'NONE',  ( 92.35000000001610942, 89.99999393654047708, 88.17456390440148084 ) ) ;
#71084 = DIRECTION ( 'NONE',  ( -1.000000000000000000, 0.000000000000000000, 0.000000000000000000 ) ) ;
#71085 = EDGE_CURVE ( 'NONE', #42391, #28639, #871, .T. ) ;
#71086 = EDGE_LOOP ( 'NONE', ( #29740, #38086, #27875, #49845 ) ) ;
#71087 = DIRECTION ( 'NONE',  ( -1.000000000000000000, 0.000000000000000000, 0.000000000000000000 ) ) ;
#71088 = EDGE_CURVE ( 'NONE', #39517, #61033, #58228, .T. ) ;
#71089 = VERTEX_POINT ( 'NONE', #8582 ) ;
#71090 = DIRECTION ( 'NONE',  ( 0.000000000000000000, 0.000000000000000000, -1.000000000000000000 ) ) ;
#71091 = ORIENTED_EDGE ( 'NONE', *, *, #43825, .T. ) ;
#71092 = ADVANCED_FACE ( 'NONE', ( #2613 ), #2969, .T. ) ;
#71093 = ORIENTED_EDGE ( 'NONE', *, *, #73574, .T. ) ;
#71094 = EDGE_LOOP ( 'NONE', ( #28043, #50977, #36492, #36076 ) ) ;
#71095 = CARTESIAN_POINT ( 'NONE',  ( 92.69370383062501162, -208.6684592857803011, 79.42989583420046529 ) ) ;
#71096 = CARTESIAN_POINT ( 'NONE',  ( -97.65000000000001990, 90.00000000000004263, 83.65000000000000568 ) ) ;
#71097 = CARTESIAN_POINT ( 'NONE',  ( -95.00000000000002842, 86.94004357329504273, 81.90375000000000227 ) ) ;
#71098 = ORIENTED_EDGE ( 'NONE', *, *, #56100, .F. ) ;
#71100 = DIRECTION ( 'NONE',  ( -1.000000000000000000, 0.000000000000000000, -0.000000000000000000 ) ) ;
#71099 = CIRCLE ( 'NONE', #14657, 42.00000000000000000 ) ;
#71101 = DIRECTION ( 'NONE',  ( 0.000000000000000000, 0.000000000000000000, 1.000000000000000000 ) ) ;
#71102 = ADVANCED_FACE ( 'NONE', ( #25856, #14954 ), #26226, .F. ) ;
#71103 = DIRECTION ( 'NONE',  ( 0.000000000000000000, 0.000000000000000000, -1.000000000000000000 ) ) ;
#71104 = DIRECTION ( 'NONE',  ( -1.000000000000000000, 0.000000000000000000, -0.000000000000000000 ) ) ;
#71105 = DIRECTION ( 'NONE',  ( 0.000000000000000000, 0.4539904997395413644, 0.8910065241883706744 ) ) ;
#71106 = CARTESIAN_POINT ( 'NONE',  ( -94.99999999999997158, -212.6630814284392557, 79.64156250086713840 ) ) ;
#71107 = CARTESIAN_POINT ( 'NONE',  ( -97.30629616937501680, 88.66845928578038638, 79.05947916753382287 ) ) ;
#71108 = AXIS2_PLACEMENT_3D ( 'NONE', #15574, #44148, #15940 ) ;
#71109 = ORIENTED_EDGE ( 'NONE', *, *, #34550, .F. ) ;
#71110 = CARTESIAN_POINT ( 'NONE',  ( 94.99999999999998579, 92.66308142843935514, 82.49906250086714010 ) ) ;
#71111 = AXIS2_PLACEMENT_3D ( 'NONE', #714, #6683, #34142 ) ;
#71112 = ORIENTED_EDGE ( 'NONE', *, *, #36711, .F. ) ;
#71113 = DIRECTION ( 'NONE',  ( -0.5200609990132993854, -0.8541291221503275466, 0.000000000000000000 ) ) ;
#71114 = DIRECTION ( 'NONE',  ( -1.000000000000000000, -0.000000000000000000, -0.000000000000000000 ) ) ;
#71115 = EDGE_CURVE ( 'NONE', #59392, #24150, #11392, .T. ) ;
#71116 = FACE_BOUND ( 'NONE', #14235, .T. ) ;
#71117 = DIRECTION ( 'NONE',  ( 0.08130631524010117905, -0.9966891607226784355, 0.000000000000000000 ) ) ;
#71118 = CARTESIAN_POINT ( 'NONE',  ( 0.000000000000000000, -39.47590169984795239, -71.87247863392457248 ) ) ;
#71119 = CARTESIAN_POINT ( 'NONE',  ( -92.69370383062498320, -209.9999999999999716, 83.61031250086713840 ) ) ;
#71120 = B_SPLINE_CURVE_WITH_KNOTS ( 'NONE', 3,
 ( #22156, #45096, #74015, #28520, #68769, #45474, #68400, #51459, #16, #17257, #40192, #63141, #11594, #379, #40552, #63503, #41652, #25109, #19461, #25479 ),
 .UNSPECIFIED., .F., .F.,
 ( 4, 2, 2, 2, 2, 2, 2, 2, 2, 4 ),
 ( 2.781148923614798380E-07, 0.0008372784139766645825, 0.001674278713060967658, 0.002511279012145270842, 0.003348279311229572942, 0.003766779460771723775, 0.004185279610313873307, 0.005022279909398174105, 0.005859280208482472302, 0.006696280507566771366 ),
 .UNSPECIFIED. ) ;
#71121 = CARTESIAN_POINT ( 'NONE',  ( 0.000000000000000000, -19.89357724625003598, 12.59942793731059574 ) ) ;
#71122 = VECTOR ( 'NONE', #35218, 1000.000000000000000 ) ;
#71123 = CARTESIAN_POINT ( 'NONE',  ( 10.00000000000000000, 0.000000000000000000, 0.000000000000000000 ) ) ;
#71124 = VERTEX_POINT ( 'NONE', #60824 ) ;
#71125 = AXIS2_PLACEMENT_3D ( 'NONE', #16588, #40638, #458 ) ;
#71126 = ORIENTED_EDGE ( 'NONE', *, *, #12323, .F. ) ;
#71127 = CARTESIAN_POINT ( 'NONE',  ( 10.00000000000000000, -4.992566952385247170, 37.16516213103275845 ) ) ;
#71128 = DIRECTION ( 'NONE',  ( -0.000000000000000000, -0.000000000000000000, -1.000000000000000000 ) ) ;
#71129 = ADVANCED_FACE ( 'NONE', ( #7833 ), #42790, .T. ) ;
#71130 = CARTESIAN_POINT ( 'NONE',  ( -97.65000000000001990, 90.00000000000004263, 77.93499999999998806 ) ) ;
#71131 = EDGE_CURVE ( 'NONE', #21230, #69181, #37115, .T. ) ;
#71132 = CARTESIAN_POINT ( 'NONE',  ( -97.30629616937501680, 88.66845928578038638, 85.88572916753382458 ) ) ;
#71133 = DIRECTION ( 'NONE',  ( -0.2867529058022035837, 0.9580045777625452175, 0.000000000000000000 ) ) ;
#71134 = CARTESIAN_POINT ( 'NONE',  ( 10.00000000000000000, 0.000000000000000000, 0.000000000000000000 ) ) ;
#71135 = LINE ( 'NONE', #19637, #7270 ) ;
#71136 = VERTEX_POINT ( 'NONE', #65361 ) ;
#71137 = CARTESIAN_POINT ( 'NONE',  ( -97.30629616937501680, 88.66845928578038638, 75.72572916753381378 ) ) ;
#71138 = CARTESIAN_POINT ( 'NONE',  ( 11.99999999999999822, 55.16347631943131091, -60.67117009219074930 ) ) ;
#71139 = DIRECTION ( 'NONE',  ( -1.000000000000000000, -0.000000000000000000, 0.000000000000000000 ) ) ;
#71140 = CARTESIAN_POINT ( 'NONE',  ( -5.000000000000000000, 2.886751345948126879, -2.079999999999992077 ) ) ;
#71141 = DIRECTION ( 'NONE',  ( 1.000000000000000000, -0.000000000000000000, -0.000000000000000000 ) ) ;
#71142 = DIRECTION ( 'NONE',  ( 1.000000000000000000, -7.571541139944063212E-15, -2.603472992745718510E-14 ) ) ;
#71143 = CARTESIAN_POINT ( 'NONE',  ( -96.15314808468747287, -208.0026889286704943, 82.07572916753382231 ) ) ;
#71144 = CARTESIAN_POINT ( 'NONE',  ( 0.000000000000000000, -14.67089635893764665, 73.72996012237435082 ) ) ;
#71145 = B_SPLINE_CURVE_WITH_KNOTS ( 'NONE', 1,
 ( #50054, #56471 ),
 .UNSPECIFIED., .F., .F.,
 ( 2, 2 ),
 ( 0.000000000000000000, 1.000000000000000000 ),
 .UNSPECIFIED. ) ;
#71146 = CARTESIAN_POINT ( 'NONE',  ( 92.69370383062498320, 90.00000000000002842, 75.19656250086714522 ) ) ;
#71147 = DIRECTION ( 'NONE',  ( -1.000000000000000000, -0.000000000000000000, 0.000000000000000000 ) ) ;
#71148 = CARTESIAN_POINT ( 'NONE',  ( -3.000000000000000000, 18.84667830672579925, 18.68964196561269020 ) ) ;
#71149 = ORIENTED_EDGE ( 'NONE', *, *, #31396, .T. ) ;
#71150 = STYLED_ITEM ( 'NONE', ( #64928 ), #55235 ) ;
#71151 = CARTESIAN_POINT ( 'NONE',  ( -96.32499999999996021, -212.2949673200287179, 81.93020833506763267 ) ) ;
#71152 = CARTESIAN_POINT ( 'NONE',  ( -3.000000000000000000, 24.81905959214261514, 9.408202855044825341 ) ) ;
#71153 = CARTESIAN_POINT ( 'NONE',  ( 11.99999999999999822, 0.000000000000000000, 0.000000000000000000 ) ) ;
#71154 = AXIS2_PLACEMENT_3D ( 'NONE', #56588, #51296, #34756 ) ;
#71155 = FACE_OUTER_BOUND ( 'NONE', #46264, .T. ) ;
#71156 = CARTESIAN_POINT ( 'NONE',  ( 95.00000000000000000, -207.3369185715606307, 89.00781250086716057 ) ) ;
#71157 = VERTEX_POINT ( 'NONE', #36394 ) ;
#71158 = ADVANCED_FACE ( 'NONE', ( #13827 ), #71711, .F. ) ;
#71159 = DIRECTION ( 'NONE',  ( 0.000000000000000000, 0.000000000000000000, 1.000000000000000000 ) ) ;
#71160 = SURFACE_STYLE_USAGE ( .BOTH. , #8026 ) ;
#71161 = ORIENTED_EDGE ( 'NONE', *, *, #28931, .F. ) ;
#71162 = VECTOR ( 'NONE', #39014, 1000.000000000000000 ) ;
#71163 =( BOUNDED_CURVE ( )  B_SPLINE_CURVE ( 2, ( #56221, #44579, #18129, #12477, #21242, #35416, #44197, #67123, #38560 ),
 .UNSPECIFIED., .F., .F. ) 
 B_SPLINE_CURVE_WITH_KNOTS ( ( 3, 2, 2, 2, 3 ),
 ( 0.5715170088666294834, 0.5785727743523534361, 0.5856285398932349340, 0.5926843054341166539, 0.5926843883797353607 ),
 .UNSPECIFIED. ) 
 CURVE ( )  GEOMETRIC_REPRESENTATION_ITEM ( )  RATIONAL_B_SPLINE_CURVE ( ( 1.000000000000000000, 0.8660254037844387076, 1.000000000000000000, 0.8660254037844387076, 1.000000000000000000, 0.8660254037844387076, 1.000000000000000000, 0.9999984250318816326, 0.9999968501007930888 ) ) 
 REPRESENTATION_ITEM ( '' )  );
#71164 = FACE_OUTER_BOUND ( 'NONE', #58316, .T. ) ;
#71165 = ORIENTED_EDGE ( 'NONE', *, *, #40427, .T. ) ;
#71166 = CIRCLE ( 'NONE', #24347, 31.99999999999998934 ) ;
#71167 = DIRECTION ( 'NONE',  ( 0.000000000000000000, 0.7071067811865439090, 0.7071067811865512365 ) ) ;
#71168 = EDGE_LOOP ( 'NONE', ( #63113, #22191, #52731, #70275 ) ) ;
#71169 = EDGE_LOOP ( 'NONE', ( #66769, #12456, #23502, #10244 ) ) ;
#71170 = EDGE_CURVE ( 'NONE', #58503, #49949, #58738, .T. ) ;
#71171 = ORIENTED_EDGE ( 'NONE', *, *, #70971, .T. ) ;
#71172 = CARTESIAN_POINT ( 'NONE',  ( 0.000000000000000000, 0.000000000000000000, 0.000000000000000000 ) ) ;
#71173 = EDGE_CURVE ( 'NONE', #64110, #25146, #25492, .T. ) ;
#71174 = ORIENTED_EDGE ( 'NONE', *, *, #23211, .F. ) ;
#71175 = ORIENTED_EDGE ( 'NONE', *, *, #38084, .T. ) ;
#71176 = CARTESIAN_POINT ( 'NONE',  ( 94.99999999999998579, 87.33691857156068750, 79.80031250086715033 ) ) ;
#71177 = FACE_BOUND ( 'NONE', #16907, .T. ) ;
#71178 = CARTESIAN_POINT ( 'NONE',  ( -97.64999999998390479, 89.99999393654049129, 88.17456390440148084 ) ) ;
#71179 = EDGE_LOOP ( 'NONE', ( #44308, #42356, #40149, #44863 ) ) ;
#71180 = EDGE_CURVE ( 'NONE', #37092, #55893, #32314, .T. ) ;
#71181 = ORIENTED_EDGE ( 'NONE', *, *, #7478, .F. ) ;
#71182 = EDGE_CURVE ( 'NONE', #14677, #8861, #59344, .T. ) ;
#71183 = ORIENTED_EDGE ( 'NONE', *, *, #59032, .T. ) ;
#71184 = DIRECTION ( 'NONE',  ( -0.2867529058022021404, 0.9580045777625456616, 0.000000000000000000 ) ) ;
#71185 = ORIENTED_EDGE ( 'NONE', *, *, #70936, .T. ) ;
#71186 = CARTESIAN_POINT ( 'NONE',  ( 0.000000000000000000, -120.0000000000000000, -40.00000000000001421 ) ) ;
#71187 = LINE ( 'NONE', #70825, #70301 ) ;
#71188 = DIRECTION ( 'NONE',  ( 0.000000000000000000, -0.7071067811865389130, -0.7071067811865561215 ) ) ;
#71189 = DIRECTION ( 'NONE',  ( 1.427937372958396981E-15, -1.000000000000000000, 1.065814103640131031E-14 ) ) ;
#71190 = DIRECTION ( 'NONE',  ( 0.000000000000000000, 0.000000000000000000, -1.000000000000000000 ) ) ;
#71191 = DIRECTION ( 'NONE',  ( 1.000000000000000000, -0.000000000000000000, 0.000000000000000000 ) ) ;
#71192 = LINE ( 'NONE', #67046, #63509 ) ;
#71193 = CARTESIAN_POINT ( 'NONE',  ( -92.34999999999999432, -209.9999999999999716, 75.79187500173429726 ) ) ;
#71194 = CARTESIAN_POINT ( 'NONE',  ( -93.84685191531254134, 91.99731107132950569, 88.31989583420048007 ) ) ;
#71195 = CIRCLE ( 'NONE', #54420, 37.49900000000000944 ) ;
#71197 = CARTESIAN_POINT ( 'NONE',  ( -97.65000000000001990, 88.47002178664754979, 74.89229166840097207 ) ) ;
#71196 = CARTESIAN_POINT ( 'NONE',  ( 93.67499999999998295, 92.29496732002878900, 76.63854166840096127 ) ) ;
#71198 = ORIENTED_EDGE ( 'NONE', *, *, #65438, .T. ) ;
#71199 = CARTESIAN_POINT ( 'NONE',  ( 93.84685191531248449, 91.99731107132950569, 75.72572916753382799 ) ) ;
#71200 = EDGE_CURVE ( 'NONE', #41863, #64009, #3533, .T. ) ;
#71201 = DIRECTION ( 'NONE',  ( 0.000000000000000000, -0.9135454576426015327, 0.4067366430757989315 ) ) ;
#71202 = CYLINDRICAL_SURFACE ( 'NONE', #35489, 31.99999999999999289 ) ;
#71203 = CARTESIAN_POINT ( 'NONE',  ( 97.65000000000000568, -208.4700217866474645, 77.11479166840095445 ) ) ;
#71204 = FACE_OUTER_BOUND ( 'NONE', #18675, .T. ) ;
#71205 = CARTESIAN_POINT ( 'NONE',  ( 0.000000000000000000, 0.000000000000000000, 125.0000000000000000 ) ) ;
#71206 = PRODUCT_DEFINITION_FORMATION_WITH_SPECIFIED_SOURCE ( 'ANY', '', #71551, .NOT_KNOWN. ) ;
#71207 = VERTEX_POINT ( 'NONE', #32226 ) ;
#71208 = CARTESIAN_POINT ( 'NONE',  ( 11.99999999999999822, 71.27951684758026829, 30.41916302227139113 ) ) ;
#71209 = CARTESIAN_POINT ( 'NONE',  ( 26.47460221209471598, -121.8961639463267090, -5.500000000000000000 ) ) ;
#71210 = ORIENTED_EDGE ( 'NONE', *, *, #9071, .F. ) ;
#71211 = EDGE_LOOP ( 'NONE', ( #36223, #56636, #20778, #20636 ) ) ;
#71212 = ADVANCED_FACE ( 'NONE', ( #3701 ), #36769, .T. ) ;
#71213 = CARTESIAN_POINT ( 'NONE',  ( 11.99999999999999822, -41.19522573413780009, 65.64334221924896440 ) ) ;
#71214 = CARTESIAN_POINT ( 'NONE',  ( 96.32499999999998863, -207.7050326799711968, 82.80333333333332746 ) ) ;
#71215 = DIRECTION ( 'NONE',  ( -1.000000000000000000, -0.000000000000000000, 0.000000000000000000 ) ) ;
#71216 = DIRECTION ( 'NONE',  ( -1.000000000000000000, 0.000000000000000000, 0.000000000000000000 ) ) ;
#71217 = CARTESIAN_POINT ( 'NONE',  ( -97.65000000000001990, 88.47002178664754979, 76.16229166840095388 ) ) ;
#71218 = AXIS2_PLACEMENT_3D ( 'NONE', #59457, #58711, #18481 ) ;
#71219 = CARTESIAN_POINT ( 'NONE',  ( -97.30629616937495996, -209.9999999999999716, 75.19656250086714522 ) ) ;
#71220 = EDGE_CURVE ( 'NONE', #23150, #41879, #34750, .T. ) ;
#71221 = VECTOR ( 'NONE', #40468, 1000.000000000000000 ) ;
#71222 = VERTEX_POINT ( 'NONE', #42421 ) ;
#71223 = CARTESIAN_POINT ( 'NONE',  ( 10.00000000000000000, -30.84782396557201878, -21.32104025579148399 ) ) ;
#71224 = CIRCLE ( 'NONE', #35226, 77.49899999999998101 ) ;
#71225 = CIRCLE ( 'NONE', #54440, 82.00000000000000000 ) ;
#71226 = CIRCLE ( 'NONE', #65249, 37.49900000000000233 ) ;
#71227 = CARTESIAN_POINT ( 'NONE',  ( -3.000000000000000000, -19.89357724625003598, 12.59942793731059574 ) ) ;
#71228 = CARTESIAN_POINT ( 'NONE',  ( -0.1219594728601508804, -118.5049662589159567, 2.500000000000000000 ) ) ;
#71229 = PLANE ( 'NONE',  #53687 ) ;
#71230 = DIRECTION ( 'NONE',  ( 1.000000000000000000, 0.000000000000000000, 0.000000000000000000 ) ) ;
#71231 = CARTESIAN_POINT ( 'NONE',  ( -90.00000000000002842, 85.00000000000002842, 90.00000000000000000 ) ) ;
#71232 = DIRECTION ( 'NONE',  ( 0.000000000000000000, 0.000000000000000000, 1.000000000000000000 ) ) ;
#71233 = FACE_OUTER_BOUND ( 'NONE', #31236, .T. ) ;
#71234 = CARTESIAN_POINT ( 'NONE',  ( -3.000000000000000000, 0.000000000000000000, 0.000000000000000000 ) ) ;
#71235 = CARTESIAN_POINT ( 'NONE',  ( 96.15314808468748708, 91.99731107132950569, 83.23989583420049598 ) ) ;
#71236 = CARTESIAN_POINT ( 'NONE',  ( -93.84685191531247028, -211.9973110713294489, 86.83822916753382515 ) ) ;
#71237 = CARTESIAN_POINT ( 'NONE',  ( 92.35004149907325655, -211.5300021728535285, 83.78229332575388355 ) ) ;
#71238 = ORIENTED_EDGE ( 'NONE', *, *, #32503, .F. ) ;
#71239 = DIRECTION ( 'NONE',  ( 0.9435911131814395114, -0.3311129884571304971, 0.000000000000000000 ) ) ;
#71240 = CARTESIAN_POINT ( 'NONE',  ( -96.32499999999996021, -207.7050326799711968, 81.63916666666666799 ) ) ;
#71241 = CARTESIAN_POINT ( 'NONE',  ( -92.69370383062504004, 90.00000000000004263, 75.99031250086714806 ) ) ;
#71242 = CARTESIAN_POINT ( 'NONE',  ( 97.30629616937498838, -208.6684592857803011, 84.93322916753379559 ) ) ;
#71243 = VERTEX_POINT ( 'NONE', #59716 ) ;
#71244 = VECTOR ( 'NONE', #62759, 1000.000000000000000 ) ;
#71245 = DIRECTION ( 'NONE',  ( -1.000000000000000000, 0.000000000000000000, -0.000000000000000000 ) ) ;
#71246 = EDGE_LOOP ( 'NONE', ( #72586, #47876, #39938, #26615 ) ) ;
#71247 = ORIENTED_EDGE ( 'NONE', *, *, #45611, .F. ) ;
#71248 = AXIS2_PLACEMENT_3D ( 'NONE', #31669, #47859, #18545 ) ;
#71249 = ORIENTED_EDGE ( 'NONE', *, *, #53570, .T. ) ;
#71250 = ADVANCED_FACE ( 'NONE', ( #48789 ), #19108, .F. ) ;
#71251 = CARTESIAN_POINT ( 'NONE',  ( -96.32500000000001705, 87.70503267997129626, 79.39020833506762642 ) ) ;
#71252 = CIRCLE ( 'NONE', #38872, 77.49899999999999523 ) ;
#71253 = EDGE_CURVE ( 'NONE', #32106, #45883, #45557, .T. ) ;
#71254 = ORIENTED_EDGE ( 'NONE', *, *, #27324, .T. ) ;
#71255 = CARTESIAN_POINT ( 'NONE',  ( 11.99999999999999822, -68.26794271651239399, -31.47745569255214093 ) ) ;
#71256 = CARTESIAN_POINT ( 'NONE',  ( 97.30629616937498838, -208.6684592857803295, 78.10697916753383652 ) ) ;
#71257 = ADVANCED_FACE ( 'NONE', ( #32608 ), #68322, .T. ) ;
#71258 = DIRECTION ( 'NONE',  ( 0.000000000000000000, -0.2334453638559127742, 0.9723699203976748917 ) ) ;
#71259 = CARTESIAN_POINT ( 'NONE',  ( -12.50000000000000000, 1.530808498934191521E-15, 0.000000000000000000 ) ) ;
#71260 = CIRCLE ( 'NONE', #7640, 31.99999999999999289 ) ;
#71261 = CARTESIAN_POINT ( 'NONE',  ( 0.000000000000000000, -23.16143007188479075, 73.95703589263966649 ) ) ;
#71262 = CARTESIAN_POINT ( 'NONE',  ( -10.00000000000000000, 0.000000000000000000, 0.000000000000000000 ) ) ;
#71263 = CIRCLE ( 'NONE', #62959, 42.00000000000000000 ) ;
#71264 = CARTESIAN_POINT ( 'NONE',  ( 10.00000000000000000, 10.96151621346540317, -35.95386929396244113 ) ) ;
#71265 = CARTESIAN_POINT ( 'NONE',  ( 93.67500000000001137, -212.2949673200287179, 79.94583333333332575 ) ) ;
#71266 = EDGE_LOOP ( 'NONE', ( #35868, #43646, #23994 ) ) ;
#71267 = ADVANCED_FACE ( 'NONE', ( #43911 ), #49894, .T. ) ;
#71268 = ORIENTED_EDGE ( 'NONE', *, *, #62822, .T. ) ;
#71269 = EDGE_LOOP ( 'NONE', ( #51012, #19630, #16846, #21630, #73890 ) ) ;
#71270 = AXIS2_PLACEMENT_3D ( 'NONE', #66810, #60440, #37507 ) ;
#71271 = ORIENTED_EDGE ( 'NONE', *, *, #46212, .T. ) ;
#71272 = CARTESIAN_POINT ( 'NONE',  ( -7.500000000000016875, -80.00000000000001421, -269.9999999999999432 ) ) ;
#71273 = CIRCLE ( 'NONE', #501, 31.99999999999999289 ) ;
#71274 = CARTESIAN_POINT ( 'NONE',  ( -95.00000000000002842, 92.66308142843932671, 82.65781250086715204 ) ) ;
#71275 = CYLINDRICAL_SURFACE ( 'NONE', #55463, 16.00000000000000000 ) ;
#71276 = DIRECTION ( 'NONE',  ( -1.000000000000000000, 0.000000000000000000, -0.000000000000000000 ) ) ;
#71277 = CARTESIAN_POINT ( 'NONE',  ( 94.99999999999998579, 93.05995642670504253, 75.23624999999999829 ) ) ;
#71278 = ORIENTED_EDGE ( 'NONE', *, *, #2266, .T. ) ;
#71279 = CARTESIAN_POINT ( 'NONE',  ( -94.99999999999997158, -213.0599564267049857, 87.69812500173429726 ) ) ;
#71280 = ORIENTED_EDGE ( 'NONE', *, *, #59971, .T. ) ;
#71281 = CYLINDRICAL_SURFACE ( 'NONE', #15811, 37.49900000000000233 ) ;
#71282 = EDGE_CURVE ( 'NONE', #14214, #52264, #62409, .T. ) ;
#71283 = ORIENTED_EDGE ( 'NONE', *, *, #2409, .T. ) ;
#71284 = CARTESIAN_POINT ( 'NONE',  ( -97.65000000000001990, 88.47002178664754979, 85.68729166840097378 ) ) ;
#71285 = VERTEX_POINT ( 'NONE', #39375 ) ;
#71286 = CARTESIAN_POINT ( 'NONE',  ( 93.84685191531248449, 88.00268892867053694, 86.09739583420049769 ) ) ;
#71287 = EDGE_CURVE ( 'NONE', #2959, #14681, #45603, .T. ) ;
#71288 = EDGE_CURVE ( 'NONE', #48188, #39963, #44408, .T. ) ;
#71289 = DIRECTION ( 'NONE',  ( -1.000000000000000000, 0.000000000000000000, 0.000000000000000000 ) ) ;
#71290 = AXIS2_PLACEMENT_3D ( 'NONE', #62742, #22878, #45813 ) ;
#71291 = DIRECTION ( 'NONE',  ( 0.000000000000000000, -0.4539904997395542430, 0.8910065241883641241 ) ) ;
#71292 = DIRECTION ( 'NONE',  ( 0.000000000000000000, 0.8090169943749447867, 0.5877852522924769119 ) ) ;
#71293 = DIRECTION ( 'NONE',  ( -1.000000000000000000, 0.000000000000000000, -0.000000000000000000 ) ) ;
#71294 = VERTEX_POINT ( 'NONE', #72812 ) ;
#71295 = FACE_OUTER_BOUND ( 'NONE', #26959, .T. ) ;
#71296 = CARTESIAN_POINT ( 'NONE',  ( -92.69370383062498320, -208.6684592857803011, 74.77322916753379900 ) ) ;
#71297 = ORIENTED_EDGE ( 'NONE', *, *, #60380, .F. ) ;
#71298 = ORIENTED_EDGE ( 'NONE', *, *, #45669, .F. ) ;
#71299 = FACE_BOUND ( 'NONE', #63842, .T. ) ;
#71300 = EDGE_CURVE ( 'NONE', #73482, #65810, #1204, .T. ) ;
#71301 = CARTESIAN_POINT ( 'NONE',  ( -2.500000000000020428, -90.00000000000000000, -310.0000000000000000 ) ) ;
#71302 = CIRCLE ( 'NONE', #43749, 42.00000000000000000 ) ;
#71303 = DIRECTION ( 'NONE',  ( -0.000000000000000000, -0.000000000000000000, 1.000000000000000000 ) ) ;
#71304 = CARTESIAN_POINT ( 'NONE',  ( -94.99999999999997158, -212.6630814284392557, 82.97531250086716170 ) ) ;
#71305 = VERTEX_POINT ( 'NONE', #72454 ) ;
#71306 = DIRECTION ( 'NONE',  ( -1.000000000000000000, 0.000000000000000000, 0.000000000000000000 ) ) ;
#71307 = ORIENTED_EDGE ( 'NONE', *, *, #5962, .T. ) ;
#71308 = ORIENTED_EDGE ( 'NONE', *, *, #60061, .T. ) ;
#71309 = CARTESIAN_POINT ( 'NONE',  ( 0.000000000000000000, 27.05870788708231700, 26.08949754953034272 ) ) ;
#71310 = AXIS2_PLACEMENT_3D ( 'NONE', #18758, #52607, #46981 ) ;
#71311 = CARTESIAN_POINT ( 'NONE',  ( 96.15314808468748708, 88.00268892867053694, 89.37822916753381719 ) ) ;
#71312 = DIRECTION ( 'NONE',  ( 0.000000000000000000, 0.000000000000000000, 1.000000000000000000 ) ) ;
#71313 = CARTESIAN_POINT ( 'NONE',  ( 92.69370383062498320, 90.00000000000002842, 80.75281250086715090 ) ) ;
#71314 = CARTESIAN_POINT ( 'NONE',  ( -3.000000000000000000, -0.9646360437372163421, -23.52805723605591126 ) ) ;
#71315 = DIRECTION ( 'NONE',  ( -1.000000000000000000, -0.000000000000000000, 0.000000000000000000 ) ) ;
#71316 = LINE ( 'NONE', #9287, #66141 ) ;
#71317 = DIRECTION ( 'NONE',  ( -1.000000000000000000, 0.000000000000000000, 0.000000000000000000 ) ) ;
#71318 = CARTESIAN_POINT ( 'NONE',  ( 12.74955575014678288, 0.001194404164533373076, 127.4927882439599927 ) ) ;
#71319 = CARTESIAN_POINT ( 'NONE',  ( 11.99999999999999822, -55.38113227695820484, 54.21277698773656084 ) ) ;
#71320 = CIRCLE ( 'NONE', #38926, 82.00000000000000000 ) ;
#71321 = VECTOR ( 'NONE', #52676, 999.9999999999998863 ) ;
#71322 = CARTESIAN_POINT ( 'NONE',  ( 10.00000000000000000, -6.555932627142143865, -37.01155633439065440 ) ) ;
#71323 = DIRECTION ( 'NONE',  ( -4.476705744456276711E-17, 1.000000000000000000, -0.000000000000000000 ) ) ;
#71324 = EDGE_LOOP ( 'NONE', ( #59745, #67597, #60300, #66929 ) ) ;
#71325 = CIRCLE ( 'NONE', #54541, 30.50000000000000000 ) ;
#71326 = CARTESIAN_POINT ( 'NONE',  ( -92.69370383062505425, 91.33154071421968467, 86.20322916753380582 ) ) ;
#71327 = AXIS2_PLACEMENT_3D ( 'NONE', #8486, #54350, #25767 ) ;
#71328 = DIRECTION ( 'NONE',  ( 0.000000000000000000, 0.000000000000000000, 1.000000000000000000 ) ) ;
#71329 = DIRECTION ( 'NONE',  ( -0.000000000000000000, 0.8090169943749426773, 0.5877852522924797984 ) ) ;
#71330 = CIRCLE ( 'NONE', #66585, 15.99999999999999645 ) ;
#71331 = ORIENTED_EDGE ( 'NONE', *, *, #67109, .T. ) ;
#71332 = CARTESIAN_POINT ( 'NONE',  ( 5.000000000000000000, -35.47612816024539484, 22.48208911017487921 ) ) ;
#71333 = CARTESIAN_POINT ( 'NONE',  ( 97.64999999999999147, -210.0000000198592716, 85.95187500101400246 ) ) ;
#71334 = DIRECTION ( 'NONE',  ( 1.000000000000000000, -3.061616997868382648E-16, -0.000000000000000000 ) ) ;
#71335 = VECTOR ( 'NONE', #57994, 1000.000000000000000 ) ;
#71336 = EDGE_CURVE ( 'NONE', #20435, #71438, #29951, .T. ) ;
#71337 = CARTESIAN_POINT ( 'NONE',  ( 93.84685191531249870, -208.0026889286704943, 82.07572916753382231 ) ) ;
#71338 = EDGE_CURVE ( 'NONE', #35131, #40037, #62705, .T. ) ;
#71339 = EDGE_CURVE ( 'NONE', #26229, #24481, #5178, .T. ) ;
#71340 = ORIENTED_EDGE ( 'NONE', *, *, #8804, .F. ) ;
#71341 = EDGE_CURVE ( 'NONE', #15633, #48915, #34098, .T. ) ;
#71342 = ORIENTED_EDGE ( 'NONE', *, *, #41662, .T. ) ;
#71343 = DIRECTION ( 'NONE',  ( 1.000000000000000000, 0.000000000000000000, -0.000000000000000000 ) ) ;
#71344 = EDGE_LOOP ( 'NONE', ( #18171, #17748 ) ) ;
#71345 = AXIS2_PLACEMENT_3D ( 'NONE', #18252, #42311, #41193 ) ;
#71346 = DIRECTION ( 'NONE',  ( 0.000000000000000000, 0.000000000000000000, 1.000000000000000000 ) ) ;
#71347 = ADVANCED_FACE ( 'NONE', ( #27331 ), #73945, .T. ) ;
#71348 = DIRECTION ( 'NONE',  ( -1.000000000000000000, -0.000000000000000000, 0.000000000000000000 ) ) ;
#71349 = VERTEX_POINT ( 'NONE', #50268 ) ;
#71350 =( NAMED_UNIT ( * ) SI_UNIT ( $, .STERADIAN. ) SOLID_ANGLE_UNIT ( ) );
#71351 = CARTESIAN_POINT ( 'NONE',  ( 96.15314808468748708, -208.0026889286704943, 74.98489583420048632 ) ) ;
#71352 = ADVANCED_FACE ( 'NONE', ( #10802 ), #66830, .T. ) ;
#71353 = ORIENTED_EDGE ( 'NONE', *, *, #72872, .F. ) ;
#71354 = PLANE ( 'NONE',  #58763 ) ;
#71355 = ORIENTED_EDGE ( 'NONE', *, *, #60303, .T. ) ;
#71356 = VERTEX_POINT ( 'NONE', #38254 ) ;
#71357 = CARTESIAN_POINT ( 'NONE',  ( 10.00000000000000000, 0.000000000000000000, 0.000000000000000000 ) ) ;
#71358 = VECTOR ( 'NONE', #4092, 1000.000000000000000 ) ;
#71359 = DIRECTION ( 'NONE',  ( 0.000000000000000000, 0.000000000000000000, 1.000000000000000000 ) ) ;
#71360 = ORIENTED_EDGE ( 'NONE', *, *, #13151, .F. ) ;
#71361 = PLANE ( 'NONE',  #12559 ) ;
#71362 = CARTESIAN_POINT ( 'NONE',  ( 97.64999999999997726, -211.5299782133524502, 82.72395833506762131 ) ) ;
#71363 = CARTESIAN_POINT ( 'NONE',  ( 96.32499999999998863, 87.70503267997126784, 85.76666666666665151 ) ) ;
#71364 = VERTEX_POINT ( 'NONE', #73199 ) ;
#71365 = CARTESIAN_POINT ( 'NONE',  ( -92.35000000000003695, 90.00000000000004263, 85.87249999999998806 ) ) ;
#71366 = CARTESIAN_POINT ( 'NONE',  ( -93.67500000000003979, 87.70503267997129626, 75.05104166840095559 ) ) ;
#71367 = ORIENTED_EDGE ( 'NONE', *, *, #64967, .F. ) ;
#71368 = ORIENTED_EDGE ( 'NONE', *, *, #44025, .F. ) ;
#71369 = CARTESIAN_POINT ( 'NONE',  ( -93.84685191531254134, 91.99731107132950569, 86.41489583420049314 ) ) ;
#71370 = CIRCLE ( 'NONE', #36607, 12.50000000000000000 ) ;
#71371 = CARTESIAN_POINT ( 'NONE',  ( 93.84685191531248449, 91.99731107132950569, 80.64697916753381435 ) ) ;
#71372 = ADVANCED_FACE ( 'NONE', ( #16817 ), #56679, .T. ) ;
#71373 = CIRCLE ( 'NONE', #19755, 31.99999999999999289 ) ;
#71374 = ORIENTED_EDGE ( 'NONE', *, *, #14696, .F. ) ;
#71375 = ADVANCED_FACE ( 'NONE', ( #28082 ), #67199, .T. ) ;
#71376 = CARTESIAN_POINT ( 'NONE',  ( 92.34999999999999432, 90.00000000000002842, 84.36437500173430237 ) ) ;
#71377 = CARTESIAN_POINT ( 'NONE',  ( 10.00000000000000000, 30.41916302227113178, 71.27951684758036777 ) ) ;
#71378 = EDGE_LOOP ( 'NONE', ( #2803, #62082, #41682, #37361 ) ) ;
#71379 = CARTESIAN_POINT ( 'NONE',  ( 93.67500000000001137, -212.2949673200287179, 78.04083333333333883 ) ) ;
#71380 = EDGE_CURVE ( 'NONE', #12604, #1097, #22802, .T. ) ;
#71382 = EDGE_CURVE ( 'NONE', #51520, #21663, #59166, .T. ) ;
#71381 = CIRCLE ( 'NONE', #34207, 82.00000000000000000 ) ;
#71383 = ORIENTED_EDGE ( 'NONE', *, *, #24841, .F. ) ;
#71384 = VERTEX_POINT ( 'NONE', #46129 ) ;
#71385 = ORIENTED_EDGE ( 'NONE', *, *, #7456, .T. ) ;
#71386 = DIRECTION ( 'NONE',  ( -1.000000000000000000, 0.000000000000000000, -0.000000000000000000 ) ) ;
#71387 = CARTESIAN_POINT ( 'NONE',  ( 0.000000000000000000, 2.956366410620650420, 75.11725578898469280 ) ) ;
#71388 = CARTESIAN_POINT ( 'NONE',  ( -96.32500000000001705, 87.70503267997129626, 85.66083333333332916 ) ) ;
#71389 = ORIENTED_EDGE ( 'NONE', *, *, #43736, .T. ) ;
#71390 = EDGE_CURVE ( 'NONE', #42798, #32631, #1691, .T. ) ;
#71391 = FACE_OUTER_BOUND ( 'NONE', #45596, .T. ) ;
#71392 = CARTESIAN_POINT ( 'NONE',  ( 7.468086116107294004, -12.33868914344945189, -1.199999999999999956 ) ) ;
#71393 = ORIENTED_EDGE ( 'NONE', *, *, #49957, .F. ) ;
#71394 =( BOUNDED_CURVE ( )  B_SPLINE_CURVE ( 2, ( #71096, #24512, #47811, #7955, #25618, #65120, #13595 ),
 .UNSPECIFIED., .F., .F. ) 
 B_SPLINE_CURVE_WITH_KNOTS ( ( 3, 2, 2, 3 ),
 ( 0.4166666666666662966, 0.4236111111111106609, 0.4305555555555550806, 0.4374999999999994449 ),
 .UNSPECIFIED. ) 
 CURVE ( )  GEOMETRIC_REPRESENTATION_ITEM ( )  RATIONAL_B_SPLINE_CURVE ( ( 1.000000000000007550, 0.8660254037844311581, 1.000000000000000000, 0.8660254037844387076, 1.000000000000000000, 0.8660254037844493658, 0.9999999999999893419 ) ) 
 REPRESENTATION_ITEM ( '' )  );
#71395 = CARTESIAN_POINT ( 'NONE',  ( 92.35000000000000853, -211.5299782133525071, 84.97291666666667709 ) ) ;
#71396 = CARTESIAN_POINT ( 'NONE',  ( -97.30629616937497417, -211.3315407142195852, 78.26572916753380582 ) ) ;
#71397 = ORIENTED_EDGE ( 'NONE', *, *, #22772, .F. ) ;
#71398 = CARTESIAN_POINT ( 'NONE',  ( -2.499999999999997780, 8.494897427831771708, 0.000000000000000000 ) ) ;
#71399 = CYLINDRICAL_SURFACE ( 'NONE', #66881, 31.99999999999998579 ) ;
#71400 = LINE ( 'NONE', #1927, #15257 ) ;
#71401 = CARTESIAN_POINT ( 'NONE',  ( 0.000000000000000000, -68.67312586194971402, -35.91791733033549860 ) ) ;
#71402 = AXIS2_PLACEMENT_3D ( 'NONE', #71841, #66234, #53825 ) ;
#71403 = DIRECTION ( 'NONE',  ( -0.000000000000000000, -0.000000000000000000, -1.000000000000000000 ) ) ;
#71404 = CYLINDRICAL_SURFACE ( 'NONE', #56564, 77.49899999999999523 ) ;
#71405 = LINE ( 'NONE', #69932, #72022 ) ;
#71406 = CARTESIAN_POINT ( 'NONE',  ( 0.000000000000000000, -120.0000000000000000, 125.0000000000000000 ) ) ;
#71407 = FACE_OUTER_BOUND ( 'NONE', #64940, .T. ) ;
#71408 = CARTESIAN_POINT ( 'NONE',  ( 11.99999999999999822, 8.840884882375075193, 74.65374052328651544 ) ) ;
#71409 = CARTESIAN_POINT ( 'NONE',  ( -96.15314808468751551, 88.00268892867056536, 89.27239583420049485 ) ) ;
#71410 = CARTESIAN_POINT ( 'NONE',  ( 0.000000000000000000, -73.72996012237449293, 14.67089635893687571 ) ) ;
#71411 = CYLINDRICAL_SURFACE ( 'NONE', #71054, 82.00000000000000000 ) ;
#71412 = PLANE ( 'NONE',  #36773 ) ;
#71413 = UNCERTAINTY_MEASURE_WITH_UNIT (LENGTH_MEASURE( 1.000000000000000082E-05 ), #30320, 'distance_accuracy_value', 'NONE');
#71414 = DIRECTION ( 'NONE',  ( 0.000000000000000000, -0.2079116908177641998, -0.9781476007338046896 ) ) ;
#71415 = LINE ( 'NONE', #58675, #22085 ) ;
#71416 = LINE ( 'NONE', #73554, #46628 ) ;
#71417 = DIRECTION ( 'NONE',  ( -1.000000000000000000, 0.000000000000000000, 0.000000000000000000 ) ) ;
#71418 = LINE ( 'NONE', #59799, #62230 ) ;
#71419 = CARTESIAN_POINT ( 'NONE',  ( 94.99999999999998579, 86.94004357329502852, 75.63312500173429953 ) ) ;
#71420 = CARTESIAN_POINT ( 'NONE',  ( -92.34999999999999432, -209.9999999999999716, 87.14249999999999829 ) ) ;
#71421 = FACE_OUTER_BOUND ( 'NONE', #12561, .T. ) ;
#71422 = VERTEX_POINT ( 'NONE', #13657 ) ;
#71423 = AXIS2_PLACEMENT_3D ( 'NONE', #275, #69028, #17513 ) ;
#71424 = DIRECTION ( 'NONE',  ( 0.000000000000000000, 0.000000000000000000, -1.000000000000000000 ) ) ;
#71425 = CIRCLE ( 'NONE', #18631, 31.99999999999999289 ) ;
#71426 = DIRECTION ( 'NONE',  ( 0.000000000000000000, -1.000000000000000000, 0.000000000000000000 ) ) ;
#71427 = DIRECTION ( 'NONE',  ( 0.000000000000000000, 0.000000000000000000, 1.000000000000000000 ) ) ;
#71428 = CARTESIAN_POINT ( 'NONE',  ( -92.35000000000005116, 91.52997821335254969, 84.65541666666669585 ) ) ;
#71429 = ADVANCED_FACE ( 'NONE', ( #7657 ), #13292, .T. ) ;
#71430 = AXIS2_PLACEMENT_3D ( 'NONE', #54800, #3330, #49524 ) ;
#71431 = ADVANCED_FACE ( 'NONE', ( #59538 ), #36591, .F. ) ;
#71432 = CIRCLE ( 'NONE', #60683, 15.99999999999999822 ) ;
#71433 = EDGE_CURVE ( 'NONE', #2268, #42999, #58791, .T. ) ;
#71434 = VERTEX_POINT ( 'NONE', #57778 ) ;
#71435 = ADVANCED_FACE ( 'NONE', ( #30942, #24943 ), #11529, .F. ) ;
#71436 = CARTESIAN_POINT ( 'NONE',  ( 8.000000000000021316, 1.526494338673934908E-13, 13.10000000000024301 ) ) ;
#71437 = PLANE ( 'NONE',  #49941 ) ;
#71438 = VERTEX_POINT ( 'NONE', #8025 ) ;
#71439 =( REPRESENTATION_RELATIONSHIP ('NONE','NONE', #31117, #54059 ) REPRESENTATION_RELATIONSHIP_WITH_TRANSFORMATION ( #53821 )SHAPE_REPRESENTATION_RELATIONSHIP( ) );
#71440 = CARTESIAN_POINT ( 'NONE',  ( 97.30629616937498838, -208.6684592857803295, 80.48822916753380241 ) ) ;
#71441 = CARTESIAN_POINT ( 'NONE',  ( 97.30629616937498838, -208.6684592857803295, 89.53697916753382913 ) ) ;
#71442 = VERTEX_POINT ( 'NONE', #34463 ) ;
#71443 = CIRCLE ( 'NONE', #39067, 31.99999999999998934 ) ;
#71444 = CARTESIAN_POINT ( 'NONE',  ( 93.84685191531249870, -208.0026889286704943, 87.15572916753382060 ) ) ;
#71445 = ORIENTED_EDGE ( 'NONE', *, *, #52611, .T. ) ;
#71446 = CARTESIAN_POINT ( 'NONE',  ( -97.64999999999996305, -209.9999999999999716, 80.47499999999999432 ) ) ;
#71447 = EDGE_LOOP ( 'NONE', ( #13735, #25468, #11848, #26643 ) ) ;
#71448 = CARTESIAN_POINT ( 'NONE',  ( -97.30629616937501680, 90.00000000000004263, 78.37156250086715659 ) ) ;
#71449 = ORIENTED_EDGE ( 'NONE', *, *, #29498, .T. ) ;
#71450 = VECTOR ( 'NONE', #51737, 1000.000000000000000 ) ;
#71451 = ORIENTED_EDGE ( 'NONE', *, *, #6288, .F. ) ;
#71452 = CYLINDRICAL_SURFACE ( 'NONE', #31671, 37.49900000000000233 ) ;
#71453 = VERTEX_POINT ( 'NONE', #57406 ) ;
#71454 = CARTESIAN_POINT ( 'NONE',  ( 97.64999999999999147, 89.99999996655866141, 87.85687500050293863 ) ) ;
#71455 = CARTESIAN_POINT ( 'NONE',  ( 2.949999999999999734, 0.000000000000000000, 2.699999999999999734 ) ) ;
#71456 = ADVANCED_FACE ( 'NONE', ( #51382 ), #17545, .F. ) ;
#71457 = ORIENTED_EDGE ( 'NONE', *, *, #52567, .F. ) ;
#71458 = DIRECTION ( 'NONE',  ( 0.000000000000000000, -0.000000000000000000, 1.000000000000000000 ) ) ;
#71459 = ORIENTED_EDGE ( 'NONE', *, *, #62659, .T. ) ;
#71460 = CARTESIAN_POINT ( 'NONE',  ( 92.35000000000010800, -211.5299782133525071, 86.24291666666667311 ) ) ;
#71461 = ORIENTED_EDGE ( 'NONE', *, *, #47517, .F. ) ;
#71462 = EDGE_LOOP ( 'NONE', ( #35420, #61770 ) ) ;
#71463 = ORIENTED_EDGE ( 'NONE', *, *, #57212, .F. ) ;
#71464 = CARTESIAN_POINT ( 'NONE',  ( 92.69370383062501162, -211.3315407142195852, 79.53572916753380184 ) ) ;
#71466 = EDGE_CURVE ( 'NONE', #38459, #53810, #22832, .T. ) ;
#71465 = LINE ( 'NONE', #35778, #59303 ) ;
#71467 = ADVANCED_FACE ( 'NONE', ( #68698 ), #11901, .T. ) ;
#71468 = CIRCLE ( 'NONE', #55882, 77.49900000000002365 ) ;
#71469 = CARTESIAN_POINT ( 'NONE',  ( 96.90829729882861443, 88.16127723153182671, 74.99954709728268654 ) ) ;
#71470 = ORIENTED_EDGE ( 'NONE', *, *, #17095, .F. ) ;
#71471 = CARTESIAN_POINT ( 'NONE',  ( -92.34999999999999432, -209.9999999999999716, 78.96687500173429441 ) ) ;
#71472 = VERTEX_POINT ( 'NONE', #63069 ) ;
#71473 = CARTESIAN_POINT ( 'NONE',  ( 0.000000000000000000, 0.000000000000000000, 0.000000000000000000 ) ) ;
#71474 = FACE_OUTER_BOUND ( 'NONE', #55306, .T. ) ;
#71475 = EDGE_LOOP ( 'NONE', ( #15137, #58849, #67490, #65760 ) ) ;
#71476 = CARTESIAN_POINT ( 'NONE',  ( -92.34999999999999432, -208.4700217866474645, 88.54479166840097548 ) ) ;
#71477 = CARTESIAN_POINT ( 'NONE',  ( 0.000000000000000000, -36.88895765772637247, 6.736453364083436313 ) ) ;
#71478 = CARTESIAN_POINT ( 'NONE',  ( -93.84685191531248449, -208.0026889286704943, 79.90614583420047268 ) ) ;
#71479 = CARTESIAN_POINT ( 'NONE',  ( -97.30629616937501680, 91.33154071421968467, 79.58864583420047722 ) ) ;
#71480 = EDGE_LOOP ( 'NONE', ( #1013, #19023, #51662, #3894 ) ) ;
#71481 = CARTESIAN_POINT ( 'NONE',  ( 92.69370383062498320, 90.00000000000002842, 80.11781250086713158 ) ) ;
#71482 = VERTEX_POINT ( 'NONE', #28827 ) ;
#71483 = DIRECTION ( 'NONE',  ( -1.000000000000000000, 0.000000000000000000, 0.000000000000000000 ) ) ;
#71484 = DIRECTION ( 'NONE',  ( 0.000000000000000000, 0.000000000000000000, 1.000000000000000000 ) ) ;
#71485 = CARTESIAN_POINT ( 'NONE',  ( 0.000000000000000000, -0.8299999999999999600, -1.199999999999999956 ) ) ;
#71486 = AXIS2_PLACEMENT_3D ( 'NONE', #63751, #5870, #52831 ) ;
#71487 = DIRECTION ( 'NONE',  ( -1.000000000000000000, -0.000000000000000000, 0.000000000000000000 ) ) ;
#71488 = DIRECTION ( 'NONE',  ( 0.000000000000000000, 0.000000000000000000, 1.000000000000000000 ) ) ;
#71489 = CARTESIAN_POINT ( 'NONE',  ( -92.69370383062498320, -211.3315407142195852, 82.28739583420048120 ) ) ;
#71490 = CARTESIAN_POINT ( 'NONE',  ( -93.67499999999998295, -212.2949673200287179, 89.57666666666666799 ) ) ;
#71491 = DIRECTION ( 'NONE',  ( 0.9848077530122080203, -0.1736481776669309696, 0.000000000000000000 ) ) ;
#71492 = VECTOR ( 'NONE', #38570, 1000.000000000000000 ) ;
#71493 = LINE ( 'NONE', #65147, #10827 ) ;
#71494 = ORIENTED_EDGE ( 'NONE', *, *, #58795, .T. ) ;
#71495 = ORIENTED_EDGE ( 'NONE', *, *, #16210, .T. ) ;
#71496 = FACE_OUTER_BOUND ( 'NONE', #12196, .T. ) ;
#71497 = VECTOR ( 'NONE', #63044, 1000.000000000000000 ) ;
#71498 = CARTESIAN_POINT ( 'NONE',  ( -95.00000000000002842, 86.94004357329504273, 75.55375000000000796 ) ) ;
#71499 = CARTESIAN_POINT ( 'NONE',  ( -95.00000000000002842, 90.00000000000004263, 90.00000000000000000 ) ) ;
#71500 = CARTESIAN_POINT ( 'NONE',  ( -92.69370383062504004, 90.00000000000004263, 83.61031250086713840 ) ) ;
#71501 = CARTESIAN_POINT ( 'NONE',  ( -96.13030974027459763, -207.8557763824826452, 74.86230178910949462 ) ) ;
#71502 = DIRECTION ( 'NONE',  ( 0.000000000000000000, 0.000000000000000000, 1.000000000000000000 ) ) ;
#71503 = VECTOR ( 'NONE', #73446, 1000.000000000000000 ) ;
#71504 = CIRCLE ( 'NONE', #31900, 82.00000000000000000 ) ;
#71505 = CARTESIAN_POINT ( 'NONE',  ( -15.50000000000000000, 1.898202538678397557E-15, 0.000000000000000000 ) ) ;
#71506 = ORIENTED_EDGE ( 'NONE', *, *, #3601, .F. ) ;
#71507 = CARTESIAN_POINT ( 'NONE',  ( -96.15314808468751551, 88.00268892867056536, 75.14364583420046984 ) ) ;
#71508 = VECTOR ( 'NONE', #55413, 1000.000000000000000 ) ;
#71509 = LINE ( 'NONE', #37328, #17746 ) ;
#71510 = CARTESIAN_POINT ( 'NONE',  ( 10.00000000000000000, 0.000000000000000000, 0.000000000000000000 ) ) ;
#71511 = CARTESIAN_POINT ( 'NONE',  ( 10.00000000000000000, 41.19522573413731692, 65.64334221924924861 ) ) ;
#71513 = CARTESIAN_POINT ( 'NONE',  ( 96.32499999999998863, -207.7050326799711968, 84.70833333333332860 ) ) ;
#71512 = AXIS2_PLACEMENT_3D ( 'NONE', #53155, #47149, #70057 ) ;
#71514 = CARTESIAN_POINT ( 'NONE',  ( 0.000000000000000000, 0.000000000000000000, 0.000000000000000000 ) ) ;
#71515 = CARTESIAN_POINT ( 'NONE',  ( -92.69370383062498320, -208.6684592857803011, 83.82197916753382572 ) ) ;
#71516 =( NAMED_UNIT ( * ) SI_UNIT ( $, .STERADIAN. ) SOLID_ANGLE_UNIT ( ) );
#71517 = DIRECTION ( 'NONE',  ( -1.000000000000000000, 3.061616997868382648E-16, 0.000000000000000000 ) ) ;
#71518 = CARTESIAN_POINT ( 'NONE',  ( 10.00000000000000000, 0.000000000000000000, 0.000000000000000000 ) ) ;
#71519 = PRODUCT_RELATED_PRODUCT_CATEGORY ( 'part', '', ( #66792 ) ) ;
#71520 = EDGE_CURVE ( 'NONE', #30711, #61695, #51759, .T. ) ;
#71521 = CYLINDRICAL_SURFACE ( 'NONE', #1035, 77.49899999999999523 ) ;
#71522 = CARTESIAN_POINT ( 'NONE',  ( -96.32500000000001705, 87.70503267997129626, 88.83583333333334053 ) ) ;
#71523 = ORIENTED_EDGE ( 'NONE', *, *, #15700, .F. ) ;
#71524 = CARTESIAN_POINT ( 'NONE',  ( 10.00000000000000000, 0.000000000000000000, 0.000000000000000000 ) ) ;
#71525 = DIRECTION ( 'NONE',  ( 0.000000000000000000, 0.000000000000000000, 1.000000000000000000 ) ) ;
#71526 = LINE ( 'NONE', #2790, #22190 ) ;
#71527 = ADVANCED_FACE ( 'NONE', ( #34843 ), #30210, .F. ) ;
#71528 = DIRECTION ( 'NONE',  ( 1.000000000000000000, 0.000000000000000000, 0.000000000000000000 ) ) ;
#71529 = CARTESIAN_POINT ( 'NONE',  ( 96.15314808468748708, -208.0026889286704943, 88.95489583420049939 ) ) ;
#71530 = ORIENTED_EDGE ( 'NONE', *, *, #73825, .F. ) ;
#71531 = ADVANCED_FACE ( 'NONE', ( #39625 ), #63584, .T. ) ;
#71532 = CARTESIAN_POINT ( 'NONE',  ( 97.64999999999999147, -209.9999999999999716, 87.14249999999999829 ) ) ;
#71533 = CARTESIAN_POINT ( 'NONE',  ( -7.500000000000016875, -80.00000000000001421, -189.9999999999999147 ) ) ;
#71534 = VERTEX_POINT ( 'NONE', #6790 ) ;
#71535 = ADVANCED_FACE ( 'NONE', ( #15939 ), #9927, .T. ) ;
#71536 = CARTESIAN_POINT ( 'NONE',  ( 0.000000000000000000, 0.000000000000000000, 0.000000000000000000 ) ) ;
#71537 = AXIS2_PLACEMENT_3D ( 'NONE', #11038, #38117, #22315 ) ;
#71538 = ORIENTED_EDGE ( 'NONE', *, *, #63346, .T. ) ;
#71539 = CARTESIAN_POINT ( 'NONE',  ( 14.59956846177685996, -138.4757300459248484, -2.500000000000000000 ) ) ;
#71540 = CIRCLE ( 'NONE', #39152, 62.50000000000000000 ) ;
#71541 = ORIENTED_EDGE ( 'NONE', *, *, #23621, .T. ) ;
#71542 = AXIS2_PLACEMENT_3D ( 'NONE', #40293, #11703, #41403 ) ;
#71543 = ORIENTED_EDGE ( 'NONE', *, *, #59842, .F. ) ;
#71544 = CIRCLE ( 'NONE', #43933, 35.50000000000000711 ) ;
#71545 = ORIENTED_EDGE ( 'NONE', *, *, #17552, .F. ) ;
#71546 = ORIENTED_EDGE ( 'NONE', *, *, #56126, .F. ) ;
#71547 = DIRECTION ( 'NONE',  ( -1.000000000000000000, -0.000000000000000000, -0.000000000000000000 ) ) ;
#71548 = ADVANCED_FACE ( 'NONE', ( #824 ), #73448, .T. ) ;
#71549 = ADVANCED_FACE ( 'NONE', ( #27592 ), #29337, .T. ) ;
#71550 = ORIENTED_EDGE ( 'NONE', *, *, #6083, .T. ) ;
#71551 = PRODUCT ( 'socket head cap screw_iso_ISO 4762 M6 x 20 - 20N', 'socket head cap screw_iso_ISO 4762 M6 x 20 - 20N', '', ( #56137 ) ) ;
#71552 = CIRCLE ( 'NONE', #57142, 16.00000000000000000 ) ;
#71553 = VECTOR ( 'NONE', #14269, 1000.000000000000000 ) ;
#71554 = VERTEX_POINT ( 'NONE', #23712 ) ;
#71555 = CARTESIAN_POINT ( 'NONE',  ( 93.84685191531248449, 88.00268892867053694, 79.11239583420048405 ) ) ;
#71556 = DIRECTION ( 'NONE',  ( -1.000000000000000000, -0.000000000000000000, -0.000000000000000000 ) ) ;
#71557 = LINE ( 'NONE', #3176, #63283 ) ;
#71558 = VERTEX_POINT ( 'NONE', #56555 ) ;
#71559 = ORIENTED_EDGE ( 'NONE', *, *, #4124, .F. ) ;
#71560 = VERTEX_POINT ( 'NONE', #45273 ) ;
#71561 = DIRECTION ( 'NONE',  ( -1.000000000000000000, -0.000000000000000000, -0.000000000000000000 ) ) ;
#71562 = EDGE_LOOP ( 'NONE', ( #54063, #37844, #66147, #35693 ) ) ;
#71563 = EDGE_CURVE ( 'NONE', #73763, #69008, #9576, .T. ) ;
#71564 = DIRECTION ( 'NONE',  ( 2.775557561562891351E-17, 0.000000000000000000, -1.000000000000000000 ) ) ;
#71565 = CYLINDRICAL_SURFACE ( 'NONE', #28291, 31.99999999999998579 ) ;
#71566 = AXIS2_PLACEMENT_3D ( 'NONE', #69962, #47779, #58698 ) ;
#71567 = DIRECTION ( 'NONE',  ( -1.000000000000000000, 0.000000000000000000, -0.000000000000000000 ) ) ;
#71568 = CARTESIAN_POINT ( 'NONE',  ( 5.000000000000000000, -67.80270845531855173, -46.11716303203261447 ) ) ;
#71569 = DIRECTION ( 'NONE',  ( 0.000000000000000000, 0.5877852522924797984, -0.8090169943749426773 ) ) ;
#71570 = CARTESIAN_POINT ( 'NONE',  ( -97.65000000000001990, 90.00000000000004263, 77.93499999999998806 ) ) ;
#71571 = CARTESIAN_POINT ( 'NONE',  ( 0.000000000000000000, 17.28742895386084655, 75.54627589209950145 ) ) ;
#71572 = CARTESIAN_POINT ( 'NONE',  ( -92.34999999999999432, -211.5299782133524502, 76.37395833506761278 ) ) ;
#71573 = CARTESIAN_POINT ( 'NONE',  ( -92.69370383062504004, 90.00000000000004263, 87.57906250086715261 ) ) ;
#71575 = CARTESIAN_POINT ( 'NONE',  ( -92.69370383062502583, 91.33154071421968467, 88.74322916753379786 ) ) ;
#71574 = CARTESIAN_POINT ( 'NONE',  ( 92.34999999999999432, 91.52997821335252127, 77.32645833506762756 ) ) ;
#71576 = EDGE_LOOP ( 'NONE', ( #53214, #54842, #43583, #74289 ) ) ;
#71577 = CARTESIAN_POINT ( 'NONE',  ( 93.84685191531248449, 88.00268892867053694, 77.20739583420048291 ) ) ;
#71578 = LINE ( 'NONE', #25726, #67360 ) ;
#71579 = DIRECTION ( 'NONE',  ( -1.000000000000000000, 0.000000000000000000, -0.000000000000000000 ) ) ;
#71580 = CARTESIAN_POINT ( 'NONE',  ( 0.000000000000000000, 81.90746397400393164, -3.894527615416986333 ) ) ;
#71581 = CARTESIAN_POINT ( 'NONE',  ( 92.35000000046409241, -210.0000309672231253, 77.38038495127494798 ) ) ;
#71582 = CARTESIAN_POINT ( 'NONE',  ( -92.35000000000012221, 91.52997821335257811, 89.10041666666667481 ) ) ;
#71583 = ORIENTED_EDGE ( 'NONE', *, *, #33536, .T. ) ;
#71584 = CARTESIAN_POINT ( 'NONE',  ( -94.99999999999997158, -213.0599564267049857, 79.99874999999998693 ) ) ;
#71585 = DIRECTION ( 'NONE',  ( -0.000000000000000000, -0.000000000000000000, 1.000000000000000000 ) ) ;
#71586 = ORIENTED_EDGE ( 'NONE', *, *, #44482, .T. ) ;
#71587 = ORIENTED_EDGE ( 'NONE', *, *, #3824, .F. ) ;
#71588 = PLANE ( 'NONE',  #70311 ) ;
#71589 = DIRECTION ( 'NONE',  ( 2.603472992746261562E-14, 2.546204323184492723E-14, -1.000000000000000000 ) ) ;
#71590 = DIRECTION ( 'NONE',  ( 0.000000000000000000, 0.7604059656000276002, 0.6494480483301877660 ) ) ;
#71591 = DIRECTION ( 'NONE',  ( -8.587739980083048116E-16, -1.065814103640131346E-14, -1.000000000000000000 ) ) ;
#71592 = LINE ( 'NONE', #65608, #21692 ) ;
#71593 = CARTESIAN_POINT ( 'NONE',  ( 93.67499999999999716, 87.70503267997126784, 84.39083333333333314 ) ) ;
#71594 = CIRCLE ( 'NONE', #45212, 77.49899999999999523 ) ;
#71595 = ORIENTED_EDGE ( 'NONE', *, *, #38875, .F. ) ;
#71596 = EDGE_CURVE ( 'NONE', #7925, #73668, #18077, .T. ) ;
#71597 = CARTESIAN_POINT ( 'NONE',  ( 11.99999999999999822, -68.26794271651286294, 31.47745569255117104 ) ) ;
#71598 = CARTESIAN_POINT ( 'NONE',  ( 0.000000000000000000, 0.000000000000000000, 52.00000000000002132 ) ) ;
#71599 = DIRECTION ( 'NONE',  ( 1.000000000000000000, -5.236901059551556403E-15, -2.618450529775778123E-14 ) ) ;
#71600 = VECTOR ( 'NONE', #31263, 1000.000000000000000 ) ;
#71601 = DIRECTION ( 'NONE',  ( -1.000000000000000000, 0.000000000000000000, 0.000000000000000000 ) ) ;
#71602 = CARTESIAN_POINT ( 'NONE',  ( 11.99999999999999822, 2.956366410621684260, -75.11725578898465017 ) ) ;
#71603 = DIRECTION ( 'NONE',  ( -1.000000000000000000, 0.000000000000000000, 0.000000000000000000 ) ) ;
#71604 = EDGE_CURVE ( 'NONE', #51310, #22671, #70792, .T. ) ;
#71606 = AXIS2_PLACEMENT_3D ( 'NONE', #73882, #46068, #34402 ) ;
#71605 = UNCERTAINTY_MEASURE_WITH_UNIT (LENGTH_MEASURE( 1.000000000000000082E-05 ), #57337, 'distance_accuracy_value', 'NONE');
#71607 = DIRECTION ( 'NONE',  ( -0.000000000000000000, -0.000000000000000000, 1.000000000000000000 ) ) ;
#71608 = CARTESIAN_POINT ( 'NONE',  ( 2.499999999999979572, 90.00000000000000000, -280.0000000000000000 ) ) ;
#71609 = EDGE_CURVE ( 'NONE', #56423, #54488, #46645, .T. ) ;
#71610 = FACE_OUTER_BOUND ( 'NONE', #5206, .T. ) ;
#71611 = VECTOR ( 'NONE', #13623, 1000.000000000000000 ) ;
#71612 =( BOUNDED_CURVE ( )  B_SPLINE_CURVE ( 2, ( #18003, #6725, #69868, #20212, #72453, #49163, #31123 ),
 .UNSPECIFIED., .F., .F. ) 
 B_SPLINE_CURVE_WITH_KNOTS ( ( 3, 2, 2, 3 ),
 ( 0.2916666666666669072, 0.2986111111111113270, 0.3055555555555557468, 0.3125000000000001665 ),
 .UNSPECIFIED. ) 
 CURVE ( )  GEOMETRIC_REPRESENTATION_ITEM ( )  RATIONAL_B_SPLINE_CURVE ( ( 0.9999999999999956701, 0.8660254037844430375, 1.000000000000000000, 0.8660254037844387076, 1.000000000000000000, 0.8660254037844354880, 1.000000000000003109 ) ) 
 REPRESENTATION_ITEM ( '' )  );
#71613 = CARTESIAN_POINT ( 'NONE',  ( 97.30629616937498838, 90.00000000000002842, 85.03906250086714635 ) ) ;
#71614 = EDGE_CURVE ( 'NONE', #71835, #6105, #55180, .T. ) ;
#71615 = CARTESIAN_POINT ( 'NONE',  ( -94.99999999999997158, -207.3369185715606307, 82.02281250086714692 ) ) ;
#71616 = CARTESIAN_POINT ( 'NONE',  ( -10.94538922500103162, 1.915100337961297692E-15, -13.90444123027096879 ) ) ;
#71617 = ORIENTED_EDGE ( 'NONE', *, *, #73262, .T. ) ;
#71618 = PLANE ( 'NONE',  #35286 ) ;
#71619 = CARTESIAN_POINT ( 'NONE',  ( -94.99999999999997158, -213.0599564267049857, 79.36374999999999602 ) ) ;
#71620 = CYLINDRICAL_SURFACE ( 'NONE', #42528, 82.00000000000000000 ) ;
#71621 = AXIS2_PLACEMENT_3D ( 'NONE', #69876, #64619, #63895 ) ;
#71622 = CARTESIAN_POINT ( 'NONE',  ( 95.00000000000000000, -207.3369185715606307, 85.03906250086714635 ) ) ;
#71623 = ORIENTED_EDGE ( 'NONE', *, *, #23193, .T. ) ;
#71624 = DIRECTION ( 'NONE',  ( -1.000000000000000000, 0.000000000000000000, -0.000000000000000000 ) ) ;
#71625 = ORIENTED_EDGE ( 'NONE', *, *, #37034, .F. ) ;
#71626 = EDGE_CURVE ( 'NONE', #53797, #62152, #64809, .T. ) ;
#71627 = ORIENTED_EDGE ( 'NONE', *, *, #67476, .T. ) ;
#71628 = CARTESIAN_POINT ( 'NONE',  ( 97.64999999999999147, -209.9999999999999716, 83.96750000000000114 ) ) ;
#71629 = AXIS2_PLACEMENT_3D ( 'NONE', #51796, #52523, #51416 ) ;
#71630 = ORIENTED_EDGE ( 'NONE', *, *, #616, .T. ) ;
#71631 = DIRECTION ( 'NONE',  ( -1.000000000000000000, 0.000000000000000000, -0.000000000000000000 ) ) ;
#71632 = CARTESIAN_POINT ( 'NONE',  ( 93.84685191531249870, -208.0026889286704943, 77.63072916753381492 ) ) ;
#71633 = EDGE_CURVE ( 'NONE', #1093, #56703, #51589, .T. ) ;
#71634 = DIRECTION ( 'NONE',  ( -1.000000000000000000, -0.000000000000000000, 0.000000000000000000 ) ) ;
#71635 = EDGE_CURVE ( 'NONE', #12564, #13600, #61201, .T. ) ;
#71636 = DIRECTION ( 'NONE',  ( 0.000000000000000000, 1.000000000000000000, -1.625241993126352398E-15 ) ) ;
#71637 = DIRECTION ( 'NONE',  ( 0.000000000000000000, 0.000000000000000000, 1.000000000000000000 ) ) ;
#71638 = DIRECTION ( 'NONE',  ( 0.7273375899149802093, -0.6862798483830544471, 0.000000000000000000 ) ) ;
#71639 = EDGE_CURVE ( 'NONE', #59562, #72371, #27541, .T. ) ;
#71640 = VECTOR ( 'NONE', #11226, 1000.000000000000000 ) ;
#71641 = CARTESIAN_POINT ( 'NONE',  ( -97.64995971452408696, 88.46999852781715390, 83.14729327728630892 ) ) ;
#71642 = CARTESIAN_POINT ( 'NONE',  ( 93.67500000000001137, -207.7050326799711968, 82.27416666666665890 ) ) ;
#71643 = CIRCLE ( 'NONE', #6826, 31.99999999999998934 ) ;
#71644 = ORIENTED_EDGE ( 'NONE', *, *, #24639, .T. ) ;
#71645 = VERTEX_POINT ( 'NONE', #67073 ) ;
#71646 = ORIENTED_EDGE ( 'NONE', *, *, #23193, .F. ) ;
#71647 = ORIENTED_EDGE ( 'NONE', *, *, #5559, .T. ) ;
#71648 = FACE_OUTER_BOUND ( 'NONE', #12029, .T. ) ;
#71649 = PRESENTATION_STYLE_ASSIGNMENT (( #55107 ) ) ;
#71650 = CARTESIAN_POINT ( 'NONE',  ( -95.00000000000002842, 87.33691857156074434, 84.24531250086715772 ) ) ;
#71651 = CARTESIAN_POINT ( 'NONE',  ( -94.99999999999997158, -209.9999999999999716, 90.00000000000000000 ) ) ;
#71652 = CIRCLE ( 'NONE', #11604, 31.99999999999999289 ) ;
#71653 = DIRECTION ( 'NONE',  ( -1.000000000000000000, -0.000000000000000000, 0.000000000000000000 ) ) ;
#71654 = CARTESIAN_POINT ( 'NONE',  ( 97.64999999999997726, 91.52997821335252127, 76.40041666666667197 ) ) ;
#71655 = CARTESIAN_POINT ( 'NONE',  ( 0.000000000000000000, 21.32104025579158701, -30.84782396557194772 ) ) ;
#71656 = EDGE_LOOP ( 'NONE', ( #64461, #425, #47178, #69304 ) ) ;
#71657 = CARTESIAN_POINT ( 'NONE',  ( -92.34999999999999432, -211.5299782133524502, 85.89895833506764689 ) ) ;
#71658 = ORIENTED_EDGE ( 'NONE', *, *, #18994, .T. ) ;
#71659 = DIRECTION ( 'NONE',  ( -0.000000000000000000, -0.000000000000000000, -1.000000000000000000 ) ) ;
#71660 = AXIS2_PLACEMENT_3D ( 'NONE', #4890, #43615, #15015 ) ;
#71661 = VERTEX_POINT ( 'NONE', #50892 ) ;
#71662 = CARTESIAN_POINT ( 'NONE',  ( -95.00000000000002842, 93.05995642670501411, 88.01562500173429271 ) ) ;
#71663 = ORIENTED_EDGE ( 'NONE', *, *, #65289, .F. ) ;
#71664 = CARTESIAN_POINT ( 'NONE',  ( 97.30629616937498838, 91.33154071421968467, 85.72697916753381264 ) ) ;
#71665 = CIRCLE ( 'NONE', #62086, 37.49900000000001654 ) ;
#71666 = DIRECTION ( 'NONE',  ( 0.000000000000000000, 0.000000000000000000, 1.000000000000000000 ) ) ;
#71667 = DIRECTION ( 'NONE',  ( -0.6862798483830544471, -0.7273375899149802093, 0.000000000000000000 ) ) ;
#71668 = DIRECTION ( 'NONE',  ( -1.000000000000000000, -0.000000000000000000, -0.000000000000000000 ) ) ;
#71669 = DIRECTION ( 'NONE',  ( 1.000000000000000000, -0.000000000000000000, -0.000000000000000000 ) ) ;
#71670 = ORIENTED_EDGE ( 'NONE', *, *, #36505, .F. ) ;
#71671 = DIRECTION ( 'NONE',  ( 8.090853898039828715E-17, -9.269810975720166919E-17, 1.000000000000000000 ) ) ;
#71672 = DIRECTION ( 'NONE',  ( -0.000000000000000000, -0.000000000000000000, -1.000000000000000000 ) ) ;
#71673 = EDGE_LOOP ( 'NONE', ( #65563, #62810, #67232, #31658 ) ) ;
#71674 = CIRCLE ( 'NONE', #26054, 82.00000000000000000 ) ;
#71675 = ORIENTED_EDGE ( 'NONE', *, *, #24718, .F. ) ;
#71676 = CARTESIAN_POINT ( 'NONE',  ( 93.67499999999999716, 87.70503267997126784, 78.75520833506763552 ) ) ;
#71677 = AXIS2_PLACEMENT_3D ( 'NONE', #28640, #17009, #33540 ) ;
#71678 = DIRECTION ( 'NONE',  ( 1.000000000000000000, 0.000000000000000000, 0.000000000000000000 ) ) ;
#71679 = DIRECTION ( 'NONE',  ( -1.000000000000000000, -0.000000000000000000, 0.000000000000000000 ) ) ;
#71680 = CARTESIAN_POINT ( 'NONE',  ( -94.99999999999997158, -207.3369185715606307, 85.83281250086714920 ) ) ;
#71681 = EDGE_LOOP ( 'NONE', ( #60942, #31121, #20516, #29845 ) ) ;
#71682 = CARTESIAN_POINT ( 'NONE',  ( -95.00000000000002842, 90.00000000000004263, 90.00000000000000000 ) ) ;
#71683 = ORIENTED_EDGE ( 'NONE', *, *, #34105, .T. ) ;
#71684 = ADVANCED_FACE ( 'NONE', ( #4316 ), #38507, .T. ) ;
#71685 = DIRECTION ( 'NONE',  ( -1.000000000000000000, -0.000000000000000000, 0.000000000000000000 ) ) ;
#71686 = FACE_OUTER_BOUND ( 'NONE', #61352, .T. ) ;
#71687 = DIRECTION ( 'NONE',  ( -1.224646799147353207E-16, 1.000000000000000000, 0.000000000000000000 ) ) ;
#71688 = CARTESIAN_POINT ( 'NONE',  ( 94.99999999999998579, 92.66308142843932671, 76.78406250086712248 ) ) ;
#71689 = CARTESIAN_POINT ( 'NONE',  ( 0.000000000000000000, -26.01480285779885904, 70.53064760720306481 ) ) ;
#71690 = CARTESIAN_POINT ( 'NONE',  ( 92.35000000003284981, 90.00000839192529156, 86.90410584365271518 ) ) ;
#71691 = EDGE_CURVE ( 'NONE', #45341, #42450, #67447, .T. ) ;
#71692 = DIRECTION ( 'NONE',  ( -1.000000000000000000, 3.061616997868382648E-16, 0.000000000000000000 ) ) ;
#71693 = CARTESIAN_POINT ( 'NONE',  ( 0.000000000000000000, 0.000000000000000000, 0.000000000000000000 ) ) ;
#71694 = FACE_OUTER_BOUND ( 'NONE', #9934, .T. ) ;
#71695 = ADVANCED_FACE ( 'NONE', ( #8264 ), #18435, .T. ) ;
#71696 = CARTESIAN_POINT ( 'NONE',  ( -24.50849501662245800, -109.8101191361138831, 5.500000000000000000 ) ) ;
#71697 = AXIS2_PLACEMENT_3D ( 'NONE', #39112, #21423, #61672 ) ;
#71698 = FACE_OUTER_BOUND ( 'NONE', #37199, .T. ) ;
#71699 = PRODUCT_DEFINITION_CONTEXT ( 'detailed design', #50808, 'design' ) ;
#71700 = EDGE_CURVE ( 'NONE', #32622, #70629, #49223, .T. ) ;
#71701 = CARTESIAN_POINT ( 'NONE',  ( 97.64999999999689351, 89.99999595380309358, 77.06187486178042434 ) ) ;
#71702 = ORIENTED_EDGE ( 'NONE', *, *, #63673, .T. ) ;
#71703 = CARTESIAN_POINT ( 'NONE',  ( -95.00000000000002842, 92.66308142843932671, 83.76906250086715033 ) ) ;
#71704 = DIRECTION ( 'NONE',  ( -0.000000000000000000, -0.000000000000000000, 1.000000000000000000 ) ) ;
#71705 = AXIS2_PLACEMENT_3D ( 'NONE', #62585, #24200, #2037 ) ;
#71706 = CARTESIAN_POINT ( 'NONE',  ( 11.99999999999999822, 8.840884882375075193, 74.65374052328651544 ) ) ;
#71707 = ORIENTED_EDGE ( 'NONE', *, *, #6079, .T. ) ;
#71708 = CARTESIAN_POINT ( 'NONE',  ( -19.90058851926621131, -132.5883508287165853, -5.500000000000000000 ) ) ;
#71709 = DIRECTION ( 'NONE',  ( 0.000000000000000000, 0.000000000000000000, 1.000000000000000000 ) ) ;
#71710 = ADVANCED_FACE ( 'NONE', ( #18795 ), #2300, .T. ) ;
#71711 = CYLINDRICAL_SURFACE ( 'NONE', #55136, 10.00000000000000178 ) ;
#71712 = CARTESIAN_POINT ( 'NONE',  ( 92.69370383062501162, -209.9999999999999716, 79.00656250086716170 ) ) ;
#71713 = AXIS2_PLACEMENT_3D ( 'NONE', #38554, #34292, #45966 ) ;
#71714 = ORIENTED_EDGE ( 'NONE', *, *, #68613, .T. ) ;
#71715 = ORIENTED_EDGE ( 'NONE', *, *, #44849, .T. ) ;
#71716 = EDGE_CURVE ( 'NONE', #70614, #60828, #56431, .T. ) ;
#71717 = DIRECTION ( 'NONE',  ( -1.000000000000000000, -0.000000000000000000, -0.000000000000000000 ) ) ;
#71718 = EDGE_CURVE ( 'NONE', #17733, #5742, #54142, .T. ) ;
#71719 = CARTESIAN_POINT ( 'NONE',  ( 10.00000000000000000, 51.03279382321166224, -55.19960302592011914 ) ) ;
#71720 = CARTESIAN_POINT ( 'NONE',  ( 11.99999999999999822, 0.000000000000000000, 0.000000000000000000 ) ) ;
#71721 = EDGE_LOOP ( 'NONE', ( #15723, #74086, #40133, #70173 ) ) ;
#71722 = DIRECTION ( 'NONE',  ( -0.000000000000000000, -0.000000000000000000, 1.000000000000000000 ) ) ;
#71723 = CARTESIAN_POINT ( 'NONE',  ( 96.15314808468748708, -208.0026889286704943, 76.88989583420048746 ) ) ;
#71724 = VERTEX_POINT ( 'NONE', #71038 ) ;
#71725 = DIRECTION ( 'NONE',  ( 0.000000000000000000, -0.3090169943749349613, -0.9510565162951576390 ) ) ;
#71726 = ORIENTED_EDGE ( 'NONE', *, *, #29628, .T. ) ;
#71727 = VERTEX_POINT ( 'NONE', #59045 ) ;
#71728 = CARTESIAN_POINT ( 'NONE',  ( -94.99999999999997158, -206.9400435732949575, 82.30062500173427509 ) ) ;
#71729 =( NAMED_UNIT ( * ) PLANE_ANGLE_UNIT ( ) SI_UNIT ( $, .RADIAN. ) );
#71730 = DIRECTION ( 'NONE',  ( 0.000000000000000000, -0.8090169943749401238, -0.5877852522924831291 ) ) ;
#71731 = ORIENTED_EDGE ( 'NONE', *, *, #12129, .T. ) ;
#71732 = DIRECTION ( 'NONE',  ( 1.000000000000000000, 0.000000000000000000, -0.000000000000000000 ) ) ;
#71733 = CARTESIAN_POINT ( 'NONE',  ( 97.64999999999999147, -209.9999999999999716, 84.68187500173429783 ) ) ;
#71734 = CARTESIAN_POINT ( 'NONE',  ( 92.34999999999999432, 90.00000000000002842, 84.28499999999999659 ) ) ;
#71735 = ORIENTED_EDGE ( 'NONE', *, *, #18426, .T. ) ;
#71736 = CARTESIAN_POINT ( 'NONE',  ( 26.09152095774781799, -124.8716048804687375, -5.500000000000000000 ) ) ;
#71737 = CARTESIAN_POINT ( 'NONE',  ( 10.00000000000000000, -35.38097989696503021, -12.42422080174676147 ) ) ;
#71738 = VERTEX_POINT ( 'NONE', #41735 ) ;
#71739 = ORIENTED_EDGE ( 'NONE', *, *, #38553, .T. ) ;
#71740 = CARTESIAN_POINT ( 'NONE',  ( -92.69370383062505425, 91.33154071421968467, 88.90197916753382401 ) ) ;
#71741 = CIRCLE ( 'NONE', #2203, 77.49899999999999523 ) ;
#71742 = CARTESIAN_POINT ( 'NONE',  ( 97.30629616937498838, 91.33154071421968467, 82.39322916753381776 ) ) ;
#71743 = EDGE_LOOP ( 'NONE', ( #35650, #43947, #6481, #11789 ) ) ;
#71744 = CARTESIAN_POINT ( 'NONE',  ( 96.32499999999998863, 87.70503267997126784, 82.03604166840096923 ) ) ;
#71745 = CARTESIAN_POINT ( 'NONE',  ( -3.000000000000000000, -22.67460108101783334, 6.353146135317912169 ) ) ;
#71746 = VERTEX_POINT ( 'NONE', #7534 ) ;
#71747 = FACE_OUTER_BOUND ( 'NONE', #776, .T. ) ;
#71748 = ORIENTED_EDGE ( 'NONE', *, *, #49748, .T. ) ;
#71749 = ORIENTED_EDGE ( 'NONE', *, *, #60751, .T. ) ;
#71750 = CIRCLE ( 'NONE', #24922, 31.99999999999999289 ) ;
#71751 = ORIENTED_EDGE ( 'NONE', *, *, #47134, .F. ) ;
#71752 = CIRCLE ( 'NONE', #12940, 31.99999999999998934 ) ;
#71753 = FACE_OUTER_BOUND ( 'NONE', #33251, .T. ) ;
#71754 = LINE ( 'NONE', #60147, #72093 ) ;
#71755 = CARTESIAN_POINT ( 'NONE',  ( -95.00000000000002842, 93.05995642670501411, 84.76125000000000398 ) ) ;
#71756 = ORIENTED_EDGE ( 'NONE', *, *, #303, .T. ) ;
#71757 = CYLINDRICAL_SURFACE ( 'NONE', #46785, 2.649999999999985700 ) ;
#71758 = EDGE_CURVE ( 'NONE', #70108, #27488, #53030, .T. ) ;
#71759 = CARTESIAN_POINT ( 'NONE',  ( 0.000000000000000000, -22.64427369931191336, 30.00120703465197280 ) ) ;
#71760 = ORIENTED_EDGE ( 'NONE', *, *, #13392, .T. ) ;
#71761 = CARTESIAN_POINT ( 'NONE',  ( -93.67499999999998295, -212.2949673200287179, 75.05104166840095559 ) ) ;
#71762 = CARTESIAN_POINT ( 'NONE',  ( -92.69370383062498320, -211.3315407142195852, 77.84239583420045960 ) ) ;
#71763 = ORIENTED_EDGE ( 'NONE', *, *, #64343, .T. ) ;
#71764 = CARTESIAN_POINT ( 'NONE',  ( 92.35000000000000853, -209.9999999999999716, 90.00000000000000000 ) ) ;
#71765 = CYLINDRICAL_SURFACE ( 'NONE', #16436, 16.00000000000000000 ) ;
#71766 = DIRECTION ( 'NONE',  ( 0.000000000000000000, 0.000000000000000000, 1.000000000000000000 ) ) ;
#71767 = CYLINDRICAL_SURFACE ( 'NONE', #27870, 31.99999999999998579 ) ;
#71768 = EDGE_CURVE ( 'NONE', #57845, #26721, #52841, .T. ) ;
#71769 = CARTESIAN_POINT ( 'NONE',  ( 10.00000000000000000, -6.555932627142143865, -37.01155633439065440 ) ) ;
#71770 = EDGE_CURVE ( 'NONE', #55213, #25600, #26417, .T. ) ;
#71771 = DIRECTION ( 'NONE',  ( 2.603472992746261562E-14, 2.546204323184492723E-14, -1.000000000000000000 ) ) ;
#71773 = AXIS2_PLACEMENT_3D ( 'NONE', #58932, #18321, #41264 ) ;
#71772 = CARTESIAN_POINT ( 'NONE',  ( 96.15314808468748708, 91.99731107132950569, 87.52614583420047722 ) ) ;
#71774 = CARTESIAN_POINT ( 'NONE',  ( 0.000000000000000000, 46.11716303203284184, -67.80270845531839541 ) ) ;
#71775 = ADVANCED_FACE ( 'NONE', ( #24819 ), #64678, .T. ) ;
#71776 = CARTESIAN_POINT ( 'NONE',  ( 15.00000000000000000, -22.67460108101782978, -6.353146135317906840 ) ) ;
#71777 = AXIS2_PLACEMENT_3D ( 'NONE', #13996, #41119, #8376 ) ;
#71778 = CARTESIAN_POINT ( 'NONE',  ( 12.00000000000000000, 22.07842321921480533, -8.187992925817425771 ) ) ;
#71779 = CARTESIAN_POINT ( 'NONE',  ( -95.00000000000002842, 92.66308142843932671, 74.87906250086713555 ) ) ;
#71780 = CYLINDRICAL_SURFACE ( 'NONE', #50288, 37.49900000000000233 ) ;
#71781 = CARTESIAN_POINT ( 'NONE',  ( 92.34999999999999432, 90.00000000000002842, 76.03000000000000114 ) ) ;
#71782 = CIRCLE ( 'NONE', #27344, 31.99999999999999289 ) ;
#71783 = CARTESIAN_POINT ( 'NONE',  ( 93.67500000000001137, -207.7050326799711968, 75.28916666666665947 ) ) ;
#71784 = CARTESIAN_POINT ( 'NONE',  ( 4.182066831946704255, -3.358985280702828646, -5.826062401966622950 ) ) ;
#71785 = EDGE_CURVE ( 'NONE', #12127, #28934, #71405, .T. ) ;
#71786 = LINE ( 'NONE', #26672, #70106 ) ;
#71787 = CARTESIAN_POINT ( 'NONE',  ( -7.499999999999968914, 79.99999999999998579, -269.9999999999999432 ) ) ;
#71788 = CARTESIAN_POINT ( 'NONE',  ( 10.00000000000000000, 17.80606268964585226, -33.00180498840028775 ) ) ;
#71789 = CARTESIAN_POINT ( 'NONE',  ( -23.30023580412278505, -123.4057321492263384, 2.500000000000000000 ) ) ;
#71790 = CARTESIAN_POINT ( 'NONE',  ( -94.99999999999997158, -213.0599564267049857, 88.25374999999999659 ) ) ;
#71791 = CARTESIAN_POINT ( 'NONE',  ( 0.000000000000000000, 18.89407956138362010, -75.16055320797013906 ) ) ;
#71792 = ADVANCED_FACE ( 'NONE', ( #1565 ), #19904, .T. ) ;
#71793 = ORIENTED_EDGE ( 'NONE', *, *, #16841, .T. ) ;
#71794 = CARTESIAN_POINT ( 'NONE',  ( -10.00000000000000000, 0.000000000000000000, 0.000000000000000000 ) ) ;
#71795 = EDGE_CURVE ( 'NONE', #25992, #69906, #69624, .T. ) ;
#71796 = LINE ( 'NONE', #43271, #2320 ) ;
#71797 = CARTESIAN_POINT ( 'NONE',  ( 10.00000000000000000, -77.32052557432845674, 5.256550761632577284 ) ) ;
#71798 = AXIS2_PLACEMENT_3D ( 'NONE', #40367, #56935, #56569 ) ;
#71799 = DIRECTION ( 'NONE',  ( 0.000000000000000000, 0.000000000000000000, 1.000000000000000000 ) ) ;
#71800 = EDGE_CURVE ( 'NONE', #8982, #9094, #30447, .T. ) ;
#71801 = CIRCLE ( 'NONE', #2211, 11.59999999999999787 ) ;
#71802 = AXIS2_PLACEMENT_3D ( 'NONE', #53772, #73189, #56286 ) ;
#71803 = ORIENTED_EDGE ( 'NONE', *, *, #11806, .T. ) ;
#71804 = ORIENTED_EDGE ( 'NONE', *, *, #71899, .T. ) ;
#71805 = CARTESIAN_POINT ( 'NONE',  ( 12.69589495141918611, -96.69089767102708777, 5.500000000000000000 ) ) ;
#71806 = EDGE_CURVE ( 'NONE', #3546, #67626, #65061, .T. ) ;
#71807 = DIRECTION ( 'NONE',  ( -0.000000000000000000, -0.000000000000000000, -1.000000000000000000 ) ) ;
#71808 = ORIENTED_EDGE ( 'NONE', *, *, #13178, .F. ) ;
#71809 = CARTESIAN_POINT ( 'NONE',  ( 97.30629616937498838, -211.3315407142195852, 80.38239583420049428 ) ) ;
#71810 = CARTESIAN_POINT ( 'NONE',  ( 93.84685191531249870, -208.0026889286704943, 83.98072916753382344 ) ) ;
#71811 = ORIENTED_EDGE ( 'NONE', *, *, #41534, .T. ) ;
#71812 = CARTESIAN_POINT ( 'NONE',  ( 93.84685191531251292, -211.9973110713294489, 86.09739583420049769 ) ) ;
#71813 = EDGE_CURVE ( 'NONE', #11307, #24488, #31557, .T. ) ;
#71814 = AXIS2_PLACEMENT_3D ( 'NONE', #38904, #27980, #21977 ) ;
#71815 = VERTEX_POINT ( 'NONE', #24097 ) ;
#71816 = CARTESIAN_POINT ( 'NONE',  ( 3.000000000000000000, 2.935248768560057897, -3.252606517456513302E-15 ) ) ;
#71817 = ORIENTED_EDGE ( 'NONE', *, *, #34062, .T. ) ;
#71818 = CARTESIAN_POINT ( 'NONE',  ( -97.30629616937501680, 91.33154071421968467, 77.04864583420048518 ) ) ;
#71819 = CIRCLE ( 'NONE', #46622, 31.99999999999998579 ) ;
#71820 = ORIENTED_EDGE ( 'NONE', *, *, #20686, .T. ) ;
#71821 = VERTEX_POINT ( 'NONE', #53758 ) ;
#71822 = AXIS2_PLACEMENT_3D ( 'NONE', #22402, #61516, #34048 ) ;
#71823 = CARTESIAN_POINT ( 'NONE',  ( 11.99999999999999822, 71.21200624218795383, 40.65526001592638039 ) ) ;
#71824 = ORIENTED_EDGE ( 'NONE', *, *, #5962, .F. ) ;
#71825 = DIRECTION ( 'NONE',  ( -1.000000000000000000, -0.000000000000000000, 0.000000000000000000 ) ) ;
#71826 = CARTESIAN_POINT ( 'NONE',  ( 92.35000000000000853, -209.9999999999999716, 79.20499999999999829 ) ) ;
#71827 = ORIENTED_EDGE ( 'NONE', *, *, #59597, .F. ) ;
#71828 = DIRECTION ( 'NONE',  ( -1.000000000000000000, 0.000000000000000000, -0.000000000000000000 ) ) ;
#71829 = VERTEX_POINT ( 'NONE', #41378 ) ;
#71830 = PRESENTATION_LAYER_ASSIGNMENT (  '', '', ( #56244 ) ) ;
#71831 =( BOUNDED_CURVE ( )  B_SPLINE_CURVE ( 2, ( #2650, #42830, #65761, #62367, #56344, #45065, #60863 ),
 .UNSPECIFIED., .F., .T. ) 
 B_SPLINE_CURVE_WITH_KNOTS ( ( 3, 2, 2, 3 ),
 ( 0.2291666666666663521, 0.2361111111111107719, 0.2430555555555551639, 0.2499999999999995837 ),
 .UNSPECIFIED. ) 
 CURVE ( )  GEOMETRIC_REPRESENTATION_ITEM ( )  RATIONAL_B_SPLINE_CURVE ( ( 1.000000000000005995, 0.8660254037844328234, 1.000000000000000000, 0.8660254037844387076, 1.000000000000000000, 0.8660254037844467012, 0.9999999999999920064 ) ) 
 REPRESENTATION_ITEM ( '' )  );
#71832 = CARTESIAN_POINT ( 'NONE',  ( 92.35000000000000853, -209.9999999999999716, 81.18937500173430521 ) ) ;
#71833 = ORIENTED_EDGE ( 'NONE', *, *, #19947, .T. ) ;
#71834 = EDGE_LOOP ( 'NONE', ( #37885, #34666, #36147, #5175 ) ) ;
#71835 = VERTEX_POINT ( 'NONE', #47023 ) ;
#71836 = CARTESIAN_POINT ( 'NONE',  ( 92.69370383062501162, -211.3315407142195852, 78.26572916753380582 ) ) ;
#71837 = CARTESIAN_POINT ( 'NONE',  ( 10.00000000000000000, 41.76106447765489094, 62.50884508063442269 ) ) ;
#71838 = DIRECTION ( 'NONE',  ( 0.000000000000000000, 8.881784197001252323E-16, 1.000000000000000000 ) ) ;
#71839 = ORIENTED_EDGE ( 'NONE', *, *, #67660, .F. ) ;
#71840 = VERTEX_POINT ( 'NONE', #64314 ) ;
#71841 = CARTESIAN_POINT ( 'NONE',  ( 11.99999999999999822, 72.35160999960844208, -20.41045688087747223 ) ) ;
#71842 = EDGE_LOOP ( 'NONE', ( #71368, #71457, #56781, #19586 ) ) ;
#71843 = DIRECTION ( 'NONE',  ( -0.08130631524009862554, 0.9966891607226787686, 0.000000000000000000 ) ) ;
#71844 = LINE ( 'NONE', #36531, #27467 ) ;
#71845 = CARTESIAN_POINT ( 'NONE',  ( -97.30629616937501680, 90.00000000000004263, 79.00656250086716170 ) ) ;
#71846 = VERTEX_POINT ( 'NONE', #35717 ) ;
#71847 = CARTESIAN_POINT ( 'NONE',  ( 94.99999999999998579, 92.66308142843935514, 79.32406250086714294 ) ) ;
#71848 = VERTEX_POINT ( 'NONE', #59408 ) ;
#71849 = LINE ( 'NONE', #19252, #67145 ) ;
#71850 = CARTESIAN_POINT ( 'NONE',  ( -93.84685191531247028, -211.9973110713294489, 87.94947916753380923 ) ) ;
#71851 = VECTOR ( 'NONE', #15560, 1000.000000000000000 ) ;
#71852 = CARTESIAN_POINT ( 'NONE',  ( 96.92442009029373651, 88.17815826261617929, 75.00000000000000000 ) ) ;
#71853 = CARTESIAN_POINT ( 'NONE',  ( 11.99999999999999822, -54.21277698773636899, -55.38113227695839669 ) ) ;
#71854 = DIRECTION ( 'NONE',  ( -1.000000000000000000, -0.000000000000000000, -0.000000000000000000 ) ) ;
#71855 = CARTESIAN_POINT ( 'NONE',  ( -96.15314808468745866, -211.9973110713294489, 82.12864583420046927 ) ) ;
#71856 = CIRCLE ( 'NONE', #67091, 77.49899999999999523 ) ;
#71857 = VECTOR ( 'NONE', #26122, 1000.000000000000227 ) ;
#71858 = EDGE_CURVE ( 'NONE', #38945, #68066, #58851, .T. ) ;
#71859 = CARTESIAN_POINT ( 'NONE',  ( 0.000000000000000000, -16.65560815589383381, -38.55633173627028754 ) ) ;
#71860 = DIRECTION ( 'NONE',  ( 1.000000000000000000, 0.000000000000000000, 0.000000000000000000 ) ) ;
#71861 = CARTESIAN_POINT ( 'NONE',  ( -2.459674775249774736, 1.628656900575240630E-13, 15.79999999999999538 ) ) ;
#71862 = VERTEX_POINT ( 'NONE', #25528 ) ;
#71863 = CIRCLE ( 'NONE', #11807, 42.00000000000000000 ) ;
#71864 = EDGE_CURVE ( 'NONE', #29201, #42911, #70851, .T. ) ;
#71865 = ORIENTED_EDGE ( 'NONE', *, *, #54722, .F. ) ;
#71866 = CARTESIAN_POINT ( 'NONE',  ( 99.99999999999998579, 95.00000000000001421, -90.00000000000002842 ) ) ;
#71867 = ADVANCED_FACE ( 'NONE', ( #54471 ), #8236, .F. ) ;
#71868 = EDGE_CURVE ( 'NONE', #61246, #65031, #3368, .T. ) ;
#71869 = CYLINDRICAL_SURFACE ( 'NONE', #37551, 77.49899999999999523 ) ;
#71870 = CARTESIAN_POINT ( 'NONE',  ( -96.32500000000001705, 87.70503267997129626, 84.47020833506762472 ) ) ;
#71871 = CARTESIAN_POINT ( 'NONE',  ( -95.00000000000002842, 87.33691857156074434, 86.62656250086715204 ) ) ;
#71872 = CARTESIAN_POINT ( 'NONE',  ( 0.000000000000000000, 0.000000000000000000, 4.750000000000000000 ) ) ;
#71873 = FACE_OUTER_BOUND ( 'NONE', #41584, .T. ) ;
#71874 = CYLINDRICAL_SURFACE ( 'NONE', #67201, 77.49899999999999523 ) ;
#71875 = ORIENTED_EDGE ( 'NONE', *, *, #10899, .F. ) ;
#71876 = DIRECTION ( 'NONE',  ( -1.000000000000000000, 0.000000000000000000, -0.000000000000000000 ) ) ;
#71877 = CIRCLE ( 'NONE', #55255, 12.49999999999999645 ) ;
#71878 = DIRECTION ( 'NONE',  ( -0.000000000000000000, -0.000000000000000000, 1.000000000000000000 ) ) ;
#71879 = AXIS2_PLACEMENT_3D ( 'NONE', #26252, #60854, #20625 ) ;
#71880 = DIRECTION ( 'NONE',  ( 0.000000000000000000, -0.8526401643540971742, 0.5224985647159409163 ) ) ;
#71881 = CARTESIAN_POINT ( 'NONE',  ( 94.99999999999998579, 90.00000000000002842, 90.00000000000000000 ) ) ;
#71882 = LINE ( 'NONE', #25665, #30130 ) ;
#71883 = CARTESIAN_POINT ( 'NONE',  ( 97.65000000000006253, 88.47002178664756400, 86.45458333333331780 ) ) ;
#71884 = CARTESIAN_POINT ( 'NONE',  ( -93.84685191531247028, -211.9973110713294489, 81.75822916753382685 ) ) ;
#71885 =( LENGTH_UNIT ( ) NAMED_UNIT ( * ) SI_UNIT ( .MILLI., .METRE. ) );
#71886 = VECTOR ( 'NONE', #30122, 1000.000000000000000 ) ;
#71887 = EDGE_CURVE ( 'NONE', #57102, #32622, #49936, .T. ) ;
#71888 = CIRCLE ( 'NONE', #74316, 42.00000000000000000 ) ;
#71889 = DIRECTION ( 'NONE',  ( -1.000000000000000000, 0.000000000000000000, 0.000000000000000000 ) ) ;
#71890 =( GEOMETRIC_REPRESENTATION_CONTEXT ( 3 ) GLOBAL_UNCERTAINTY_ASSIGNED_CONTEXT ( ( #60175 ) ) GLOBAL_UNIT_ASSIGNED_CONTEXT ( ( #57499, #31032, #49072 ) ) REPRESENTATION_CONTEXT ( 'NONE', 'WORKASPACE' ) );
#71891 = CARTESIAN_POINT ( 'NONE',  ( -10.00000000000000000, 0.000000000000000000, 0.000000000000000000 ) ) ;
#71892 = CARTESIAN_POINT ( 'NONE',  ( 15.00000000000000000, 22.07842321921480888, -8.187992925817425771 ) ) ;
#71893 = DIRECTION ( 'NONE',  ( 0.000000000000000000, 0.000000000000000000, 1.000000000000000000 ) ) ;
#71894 = VERTEX_POINT ( 'NONE', #60501 ) ;
#71895 = CARTESIAN_POINT ( 'NONE',  ( 16.30584220631899228, -140.9432449716519784, 5.500000000000000000 ) ) ;
#71896 = CYLINDRICAL_SURFACE ( 'NONE', #49077, 42.00000000000000000 ) ;
#71897 = LINE ( 'NONE', #32415, #16172 ) ;
#71898 = EDGE_CURVE ( 'NONE', #5103, #57712, #3637, .T. ) ;
#71899 = EDGE_CURVE ( 'NONE', #73400, #60921, #26261, .T. ) ;
#71900 = DIRECTION ( 'NONE',  ( 0.000000000000000000, 0.000000000000000000, 1.000000000000000000 ) ) ;
#71901 = EDGE_LOOP ( 'NONE', ( #12036, #22254, #72094, #20305 ) ) ;
#71902 = CIRCLE ( 'NONE', #7087, 15.69999999999999929 ) ;
#71903 = FACE_OUTER_BOUND ( 'NONE', #61932, .T. ) ;
#71904 = CARTESIAN_POINT ( 'NONE',  ( 19.29194287201271862, -133.5026271600380880, -5.500000000000000000 ) ) ;
#71905 = ORIENTED_EDGE ( 'NONE', *, *, #66241, .T. ) ;
#71906 = FACE_OUTER_BOUND ( 'NONE', #17955, .T. ) ;
#71907 = ORIENTED_EDGE ( 'NONE', *, *, #546, .T. ) ;
#71908 = AXIS2_PLACEMENT_3D ( 'NONE', #52043, #23852, #47524 ) ;
#71909 = CIRCLE ( 'NONE', #67092, 31.99999999999998579 ) ;
#71910 = ORIENTED_EDGE ( 'NONE', *, *, #43748, .F. ) ;
#71911 = CARTESIAN_POINT ( 'NONE',  ( 11.99999999999999822, -11.30684508768393748, 76.66974797899833050 ) ) ;
#71912 = CIRCLE ( 'NONE', #10700, 16.00000000000000000 ) ;
#71913 = ORIENTED_EDGE ( 'NONE', *, *, #4032, .T. ) ;
#71914 = ORIENTED_EDGE ( 'NONE', *, *, #40194, .F. ) ;
#71915 = AXIS2_PLACEMENT_3D ( 'NONE', #29637, #24750, #57498 ) ;
#71916 = ORIENTED_EDGE ( 'NONE', *, *, #59441, .F. ) ;
#71917 = ORIENTED_EDGE ( 'NONE', *, *, #48364, .F. ) ;
#71918 = CARTESIAN_POINT ( 'NONE',  ( -2.500000000000015543, -73.00000000000001421, -204.9999999999999716 ) ) ;
#71919 = ORIENTED_EDGE ( 'NONE', *, *, #3942, .T. ) ;
#71920 = ORIENTED_EDGE ( 'NONE', *, *, #38527, .T. ) ;
#71921 = CARTESIAN_POINT ( 'NONE',  ( 97.30629616937498838, 91.33154071421968467, 77.47197916753381719 ) ) ;
#71922 = DIRECTION ( 'NONE',  ( -1.000000000000000000, 0.000000000000000000, -0.000000000000000000 ) ) ;
#71923 = CARTESIAN_POINT ( 'NONE',  ( -96.32500000000001705, 87.70503267997129626, 85.02583333333332405 ) ) ;
#71924 = VECTOR ( 'NONE', #50421, 1000.000000000000000 ) ;
#71925 = ORIENTED_EDGE ( 'NONE', *, *, #22571, .F. ) ;
#71927 = ORIENTED_EDGE ( 'NONE', *, *, #19114, .F. ) ;
#71926 = CIRCLE ( 'NONE', #49135, 42.00000000000000000 ) ;
#71928 = ORIENTED_EDGE ( 'NONE', *, *, #485, .T. ) ;
#71929 = CARTESIAN_POINT ( 'NONE',  ( 0.000000000000000000, -16.45098606841102651, -33.79645857604531045 ) ) ;
#71930 = ORIENTED_EDGE ( 'NONE', *, *, #56192, .F. ) ;
#71931 = CARTESIAN_POINT ( 'NONE',  ( 95.00000000000000000, -206.9400435732949575, 74.68062500173429896 ) ) ;
#71932 = AXIS2_PLACEMENT_3D ( 'NONE', #61293, #55640, #61659 ) ;
#71933 = AXIS2_PLACEMENT_3D ( 'NONE', #32188, #37111, #4392 ) ;
#71934 = CARTESIAN_POINT ( 'NONE',  ( 0.2222846562986464380, 0.7996808935908076288, 53.20000000000001705 ) ) ;
#71935 = CARTESIAN_POINT ( 'NONE',  ( 97.64999999999999147, 90.00000000000002842, 83.96750000000000114 ) ) ;
#71936 = CARTESIAN_POINT ( 'NONE',  ( -95.78927932462359252, 92.27861417635790531, 74.85481846778735360 ) ) ;
#71937 = CARTESIAN_POINT ( 'NONE',  ( 10.00000000000000000, 30.80686688397010542, 21.53537804866092387 ) ) ;
#71938 = DIRECTION ( 'NONE',  ( -0.000000000000000000, -0.000000000000000000, 1.000000000000000000 ) ) ;
#71939 = CARTESIAN_POINT ( 'NONE',  ( -94.99999999999997158, -209.9999999999999716, 90.00000000000000000 ) ) ;
#71940 = CIRCLE ( 'NONE', #47910, 82.00000000000000000 ) ;
#71941 = DIRECTION ( 'NONE',  ( 0.000000000000000000, 1.000000000000000000, 3.491481338843133355E-15 ) ) ;
#71942 = CIRCLE ( 'NONE', #34713, 77.49899999999999523 ) ;
#71943 = CARTESIAN_POINT ( 'NONE',  ( -97.64999999999994884, -211.5299782133524502, 76.79729166840095900 ) ) ;
#71944 = DIRECTION ( 'NONE',  ( 0.000000000000000000, 0.000000000000000000, 1.000000000000000000 ) ) ;
#71945 = ORIENTED_EDGE ( 'NONE', *, *, #66053, .F. ) ;
#71947 = CARTESIAN_POINT ( 'NONE',  ( -92.69370383062504004, 90.00000000000004263, 87.42031250086714067 ) ) ;
#71946 = CARTESIAN_POINT ( 'NONE',  ( 96.15314808468748708, 91.99731107132950569, 86.89114583420047211 ) ) ;
#71948 = ORIENTED_EDGE ( 'NONE', *, *, #55798, .F. ) ;
#71949 = CARTESIAN_POINT ( 'NONE',  ( 94.99999999999998579, 87.33691857156068750, 77.26031250086714408 ) ) ;
#71950 = CARTESIAN_POINT ( 'NONE',  ( 0.000000000000000000, -46.11716303203136391, -67.80270845531939017 ) ) ;
#71951 = CARTESIAN_POINT ( 'NONE',  ( 95.00000000000000000, -213.0599564267049857, 87.61874999999999147 ) ) ;
#71952 = DIRECTION ( 'NONE',  ( 0.000000000000000000, 0.000000000000000000, 1.000000000000000000 ) ) ;
#71953 = CARTESIAN_POINT ( 'NONE',  ( -92.35000000000005116, 89.99998452726650555, 78.33187446658585884 ) ) ;
#71954 = CARTESIAN_POINT ( 'NONE',  ( -92.35000000000003695, 90.00000000000004263, 89.04749999999999943 ) ) ;
#71955 = EDGE_CURVE ( 'NONE', #46060, #29601, #10809, .T. ) ;
#71956 = CARTESIAN_POINT ( 'NONE',  ( 10.00000000000000000, 37.58145647212455032, -0.6853352020786441789 ) ) ;
#71957 = ORIENTED_EDGE ( 'NONE', *, *, #52288, .T. ) ;
#71958 = ADVANCED_FACE ( 'NONE', ( #37196 ), #54117, .T. ) ;
#71959 = ORIENTED_EDGE ( 'NONE', *, *, #66619, .F. ) ;
#71960 = EDGE_CURVE ( 'NONE', #59828, #503, #1248, .T. ) ;
#71961 = CARTESIAN_POINT ( 'NONE',  ( 10.00000000000000000, -74.65491531819111515, -8.830959090343204920 ) ) ;
#71962 = CARTESIAN_POINT ( 'NONE',  ( 11.99999999999999822, 0.000000000000000000, 0.000000000000000000 ) ) ;
#71963 = CARTESIAN_POINT ( 'NONE',  ( -96.32500000000001705, 92.29496732002878900, 86.16354166840096696 ) ) ;
#71964 = FACE_OUTER_BOUND ( 'NONE', #53908, .T. ) ;
#71965 = DIRECTION ( 'NONE',  ( -1.000000000000000000, -0.000000000000000000, -0.000000000000000000 ) ) ;
#71966 = CARTESIAN_POINT ( 'NONE',  ( 11.99999999999999822, 63.97538442413427617, 51.29473840253247374 ) ) ;
#71967 = EDGE_CURVE ( 'NONE', #18041, #37728, #49566, .T. ) ;
#71968 = AXIS2_PLACEMENT_3D ( 'NONE', #47377, #36089, #13525 ) ;
#71969 = EDGE_LOOP ( 'NONE', ( #28288, #56596, #32811, #45514 ) ) ;
#71970 = CARTESIAN_POINT ( 'NONE',  ( -96.15314808468751551, 88.00268892867056536, 82.76364583420047438 ) ) ;
#71972 = CARTESIAN_POINT ( 'NONE',  ( -20.63750000000000284, -2.946905753441389499E-14, -1.643265707204933640E-14 ) ) ;
#71971 = AXIS2_PLACEMENT_3D ( 'NONE', #38770, #72956, #9821 ) ;
#71973 = LINE ( 'NONE', #72699, #22264 ) ;
#71974 = SURFACE_SIDE_STYLE ('',( #9199 ) ) ;
#71975 = CYLINDRICAL_SURFACE ( 'NONE', #934, 82.00000000000000000 ) ;
#71976 = VECTOR ( 'NONE', #53154, 1000.000000000000000 ) ;
#71977 = CARTESIAN_POINT ( 'NONE',  ( 10.00000000000000000, 49.70050353004889132, 59.46389618801982380 ) ) ;
#71978 = DIRECTION ( 'NONE',  ( -1.000000000000000000, 0.000000000000000000, 0.000000000000000000 ) ) ;
#71979 = DIRECTION ( 'NONE',  ( 1.000000000000000000, -0.000000000000000000, -0.000000000000000000 ) ) ;
#71980 = CARTESIAN_POINT ( 'NONE',  ( 11.99999999999999822, -59.46389618801999433, 49.70050353004867816 ) ) ;
#71981 = EDGE_CURVE ( 'NONE', #22641, #15441, #43246, .T. ) ;
#71982 = DIRECTION ( 'NONE',  ( 0.000000000000000000, 0.000000000000000000, 1.000000000000000000 ) ) ;
#71983 = ADVANCED_FACE ( 'NONE', ( #3736 ), #14987, .T. ) ;
#71984 = CARTESIAN_POINT ( 'NONE',  ( 96.15314808468748708, 88.00268892867053694, 79.85322916753381151 ) ) ;
#71985 = CARTESIAN_POINT ( 'NONE',  ( -96.15314808468745866, -211.9973110713294489, 84.19239583420049655 ) ) ;
#71986 = FACE_OUTER_BOUND ( 'NONE', #57619, .T. ) ;
#71987 = VECTOR ( 'NONE', #57010, 1000.000000000000000 ) ;
#71988 = ORIENTED_EDGE ( 'NONE', *, *, #70119, .F. ) ;
#71989 = FACE_OUTER_BOUND ( 'NONE', #47735, .T. ) ;
#71990 = UNCERTAINTY_MEASURE_WITH_UNIT (LENGTH_MEASURE( 1.000000000000000082E-05 ), #31516, 'distance_accuracy_value', 'NONE');
#71991 = CARTESIAN_POINT ( 'NONE',  ( -97.64999999999994884, -211.5299782133524502, 79.25791666666665947 ) ) ;
#71992 = CARTESIAN_POINT ( 'NONE',  ( 10.00000000000000000, 6.555932627142952995, -37.01155633439051940 ) ) ;
#71993 = VECTOR ( 'NONE', #67511, 1000.000000000000114 ) ;
#71994 = ADVANCED_FACE ( 'NONE', ( #55214 ), #43948, .F. ) ;
#71995 = EDGE_CURVE ( 'NONE', #72558, #23616, #42052, .T. ) ;
#71996 = AXIS2_PLACEMENT_3D ( 'NONE', #17141, #40076, #28407 ) ;
#71997 = CIRCLE ( 'NONE', #1221, 82.00000000000000000 ) ;
#71998 = CIRCLE ( 'NONE', #45631, 77.49899999999999523 ) ;
#71999 = CARTESIAN_POINT ( 'NONE',  ( 92.69370383062501162, -209.9999999999999716, 84.56281250086713897 ) ) ;
#72000 = EDGE_LOOP ( 'NONE', ( #50283, #40311, #24212, #52504 ) ) ;
#72001 = DIRECTION ( 'NONE',  ( -1.000000000000000000, 0.000000000000000000, 0.000000000000000000 ) ) ;
#72002 = ORIENTED_EDGE ( 'NONE', *, *, #28248, .F. ) ;
#72003 = LINE ( 'NONE', #49447, #6832 ) ;
#72004 = VERTEX_POINT ( 'NONE', #72852 ) ;
#72005 = DIRECTION ( 'NONE',  ( -1.000000000000000000, 0.000000000000000000, -0.000000000000000000 ) ) ;
#72006 = ORIENTED_EDGE ( 'NONE', *, *, #42953, .F. ) ;
#72007 = CARTESIAN_POINT ( 'NONE',  ( 97.30629616937498838, -211.3315407142195852, 76.73114583420048973 ) ) ;
#72008 = CARTESIAN_POINT ( 'NONE',  ( -7.670864526094547386, -97.73662565058241114, -2.500000000000000000 ) ) ;
#72009 = CARTESIAN_POINT ( 'NONE',  ( 0.000000000000000000, 0.000000000000000000, 0.000000000000000000 ) ) ;
#72010 = CARTESIAN_POINT ( 'NONE',  ( -97.51367041768835975, 89.99999999999990052, 74.91808492278043730 ) ) ;
#72011 = CARTESIAN_POINT ( 'NONE',  ( 7.001685179585692254, -14.98378029539707512, -1.199999999999999956 ) ) ;
#72012 = DIRECTION ( 'NONE',  ( 0.000000000000000000, 0.5877852522924684742, 0.8090169943749506709 ) ) ;
#72013 = CARTESIAN_POINT ( 'NONE',  ( 93.67500000000001137, -212.2949673200287179, 81.21583333333333599 ) ) ;
#72014 = CIRCLE ( 'NONE', #15581, 82.00000000000000000 ) ;
#72015 = EDGE_LOOP ( 'NONE', ( #44936, #50406, #63929, #8312 ) ) ;
#72016 = ORIENTED_EDGE ( 'NONE', *, *, #8397, .F. ) ;
#72017 = VERTEX_POINT ( 'NONE', #42462 ) ;
#72018 = ORIENTED_EDGE ( 'NONE', *, *, #37251, .F. ) ;
#72019 = DIRECTION ( 'NONE',  ( 0.000000000000000000, 0.000000000000000000, 1.000000000000000000 ) ) ;
#72020 = CARTESIAN_POINT ( 'NONE',  ( -92.69370383062502583, 91.33154071421968467, 83.82197916753382572 ) ) ;
#72021 = CARTESIAN_POINT ( 'NONE',  ( -95.00000000000002842, 86.94004357329504273, 81.98312500173430806 ) ) ;
#72022 = VECTOR ( 'NONE', #30084, 1000.000000000000114 ) ;
#72023 = EDGE_CURVE ( 'NONE', #53084, #45726, #65402, .T. ) ;
#72024 = CARTESIAN_POINT ( 'NONE',  ( 11.99999999999999822, -34.44570377933647620, 69.42325613327427902 ) ) ;
#72025 = CARTESIAN_POINT ( 'NONE',  ( 95.53230763903962952, 86.73322217287211799, 74.92222617501700199 ) ) ;
#72026 = CARTESIAN_POINT ( 'NONE',  ( 11.99999999999999822, 66.50666863322055633, -39.78640506895536078 ) ) ;
#72027 = EDGE_CURVE ( 'NONE', #36877, #10469, #59755, .T. ) ;
#72028 = ORIENTED_EDGE ( 'NONE', *, *, #38968, .T. ) ;
#72029 = CARTESIAN_POINT ( 'NONE',  ( -96.32499999999996021, -207.7050326799711968, 85.52854166840096184 ) ) ;
#72030 = ORIENTED_EDGE ( 'NONE', *, *, #20488, .T. ) ;
#72031 = CARTESIAN_POINT ( 'NONE',  ( 10.00000000000000000, 0.000000000000000000, 0.000000000000000000 ) ) ;
#72033 = VERTEX_POINT ( 'NONE', #33769 ) ;
#72032 = EDGE_CURVE ( 'NONE', #3104, #64823, #37272, .T. ) ;
#72034 = CARTESIAN_POINT ( 'NONE',  ( -95.00000000000002842, 93.05995642670501411, 83.57062500173429953 ) ) ;
#72035 = ORIENTED_EDGE ( 'NONE', *, *, #33710, .F. ) ;
#72036 = CARTESIAN_POINT ( 'NONE',  ( 94.99999999999998579, 92.66308142843935514, 87.73781250086715033 ) ) ;
#72037 = DIRECTION ( 'NONE',  ( 0.000000000000000000, -0.3090169943749548342, 0.9510565162951511997 ) ) ;
#72038 = LINE ( 'NONE', #55502, #12622 ) ;
#72039 = EDGE_CURVE ( 'NONE', #32534, #66402, #13210, .T. ) ;
#72040 = CARTESIAN_POINT ( 'NONE',  ( 10.00000000000000000, -22.64427369931148348, -30.00120703465229965 ) ) ;
#72041 = VECTOR ( 'NONE', #46095, 999.9999999999998863 ) ;
#72042 = DIRECTION ( 'NONE',  ( -1.000000000000000000, -0.000000000000000000, -0.000000000000000000 ) ) ;
#72043 = FACE_OUTER_BOUND ( 'NONE', #24944, .T. ) ;
#72044 = ORIENTED_EDGE ( 'NONE', *, *, #65536, .F. ) ;
#72045 = FACE_OUTER_BOUND ( 'NONE', #12289, .T. ) ;
#72046 = CIRCLE ( 'NONE', #8410, 77.49899999999999523 ) ;
#72048 = CARTESIAN_POINT ( 'NONE',  ( 99.99999999999998579, 95.00000000000002842, -90.00000000000000000 ) ) ;
#72047 = AXIS2_PLACEMENT_3D ( 'NONE', #25645, #36924, #60965 ) ;
#72049 = VERTEX_POINT ( 'NONE', #73985 ) ;
#72050 = ADVANCED_FACE ( 'NONE', ( #33382 ), #34504, .F. ) ;
#72051 = ORIENTED_EDGE ( 'NONE', *, *, #9273, .T. ) ;
#72052 = CARTESIAN_POINT ( 'NONE',  ( 92.34999999999999432, 88.47002178664752137, 78.70229166840096013 ) ) ;
#72053 = AXIS2_PLACEMENT_3D ( 'NONE', #39125, #21825, #44772 ) ;
#72054 = VECTOR ( 'NONE', #17363, 1000.000000000000000 ) ;
#72055 = DIRECTION ( 'NONE',  ( -1.000000000000000000, -0.000000000000000000, 0.000000000000000000 ) ) ;
#72056 = CARTESIAN_POINT ( 'NONE',  ( -96.32499999999996021, -212.2949673200287179, 83.12083333333332291 ) ) ;
#72057 =( BOUNDED_CURVE ( )  B_SPLINE_CURVE ( 2, ( #2376, #42194, #53095, #65860, #7235, #13960, #59112 ),
 .UNSPECIFIED., .F., .F. ) 
 B_SPLINE_CURVE_WITH_KNOTS ( ( 3, 2, 2, 3 ),
 ( 0.9374999999999995559, 0.9444444444444441977, 0.9513888888888889506, 0.9583333333333337034 ),
 .UNSPECIFIED. ) 
 CURVE ( )  GEOMETRIC_REPRESENTATION_ITEM ( )  RATIONAL_B_SPLINE_CURVE ( ( 1.000000000000008660, 0.8660254037844301589, 1.000000000000000000, 0.8660254037844387076, 1.000000000000000000, 0.8660254037844322683, 1.000000000000006439 ) ) 
 REPRESENTATION_ITEM ( '' )  );
#72058 = CARTESIAN_POINT ( 'NONE',  ( -96.15314808468745866, -211.9973110713294489, 84.19239583420049655 ) ) ;
#72059 = ORIENTED_EDGE ( 'NONE', *, *, #25235, .T. ) ;
#72060 = ADVANCED_FACE ( 'NONE', ( #22122 ), #61984, .T. ) ;
#72061 = FACE_OUTER_BOUND ( 'NONE', #74233, .T. ) ;
#72062 = ORIENTED_EDGE ( 'NONE', *, *, #51929, .F. ) ;
#72063 = DIRECTION ( 'NONE',  ( -1.000000000000000000, 0.000000000000000000, 0.000000000000000000 ) ) ;
#72064 = VECTOR ( 'NONE', #24745, 1000.000000000000000 ) ;
#72065 = DIRECTION ( 'NONE',  ( -1.000000000000000000, -0.000000000000000000, -0.000000000000000000 ) ) ;
#72066 = FACE_OUTER_BOUND ( 'NONE', #23065, .T. ) ;
#72067 = CARTESIAN_POINT ( 'NONE',  ( 92.69370383062498320, 88.66845928578035796, 78.90072916753381094 ) ) ;
#72068 = CARTESIAN_POINT ( 'NONE',  ( 0.000000000000000000, -6.903761155837269570, -77.19088730480530103 ) ) ;
#72069 = FACE_OUTER_BOUND ( 'NONE', #54852, .T. ) ;
#72070 = CARTESIAN_POINT ( 'NONE',  ( 11.99999999999999822, 0.000000000000000000, 0.000000000000000000 ) ) ;
#72071 = CARTESIAN_POINT ( 'NONE',  ( 92.54662210827905255, 90.48452257634333762, 74.90854212414863866 ) ) ;
#72072 = FACE_BOUND ( 'NONE', #56217, .T. ) ;
#72073 = EDGE_CURVE ( 'NONE', #56506, #64475, #22839, .T. ) ;
#72074 = LINE ( 'NONE', #71696, #10579 ) ;
#72075 = EDGE_CURVE ( 'NONE', #44373, #13681, #73611, .T. ) ;
#72076 = DIRECTION ( 'NONE',  ( -0.000000000000000000, -0.000000000000000000, 1.000000000000000000 ) ) ;
#72077 = CARTESIAN_POINT ( 'NONE',  ( 92.35000000039373447, 90.00002930740642171, 76.74344264317738862 ) ) ;
#72078 = ORIENTED_EDGE ( 'NONE', *, *, #14063, .T. ) ;
#72079 = AXIS2_PLACEMENT_3D ( 'NONE', #741, #33407, #10874 ) ;
#72080 = CARTESIAN_POINT ( 'NONE',  ( -97.30629616937501680, 88.66845928578038638, 81.44072916753380298 ) ) ;
#72081 = AXIS2_PLACEMENT_3D ( 'NONE', #15297, #43890, #20192 ) ;
#72082 = DIRECTION ( 'NONE',  ( 2.628368902995175337E-16, 1.000000000000000000, 0.000000000000000000 ) ) ;
#72083 = AXIS2_PLACEMENT_3D ( 'NONE', #3655, #60056, #43866 ) ;
#72084 = LINE ( 'NONE', #20593, #45031 ) ;
#72085 = ORIENTED_EDGE ( 'NONE', *, *, #62121, .T. ) ;
#72086 = DIRECTION ( 'NONE',  ( -1.000000000000000000, 0.000000000000000000, 0.000000000000000000 ) ) ;
#72087 = LINE ( 'NONE', #37895, #25219 ) ;
#72088 = DIRECTION ( 'NONE',  ( 0.000000000000000000, 0.000000000000000000, 1.000000000000000000 ) ) ;
#72089 = VECTOR ( 'NONE', #54594, 1000.000000000000000 ) ;
#72090 = AXIS2_PLACEMENT_3D ( 'NONE', #62072, #72218, #20722 ) ;
#72091 = CARTESIAN_POINT ( 'NONE',  ( -6.880223345695647197, -142.5202692415819854, -5.500000000000000000 ) ) ;
#72092 = CARTESIAN_POINT ( 'NONE',  ( 97.30629616937498838, -208.6684592857803011, 79.37697916753381833 ) ) ;
#72093 = VECTOR ( 'NONE', #24798, 1000.000000000000000 ) ;
#72094 = ORIENTED_EDGE ( 'NONE', *, *, #30013, .F. ) ;
#72095 = AXIS2_PLACEMENT_3D ( 'NONE', #18918, #1688, #20416 ) ;
#72096 = EDGE_LOOP ( 'NONE', ( #16787, #69447, #69843, #51686 ) ) ;
#72097 = EDGE_CURVE ( 'NONE', #59464, #71835, #32416, .T. ) ;
#72098 = CARTESIAN_POINT ( 'NONE',  ( 0.000000000000000000, 62.20884554314086046, -46.21855187248561236 ) ) ;
#72099 = LINE ( 'NONE', #37902, #64174 ) ;
#72100 = PLANE ( 'NONE',  #1610 ) ;
#72101 = SURFACE_SIDE_STYLE ('',( #43923 ) ) ;
#72102 = CARTESIAN_POINT ( 'NONE',  ( 93.84685191531251292, -211.9973110713294489, 77.20739583420048291 ) ) ;
#72103 = ORIENTED_EDGE ( 'NONE', *, *, #32592, .T. ) ;
#72104 = FACE_OUTER_BOUND ( 'NONE', #61313, .T. ) ;
#72105 = VERTEX_POINT ( 'NONE', #16482 ) ;
#72106 = ORIENTED_EDGE ( 'NONE', *, *, #16385, .T. ) ;
#72107 = DIRECTION ( 'NONE',  ( 1.000000000000000000, 0.000000000000000000, 0.000000000000000000 ) ) ;
#72108 = FILL_AREA_STYLE ('',( #66490 ) ) ;
#72109 = CARTESIAN_POINT ( 'NONE',  ( 22.51310757741980240, -113.2613067136482101, -2.500000000000000000 ) ) ;
#72110 = EDGE_CURVE ( 'NONE', #70989, #9267, #44312, .T. ) ;
#72111 = ORIENTED_EDGE ( 'NONE', *, *, #9585, .F. ) ;
#72112 = CARTESIAN_POINT ( 'NONE',  ( 10.00000000000000000, -21.53537804866058991, -30.80686688397033635 ) ) ;
#72113 = CARTESIAN_POINT ( 'NONE',  ( 97.64999999999999147, -209.9999999999999716, 79.60187500173429953 ) ) ;
#72114 = CARTESIAN_POINT ( 'NONE',  ( 97.64999999999997726, 88.47002178664753558, 85.81958333333331268 ) ) ;
#72115 = EDGE_CURVE ( 'NONE', #45142, #42699, #4859, .T. ) ;
#72116 = VERTEX_POINT ( 'NONE', #10464 ) ;
#72117 = CARTESIAN_POINT ( 'NONE',  ( 0.000000000000000000, -56.15606465355001120, 59.75363087400055662 ) ) ;
#72118 = DIRECTION ( 'NONE',  ( 0.000000000000000000, 0.000000000000000000, 1.000000000000000000 ) ) ;
#72119 = ORIENTED_EDGE ( 'NONE', *, *, #47267, .T. ) ;
#72120 = LINE ( 'NONE', #67980, #70443 ) ;
#72121 = CARTESIAN_POINT ( 'NONE',  ( -97.30629616937501680, 91.33154071421968467, 85.30364583420048064 ) ) ;
#72122 = CARTESIAN_POINT ( 'NONE',  ( 97.30629616937498838, 90.00000000000002842, 81.70531250086713726 ) ) ;
#72123 = ORIENTED_EDGE ( 'NONE', *, *, #62951, .T. ) ;
#72124 = EDGE_CURVE ( 'NONE', #62825, #47275, #64906, .T. ) ;
#72125 = ADVANCED_FACE ( 'NONE', ( #50685 ), #39420, .F. ) ;
#72126 = CIRCLE ( 'NONE', #8495, 82.00000000000000000 ) ;
#72127 = VECTOR ( 'NONE', #37009, 1000.000000000000000 ) ;
#72128 = DIRECTION ( 'NONE',  ( 0.000000000000000000, -0.8090169943749532244, 0.5877852522924652545 ) ) ;
#72129 = ORIENTED_EDGE ( 'NONE', *, *, #4530, .F. ) ;
#72130 = CARTESIAN_POINT ( 'NONE',  ( 0.000000000000000000, 34.44570377933598593, 69.42325613327452061 ) ) ;
#72131 = CIRCLE ( 'NONE', #16928, 11.59999999999999787 ) ;
#72132 = VERTEX_POINT ( 'NONE', #45441 ) ;
#72133 = ORIENTED_EDGE ( 'NONE', *, *, #59610, .T. ) ;
#72134 = ORIENTED_EDGE ( 'NONE', *, *, #17925, .F. ) ;
#72135 = DIRECTION ( 'NONE',  ( -1.000000000000000000, -0.000000000000000000, -0.000000000000000000 ) ) ;
#72136 = VERTEX_POINT ( 'NONE', #11569 ) ;
#72137 = DIRECTION ( 'NONE',  ( -1.000000000000000000, -0.000000000000000000, -0.000000000000000000 ) ) ;
#72138 = DIRECTION ( 'NONE',  ( -1.000000000000000000, -0.000000000000000000, 0.000000000000000000 ) ) ;
#72139 = ORIENTED_EDGE ( 'NONE', *, *, #62214, .F. ) ;
#72140 = CARTESIAN_POINT ( 'NONE',  ( 0.000000000000000000, 12.93880638057426502, -76.41127070299258150 ) ) ;
#72141 = CARTESIAN_POINT ( 'NONE',  ( -97.30629616937495996, -209.9999999999999716, 78.21281250086714465 ) ) ;
#72142 = ORIENTED_EDGE ( 'NONE', *, *, #917, .T. ) ;
#72144 = EDGE_CURVE ( 'NONE', #15908, #61999, #44545, .T. ) ;
#72143 = DIRECTION ( 'NONE',  ( 0.000000000000000000, 0.4539904997395477482, -0.8910065241883673437 ) ) ;
#72145 = DIRECTION ( 'NONE',  ( 0.000000000000000000, -0.8660254037844374864, 0.5000000000000019984 ) ) ;
#72146 = LINE ( 'NONE', #20656, #15310 ) ;
#72147 = CARTESIAN_POINT ( 'NONE',  ( -96.32499999999996021, -207.7050326799711968, 89.33854166840096411 ) ) ;
#72148 = DIRECTION ( 'NONE',  ( -1.000000000000000000, -0.000000000000000000, 0.000000000000000000 ) ) ;
#72149 = AXIS2_PLACEMENT_3D ( 'NONE', #70641, #53013, #42105 ) ;
#72150 = VECTOR ( 'NONE', #53658, 1000.000000000000227 ) ;
#72151 = CARTESIAN_POINT ( 'NONE',  ( 0.000000000000000000, -41.81611651403864727, 3.925862922256025289 ) ) ;
#72152 = CARTESIAN_POINT ( 'NONE',  ( 93.84685191531248449, 91.99731107132950569, 89.53697916753381492 ) ) ;
#72153 = CYLINDRICAL_SURFACE ( 'NONE', #55626, 2.649999999999985700 ) ;
#72154 = AXIS2_PLACEMENT_3D ( 'NONE', #7457, #7084, #1491 ) ;
#72155 = DIRECTION ( 'NONE',  ( -1.000000000000000000, 0.000000000000000000, -0.000000000000000000 ) ) ;
#72156 = CARTESIAN_POINT ( 'NONE',  ( -97.65000000000001990, 89.99996562134467126, 88.80937619077336365 ) ) ;
#72157 = DIRECTION ( 'NONE',  ( -1.000000000000000000, 0.000000000000000000, 0.000000000000000000 ) ) ;
#72158 = EDGE_CURVE ( 'NONE', #33464, #36312, #70726, .T. ) ;
#72159 = DIRECTION ( 'NONE',  ( -1.000000000000000000, -0.000000000000000000, 0.000000000000000000 ) ) ;
#72160 = CARTESIAN_POINT ( 'NONE',  ( 11.99999999999999822, 55.19960302592141232, -51.03279382321027668 ) ) ;
#72161 = CARTESIAN_POINT ( 'NONE',  ( 3.000000000000000000, 2.935248768560057897, -3.252606517456513302E-15 ) ) ;
#72162 = EDGE_CURVE ( 'NONE', #64812, #43566, #67243, .T. ) ;
#72163 = DIRECTION ( 'NONE',  ( 0.000000000000000000, -6.938893903907231533E-15, 1.000000000000000000 ) ) ;
#72164 = DIRECTION ( 'NONE',  ( 1.000000000000000000, 0.000000000000000000, 0.000000000000000000 ) ) ;
#72165 = CARTESIAN_POINT ( 'NONE',  ( 5.000000000000000000, 51.29473840253317718, -63.97538442413369353 ) ) ;
#72166 = DIRECTION ( 'NONE',  ( 0.000000000000000000, 0.7071067811865487940, -0.7071067811865462405 ) ) ;
#72167 = DIRECTION ( 'NONE',  ( 1.000000000000000000, -0.000000000000000000, 0.000000000000000000 ) ) ;
#72168 = CARTESIAN_POINT ( 'NONE',  ( -97.64999999999994884, -208.4700217866474645, 88.67708333333332860 ) ) ;
#72169 = LINE ( 'NONE', #3778, #50590 ) ;
#72170 = ORIENTED_EDGE ( 'NONE', *, *, #22835, .T. ) ;
#72171 = LINE ( 'NONE', #43992, #8862 ) ;
#72172 = LINE ( 'NONE', #60189, #67100 ) ;
#72173 = FILL_AREA_STYLE_COLOUR ( '', #1054 ) ;
#72174 = CARTESIAN_POINT ( 'NONE',  ( -10.00000000000000000, 0.000000000000000000, 0.000000000000000000 ) ) ;
#72175 = AXIS2_PLACEMENT_3D ( 'NONE', #64395, #51623, #69655 ) ;
#72176 = CIRCLE ( 'NONE', #35009, 42.00000000000000000 ) ;
#72177 = AXIS2_PLACEMENT_3D ( 'NONE', #51997, #549, #69670 ) ;
#72178 = ORIENTED_EDGE ( 'NONE', *, *, #32044, .T. ) ;
#72179 = ORIENTED_EDGE ( 'NONE', *, *, #51999, .T. ) ;
#72180 = DIRECTION ( 'NONE',  ( 0.000000000000000000, -0.4539904997395350916, -0.8910065241883738940 ) ) ;
#72181 = VECTOR ( 'NONE', #54390, 1000.000000000000000 ) ;
#72182 = LINE ( 'NONE', #44002, #5546 ) ;
#72183 = ORIENTED_EDGE ( 'NONE', *, *, #15867, .T. ) ;
#72184 = EDGE_CURVE ( 'NONE', #32720, #66019, #10846, .T. ) ;
#72185 = CARTESIAN_POINT ( 'NONE',  ( 95.00000000000000000, -212.6630814284392557, 82.18156250086715886 ) ) ;
#72186 = CARTESIAN_POINT ( 'NONE',  ( 95.00000000000000000, -212.6630814284392557, 84.88031250086713442 ) ) ;
#72187 = ORIENTED_EDGE ( 'NONE', *, *, #36343, .F. ) ;
#72188 = CARTESIAN_POINT ( 'NONE',  ( 93.84685191531251292, -211.9973110713294489, 87.36739583420049371 ) ) ;
#72189 = ORIENTED_EDGE ( 'NONE', *, *, #5276, .F. ) ;
#72190 = CARTESIAN_POINT ( 'NONE',  ( -15.50000000000000000, 1.898202538678397557E-15, -4.400000000000001243 ) ) ;
#72191 = ORIENTED_EDGE ( 'NONE', *, *, #53833, .F. ) ;
#72192 = AXIS2_PLACEMENT_3D ( 'NONE', #47110, #909, #23796 ) ;
#72193 = CARTESIAN_POINT ( 'NONE',  ( -93.84685191531254134, 91.99731107132950569, 77.52489583420047836 ) ) ;
#72194 = EDGE_CURVE ( 'NONE', #2973, #1386, #48102, .T. ) ;
#72195 = AXIS2_PLACEMENT_3D ( 'NONE', #8143, #31068, #35602 ) ;
#72196 = EDGE_LOOP ( 'NONE', ( #67357, #22945 ) ) ;
#72197 = VERTEX_POINT ( 'NONE', #41627 ) ;
#72198 = CARTESIAN_POINT ( 'NONE',  ( 0.000000000000000000, -35.91791733033525702, 68.67312586194982771 ) ) ;
#72199 = EDGE_CURVE ( 'NONE', #14912, #38997, #20474, .T. ) ;
#72200 = ORIENTED_EDGE ( 'NONE', *, *, #14170, .F. ) ;
#72201 = CARTESIAN_POINT ( 'NONE',  ( 0.000000000000000000, -8.966570791701281351, 81.50828551894224461 ) ) ;
#72202 = CARTESIAN_POINT ( 'NONE',  ( 0.000000000000000000, 0.000000000000000000, 0.000000000000000000 ) ) ;
#72203 = ORIENTED_EDGE ( 'NONE', *, *, #2897, .T. ) ;
#72204 = CARTESIAN_POINT ( 'NONE',  ( 0.000000000000000000, 78.73519480814985627, -22.90783923731548910 ) ) ;
#72205 = EDGE_LOOP ( 'NONE', ( #58631, #28201, #34508, #18476 ) ) ;
#72206 = AXIS2_PLACEMENT_3D ( 'NONE', #36855, #59802, #8286 ) ;
#72207 = CARTESIAN_POINT ( 'NONE',  ( 97.65000000000000568, -211.5299782133524218, 81.45395833506763950 ) ) ;
#72208 = ORIENTED_EDGE ( 'NONE', *, *, #49829, .F. ) ;
#72209 = EDGE_CURVE ( 'NONE', #52406, #58523, #41664, .T. ) ;
#72210 = EDGE_LOOP ( 'NONE', ( #42540, #46059, #52919, #37404 ) ) ;
#72211 = ORIENTED_EDGE ( 'NONE', *, *, #20877, .T. ) ;
#72212 = CARTESIAN_POINT ( 'NONE',  ( 97.30629616937498838, -208.6684592857803011, 77.31322916753380525 ) ) ;
#72213 = ITEM_DEFINED_TRANSFORMATION ( 'NONE', 'NONE', #9977,  #43395 ) ;
#72214 = LINE ( 'NONE', #67703, #52229 ) ;
#72215 = ORIENTED_EDGE ( 'NONE', *, *, #18311, .F. ) ;
#72216 = ORIENTED_EDGE ( 'NONE', *, *, #1341, .F. ) ;
#72217 = ORIENTED_EDGE ( 'NONE', *, *, #8653, .F. ) ;
#72218 = DIRECTION ( 'NONE',  ( 0.000000000000000000, 0.000000000000000000, -1.000000000000000000 ) ) ;
#72219 = CARTESIAN_POINT ( 'NONE',  ( 0.000000000000000000, 0.000000000000000000, 0.000000000000000000 ) ) ;
#72220 = CARTESIAN_POINT ( 'NONE',  ( -92.69370383062504004, 90.00000000000004263, 78.68906250086715204 ) ) ;
#72221 = EDGE_LOOP ( 'NONE', ( #12523, #38372, #49248, #32704 ) ) ;
#72222 = EDGE_CURVE ( 'NONE', #29677, #42164, #1308, .T. ) ;
#72223 = CARTESIAN_POINT ( 'NONE',  ( 96.15314808468748708, 91.99731107132950569, 76.09614583420047040 ) ) ;
#72224 = ORIENTED_EDGE ( 'NONE', *, *, #59842, .T. ) ;
#72225 = FILL_AREA_STYLE ('',( #67713 ) ) ;
#72226 = FACE_OUTER_BOUND ( 'NONE', #53713, .T. ) ;
#72228 = ADVANCED_FACE ( 'NONE', ( #69823 ), #46913, .F. ) ;
#72227 = DIRECTION ( 'NONE',  ( -0.000000000000000000, -0.000000000000000000, -1.000000000000000000 ) ) ;
#72229 = CYLINDRICAL_SURFACE ( 'NONE', #68022, 32.00000000000000000 ) ;
#72230 = FACE_OUTER_BOUND ( 'NONE', #63892, .T. ) ;
#72231 = CARTESIAN_POINT ( 'NONE',  ( -92.69370383062498320, -208.6684592857803295, 77.94822916753381037 ) ) ;
#72232 = PRESENTATION_LAYER_ASSIGNMENT (  '', '', ( #31450 ) ) ;
#72233 = CIRCLE ( 'NONE', #61472, 31.99999999999999289 ) ;
#72234 = DIRECTION ( 'NONE',  ( -1.000000000000000000, 0.000000000000000000, -0.000000000000000000 ) ) ;
#72235 = CARTESIAN_POINT ( 'NONE',  ( 11.99999999999999822, 0.000000000000000000, 0.000000000000000000 ) ) ;
#72236 = EDGE_CURVE ( 'NONE', #47150, #66356, #74104, .T. ) ;
#72237 = CARTESIAN_POINT ( 'NONE',  ( 5.000000000000000000, -35.47612816024506088, -22.48208911017539435 ) ) ;
#72238 = ORIENTED_EDGE ( 'NONE', *, *, #66278, .F. ) ;
#72239 = CIRCLE ( 'NONE', #66255, 31.99999999999998934 ) ;
#72240 = VERTEX_POINT ( 'NONE', #35252 ) ;
#72241 = CARTESIAN_POINT ( 'NONE',  ( 0.000000000000000000, -18.89407956138310496, 75.16055320797023853 ) ) ;
#72242 = DIRECTION ( 'NONE',  ( 0.000000000000000000, 0.000000000000000000, 1.000000000000000000 ) ) ;
#72243 = CARTESIAN_POINT ( 'NONE',  ( -11.63999999999999702, 0.000000000000000000, 12.50000000000000000 ) ) ;
#72244 = AXIS2_PLACEMENT_3D ( 'NONE', #30988, #53944, #2482 ) ;
#72245 = EDGE_CURVE ( 'NONE', #34982, #5325, #18325, .T. ) ;
#72246 = CARTESIAN_POINT ( 'NONE',  ( -93.84685191531254134, 91.99731107132950569, 86.25614583420048120 ) ) ;
#72247 = DIRECTION ( 'NONE',  ( -1.000000000000000000, -0.000000000000000000, -0.000000000000000000 ) ) ;
#72248 = CARTESIAN_POINT ( 'NONE',  ( 5.822613034544236399, -142.8165987265839760, 5.500000000000000000 ) ) ;
#72249 = VECTOR ( 'NONE', #66765, 1000.000000000000000 ) ;
#72250 = ORIENTED_EDGE ( 'NONE', *, *, #53131, .F. ) ;
#72251 = DIRECTION ( 'NONE',  ( 0.000000000000000000, -0.9510565162951565288, 0.3090169943749384029 ) ) ;
#72252 = VECTOR ( 'NONE', #22606, 1000.000000000000000 ) ;
#72253 = CARTESIAN_POINT ( 'NONE',  ( 11.99999999999999822, -74.65491531819111515, 23.16904090965678265 ) ) ;
#72254 = DIRECTION ( 'NONE',  ( -1.000000000000000000, 0.000000000000000000, 0.000000000000000000 ) ) ;
#72255 = VECTOR ( 'NONE', #71659, 1000.000000000000000 ) ;
#72256 = CARTESIAN_POINT ( 'NONE',  ( 5.000000000000000000, -77.16300072079681627, 27.74655509720641078 ) ) ;
#72257 = CARTESIAN_POINT ( 'NONE',  ( 10.00000000000000000, -31.46837873494930093, -68.27212725128309501 ) ) ;
#72258 = DIRECTION ( 'NONE',  ( -0.000000000000000000, 0.000000000000000000, -1.000000000000000000 ) ) ;
#72259 = CARTESIAN_POINT ( 'NONE',  ( -97.30629616937495996, -209.9999999999999716, 84.08656250086716000 ) ) ;
#72260 = SURFACE_SIDE_STYLE ('',( #48236 ) ) ;
#72261 = AXIS2_PLACEMENT_3D ( 'NONE', #7645, #47501, #70402 ) ;
#72262 = CARTESIAN_POINT ( 'NONE',  ( 10.00000000000000000, 75.54627589209970040, -17.28742895386005785 ) ) ;
#72263 =( BOUNDED_CURVE ( )  B_SPLINE_CURVE ( 2, ( #4407, #50239, #16791, #16412, #22051, #33700, #67545 ),
 .UNSPECIFIED., .F., .F. ) 
 B_SPLINE_CURVE_WITH_KNOTS ( ( 3, 2, 2, 3 ),
 ( 0.7831899741104385582, 0.7902457405827062464, 0.7973015061236232714, 0.8043570860693807223 ),
 .UNSPECIFIED. ) 
 CURVE ( )  GEOMETRIC_REPRESENTATION_ITEM ( )  RATIONAL_B_SPLINE_CURVE ( ( 1.000000000000000000, 0.8660254037844387076, 1.000000000000000000, 0.8660254037844387076, 1.000000000000000000, 0.8660289278579667016, 0.9999929520383388226 ) ) 
 REPRESENTATION_ITEM ( '' )  );
#72264 = DIRECTION ( 'NONE',  ( -1.000000000000000000, 0.000000000000000000, -0.000000000000000000 ) ) ;
#72265 = CARTESIAN_POINT ( 'NONE',  ( 10.00000000000000000, -39.78640506895559525, -66.50666863322042843 ) ) ;
#72266 = DIRECTION ( 'NONE',  ( -0.9966891607226786576, -0.08130631524009861166, 0.000000000000000000 ) ) ;
#72267 = EDGE_LOOP ( 'NONE', ( #73556, #65523, #55923, #7404 ) ) ;
#72268 = CARTESIAN_POINT ( 'NONE',  ( 11.99999999999999822, 65.58780272294129077, -36.73666225445822420 ) ) ;
#72269 = CARTESIAN_POINT ( 'NONE',  ( 11.99999999999999822, -26.02418014898359289, 70.52718814184250107 ) ) ;
#72270 = ADVANCED_BREP_SHAPE_REPRESENTATION ( '', ( #12168, #43395 ), #32718 ) ;
#72271 = CARTESIAN_POINT ( 'NONE',  ( 97.65000000000000568, -208.4700217866474645, 79.57541666666666913 ) ) ;
#72272 = CARTESIAN_POINT ( 'NONE',  ( 0.000000000000000000, 6.903761155837774943, 77.19088730480525840 ) ) ;
#72273 = ORIENTED_EDGE ( 'NONE', *, *, #35256, .T. ) ;
#72274 = CARTESIAN_POINT ( 'NONE',  ( 0.000000000000000000, 0.000000000000000000, 0.000000000000000000 ) ) ;
#72275 = DIRECTION ( 'NONE',  ( 0.000000000000000000, 0.000000000000000000, -1.000000000000000000 ) ) ;
#72276 = ORIENTED_EDGE ( 'NONE', *, *, #40309, .T. ) ;
#72277 = CARTESIAN_POINT ( 'NONE',  ( -2.500000000000015543, -73.00000000000001421, -208.2999999999999261 ) ) ;
#72278 = CARTESIAN_POINT ( 'NONE',  ( 0.000000000000000000, 37.22597642581158084, -5.202137450156524068 ) ) ;
#72279 = ORIENTED_EDGE ( 'NONE', *, *, #2933, .F. ) ;
#72280 = ADVANCED_FACE ( 'NONE', ( #1458 ), #24078, .F. ) ;
#72281 = DIRECTION ( 'NONE',  ( 0.000000000000000000, -0.9945218953682730678, -0.1045284632676570791 ) ) ;
#72282 =( GEOMETRIC_REPRESENTATION_CONTEXT ( 3 ) GLOBAL_UNCERTAINTY_ASSIGNED_CONTEXT ( ( #55730 ) ) GLOBAL_UNIT_ASSIGNED_CONTEXT ( ( #19864, #10443, #57428 ) ) REPRESENTATION_CONTEXT ( 'NONE', 'WORKASPACE' ) );
#72283 = VECTOR ( 'NONE', #42483, 1000.000000000000114 ) ;
#72284 = ADVANCED_FACE ( 'NONE', ( #64565 ), #58546, .F. ) ;
#72285 = ORIENTED_EDGE ( 'NONE', *, *, #33025, .T. ) ;
#72286 = DIRECTION ( 'NONE',  ( -1.000000000000000000, 0.000000000000000000, -0.000000000000000000 ) ) ;
#72287 = EDGE_CURVE ( 'NONE', #61965, #71862, #52166, .T. ) ;
#72288 = AXIS2_PLACEMENT_3D ( 'NONE', #11240, #52199, #68770 ) ;
#72289 = VERTEX_POINT ( 'NONE', #52918 ) ;
#72290 = ORIENTED_EDGE ( 'NONE', *, *, #6160, .T. ) ;
#72292 = ORIENTED_EDGE ( 'NONE', *, *, #42860, .T. ) ;
#72291 = EDGE_CURVE ( 'NONE', #41798, #20819, #19111, .T. ) ;
#72293 = EDGE_LOOP ( 'NONE', ( #71445, #73388, #65322, #5858 ) ) ;
#72294 = CYLINDRICAL_SURFACE ( 'NONE', #10691, 3.299999999999969624 ) ;
#72295 = AXIS2_PLACEMENT_3D ( 'NONE', #68574, #3946, #73816 ) ;
#72296 = ORIENTED_EDGE ( 'NONE', *, *, #1764, .T. ) ;
#72297 = VECTOR ( 'NONE', #61524, 1000.000000000000000 ) ;
#72299 = EDGE_CURVE ( 'NONE', #11546, #23616, #1821, .T. ) ;
#72298 = ORIENTED_EDGE ( 'NONE', *, *, #58415, .F. ) ;
#72300 = CARTESIAN_POINT ( 'NONE',  ( 97.30629616937498838, 91.33154071421968467, 76.20197916753382117 ) ) ;
#72301 = CYLINDRICAL_SURFACE ( 'NONE', #21547, 16.00000000000000000 ) ;
#72302 = FACE_OUTER_BOUND ( 'NONE', #43842, .T. ) ;
#72303 = VERTEX_POINT ( 'NONE', #24708 ) ;
#72304 = EDGE_LOOP ( 'NONE', ( #13410, #15141, #28101, #18247 ) ) ;
#72305 = ORIENTED_EDGE ( 'NONE', *, *, #25902, .T. ) ;
#72306 = CARTESIAN_POINT ( 'NONE',  ( 92.69370383062498320, 91.33154071421968467, 87.04989583420048405 ) ) ;
#72307 = VECTOR ( 'NONE', #8082, 1000.000000000000000 ) ;
#72308 = VERTEX_POINT ( 'NONE', #70547 ) ;
#72309 = CARTESIAN_POINT ( 'NONE',  ( 97.30629616937498838, -209.9999999999999716, 88.69031250086715090 ) ) ;
#72310 = CIRCLE ( 'NONE', #59071, 35.50000000000001421 ) ;
#72311 = DIRECTION ( 'NONE',  ( 0.7533909544171997208, 0.6575728627325956310, 0.000000000000000000 ) ) ;
#72312 = CARTESIAN_POINT ( 'NONE',  ( -2.459674775249762302, -2.163329239379351016E-13, -20.20000000000039009 ) ) ;
#72313 = FACE_OUTER_BOUND ( 'NONE', #68249, .T. ) ;
#72314 = LINE ( 'NONE', #60320, #60538 ) ;
#72315 = CARTESIAN_POINT ( 'NONE',  ( 0.000000000000000000, 0.000000000000000000, 0.000000000000000000 ) ) ;
#72316 = DIRECTION ( 'NONE',  ( -0.02332147558787823344, -0.9997280174009349762, 0.000000000000000000 ) ) ;
#72317 = DIRECTION ( 'NONE',  ( 0.000000000000000000, 0.000000000000000000, 1.000000000000000000 ) ) ;
#72318 = CARTESIAN_POINT ( 'NONE',  ( -94.99999999999997158, -206.9400435732949575, 75.95062500173428077 ) ) ;
#72319 = CARTESIAN_POINT ( 'NONE',  ( -93.84685191531254134, 91.99731107132950569, 87.68489583420048916 ) ) ;
#72320 = ORIENTED_EDGE ( 'NONE', *, *, #40014, .F. ) ;
#72322 = CARTESIAN_POINT ( 'NONE',  ( -93.84685191531254134, 91.99731107132950569, 86.89114583420047211 ) ) ;
#72321 = CARTESIAN_POINT ( 'NONE',  ( 94.99999999999998579, 92.66308142843935514, 87.57906250086713840 ) ) ;
#72323 = ORIENTED_EDGE ( 'NONE', *, *, #45361, .T. ) ;
#72324 = CARTESIAN_POINT ( 'NONE',  ( 11.99999999999999822, 58.39081064771751528, 50.95692526931350841 ) ) ;
#72326 = EDGE_CURVE ( 'NONE', #1061, #366, #35912, .T. ) ;
#72325 = DIRECTION ( 'NONE',  ( 0.000000000000000000, 0.000000000000000000, 1.000000000000000000 ) ) ;
#72327 = DIRECTION ( 'NONE',  ( 0.000000000000000000, 0.000000000000000000, 1.000000000000000000 ) ) ;
#72328 = CARTESIAN_POINT ( 'NONE',  ( 11.99999999999999822, 70.52718814184294160, -26.02418014898236720 ) ) ;
#72329 = CARTESIAN_POINT ( 'NONE',  ( 97.64999999999996305, -209.9999996502043018, 77.69687501385438111 ) ) ;
#72330 = DIRECTION ( 'NONE',  ( -1.000000000000000000, 0.000000000000000000, 0.000000000000000000 ) ) ;
#72331 = CARTESIAN_POINT ( 'NONE',  ( 6.782329983125270800, 10.49999999999999467, 20.00000000000000000 ) ) ;
#72332 = ADVANCED_FACE ( 'NONE', ( #13425 ), #29227, .F. ) ;
#72333 = EDGE_CURVE ( 'NONE', #8374, #36975, #23243, .T. ) ;
#72334 = DIRECTION ( 'NONE',  ( 1.000000000000000000, 0.000000000000000000, 0.000000000000000000 ) ) ;
#72335 = EDGE_LOOP ( 'NONE', ( #23507, #25959 ) ) ;
#72336 = EDGE_LOOP ( 'NONE', ( #36433, #11143, #32451, #46576 ) ) ;
#72337 = CARTESIAN_POINT ( 'NONE',  ( -97.65000000000001990, 91.52997821335253548, 82.96208333333333940 ) ) ;
#72338 = CARTESIAN_POINT ( 'NONE',  ( 10.00000000000000000, 0.000000000000000000, 0.000000000000000000 ) ) ;
#72339 = ADVANCED_FACE ( 'NONE', ( #55129 ), #42378, .F. ) ;
#72340 = CARTESIAN_POINT ( 'NONE',  ( 92.35000000000000853, -209.9999999999999716, 76.03000000000000114 ) ) ;
#72341 = CARTESIAN_POINT ( 'NONE',  ( 11.99999999999999822, 68.27212725128275395, 31.46837873495001503 ) ) ;
#72342 = CARTESIAN_POINT ( 'NONE',  ( 0.000000000000000000, 30.84782396557217865, 21.32104025579125306 ) ) ;
#72343 = CARTESIAN_POINT ( 'NONE',  ( 19.12409105625795291, -101.5943176906707919, 5.500000000000000000 ) ) ;
#72344 = CARTESIAN_POINT ( 'NONE',  ( 97.64999999999999147, 90.00000000000002842, 84.60249999999999204 ) ) ;
#72345 = EDGE_LOOP ( 'NONE', ( #36969, #41500, #18416, #47727 ) ) ;
#72346 = CARTESIAN_POINT ( 'NONE',  ( -93.84685191531254134, 91.99731107132950569, 81.81114583420047381 ) ) ;
#72347 = PRESENTATION_LAYER_ASSIGNMENT (  '', '', ( #63986 ) ) ;
#72348 = CARTESIAN_POINT ( 'NONE',  ( 92.34999999999999432, 90.00003216987884969, 82.45937388908920695 ) ) ;
#72349 = CARTESIAN_POINT ( 'NONE',  ( -96.32500000000001705, 87.70503267997129626, 85.66083333333332916 ) ) ;
#72350 = CIRCLE ( 'NONE', #2791, 31.99999999999998579 ) ;
#72351 = DIRECTION ( 'NONE',  ( 0.9966891607226785466, 0.08130631524009969413, -0.000000000000000000 ) ) ;
#72352 = CARTESIAN_POINT ( 'NONE',  ( 0.000000000000000000, 76.41127070299290835, -12.93880638057231991 ) ) ;
#72353 = DIRECTION ( 'NONE',  ( 0.000000000000000000, 0.000000000000000000, -1.000000000000000000 ) ) ;
#72354 = CARTESIAN_POINT ( 'NONE',  ( -97.64999999999996305, -209.9999999999999716, 86.18999999999999773 ) ) ;
#72355 = LINE ( 'NONE', #60356, #31339 ) ;
#72356 = FACE_OUTER_BOUND ( 'NONE', #43430, .T. ) ;
#72357 = CIRCLE ( 'NONE', #7377, 77.49899999999999523 ) ;
#72358 = AXIS2_PLACEMENT_3D ( 'NONE', #11537, #73207, #16827 ) ;
#72359 = CARTESIAN_POINT ( 'NONE',  ( 96.15314808468748708, 91.99731107132950569, 81.33489583420049485 ) ) ;
#72360 = CARTESIAN_POINT ( 'NONE',  ( -92.69370383062498320, -211.3315407142195852, 83.08114583420048405 ) ) ;
#72361 = FACE_OUTER_BOUND ( 'NONE', #2339, .T. ) ;
#72362 = VERTEX_POINT ( 'NONE', #65317 ) ;
#72363 = CARTESIAN_POINT ( 'NONE',  ( 5.000000000000000000, -21.40280677340398086, 36.13751322684410638 ) ) ;
#72364 = CARTESIAN_POINT ( 'NONE',  ( -92.34999999999999432, -209.9999999999999716, 76.34749999999999659 ) ) ;
#72365 = CYLINDRICAL_SURFACE ( 'NONE', #558, 2.649999999999985700 ) ;
#72366 = VECTOR ( 'NONE', #54144, 1000.000000000000000 ) ;
#72367 = AXIS2_PLACEMENT_3D ( 'NONE', #10956, #33881, #74097 ) ;
#72368 = CARTESIAN_POINT ( 'NONE',  ( 92.69370383062501162, -209.9999999999999716, 83.92781250086714806 ) ) ;
#72369 = VERTEX_POINT ( 'NONE', #13784 ) ;
#72370 = DIRECTION ( 'NONE',  ( -0.000000000000000000, -0.000000000000000000, 1.000000000000000000 ) ) ;
#72371 = VERTEX_POINT ( 'NONE', #48746 ) ;
#72372 = CARTESIAN_POINT ( 'NONE',  ( 10.00000000000000000, 46.54456581323805153, 59.03342792756280488 ) ) ;
#72373 = ORIENTED_EDGE ( 'NONE', *, *, #65767, .T. ) ;
#72374 = CARTESIAN_POINT ( 'NONE',  ( -4.749999999999999112, 0.000000000000000000, 0.000000000000000000 ) ) ;
#72375 = EDGE_CURVE ( 'NONE', #71384, #60009, #66061, .T. ) ;
#72376 = EDGE_CURVE ( 'NONE', #23893, #4586, #64742, .T. ) ;
#72377 = CARTESIAN_POINT ( 'NONE',  ( 93.84685191531251292, -211.9973110713294489, 77.20739583420048291 ) ) ;
#72378 = DIRECTION ( 'NONE',  ( 0.000000000000000000, 0.000000000000000000, 1.000000000000000000 ) ) ;
#72379 = CARTESIAN_POINT ( 'NONE',  ( -10.00000000000000000, 0.000000000000000000, 0.000000000000000000 ) ) ;
#72380 = FACE_OUTER_BOUND ( 'NONE', #42994, .T. ) ;
#72381 = CARTESIAN_POINT ( 'NONE',  ( 97.30629616937498838, 88.66845928578037217, 88.16114583420048234 ) ) ;
#72382 = EDGE_CURVE ( 'NONE', #10842, #9979, #39693, .T. ) ;
#72383 = CARTESIAN_POINT ( 'NONE',  ( 97.64999999999997726, -211.5299782133524502, 82.64458333333331552 ) ) ;
#72384 = ORIENTED_EDGE ( 'NONE', *, *, #53659, .T. ) ;
#72385 = AXIS2_PLACEMENT_3D ( 'NONE', #59191, #59946, #42282 ) ;
#72386 = EDGE_LOOP ( 'NONE', ( #68900, #2394, #56223, #62208 ) ) ;
#72387 = ORIENTED_EDGE ( 'NONE', *, *, #18518, .T. ) ;
#72388 = ORIENTED_EDGE ( 'NONE', *, *, #61397, .F. ) ;
#72389 = DIRECTION ( 'NONE',  ( -1.000000000000000000, -0.000000000000000000, 0.000000000000000000 ) ) ;
#72390 = VECTOR ( 'NONE', #54446, 1000.000000000000000 ) ;
#72391 = CARTESIAN_POINT ( 'NONE',  ( -92.69370383062502583, 88.66845928578038638, 83.71614583420050337 ) ) ;
#72392 = DIRECTION ( 'NONE',  ( -1.000000000000000000, 0.000000000000000000, 0.000000000000000000 ) ) ;
#72393 = DIRECTION ( 'NONE',  ( -1.000000000000000000, 0.000000000000000000, -0.000000000000000000 ) ) ;
#72394 =( BOUNDED_CURVE ( )  B_SPLINE_CURVE ( 2, ( #74007, #27393, #44334, #10113, #5611, #67634, #39068 ),
 .UNSPECIFIED., .F., .F. ) 
 B_SPLINE_CURVE_WITH_KNOTS ( ( 3, 2, 2, 3 ),
 ( 0.5624999999999997780, 0.5694444444444440867, 0.5763888888888885065, 0.5833333333333329263 ),
 .UNSPECIFIED. ) 
 CURVE ( )  GEOMETRIC_REPRESENTATION_ITEM ( )  RATIONAL_B_SPLINE_CURVE ( ( 1.000000000000004219, 0.8660254037844343777, 1.000000000000000000, 0.8660254037844387076, 1.000000000000000000, 0.8660254037844472563, 0.9999999999999914513 ) ) 
 REPRESENTATION_ITEM ( '' )  );
#72395 = PLANE ( 'NONE',  #20378 ) ;
#72396 = EDGE_CURVE ( 'NONE', #15358, #6553, #47941, .T. ) ;
#72397 = CARTESIAN_POINT ( 'NONE',  ( 6.000000000000000000, -80.55351364060578589, -15.33399622253569383 ) ) ;
#72398 = ORIENTED_EDGE ( 'NONE', *, *, #65059, .F. ) ;
#72399 = CARTESIAN_POINT ( 'NONE',  ( -92.34999999999999432, -209.9999999999999716, 85.95187500173430806 ) ) ;
#72400 = ORIENTED_EDGE ( 'NONE', *, *, #66382, .F. ) ;
#72401 = EDGE_CURVE ( 'NONE', #19971, #8287, #20554, .T. ) ;
#72402 = FACE_OUTER_BOUND ( 'NONE', #73002, .T. ) ;
#72403 = ORIENTED_EDGE ( 'NONE', *, *, #66112, .F. ) ;
#72404 = CARTESIAN_POINT ( 'NONE',  ( -93.67500000000003979, 87.70503267997129626, 83.30604166840096525 ) ) ;
#72405 = ORIENTED_EDGE ( 'NONE', *, *, #51546, .F. ) ;
#72406 = CARTESIAN_POINT ( 'NONE',  ( 92.69370383062498320, 91.33154071421968467, 86.57364583420047666 ) ) ;
#72407 = CIRCLE ( 'NONE', #20946, 31.99999999999999645 ) ;
#72408 = CYLINDRICAL_SURFACE ( 'NONE', #3439, 37.49900000000000233 ) ;
#72409 = DIRECTION ( 'NONE',  ( 0.000000000000000000, 0.000000000000000000, 1.000000000000000000 ) ) ;
#72410 = DIRECTION ( 'NONE',  ( 0.000000000000000000, 0.000000000000000000, 1.000000000000000000 ) ) ;
#72411 = DIRECTION ( 'NONE',  ( -0.000000000000000000, -0.000000000000000000, -1.000000000000000000 ) ) ;
#72412 = CARTESIAN_POINT ( 'NONE',  ( 10.00000000000000000, 0.000000000000000000, 0.000000000000000000 ) ) ;
#72413 = ORIENTED_EDGE ( 'NONE', *, *, #30270, .F. ) ;
#72414 = CARTESIAN_POINT ( 'NONE',  ( 92.35000000000000853, -209.9999999999999716, 77.93499999999998806 ) ) ;
#72415 = AXIS2_PLACEMENT_3D ( 'NONE', #24368, #40930, #70207 ) ;
#72416 = ADVANCED_FACE ( 'NONE', ( #14158 ), #59669, .T. ) ;
#72418 = EDGE_CURVE ( 'NONE', #5982, #45341, #9266, .T. ) ;
#72417 = VECTOR ( 'NONE', #14645, 1000.000000000000000 ) ;
#72419 = CARTESIAN_POINT ( 'NONE',  ( -43.60332556124591008, -123.0000000000000142, -2.500000000000000000 ) ) ;
#72420 = EDGE_LOOP ( 'NONE', ( #69111, #46586, #7225, #26064 ) ) ;
#72421 = ORIENTED_EDGE ( 'NONE', *, *, #15248, .T. ) ;
#72422 = DIRECTION ( 'NONE',  ( -1.000000000000000000, -0.000000000000000000, -0.000000000000000000 ) ) ;
#72423 = CARTESIAN_POINT ( 'NONE',  ( 12.00000000000000000, 24.81905959214260804, -9.408202855044827118 ) ) ;
#72424 = DIRECTION ( 'NONE',  ( -0.000000000000000000, -0.000000000000000000, 1.000000000000000000 ) ) ;
#72425 = CARTESIAN_POINT ( 'NONE',  ( -93.84685191531248449, -208.0026889286704943, 85.77989583420048803 ) ) ;
#72426 = ORIENTED_EDGE ( 'NONE', *, *, #27512, .T. ) ;
#72427 = CARTESIAN_POINT ( 'NONE',  ( 12.69589495141918611, -96.69089767102708777, -2.500000000000000444 ) ) ;
#72428 = ORIENTED_EDGE ( 'NONE', *, *, #71716, .F. ) ;
#72429 = DIRECTION ( 'NONE',  ( 0.000000000000000000, 0.000000000000000000, 1.000000000000000000 ) ) ;
#72430 = CARTESIAN_POINT ( 'NONE',  ( 97.64999999999324132, 90.00000598221777182, 82.14187520865721126 ) ) ;
#72431 = CARTESIAN_POINT ( 'NONE',  ( 92.34999999999999432, -210.0000348885106405, 83.09437620840748195 ) ) ;
#72432 = CARTESIAN_POINT ( 'NONE',  ( 92.69370383062498320, 88.66845928578035796, 76.99572916753380980 ) ) ;
#72433 = DIRECTION ( 'NONE',  ( -1.000000000000000000, 0.000000000000000000, 0.000000000000000000 ) ) ;
#72434 = LINE ( 'NONE', #8559, #50615 ) ;
#72435 = CARTESIAN_POINT ( 'NONE',  ( 0.000000000000000000, -69.42325613327415113, -34.44570377933673200 ) ) ;
#72436 = CARTESIAN_POINT ( 'NONE',  ( 0.000000000000000000, 0.000000000000000000, 0.000000000000000000 ) ) ;
#72437 = DIRECTION ( 'NONE',  ( 1.000000000000000000, 0.000000000000000000, 0.000000000000000000 ) ) ;
#72438 = CARTESIAN_POINT ( 'NONE',  ( -93.67499999999998295, -212.2949673200287179, 87.03666666666666174 ) ) ;
#72439 = APPLICATION_CONTEXT ( 'automotive_design' ) ;
#72440 = CARTESIAN_POINT ( 'NONE',  ( 0.000000000000000000, 0.000000000000000000, 0.000000000000000000 ) ) ;
#72441 = PRODUCT_DEFINITION_CONTEXT ( 'detailed design', #56092, 'design' ) ;
#72442 = ORIENTED_EDGE ( 'NONE', *, *, #9864, .T. ) ;
#72443 = CARTESIAN_POINT ( 'NONE',  ( 93.67499999999998295, 92.29496732002878900, 89.25916666666667254 ) ) ;
#72444 = EDGE_LOOP ( 'NONE', ( #62888, #28130, #45949, #58199 ) ) ;
#72445 = CARTESIAN_POINT ( 'NONE',  ( -96.15314808468751551, 88.00268892867056536, 82.76364583420047438 ) ) ;
#72446 = CYLINDRICAL_SURFACE ( 'NONE', #49165, 82.00000000000000000 ) ;
#72447 = AXIS2_PLACEMENT_3D ( 'NONE', #9972, #38927, #9611 ) ;
#72448 = DIRECTION ( 'NONE',  ( -1.000000000000000000, 0.000000000000000000, 0.000000000000000000 ) ) ;
#72449 = EDGE_CURVE ( 'NONE', #61705, #66826, #32477, .T. ) ;
#72450 = ORIENTED_EDGE ( 'NONE', *, *, #66488, .F. ) ;
#72451 = AXIS2_PLACEMENT_3D ( 'NONE', #9419, #33085, #4177 ) ;
#72452 = CARTESIAN_POINT ( 'NONE',  ( -97.64999999993855795, 90.00001182178863246, 76.10900611559313234 ) ) ;
#72453 = CARTESIAN_POINT ( 'NONE',  ( 96.32499999999997442, 92.29496732002878900, 85.34333333333333371 ) ) ;
#72454 = CARTESIAN_POINT ( 'NONE',  ( 10.00000000000000000, -41.19522573413687638, -65.64334221924953283 ) ) ;
#72455 = ADVANCED_FACE ( 'NONE', ( #15276 ), #66428, .F. ) ;
#72456 = DIRECTION ( 'NONE',  ( -1.000000000000000000, -0.000000000000000000, -0.000000000000000000 ) ) ;
#72457 = AXIS2_PLACEMENT_3D ( 'NONE', #23541, #35190, #36292 ) ;
#72458 = CARTESIAN_POINT ( 'NONE',  ( 97.30629616937498838, -211.3315407142195852, 77.36614583420048064 ) ) ;
#72459 = ADVANCED_FACE ( 'NONE', ( #54393 ), #54762, .T. ) ;
#72460 = ORIENTED_EDGE ( 'NONE', *, *, #8347, .T. ) ;
#72461 = ORIENTED_EDGE ( 'NONE', *, *, #30308, .F. ) ;
#72462 = EDGE_CURVE ( 'NONE', #24570, #278, #37852, .T. ) ;
#72463 = FACE_OUTER_BOUND ( 'NONE', #46980, .T. ) ;
#72464 = CARTESIAN_POINT ( 'NONE',  ( -2.499999999999970690, 73.00000000000001421, -255.0000000000000000 ) ) ;
#72465 = CARTESIAN_POINT ( 'NONE',  ( 0.000000000000000000, -36.72794159290288718, 65.59268652807197952 ) ) ;
#72466 = CYLINDRICAL_SURFACE ( 'NONE', #37448, 12.49999999999999822 ) ;
#72467 = ADVANCED_FACE ( 'NONE', ( #72043 ), #19797, .F. ) ;
#72468 = DIRECTION ( 'NONE',  ( -1.000000000000000000, -0.000000000000000000, 0.000000000000000000 ) ) ;
#72469 = CARTESIAN_POINT ( 'NONE',  ( 95.00000000000000000, -212.6630814284392557, 77.89531250086714920 ) ) ;
#72470 = AXIS2_PLACEMENT_3D ( 'NONE', #13956, #42191, #59110 ) ;
#72471 = ORIENTED_EDGE ( 'NONE', *, *, #48346, .T. ) ;
#72472 = CARTESIAN_POINT ( 'NONE',  ( 0.000000000000000000, -120.0000000000000000, 102.9091629284897493 ) ) ;
#72473 = ORIENTED_EDGE ( 'NONE', *, *, #2882, .F. ) ;
#72474 = ORIENTED_EDGE ( 'NONE', *, *, #751, .T. ) ;
#72475 = CARTESIAN_POINT ( 'NONE',  ( 11.99999999999999822, 75.16055320797057959, -18.89407956138179046 ) ) ;
#72476 =( LENGTH_UNIT ( ) NAMED_UNIT ( * ) SI_UNIT ( .MILLI., .METRE. ) );
#72477 = DIRECTION ( 'NONE',  ( -1.000000000000000000, -0.000000000000000000, 0.000000000000000000 ) ) ;
#72478 = ORIENTED_EDGE ( 'NONE', *, *, #28494, .T. ) ;
#72479 = CARTESIAN_POINT ( 'NONE',  ( 0.6180191030787338669, -93.50720753887522108, 2.500000000000000000 ) ) ;
#72480 = CARTESIAN_POINT ( 'NONE',  ( 97.64999999999997726, -208.4700217866474645, 80.92479166840098515 ) ) ;
#72481 = CARTESIAN_POINT ( 'NONE',  ( 92.34999999999999432, 91.52997821335252127, 84.86708333333334053 ) ) ;
#72482 = EDGE_CURVE ( 'NONE', #50011, #40286, #51702, .T. ) ;
#72483 = ORIENTED_EDGE ( 'NONE', *, *, #25415, .T. ) ;
#72484 = CARTESIAN_POINT ( 'NONE',  ( -2.499999999999974243, 62.44997998398397954, -270.0000000000000000 ) ) ;
#72485 = EDGE_CURVE ( 'NONE', #21360, #70060, #61156, .T. ) ;
#72486 = CARTESIAN_POINT ( 'NONE',  ( 23.11608002360578240, -124.4885236261218182, 5.500000000000000000 ) ) ;
#72487 = AXIS2_PLACEMENT_3D ( 'NONE', #5603, #51817, #51437 ) ;
#72488 = ORIENTED_EDGE ( 'NONE', *, *, #42306, .F. ) ;
#72489 = CYLINDRICAL_SURFACE ( 'NONE', #16370, 12.50000000000000000 ) ;
#72490 =( BOUNDED_CURVE ( )  B_SPLINE_CURVE ( 2, ( #51372, #51748, #40465, #295, #5541, #63059, #22823 ),
 .UNSPECIFIED., .F., .F. ) 
 B_SPLINE_CURVE_WITH_KNOTS ( ( 3, 2, 2, 3 ),
 ( 0.4791666666666668517, 0.4861111111111112160, 0.4930555555555556357, 0.5000000000000000000 ),
 .UNSPECIFIED. ) 
 CURVE ( )  GEOMETRIC_REPRESENTATION_ITEM ( )  RATIONAL_B_SPLINE_CURVE ( ( 0.9999999999999967804, 0.8660254037844419273, 1.000000000000000000, 0.8660254037844387076, 1.000000000000000000, 0.8660254037844387076, 1.000000000000000000 ) ) 
 REPRESENTATION_ITEM ( '' )  );
#72491 = CARTESIAN_POINT ( 'NONE',  ( -92.69370383062505425, 88.66845928578038638, 83.71614583420048916 ) ) ;
#72492 = CARTESIAN_POINT ( 'NONE',  ( 92.69370383062498320, 91.33154071421968467, 83.23989583420046756 ) ) ;
#72493 = EDGE_LOOP ( 'NONE', ( #16737, #71748, #73990, #5657 ) ) ;
#72494 = CARTESIAN_POINT ( 'NONE',  ( -21.67772167707813935, -110.8034581014852762, 5.500000000000000000 ) ) ;
#72495 = VERTEX_POINT ( 'NONE', #49117 ) ;
#72496 = DIRECTION ( 'NONE',  ( 1.000000000000000000, 0.000000000000000000, 0.000000000000000000 ) ) ;
#72497 = AXIS2_PLACEMENT_3D ( 'NONE', #51131, #50381, #4925 ) ;
#72498 = ORIENTED_EDGE ( 'NONE', *, *, #65899, .T. ) ;
#72499 = ORIENTED_EDGE ( 'NONE', *, *, #4043, .T. ) ;
#72500 = CARTESIAN_POINT ( 'NONE',  ( 96.32499999999998863, 87.70503267997126784, 80.05166666666666231 ) ) ;
#72501 = ORIENTED_EDGE ( 'NONE', *, *, #46112, .F. ) ;
#72502 = DIRECTION ( 'NONE',  ( -0.000000000000000000, -0.000000000000000000, 1.000000000000000000 ) ) ;
#72503 = VECTOR ( 'NONE', #46979, 1000.000000000000000 ) ;
#72504 = CARTESIAN_POINT ( 'NONE',  ( 93.67499999999999716, 87.70503267997126784, 88.28020833506764120 ) ) ;
#72505 = VERTEX_POINT ( 'NONE', #2190 ) ;
#72506 = FACE_OUTER_BOUND ( 'NONE', #4215, .T. ) ;
#72507 = CARTESIAN_POINT ( 'NONE',  ( -92.69370383062498320, -208.6684592857803011, 80.48822916753383083 ) ) ;
#72508 = EDGE_LOOP ( 'NONE', ( #864, #33364, #40243, #59686 ) ) ;
#72509 = CIRCLE ( 'NONE', #34096, 31.99999999999998934 ) ;
#72510 = DIRECTION ( 'NONE',  ( 0.2867529058022035837, -0.9580045777625452175, 0.000000000000000000 ) ) ;
#72511 = DIRECTION ( 'NONE',  ( -1.000000000000000000, 0.000000000000000000, 0.000000000000000000 ) ) ;
#72512 = DIRECTION ( 'NONE',  ( -1.000000000000000000, -0.000000000000000000, -0.000000000000000000 ) ) ;
#72513 = DIRECTION ( 'NONE',  ( 0.000000000000000000, 0.3090169943749482839, -0.9510565162951533091 ) ) ;
#72514 = CARTESIAN_POINT ( 'NONE',  ( 10.00000000000000000, -37.58145647212455032, 0.6853352020789044152 ) ) ;
#72515 = AXIS2_PLACEMENT_3D ( 'NONE', #7908, #70673, #35727 ) ;
#72516 = CARTESIAN_POINT ( 'NONE',  ( 0.000000000000000000, 0.000000000000000000, -4.400000000000001243 ) ) ;
#72517 = CARTESIAN_POINT ( 'NONE',  ( 94.99999999999998579, 92.66308142843932671, 88.84906250086713442 ) ) ;
#72518 = DIRECTION ( 'NONE',  ( -1.000000000000000000, 0.000000000000000000, 0.000000000000000000 ) ) ;
#72519 = DIRECTION ( 'NONE',  ( -1.000000000000000000, -0.000000000000000000, 0.000000000000000000 ) ) ;
#72520 = DIRECTION ( 'NONE',  ( 0.8225049752423776450, 0.5687579148473764779, 0.000000000000000000 ) ) ;
#72521 = CARTESIAN_POINT ( 'NONE',  ( -3.000000000000000000, -23.29833615347109443, 3.418703333116492438 ) ) ;
#72522 = CARTESIAN_POINT ( 'NONE',  ( 0.000000000000000000, 10.41901085202078292, 40.68715046381932865 ) ) ;
#72523 = DIRECTION ( 'NONE',  ( 0.000000000000000000, -0.7431448254773938000, -0.6691306063588585706 ) ) ;
#72524 = DIRECTION ( 'NONE',  ( 1.000000000000000000, 0.000000000000000000, 0.000000000000000000 ) ) ;
#72525 = LINE ( 'NONE', #38708, #60465 ) ;
#72526 = EDGE_CURVE ( 'NONE', #13949, #34086, #61155, .T. ) ;
#72527 = AXIS2_PLACEMENT_3D ( 'NONE', #163, #63278, #45984 ) ;
#72528 = CARTESIAN_POINT ( 'NONE',  ( 0.000000000000000000, 0.000000000000000000, 0.000000000000000000 ) ) ;
#72529 = DIRECTION ( 'NONE',  ( -1.000000000000000000, -0.000000000000000000, 0.000000000000000000 ) ) ;
#72530 = CARTESIAN_POINT ( 'NONE',  ( -93.67499999999998295, -207.7050326799711968, 84.70833333333332860 ) ) ;
#72531 = EDGE_CURVE ( 'NONE', #39794, #36331, #48378, .T. ) ;
#72532 = ADVANCED_FACE ( 'NONE', ( #62653 ), #44977, .T. ) ;
#72533 = FACE_OUTER_BOUND ( 'NONE', #53261, .T. ) ;
#72534 = VECTOR ( 'NONE', #32193, 1000.000000000000000 ) ;
#72535 = ORIENTED_EDGE ( 'NONE', *, *, #29206, .T. ) ;
#72536 = CARTESIAN_POINT ( 'NONE',  ( 0.000000000000000000, 0.000000000000000000, 0.000000000000000000 ) ) ;
#72537 = CYLINDRICAL_SURFACE ( 'NONE', #58684, 37.49900000000000233 ) ;
#72538 = EDGE_CURVE ( 'NONE', #36312, #57978, #67903, .T. ) ;
#72539 = LINE ( 'NONE', #38723, #14984 ) ;
#72540 = VECTOR ( 'NONE', #28471, 1000.000000000000000 ) ;
#72541 = ORIENTED_EDGE ( 'NONE', *, *, #8139, .T. ) ;
#72542 = EDGE_LOOP ( 'NONE', ( #52715, #23802, #27083, #17542 ) ) ;
#72543 = CARTESIAN_POINT ( 'NONE',  ( 10.00000000000000000, 10.96151621346540317, -35.95386929396244113 ) ) ;
#72544 = DIRECTION ( 'NONE',  ( 1.000000000000000000, 0.000000000000000000, 0.000000000000000000 ) ) ;
#72545 = ORIENTED_EDGE ( 'NONE', *, *, #47228, .F. ) ;
#72546 = CIRCLE ( 'NONE', #7747, 23.50000000000000355 ) ;
#72547 = CARTESIAN_POINT ( 'NONE',  ( 93.84685191531251292, -211.9973110713294489, 80.22364583420046813 ) ) ;
#72548 = CARTESIAN_POINT ( 'NONE',  ( 97.30629616937498838, -211.3315407142195852, 84.35114583420050849 ) ) ;
#72549 = EDGE_CURVE ( 'NONE', #15281, #48178, #44611, .T. ) ;
#72550 = ORIENTED_EDGE ( 'NONE', *, *, #42673, .F. ) ;
#72551 = CARTESIAN_POINT ( 'NONE',  ( 93.84685191531251292, -211.9973110713294489, 84.82739583420048746 ) ) ;
#72552 = ORIENTED_EDGE ( 'NONE', *, *, #27655, .F. ) ;
#72553 = DIRECTION ( 'NONE',  ( -1.000000000000000000, 0.000000000000000000, -0.000000000000000000 ) ) ;
#72554 = VERTEX_POINT ( 'NONE', #10756 ) ;
#72555 = CIRCLE ( 'NONE', #2962, 3.250000000000001332 ) ;
#72556 = CARTESIAN_POINT ( 'NONE',  ( -92.69370383062504004, 90.00000000000004263, 76.78406250086715090 ) ) ;
#72557 = ORIENTED_EDGE ( 'NONE', *, *, #54555, .F. ) ;
#72558 = VERTEX_POINT ( 'NONE', #4770 ) ;
#72559 = CARTESIAN_POINT ( 'NONE',  ( 0.000000000000000000, 70.52718814184294160, -26.02418014898236720 ) ) ;
#72560 = AXIS2_PLACEMENT_3D ( 'NONE', #66627, #15110, #38049 ) ;
#72561 = ORIENTED_EDGE ( 'NONE', *, *, #58749, .T. ) ;
#72562 = FACE_OUTER_BOUND ( 'NONE', #22242, .T. ) ;
#72563 = DIRECTION ( 'NONE',  ( -1.000000000000000000, 0.000000000000000000, -0.000000000000000000 ) ) ;
#72564 = ADVANCED_FACE ( 'NONE', ( #27673 ), #27285, .T. ) ;
#72565 = ORIENTED_EDGE ( 'NONE', *, *, #55237, .T. ) ;
#72566 = CARTESIAN_POINT ( 'NONE',  ( 10.00000000000000000, -31.52238457039619490, 27.75498641678731104 ) ) ;
#72567 = EDGE_CURVE ( 'NONE', #64357, #47972, #72768, .T. ) ;
#72568 = CIRCLE ( 'NONE', #6541, 42.00000000000000000 ) ;
#72569 = ORIENTED_EDGE ( 'NONE', *, *, #23448, .T. ) ;
#72570 = LINE ( 'NONE', #67695, #49243 ) ;
#72571 = EDGE_CURVE ( 'NONE', #29346, #10762, #39571, .T. ) ;
#72572 = ORIENTED_EDGE ( 'NONE', *, *, #3350, .T. ) ;
#72573 = AXIS2_PLACEMENT_3D ( 'NONE', #59668, #59294, #52530 ) ;
#72574 = ORIENTED_EDGE ( 'NONE', *, *, #64209, .F. ) ;
#72575 = ORIENTED_EDGE ( 'NONE', *, *, #21049, .T. ) ;
#72576 = CARTESIAN_POINT ( 'NONE',  ( 97.30629616937498838, -209.9999999999999716, 74.72031250086713783 ) ) ;
#72577 = DIRECTION ( 'NONE',  ( -1.000000000000000000, 3.061616997868382648E-16, 0.000000000000000000 ) ) ;
#72578 = ORIENTED_EDGE ( 'NONE', *, *, #25199, .T. ) ;
#72579 = ORIENTED_EDGE ( 'NONE', *, *, #73829, .F. ) ;
#72580 = ORIENTED_EDGE ( 'NONE', *, *, #33635, .F. ) ;
#72581 = CARTESIAN_POINT ( 'NONE',  ( -97.64999999999992042, -211.5299782133524786, 84.33791666666667197 ) ) ;
#72582 = DIRECTION ( 'NONE',  ( -1.000000000000000000, -0.000000000000000000, -0.000000000000000000 ) ) ;
#72583 = CARTESIAN_POINT ( 'NONE',  ( -96.32500000000001705, 92.29496732002878900, 89.89416666666666345 ) ) ;
#72584 = ORIENTED_EDGE ( 'NONE', *, *, #2355, .F. ) ;
#72585 = CARTESIAN_POINT ( 'NONE',  ( 96.15314808468748708, 91.99731107132950569, 78.00114583420048575 ) ) ;
#72586 = ORIENTED_EDGE ( 'NONE', *, *, #11691, .F. ) ;
#72587 = CARTESIAN_POINT ( 'NONE',  ( -97.30629616937497417, -208.6684592857803011, 89.58989583420047609 ) ) ;
#72588 = CARTESIAN_POINT ( 'NONE',  ( 0.9154378789997317245, -5.244974386029391589, -1.156968425231173381 ) ) ;
#72589 = DIRECTION ( 'NONE',  ( 0.000000000000000000, 1.000000000000000000, 3.491481338843133750E-15 ) ) ;
#72590 = CARTESIAN_POINT ( 'NONE',  ( 10.00000000000000000, 73.44644590900061587, 24.73286445877730699 ) ) ;
#72591 = CARTESIAN_POINT ( 'NONE',  ( -96.15314808468747287, -208.0026889286704943, 79.37697916753380412 ) ) ;
#72592 = CARTESIAN_POINT ( 'NONE',  ( 0.000000000000000000, -81.50828551894220197, -8.966570791701586884 ) ) ;
#72593 = LINE ( 'NONE', #71121, #40342 ) ;
#72594 = DIRECTION ( 'NONE',  ( 0.000000000000000000, 0.8090169943749486725, -0.5877852522924713607 ) ) ;
#72595 = ORIENTED_EDGE ( 'NONE', *, *, #48346, .F. ) ;
#72596 = AXIS2_PLACEMENT_3D ( 'NONE', #54377, #65301, #26161 ) ;
#72597 = VERTEX_POINT ( 'NONE', #10378 ) ;
#72598 = DIRECTION ( 'NONE',  ( 0.000000000000000000, 0.9510565162951521989, 0.3090169943749515591 ) ) ;
#72599 = CARTESIAN_POINT ( 'NONE',  ( -97.64999999999984936, -211.5299782133525071, 88.78291666666667936 ) ) ;
#72600 = CARTESIAN_POINT ( 'NONE',  ( 97.64999999999999147, 89.99999990163419739, 80.23687499810812085 ) ) ;
#72601 = CARTESIAN_POINT ( 'NONE',  ( -97.30629616937501680, 88.66845928578038638, 82.71072916753379900 ) ) ;
#72602 = CARTESIAN_POINT ( 'NONE',  ( 15.00000000000000000, 14.60985201121703980, -18.46759930825707841 ) ) ;
#72603 = DIRECTION ( 'NONE',  ( 0.000000000000000000, 0.000000000000000000, 1.000000000000000000 ) ) ;
#72604 = CIRCLE ( 'NONE', #19809, 82.00000000000000000 ) ;
#72605 = ORIENTED_EDGE ( 'NONE', *, *, #60467, .F. ) ;
#72606 = AXIS2_PLACEMENT_3D ( 'NONE', #16191, #33469, #56428 ) ;
#72607 = CARTESIAN_POINT ( 'NONE',  ( 11.99999999999999822, -50.95692526931287603, -58.39081064771804819 ) ) ;
#72608 = EDGE_CURVE ( 'NONE', #58924, #22889, #4769, .T. ) ;
#72610 = CARTESIAN_POINT ( 'NONE',  ( 2.184357737007946383E-12, -120.0000000000000000, -48.99999999999997158 ) ) ;
#72609 = CIRCLE ( 'NONE', #45016, 31.99999999999998579 ) ;
#72611 = CARTESIAN_POINT ( 'NONE',  ( 0.000000000000000000, -44.88180994100329713, -63.18004540533077318 ) ) ;
#72612 = DIRECTION ( 'NONE',  ( -1.000000000000000000, 0.000000000000000000, 0.000000000000000000 ) ) ;
#72613 = DIRECTION ( 'NONE',  ( 0.000000000000000000, 0.9510565162951546414, -0.3090169943749446202 ) ) ;
#72614 = CARTESIAN_POINT ( 'NONE',  ( -96.15314808468745866, -211.9973110713294489, 84.19239583420049655 ) ) ;
#72615 = EDGE_CURVE ( 'NONE', #53345, #37277, #33541, .T. ) ;
#72616 = AXIS2_PLACEMENT_3D ( 'NONE', #54410, #71685, #13801 ) ;
#72617 = EDGE_CURVE ( 'NONE', #40541, #23489, #28783, .T. ) ;
#72618 = PLANE ( 'NONE',  #48461 ) ;
#72619 = ORIENTED_EDGE ( 'NONE', *, *, #13473, .F. ) ;
#72620 = CARTESIAN_POINT ( 'NONE',  ( 5.000000000000000000, 41.91543099594818500, 2.663952781846291362 ) ) ;
#72621 = AXIS2_PLACEMENT_3D ( 'NONE', #8537, #66427, #15274 ) ;
#72622 = CARTESIAN_POINT ( 'NONE',  ( 11.99999999999999822, 0.000000000000000000, 0.000000000000000000 ) ) ;
#72623 = ORIENTED_EDGE ( 'NONE', *, *, #24354, .F. ) ;
#72624 = EDGE_CURVE ( 'NONE', #26970, #32269, #32357, .T. ) ;
#72625 = DIRECTION ( 'NONE',  ( -1.000000000000000000, 0.000000000000000000, 0.000000000000000000 ) ) ;
#72626 = FACE_OUTER_BOUND ( 'NONE', #3117, .T. ) ;
#72627 = CARTESIAN_POINT ( 'NONE',  ( 11.99999999999999822, -17.28742895386031719, -75.54627589209962935 ) ) ;
#72628 = AXIS2_PLACEMENT_3D ( 'NONE', #1389, #35914, #58865 ) ;
#72629 = DIRECTION ( 'NONE',  ( 0.000000000000000000, 0.000000000000000000, 1.000000000000000000 ) ) ;
#72630 = ORIENTED_EDGE ( 'NONE', *, *, #73314, .F. ) ;
#72631 = CARTESIAN_POINT ( 'NONE',  ( 10.00000000000000000, -37.16516213103280108, 4.992566952384862589 ) ) ;
#72632 = LINE ( 'NONE', #31686, #42707 ) ;
#72633 = VERTEX_POINT ( 'NONE', #38962 ) ;
#72634 = CIRCLE ( 'NONE', #10236, 77.49899999999999523 ) ;
#72635 = CARTESIAN_POINT ( 'NONE',  ( 10.00000000000000000, 36.13751322684419165, 21.40280677340384230 ) ) ;
#72636 = CARTESIAN_POINT ( 'NONE',  ( -92.35000000000000853, 91.52997821335250705, 77.67041666666666799 ) ) ;
#72637 = ADVANCED_FACE ( 'NONE', ( #38589 ), #34052, .T. ) ;
#72638 = ORIENTED_EDGE ( 'NONE', *, *, #61794, .F. ) ;
#72639 = CARTESIAN_POINT ( 'NONE',  ( 1.029419772574596825, -118.9089936151275140, 2.500000000000000000 ) ) ;
#72640 = ORIENTED_EDGE ( 'NONE', *, *, #49841, .F. ) ;
#72641 = DIRECTION ( 'NONE',  ( 0.000000000000000000, -0.000000000000000000, 1.000000000000000000 ) ) ;
#72642 = CIRCLE ( 'NONE', #40265, 0.2500000000000002220 ) ;
#72643 = VERTEX_POINT ( 'NONE', #22407 ) ;
#72644 = EDGE_LOOP ( 'NONE', ( #44616, #13342, #48170, #42255 ) ) ;
#72645 = ORIENTED_EDGE ( 'NONE', *, *, #4377, .F. ) ;
#72646 = DIRECTION ( 'NONE',  ( 0.000000000000000000, 0.000000000000000000, 1.000000000000000000 ) ) ;
#72647 = EDGE_CURVE ( 'NONE', #51903, #44494, #20882, .T. ) ;
#72648 = ORIENTED_EDGE ( 'NONE', *, *, #10467, .T. ) ;
#72649 = EDGE_CURVE ( 'NONE', #51709, #5557, #4388, .T. ) ;
#72650 = ORIENTED_EDGE ( 'NONE', *, *, #57597, .T. ) ;
#72651 = CARTESIAN_POINT ( 'NONE',  ( 92.69370383062498320, 90.00000000000002842, 75.83156250086716454 ) ) ;
#72652 = VECTOR ( 'NONE', #49858, 1000.000000000000000 ) ;
#72653 = CARTESIAN_POINT ( 'NONE',  ( 10.00000000000000000, 0.000000000000000000, 0.000000000000000000 ) ) ;
#72655 = LINE ( 'NONE', #32807, #59721 ) ;
#72654 = AXIS2_PLACEMENT_3D ( 'NONE', #49848, #50972, #73521 ) ;
#72656 = ORIENTED_EDGE ( 'NONE', *, *, #29030, .T. ) ;
#72657 = ORIENTED_EDGE ( 'NONE', *, *, #52444, .T. ) ;
#72658 = VERTEX_POINT ( 'NONE', #50217 ) ;
#72659 = CARTESIAN_POINT ( 'NONE',  ( 97.30629616937498838, 91.33154071421968467, 88.10822916753380696 ) ) ;
#72660 = VERTEX_POINT ( 'NONE', #32560 ) ;
#72661 = CARTESIAN_POINT ( 'NONE',  ( 97.30629616937498838, -211.3315407142195852, 85.46239583420047836 ) ) ;
#72662 = APPLICATION_PROTOCOL_DEFINITION ( 'draft international standard', 'automotive_design', 1998, #61373 ) ;
#72663 = CARTESIAN_POINT ( 'NONE',  ( 10.00000000000000000, 36.73666225445988687, -65.58780272294035285 ) ) ;
#72664 = CARTESIAN_POINT ( 'NONE',  ( -97.65000000000001990, 91.52997821335253548, 77.32645833506762756 ) ) ;
#72665 = DIRECTION ( 'NONE',  ( -1.000000000000000000, 0.000000000000000000, -0.000000000000000000 ) ) ;
#72666 = CARTESIAN_POINT ( 'NONE',  ( 15.00000000000000000, 23.49999999999999645, 1.499999999999995337 ) ) ;
#72667 = CIRCLE ( 'NONE', #67928, 12.50000000000000000 ) ;
#72668 = FACE_OUTER_BOUND ( 'NONE', #57976, .T. ) ;
#72669 = DIRECTION ( 'NONE',  ( -1.000000000000000000, -0.000000000000000000, -0.000000000000000000 ) ) ;
#72670 = CARTESIAN_POINT ( 'NONE',  ( -93.84685191531247028, -211.9973110713294489, 88.58447916753381435 ) ) ;
#72671 = CARTESIAN_POINT ( 'NONE',  ( -97.30629616937501680, 90.00000000000004263, 89.16656250086715829 ) ) ;
#72672 = ORIENTED_EDGE ( 'NONE', *, *, #28192, .F. ) ;
#72674 = CARTESIAN_POINT ( 'NONE',  ( -93.84685191531254134, 91.99731107132950569, 87.52614583420047722 ) ) ;
#72673 = CARTESIAN_POINT ( 'NONE',  ( 97.30629616937498838, 91.33154071421968467, 88.10822916753380696 ) ) ;
#72675 = ORIENTED_EDGE ( 'NONE', *, *, #10033, .T. ) ;
#72676 = CARTESIAN_POINT ( 'NONE',  ( 96.32499999999998863, -212.2949673200287179, 84.57604166840096127 ) ) ;
#72677 = DIRECTION ( 'NONE',  ( -1.000000000000000000, -0.000000000000000000, 0.000000000000000000 ) ) ;
#72678 = DIRECTION ( 'NONE',  ( 0.000000000000000000, -0.3090169943749349057, -0.9510565162951577500 ) ) ;
#72679 = CARTESIAN_POINT ( 'NONE',  ( 94.99999999999998579, 93.05995642670504253, 82.30062500173427509 ) ) ;
#72680 = AXIS2_PLACEMENT_3D ( 'NONE', #43034, #14447, #54313 ) ;
#72681 = CARTESIAN_POINT ( 'NONE',  ( -96.15314808468747287, -208.0026889286704943, 88.90197916753380980 ) ) ;
#72682 = LINE ( 'NONE', #50883, #60205 ) ;
#72683 = LINE ( 'NONE', #60703, #73219 ) ;
#72684 = ORIENTED_EDGE ( 'NONE', *, *, #9518, .T. ) ;
#72685 = VECTOR ( 'NONE', #43731, 1000.000000000000000 ) ;
#72686 = ORIENTED_EDGE ( 'NONE', *, *, #1588, .F. ) ;
#72687 = CARTESIAN_POINT ( 'NONE',  ( -92.35000000000003695, 90.00000000000004263, 82.06250000000000000 ) ) ;
#72688 = CARTESIAN_POINT ( 'NONE',  ( 11.99999999999999822, -26.01480285779785362, -70.53064760720343429 ) ) ;
#72689 = DIRECTION ( 'NONE',  ( 0.000000000000000000, 0.000000000000000000, 1.000000000000000000 ) ) ;
#72690 = CYLINDRICAL_SURFACE ( 'NONE', #72295, 12.49999999999999645 ) ;
#72691 = LINE ( 'NONE', #15575, #62797 ) ;
#72692 = CARTESIAN_POINT ( 'NONE',  ( -97.64999999993855795, 90.00001182178863246, 76.10900611559313234 ) ) ;
#72693 =( BOUNDED_CURVE ( )  B_SPLINE_CURVE ( 2, ( #52156, #57438, #40512, #63457, #16472, #40147, #51794, #67604, #28114, #67977, #61972 ),
 .UNSPECIFIED., .F., .F. ) 
 B_SPLINE_CURVE_WITH_KNOTS ( ( 3, 2, 2, 2, 2, 3 ),
 ( 0.4233457466706606609, 0.4233459324550212788, 0.4304016979959381928, 0.4374574635368551623, 0.4445132290777720763, 0.4445132602993024373 ),
 .UNSPECIFIED. ) 
 CURVE ( )  GEOMETRIC_REPRESENTATION_ITEM ( )  RATIONAL_B_SPLINE_CURVE ( ( 0.9999929448536319931, 0.9999964723339295203, 1.000000000000000000, 0.8660254037844387076, 1.000000000000000000, 0.8660254037844387076, 1.000000000000000000, 0.8660254037844387076, 1.000000000000000000, 0.9999994071668198981, 0.9999988143388863771 ) ) 
 REPRESENTATION_ITEM ( '' )  );
#72694 = CARTESIAN_POINT ( 'NONE',  ( 11.99999999999999822, -79.10210256391381733, 21.60688246758557796 ) ) ;
#72695 = ORIENTED_EDGE ( 'NONE', *, *, #4784, .F. ) ;
#72696 = CARTESIAN_POINT ( 'NONE',  ( -92.69370383062502583, 88.66845928578038638, 82.28739583420048120 ) ) ;
#72697 = ADVANCED_FACE ( 'NONE', ( #55508 ), #73524, .F. ) ;
#72698 = FACE_BOUND ( 'NONE', #3908, .T. ) ;
#72699 = CARTESIAN_POINT ( 'NONE',  ( 10.00000000000000000, 66.50666863322055633, -39.78640506895536078 ) ) ;
#72700 = EDGE_CURVE ( 'NONE', #37771, #60557, #70008, .T. ) ;
#72701 = CARTESIAN_POINT ( 'NONE',  ( -10.00000000000000000, 0.000000000000000000, 0.000000000000000000 ) ) ;
#72702 = CARTESIAN_POINT ( 'NONE',  ( 12.69589495141918611, -96.69089767102708777, 5.500000000000000000 ) ) ;
#72703 = DIRECTION ( 'NONE',  ( 0.000000000000000000, 0.4539904997395413089, 0.8910065241883705633 ) ) ;
#72704 = DIRECTION ( 'NONE',  ( 8.090853898039828715E-17, -9.269810975720166919E-17, 1.000000000000000000 ) ) ;
#72705 = ADVANCED_FACE ( 'NONE', ( #41450 ), #65139, .F. ) ;
#72706 = DIRECTION ( 'NONE',  ( -0.000000000000000000, -1.000000000000000000, -0.000000000000000000 ) ) ;
#72707 =( BOUNDED_CURVE ( )  B_SPLINE_CURVE ( 2, ( #55871, #56630, #4762, #28031, #16769, #16389, #68650 ),
 .UNSPECIFIED., .F., .F. ) 
 B_SPLINE_CURVE_WITH_KNOTS ( ( 3, 2, 2, 3 ),
 ( 0.2083333333333331483, 0.2152777777777775681, 0.2222222222222219323, 0.2291666666666663521 ),
 .UNSPECIFIED. ) 
 CURVE ( )  GEOMETRIC_REPRESENTATION_ITEM ( )  RATIONAL_B_SPLINE_CURVE ( ( 1.000000000000003775, 0.8660254037844349329, 1.000000000000000000, 0.8660254037844387076, 1.000000000000000000, 0.8660254037844445918, 0.9999999999999941158 ) ) 
 REPRESENTATION_ITEM ( '' )  );
#72708 = VECTOR ( 'NONE', #19709, 1000.000000000000000 ) ;
#72709 = CARTESIAN_POINT ( 'NONE',  ( 93.84685191531248449, 91.99731107132950569, 80.80572916753382628 ) ) ;
#72710 = CARTESIAN_POINT ( 'NONE',  ( -94.99999999999997158, -212.6630814284392557, 83.61031250086715261 ) ) ;
#72711 = DIRECTION ( 'NONE',  ( -1.000000000000000000, 0.000000000000000000, 0.000000000000000000 ) ) ;
#72712 = ORIENTED_EDGE ( 'NONE', *, *, #36143, .T. ) ;
#72713 = EDGE_CURVE ( 'NONE', #38392, #45539, #13159, .T. ) ;
#72714 = CARTESIAN_POINT ( 'NONE',  ( -97.65000000000003411, 90.00000928824094615, 86.90437468048608594 ) ) ;
#72715 = CARTESIAN_POINT ( 'NONE',  ( -92.34999999999999432, -211.5299782133524502, 76.92958333333332632 ) ) ;
#72716 = FACE_OUTER_BOUND ( 'NONE', #11919, .T. ) ;
#72717 = VECTOR ( 'NONE', #54656, 1000.000000000000114 ) ;
#72718 = CIRCLE ( 'NONE', #23535, 15.99999999999999822 ) ;
#72719 = AXIS2_PLACEMENT_3D ( 'NONE', #69307, #51650, #11772 ) ;
#72720 = CARTESIAN_POINT ( 'NONE',  ( -93.84685191531254134, 91.99731107132950569, 77.52489583420047836 ) ) ;
#72721 = CARTESIAN_POINT ( 'NONE',  ( 95.00000000000000000, -212.6630814284392557, 84.72156250086713669 ) ) ;
#72722 = EDGE_LOOP ( 'NONE', ( #11440, #23576, #62370, #51889 ) ) ;
#72723 = LINE ( 'NONE', #38912, #67077 ) ;
#72724 = EDGE_CURVE ( 'NONE', #24993, #22209, #54222, .T. ) ;
#72725 = ORIENTED_EDGE ( 'NONE', *, *, #66380, .F. ) ;
#72726 = AXIS2_PLACEMENT_3D ( 'NONE', #2760, #66252, #49308 ) ;
#72727 = LINE ( 'NONE', #44182, #59649 ) ;
#72728 = EDGE_CURVE ( 'NONE', #38655, #54641, #27534, .T. ) ;
#72729 = EDGE_CURVE ( 'NONE', #503, #23895, #56383, .T. ) ;
#72730 = EDGE_LOOP ( 'NONE', ( #42261, #22282, #2998, #62617 ) ) ;
#72731 = CARTESIAN_POINT ( 'NONE',  ( -97.64999999999996305, -209.9999999999999716, 83.65000000000000568 ) ) ;
#72732 = ADVANCED_FACE ( 'NONE', ( #53106 ), #1643, .F. ) ;
#72733 = ADVANCED_FACE ( 'NONE', ( #36916 ), #20344, .F. ) ;
#72734 = ORIENTED_EDGE ( 'NONE', *, *, #42342, .F. ) ;
#72735 = ORIENTED_EDGE ( 'NONE', *, *, #22772, .T. ) ;
#72736 = FACE_OUTER_BOUND ( 'NONE', #9634, .T. ) ;
#72737 = FACE_OUTER_BOUND ( 'NONE', #16382, .T. ) ;
#72738 = EDGE_CURVE ( 'NONE', #48910, #67887, #30160, .T. ) ;
#72739 = DIRECTION ( 'NONE',  ( -1.000000000000000000, 0.000000000000000000, 0.000000000000000000 ) ) ;
#72740 = CARTESIAN_POINT ( 'NONE',  ( -94.99999999999997158, -209.9999999999999716, 90.00000000000000000 ) ) ;
#72741 = CARTESIAN_POINT ( 'NONE',  ( 97.30629616937498838, 88.66845928578037217, 87.52614583420049144 ) ) ;
#72742 = CARTESIAN_POINT ( 'NONE',  ( 11.99999999999999822, 40.65526001592713357, -71.21200624218752750 ) ) ;
#72743 = CARTESIAN_POINT ( 'NONE',  ( 92.35000000000002274, -208.4700217866474645, 77.24708333333332178 ) ) ;
#72744 = EDGE_LOOP ( 'NONE', ( #65867, #25410, #7100, #6480 ) ) ;
#72745 = ADVANCED_FACE ( 'NONE', ( #19985 ), #59862, .F. ) ;
#72746 = ORIENTED_EDGE ( 'NONE', *, *, #53002, .F. ) ;
#72747 = VERTEX_POINT ( 'NONE', #64394 ) ;
#72748 = VERTEX_POINT ( 'NONE', #70747 ) ;
#72749 = DIRECTION ( 'NONE',  ( 0.7950889364178788110, -0.6064928550163524168, 0.000000000000000000 ) ) ;
#72750 = DIRECTION ( 'NONE',  ( -0.000000000000000000, 0.5000000000000003331, -0.8660254037844384856 ) ) ;
#72751 = CARTESIAN_POINT ( 'NONE',  ( -92.34999999999999432, -208.4700217866474645, 77.03541666666666288 ) ) ;
#72752 = CARTESIAN_POINT ( 'NONE',  ( -10.00000000000000000, 0.000000000000000000, 0.000000000000000000 ) ) ;
#72753 = DIRECTION ( 'NONE',  ( 0.000000000000000000, 0.000000000000000000, -1.000000000000000000 ) ) ;
#72754 = DIRECTION ( 'NONE',  ( 0.000000000000000000, 0.000000000000000000, 1.000000000000000000 ) ) ;
#72755 = ORIENTED_EDGE ( 'NONE', *, *, #34196, .F. ) ;
#72756 = CARTESIAN_POINT ( 'NONE',  ( -93.67499999999998295, -207.7050326799711968, 85.42270833506762528 ) ) ;
#72757 = ORIENTED_EDGE ( 'NONE', *, *, #18987, .F. ) ;
#72758 = CARTESIAN_POINT ( 'NONE',  ( 15.00000000000000000, -14.54903810567676636, -22.19967320028755964 ) ) ;
#72759 = VERTEX_POINT ( 'NONE', #12503 ) ;
#72760 = CARTESIAN_POINT ( 'NONE',  ( -96.32500000000001705, 87.70503267997129626, 81.29520833506762756 ) ) ;
#72761 = ORIENTED_EDGE ( 'NONE', *, *, #9131, .T. ) ;
#72762 = CARTESIAN_POINT ( 'NONE',  ( 93.84685191531248449, 91.99731107132950569, 82.07572916753382231 ) ) ;
#72763 = VECTOR ( 'NONE', #53840, 1000.000000000000000 ) ;
#72764 = DIRECTION ( 'NONE',  ( 1.000000000000000000, 0.000000000000000000, 0.000000000000000000 ) ) ;
#72765 = CARTESIAN_POINT ( 'NONE',  ( 10.00000000000000000, 16.65972982745046238, -80.28980883073739960 ) ) ;
#72766 = FACE_OUTER_BOUND ( 'NONE', #72644, .T. ) ;
#72767 = CARTESIAN_POINT ( 'NONE',  ( -6.782329983125270800, 10.49999999999999467, -145.0000000000000000 ) ) ;
#72768 = LINE ( 'NONE', #11127, #14457 ) ;
#72769 = ORIENTED_EDGE ( 'NONE', *, *, #14493, .T. ) ;
#72770 = CARTESIAN_POINT ( 'NONE',  ( 12.69589495141918611, -96.69089767102708777, -5.500000000000000000 ) ) ;
#72771 = CARTESIAN_POINT ( 'NONE',  ( 11.99999999999999822, -77.19088730480528682, 6.903761155837505825 ) ) ;
#72772 = ORIENTED_EDGE ( 'NONE', *, *, #4513, .T. ) ;
#72773 = AXIS2_PLACEMENT_3D ( 'NONE', #29399, #34686, #23416 ) ;
#72774 = VERTEX_POINT ( 'NONE', #12864 ) ;
#72775 = VECTOR ( 'NONE', #15641, 1000.000000000000000 ) ;
#72776 = PRODUCT ( 'radial ball bearing_68_iso_ISO 15 RBB - 3025 - 14,SI,NC,14_68', 'radial ball bearing_68_iso_ISO 15 RBB - 3025 - 14,SI,NC,14_68', '', ( #34680 ) ) ;
#72777 = CARTESIAN_POINT ( 'NONE',  ( -10.00000000000000000, 0.000000000000000000, 0.000000000000000000 ) ) ;
#72778 = CIRCLE ( 'NONE', #28358, 15.50000000000000000 ) ;
#72779 = FACE_OUTER_BOUND ( 'NONE', #57181, .T. ) ;
#72780 = DIRECTION ( 'NONE',  ( 0.5687579148473743684, -0.8225049752423791993, 0.000000000000000000 ) ) ;
#72781 = CARTESIAN_POINT ( 'NONE',  ( -92.69370383062498320, -208.6684592857803011, 85.09197916753380753 ) ) ;
#72782 = ORIENTED_EDGE ( 'NONE', *, *, #13660, .T. ) ;
#72783 = CARTESIAN_POINT ( 'NONE',  ( 92.35000000000000853, -209.9999999999999716, 81.10999999999999943 ) ) ;
#72784 = ORIENTED_EDGE ( 'NONE', *, *, #23352, .F. ) ;
#72785 = EDGE_CURVE ( 'NONE', #5647, #12010, #35793, .T. ) ;
#72786 = DIRECTION ( 'NONE',  ( -1.000000000000000000, -0.000000000000000000, -0.000000000000000000 ) ) ;
#72787 = DIRECTION ( 'NONE',  ( -0.000000000000000000, -0.000000000000000000, 1.000000000000000000 ) ) ;
#72788 = ADVANCED_FACE ( 'NONE', ( #7248 ), #58369, .T. ) ;
#72789 = CARTESIAN_POINT ( 'NONE',  ( 10.00000000000000000, 41.76937507738788469, 62.50329211542452157 ) ) ;
#72790 = CARTESIAN_POINT ( 'NONE',  ( 92.69370383062498320, 91.33154071421968467, 78.79489583420047438 ) ) ;
#72791 = CARTESIAN_POINT ( 'NONE',  ( 5.000000000000002665, -16.65972982744877484, -80.28980883073775487 ) ) ;
#72792 = LINE ( 'NONE', #55532, #41028 ) ;
#72793 = CARTESIAN_POINT ( 'NONE',  ( 23.49916127795269460, -121.5130826919798039, 5.500000000000000000 ) ) ;
#72794 = DIRECTION ( 'NONE',  ( 0.000000000000000000, 0.000000000000000000, 1.000000000000000000 ) ) ;
#72795 = EDGE_CURVE ( 'NONE', #65945, #5973, #43181, .T. ) ;
#72797 = EDGE_CURVE ( 'NONE', #50886, #58346, #24170, .T. ) ;
#72796 = CARTESIAN_POINT ( 'NONE',  ( 0.000000000000000000, -51.29473840253270112, 63.97538442413407012 ) ) ;
#72798 = CARTESIAN_POINT ( 'NONE',  ( 6.509281303079589520, -14.89695620656361008, -1.199999999999999956 ) ) ;
#72799 = CARTESIAN_POINT ( 'NONE',  ( -100.0000000000000142, 95.00000000000002842, -90.00000000000000000 ) ) ;
#72800 = CARTESIAN_POINT ( 'NONE',  ( 10.00000000000000000, -9.188173127307003085, -40.98264845739760176 ) ) ;
#72801 = CARTESIAN_POINT ( 'NONE',  ( -93.67499999999998295, -212.2949673200287179, 75.68604166840097491 ) ) ;
#72802 = EDGE_LOOP ( 'NONE', ( #3464, #11011, #59387, #64757 ) ) ;
#72803 = CARTESIAN_POINT ( 'NONE',  ( -92.69370383062504004, 90.00000000000004263, 83.61031250086713840 ) ) ;
#72804 = CYLINDRICAL_SURFACE ( 'NONE', #4765, 82.00000000000000000 ) ;
#72805 = CLOSED_SHELL ( 'NONE', ( #8900, #50563, #26284, #29103, #63156, #32860, #5995, #6331, #57401, #71531, #62601, #63426, #46180, #66320, #62958, #34714, #68760, #11105, #48782, #29414, #7500, #47676 ) ) ;
#72806 = EDGE_CURVE ( 'NONE', #11119, #9632, #36175, .T. ) ;
#72807 = DIRECTION ( 'NONE',  ( 0.000000000000000000, 0.000000000000000000, -1.000000000000000000 ) ) ;
#72808 = ORIENTED_EDGE ( 'NONE', *, *, #7290, .T. ) ;
#72809 = LINE ( 'NONE', #32224, #23478 ) ;
#72810 = CARTESIAN_POINT ( 'NONE',  ( 10.00000000000000000, -36.73666225445940370, 65.58780272294062286 ) ) ;
#72811 = CIRCLE ( 'NONE', #5625, 31.99999999999999289 ) ;
#72812 = CARTESIAN_POINT ( 'NONE',  ( 0.000000000000000000, -73.95703589263958122, -23.16143007188506431 ) ) ;
#72813 = VECTOR ( 'NONE', #34295, 1000.000000000000000 ) ;
#72814 = DIRECTION ( 'NONE',  ( -0.000000000000000000, -0.000000000000000000, 1.000000000000000000 ) ) ;
#72815 = EDGE_CURVE ( 'NONE', #4680, #9035, #30524, .T. ) ;
#72816 = EDGE_CURVE ( 'NONE', #69166, #32269, #24898, .T. ) ;
#72817 = CARTESIAN_POINT ( 'NONE',  ( 93.84685191531249870, -208.0026889286704943, 78.90072916753382515 ) ) ;
#72818 = ORIENTED_EDGE ( 'NONE', *, *, #44168, .T. ) ;
#72819 = AXIS2_PLACEMENT_3D ( 'NONE', #29901, #41203, #13722 ) ;
#72821 = EDGE_LOOP ( 'NONE', ( #61512, #61674, #31860, #73563 ) ) ;
#72820 = SHAPE_REPRESENTATION ( 'electric motor unit', ( #43395 ), #41132 ) ;
#72822 = CYLINDRICAL_SURFACE ( 'NONE', #14030, 31.99999999999999289 ) ;
#72823 = VECTOR ( 'NONE', #68399, 1000.000000000000000 ) ;
#72824 = LINE ( 'NONE', #26605, #73757 ) ;
#72825 = CARTESIAN_POINT ( 'NONE',  ( -97.64999999999996305, -210.0000359324575925, 85.63437624451401575 ) ) ;
#72826 = CARTESIAN_POINT ( 'NONE',  ( -8.637688417678527131, 13.69818742750669394, 42.00000000000001421 ) ) ;
#72827 = LINE ( 'NONE', #54093, #36899 ) ;
#72828 = CARTESIAN_POINT ( 'NONE',  ( 95.00000000000000000, -207.3369185715606307, 76.94281250086714863 ) ) ;
#72829 = VERTEX_POINT ( 'NONE', #3835 ) ;
#72830 = DIRECTION ( 'NONE',  ( -1.000000000000000000, 0.000000000000000000, 0.000000000000000000 ) ) ;
#72831 = ORIENTED_EDGE ( 'NONE', *, *, #6036, .F. ) ;
#72832 = ORIENTED_EDGE ( 'NONE', *, *, #47052, .F. ) ;
#72833 = LINE ( 'NONE', #66849, #14111 ) ;
#72834 = CIRCLE ( 'NONE', #5698, 16.00000000000000355 ) ;
#72835 = PRESENTATION_STYLE_ASSIGNMENT (( #49917 ) ) ;
#72836 = LINE ( 'NONE', #60485, #16119 ) ;
#72837 = ORIENTED_EDGE ( 'NONE', *, *, #10807, .F. ) ;
#72838 = LINE ( 'NONE', #67226, #34145 ) ;
#72839 = CARTESIAN_POINT ( 'NONE',  ( 92.35000000000002274, -211.5299782133524502, 79.33729166840096525 ) ) ;
#72840 = CARTESIAN_POINT ( 'NONE',  ( 94.99999999999998579, 86.94004357329500010, 81.90374999999998806 ) ) ;
#72841 = CIRCLE ( 'NONE', #41739, 77.49900000000000944 ) ;
#72842 = ORIENTED_EDGE ( 'NONE', *, *, #49659, .F. ) ;
#72843 = DIRECTION ( 'NONE',  ( -0.000000000000000000, -0.000000000000000000, -1.000000000000000000 ) ) ;
#72844 = EDGE_LOOP ( 'NONE', ( #37189, #65000, #30618, #67865 ) ) ;
#72845 = CARTESIAN_POINT ( 'NONE',  ( -96.32499999999996021, -212.2949673200287179, 88.91520833506763211 ) ) ;
#72846 = ORIENTED_EDGE ( 'NONE', *, *, #58382, .F. ) ;
#72847 = CARTESIAN_POINT ( 'NONE',  ( 94.99999999999998579, 93.05995642670504253, 84.20562500173429044 ) ) ;
#72848 = CARTESIAN_POINT ( 'NONE',  ( -97.30629616937501680, 90.00000000000004263, 85.99156250086716113 ) ) ;
#72849 = CARTESIAN_POINT ( 'NONE',  ( 92.69370383062498320, 90.00000000000002842, 78.21281250086714465 ) ) ;
#72850 = VERTEX_POINT ( 'NONE', #60958 ) ;
#72851 = CARTESIAN_POINT ( 'NONE',  ( 10.00000000000000000, 37.58145647212453611, 0.6853352020791767529 ) ) ;
#72852 = CARTESIAN_POINT ( 'NONE',  ( 0.000000000000000000, 54.21277698773752718, -55.38113227695725271 ) ) ;
#72853 = ORIENTED_EDGE ( 'NONE', *, *, #73939, .T. ) ;
#72854 = DIRECTION ( 'NONE',  ( 0.000000000000000000, 0.000000000000000000, -1.000000000000000000 ) ) ;
#72855 = CARTESIAN_POINT ( 'NONE',  ( -92.69370383062498320, -208.6684592857803011, 79.85322916753379729 ) ) ;
#72856 = ORIENTED_EDGE ( 'NONE', *, *, #50061, .T. ) ;
#72857 = ORIENTED_EDGE ( 'NONE', *, *, #8450, .F. ) ;
#72858 = CARTESIAN_POINT ( 'NONE',  ( 92.34999999999999432, 90.00000000000002842, 79.83999999999998920 ) ) ;
#72859 = EDGE_LOOP ( 'NONE', ( #54912, #18643, #10047, #62640 ) ) ;
#72860 = CARTESIAN_POINT ( 'NONE',  ( -97.64995694994090059, -208.4699969316842783, 81.13645661577280066 ) ) ;
#72861 = CARTESIAN_POINT ( 'NONE',  ( 94.99999999999998579, 93.05995642670504253, 89.28562500173430294 ) ) ;
#72862 = ORIENTED_EDGE ( 'NONE', *, *, #63347, .F. ) ;
#72863 = CARTESIAN_POINT ( 'NONE',  ( -93.84685191531247028, -211.9973110713294489, 80.96447916753380980 ) ) ;
#72864 = ORIENTED_EDGE ( 'NONE', *, *, #23604, .F. ) ;
#72865 = DIRECTION ( 'NONE',  ( -1.000000000000000000, -0.000000000000000000, 0.000000000000000000 ) ) ;
#72866 = CIRCLE ( 'NONE', #58455, 82.00000000000000000 ) ;
#72867 = DIRECTION ( 'NONE',  ( 0.000000000000000000, -0.4999999999999930611, 0.8660254037844425934 ) ) ;
#72868 = DIRECTION ( 'NONE',  ( -1.000000000000000000, 0.000000000000000000, 0.000000000000000000 ) ) ;
#72869 = LINE ( 'NONE', #21374, #39911 ) ;
#72870 = ADVANCED_FACE ( 'NONE', ( #72226 ), #43325, .T. ) ;
#72871 = VECTOR ( 'NONE', #60503, 1000.000000000000000 ) ;
#72872 = EDGE_CURVE ( 'NONE', #52624, #48290, #10755, .T. ) ;
#72873 = CARTESIAN_POINT ( 'NONE',  ( 15.00000000000000000, 8.688484142253932063, -21.88630264137371029 ) ) ;
#72874 = VECTOR ( 'NONE', #62468, 1000.000000000000000 ) ;
#72875 = EDGE_CURVE ( 'NONE', #21153, #5291, #66245, .T. ) ;
#72876 = CARTESIAN_POINT ( 'NONE',  ( 96.32499999999998863, -207.7050326799711968, 82.24770833506762813 ) ) ;
#72877 = CARTESIAN_POINT ( 'NONE',  ( 96.15314808468748708, 88.00268892867053694, 87.94947916753380923 ) ) ;
#72878 = AXIS2_PLACEMENT_3D ( 'NONE', #40368, #63315, #62196 ) ;
#72879 = DIRECTION ( 'NONE',  ( -1.000000000000000000, 0.000000000000000000, -0.000000000000000000 ) ) ;
#72880 = DIRECTION ( 'NONE',  ( 0.000000000000000000, -0.4999999999999913403, -0.8660254037844435926 ) ) ;
#72881 = CARTESIAN_POINT ( 'NONE',  ( -95.00000000000002842, 86.94004357329504273, 86.98374999999998636 ) ) ;
#72883 = EDGE_CURVE ( 'NONE', #7244, #73443, #14356, .T. ) ;
#72882 = CARTESIAN_POINT ( 'NONE',  ( 10.00000000000000000, 65.59268652807210742, 36.72794159290264560 ) ) ;
#72884 = DIRECTION ( 'NONE',  ( 0.000000000000000000, 0.000000000000000000, 1.000000000000000000 ) ) ;
#72885 = DIRECTION ( 'NONE',  ( -1.000000000000000000, -0.000000000000000000, -0.000000000000000000 ) ) ;
#72886 = CARTESIAN_POINT ( 'NONE',  ( -92.35000000000003695, 90.00000000000004263, 75.71250000000000568 ) ) ;
#72887 = EDGE_CURVE ( 'NONE', #24570, #72748, #62404, .T. ) ;
#72888 = CARTESIAN_POINT ( 'NONE',  ( 3.351853367131008454, -3.838309248099023296, -6.000000000000000000 ) ) ;
#72889 = CARTESIAN_POINT ( 'NONE',  ( 6.000000000000000000, 80.55351364060589958, 15.33399622253512540 ) ) ;
#72890 = CYLINDRICAL_SURFACE ( 'NONE', #50282, 2.649999999999985700 ) ;
#72891 = AXIS2_PLACEMENT_3D ( 'NONE', #74143, #22654, #32616 ) ;
#72892 = CARTESIAN_POINT ( 'NONE',  ( -93.67499999999998295, -207.7050326799711968, 85.97833333333332462 ) ) ;
#72893 = EDGE_CURVE ( 'NONE', #11217, #52914, #29945, .T. ) ;
#72894 = VECTOR ( 'NONE', #23234, 1000.000000000000227 ) ;
#72895 = CARTESIAN_POINT ( 'NONE',  ( -92.34999999999999432, -209.9999999999999716, 90.00000000000000000 ) ) ;
#72896 = EDGE_CURVE ( 'NONE', #12388, #43826, #2365, .T. ) ;
#72897 = DIRECTION ( 'NONE',  ( -1.000000000000000000, -0.000000000000000000, -0.000000000000000000 ) ) ;
#72898 = CARTESIAN_POINT ( 'NONE',  ( 11.99999999999999822, -62.20884554314051229, 46.21855187248609553 ) ) ;
#72899 = CARTESIAN_POINT ( 'NONE',  ( 7.999999999999992895, 1.142349898368116708E-14, 6.370018489481387452E-15 ) ) ;
#72900 = DIRECTION ( 'NONE',  ( 0.000000000000000000, 0.000000000000000000, 1.000000000000000000 ) ) ;
#72901 = EDGE_CURVE ( 'NONE', #29598, #63684, #3588, .T. ) ;
#72902 = ADVANCED_FACE ( 'NONE', ( #21456 ), #26723, .F. ) ;
#72903 = CARTESIAN_POINT ( 'NONE',  ( 92.69370383062501162, -209.9999999999999716, 75.03781250086713328 ) ) ;
#72904 = ORIENTED_EDGE ( 'NONE', *, *, #14413, .F. ) ;
#72905 = ORIENTED_EDGE ( 'NONE', *, *, #62515, .F. ) ;
#72906 = CARTESIAN_POINT ( 'NONE',  ( 10.00000000000000000, -10.96151621346514382, 35.95386929396252640 ) ) ;
#72907 = CARTESIAN_POINT ( 'NONE',  ( 0.000000000000000000, 0.000000000000000000, 0.000000000000000000 ) ) ;
#72908 = ORIENTED_EDGE ( 'NONE', *, *, #23881, .T. ) ;
#72909 =( BOUNDED_CURVE ( )  B_SPLINE_CURVE ( 2, ( #33399, #27778, #72147, #73628, #21013, #22142, #43965, #9002, #61259 ),
 .UNSPECIFIED., .F., .F. ) 
 B_SPLINE_CURVE_WITH_KNOTS ( ( 3, 2, 2, 2, 3 ),
 ( 0.000000000000000000, 0.007055765540917050167, 0.01411153108183410033, 0.02116729662275115137, 0.02116741234835334273 ),
 .UNSPECIFIED. ) 
 CURVE ( )  GEOMETRIC_REPRESENTATION_ITEM ( )  RATIONAL_B_SPLINE_CURVE ( ( 1.000000000000000000, 0.8660254037844387076, 1.000000000000000000, 0.8660254037844387076, 1.000000000000000000, 0.8660254037844387076, 1.000000000000000000, 0.9999978026068560011, 0.9999956052857933431 ) ) 
 REPRESENTATION_ITEM ( '' )  );
#72910 = CARTESIAN_POINT ( 'NONE',  ( 92.69370383062501162, -208.6684592857803295, 78.79489583420047438 ) ) ;
#72911 = CARTESIAN_POINT ( 'NONE',  ( 92.69370383062501162, -211.3315407142195852, 84.13947916753383538 ) ) ;
#72912 = CIRCLE ( 'NONE', #8108, 31.99999999999999289 ) ;
#72913 = VERTEX_POINT ( 'NONE', #48678 ) ;
#72914 = CARTESIAN_POINT ( 'NONE',  ( 92.69370383062501162, -209.9999999999999716, 84.72156250086715090 ) ) ;
#72915 = CIRCLE ( 'NONE', #64579, 12.49999999999999645 ) ;
#72916 = ORIENTED_EDGE ( 'NONE', *, *, #20806, .F. ) ;
#72917 = DIRECTION ( 'NONE',  ( 0.000000000000000000, 0.9876883405951383255, -0.1564344650402277048 ) ) ;
#72918 = ORIENTED_EDGE ( 'NONE', *, *, #61890, .T. ) ;
#72919 = CARTESIAN_POINT ( 'NONE',  ( 12.00000000000000000, -11.95096189432312350, 23.69967320028773017 ) ) ;
#72920 = VECTOR ( 'NONE', #55976, 1000.000000000000114 ) ;
#72921 = ORIENTED_EDGE ( 'NONE', *, *, #54685, .F. ) ;
#72922 = DIRECTION ( 'NONE',  ( -1.000000000000000000, 0.000000000000000000, 0.000000000000000000 ) ) ;
#72923 = AXIS2_PLACEMENT_3D ( 'NONE', #74112, #34261, #57208 ) ;
#72924 = EDGE_LOOP ( 'NONE', ( #13381, #20868, #36795, #59764 ) ) ;
#72925 = CYLINDRICAL_SURFACE ( 'NONE', #60555, 82.00000000000000000 ) ;
#72926 = CARTESIAN_POINT ( 'NONE',  ( 97.64999999999997726, -211.5299782133524502, 89.07395833506762983 ) ) ;
#72927 = ORIENTED_EDGE ( 'NONE', *, *, #55153, .T. ) ;
#72928 = DIRECTION ( 'NONE',  ( 1.000000000000000000, -0.000000000000000000, -0.000000000000000000 ) ) ;
#72929 = ORIENTED_EDGE ( 'NONE', *, *, #2237, .F. ) ;
#72930 = CYLINDRICAL_SURFACE ( 'NONE', #72053, 77.49899999999999523 ) ;
#72931 = ORIENTED_EDGE ( 'NONE', *, *, #12454, .T. ) ;
#72932 = ADVANCED_FACE ( 'NONE', ( #37781 ), #8084, .T. ) ;
#72933 = ORIENTED_EDGE ( 'NONE', *, *, #66073, .F. ) ;
#72934 = ORIENTED_EDGE ( 'NONE', *, *, #54598, .F. ) ;
#72935 = CARTESIAN_POINT ( 'NONE',  ( 97.30629616937498838, -209.9999999999999716, 76.62531250086713897 ) ) ;
#72936 = ITEM_DEFINED_TRANSFORMATION ( 'NONE', 'NONE', #68817,  #43395 ) ;
#72937 = CARTESIAN_POINT ( 'NONE',  ( 11.99999999999999822, -72.35432306680498016, 20.40083707022857951 ) ) ;
#72938 = ORIENTED_EDGE ( 'NONE', *, *, #62686, .F. ) ;
#72939 = CIRCLE ( 'NONE', #6961, 32.50000000000000000 ) ;
#72940 = VERTEX_POINT ( 'NONE', #13715 ) ;
#72941 = CIRCLE ( 'NONE', #50148, 77.49899999999998101 ) ;
#72943 = EDGE_CURVE ( 'NONE', #44177, #18340, #5680, .T. ) ;
#72942 = ORIENTED_EDGE ( 'NONE', *, *, #19242, .T. ) ;
#72944 = CARTESIAN_POINT ( 'NONE',  ( 7.999999999999994671, -1.569751293914625593E-13, -15.80000000000027605 ) ) ;
#72945 = CARTESIAN_POINT ( 'NONE',  ( -5.250000000000000888, -13.95926121303099343, -1.199999999999999956 ) ) ;
#72946 = VECTOR ( 'NONE', #14491, 1000.000000000000000 ) ;
#72948 = EDGE_CURVE ( 'NONE', #53187, #62552, #70790, .T. ) ;
#72947 = VECTOR ( 'NONE', #61734, 1000.000000000000000 ) ;
#72949 = CARTESIAN_POINT ( 'NONE',  ( -97.65000000000001990, 91.52997821335253548, 89.94708333333333883 ) ) ;
#72950 = ORIENTED_EDGE ( 'NONE', *, *, #9855, .F. ) ;
#72951 = CARTESIAN_POINT ( 'NONE',  ( 94.99999999999998579, 92.66308142843935514, 78.68906250086713783 ) ) ;
#72952 = EDGE_CURVE ( 'NONE', #73705, #39929, #15582, .T. ) ;
#72953 = VECTOR ( 'NONE', #61746, 1000.000000000000000 ) ;
#72954 = VERTEX_POINT ( 'NONE', #26106 ) ;
#72955 = CARTESIAN_POINT ( 'NONE',  ( 12.00000000000000000, -13.04903810567675393, -19.60159698893424718 ) ) ;
#72956 = DIRECTION ( 'NONE',  ( -1.000000000000000000, -0.000000000000000000, 0.000000000000000000 ) ) ;
#72957 = VERTEX_POINT ( 'NONE', #25386 ) ;
#72958 = CARTESIAN_POINT ( 'NONE',  ( 0.000000000000000000, 0.000000000000000000, 0.000000000000000000 ) ) ;
#72959 = CARTESIAN_POINT ( 'NONE',  ( 10.00000000000000000, -72.35432306680469594, -20.40083707022958848 ) ) ;
#72960 = CARTESIAN_POINT ( 'NONE',  ( 10.00000000000000000, 0.000000000000000000, 0.000000000000000000 ) ) ;
#72961 = CARTESIAN_POINT ( 'NONE',  ( -93.84685191531247028, -211.9973110713294489, 78.42447916753381776 ) ) ;
#72962 = ADVANCED_FACE ( 'NONE', ( #38135 ), #61072, .T. ) ;
#72963 = FACE_OUTER_BOUND ( 'NONE', #768, .T. ) ;
#72964 = CARTESIAN_POINT ( 'NONE',  ( 10.00000000000000000, 14.66109333815564852, -73.73191006444555740 ) ) ;
#72965 = CARTESIAN_POINT ( 'NONE',  ( 10.00000000000000000, 0.000000000000000000, 0.000000000000000000 ) ) ;
#72966 = ORIENTED_EDGE ( 'NONE', *, *, #9253, .F. ) ;
#72968 = VERTEX_POINT ( 'NONE', #71966 ) ;
#72967 = EDGE_CURVE ( 'NONE', #19971, #43677, #67155, .T. ) ;
#72969 = DIRECTION ( 'NONE',  ( -1.000000000000000000, -0.000000000000000000, -0.000000000000000000 ) ) ;
#72970 = DIRECTION ( 'NONE',  ( 0.000000000000000000, 0.7604059656000276002, 0.6494480483301876550 ) ) ;
#72971 = CARTESIAN_POINT ( 'NONE',  ( 93.09104985768162521, -208.4386293813703048, 74.88237134757146407 ) ) ;
#72972 = CARTESIAN_POINT ( 'NONE',  ( -92.69370383062502583, 91.33154071421968467, 81.75822916753381264 ) ) ;
#72973 = LINE ( 'NONE', #72602, #16659 ) ;
#72974 = CARTESIAN_POINT ( 'NONE',  ( 10.00000000000000000, -35.53030884539077050, -12.26510123303296851 ) ) ;
#72975 = ADVANCED_FACE ( 'NONE', ( #60713 ), #9192, .F. ) ;
#72976 = VECTOR ( 'NONE', #50287, 1000.000000000000000 ) ;
#72977 = ORIENTED_EDGE ( 'NONE', *, *, #7654, .T. ) ;
#72978 = CARTESIAN_POINT ( 'NONE',  ( 2.499999999999979572, 90.00000000000000000, -280.0000000000000000 ) ) ;
#72979 = AXIS2_PLACEMENT_3D ( 'NONE', #11776, #51271, #62584 ) ;
#72980 = AXIS2_PLACEMENT_3D ( 'NONE', #54419, #66450, #48774 ) ;
#72981 = CARTESIAN_POINT ( 'NONE',  ( 0.000000000000000000, 77.16300072079660310, 27.74655509720696500 ) ) ;
#72982 = LINE ( 'NONE', #15865, #5750 ) ;
#72983 = AXIS2_PLACEMENT_3D ( 'NONE', #2027, #36554, #66262 ) ;
#72984 = CARTESIAN_POINT ( 'NONE',  ( 10.00000000000000000, 0.000000000000000000, 0.000000000000000000 ) ) ;
#72985 = CARTESIAN_POINT ( 'NONE',  ( -92.35000000000006537, 91.52997821335257811, 87.19541666666667368 ) ) ;
#72986 = CARTESIAN_POINT ( 'NONE',  ( -96.15314808468745866, -211.9973110713294489, 80.38239583420048007 ) ) ;
#72987 = EDGE_CURVE ( 'NONE', #42112, #37729, #8329, .T. ) ;
#72988 = CARTESIAN_POINT ( 'NONE',  ( -92.35000000045951651, -209.9999506483816560, 87.22187670868756015 ) ) ;
#72989 = EDGE_CURVE ( 'NONE', #50748, #9521, #62448, .T. ) ;
#72990 = EDGE_CURVE ( 'NONE', #1800, #7004, #21021, .T. ) ;
#72991 = VERTEX_POINT ( 'NONE', #9931 ) ;
#72992 = CARTESIAN_POINT ( 'NONE',  ( 5.999999999999999112, -71.21200624218768382, -40.65526001592688488 ) ) ;
#72993 = CARTESIAN_POINT ( 'NONE',  ( 10.00000000000000000, 0.000000000000000000, 0.000000000000000000 ) ) ;
#72994 = ORIENTED_EDGE ( 'NONE', *, *, #72162, .F. ) ;
#72995 = CARTESIAN_POINT ( 'NONE',  ( 10.00000000000000000, 26.08949754953024325, 27.05870788708241648 ) ) ;
#72996 = LINE ( 'NONE', #58226, #52188 ) ;
#72997 = CIRCLE ( 'NONE', #22706, 11.59999999999999787 ) ;
#72998 = UNCERTAINTY_MEASURE_WITH_UNIT (LENGTH_MEASURE( 1.000000000000000082E-05 ), #4459, 'distance_accuracy_value', 'NONE');
#72999 = AXIS2_PLACEMENT_3D ( 'NONE', #21264, #61893, #33292 ) ;
#73001 = CYLINDRICAL_SURFACE ( 'NONE', #63626, 2.649999999999985700 ) ;
#73000 = VECTOR ( 'NONE', #19306, 1000.000000000000000 ) ;
#73002 = EDGE_LOOP ( 'NONE', ( #19015, #3375, #41448, #18289 ) ) ;
#73003 = AXIS2_PLACEMENT_3D ( 'NONE', #23364, #57582, #27879 ) ;
#73004 = CARTESIAN_POINT ( 'NONE',  ( -92.35000000000179909, 90.00000306648279036, 75.79187510780352000 ) ) ;
#73005 = FACE_OUTER_BOUND ( 'NONE', #25624, .T. ) ;
#73006 = ORIENTED_EDGE ( 'NONE', *, *, #743, .F. ) ;
#73007 = VECTOR ( 'NONE', #11993, 1000.000000000000000 ) ;
#73008 = CARTESIAN_POINT ( 'NONE',  ( 6.000000000000000000, -34.94270380257585629, -74.18225833017926618 ) ) ;
#73009 = DIRECTION ( 'NONE',  ( 0.000000000000000000, -0.000000000000000000, 1.000000000000000000 ) ) ;
#73010 = ORIENTED_EDGE ( 'NONE', *, *, #24352, .F. ) ;
#73011 = DIRECTION ( 'NONE',  ( 1.000000000000000000, -3.061616997868382648E-16, 0.000000000000000000 ) ) ;
#73012 = ORIENTED_EDGE ( 'NONE', *, *, #73303, .T. ) ;
#73013 = CYLINDRICAL_SURFACE ( 'NONE', #38193, 31.99999999999998579 ) ;
#73014 = CARTESIAN_POINT ( 'NONE',  ( 92.35000000000000853, -209.9999999999999716, 81.74500000000000455 ) ) ;
#73015 = ORIENTED_EDGE ( 'NONE', *, *, #61781, .T. ) ;
#73016 = ORIENTED_EDGE ( 'NONE', *, *, #15289, .F. ) ;
#73017 = ORIENTED_EDGE ( 'NONE', *, *, #26796, .F. ) ;
#73018 = CARTESIAN_POINT ( 'NONE',  ( 2.500000000000034639, 90.00000000000000000, -90.00000000000000000 ) ) ;
#73019 = EDGE_CURVE ( 'NONE', #53437, #48441, #68, .T. ) ;
#73020 = VERTEX_POINT ( 'NONE', #21197 ) ;
#73021 = EDGE_LOOP ( 'NONE', ( #14411, #6778, #33257, #2816 ) ) ;
#73022 = CARTESIAN_POINT ( 'NONE',  ( 97.30629616937498838, 88.66845928578037217, 75.46114583420049371 ) ) ;
#73023 = CARTESIAN_POINT ( 'NONE',  ( 15.00000000000000000, -20.55727247249726020, 16.78983467731313084 ) ) ;
#73024 = CIRCLE ( 'NONE', #5827, 16.00000000000000000 ) ;
#73025 = DIRECTION ( 'NONE',  ( 0.000000000000000000, -0.000000000000000000, 1.000000000000000000 ) ) ;
#73026 = CIRCLE ( 'NONE', #65878, 77.49899999999999523 ) ;
#73027 = ORIENTED_EDGE ( 'NONE', *, *, #69994, .T. ) ;
#73028 = VERTEX_POINT ( 'NONE', #38883 ) ;
#73029 = ORIENTED_EDGE ( 'NONE', *, *, #44292, .T. ) ;
#73030 = CARTESIAN_POINT ( 'NONE',  ( 97.30629616937498838, 90.00000000000002842, 88.05531250086713158 ) ) ;
#73031 = VERTEX_POINT ( 'NONE', #10676 ) ;
#73032 = CARTESIAN_POINT ( 'NONE',  ( 92.69370383062501162, -211.3315407142195852, 86.52072916753381548 ) ) ;
#73033 = PRODUCT_CONTEXT ( 'NONE', #62377, 'mechanical' ) ;
#73034 = CARTESIAN_POINT ( 'NONE',  ( 10.00000000000000000, 0.000000000000000000, 0.000000000000000000 ) ) ;
#73035 = TOROIDAL_SURFACE ( 'NONE', #39474, 4.700000000000000178, 0.2999999999999999889 ) ;
#73036 = DIRECTION ( 'NONE',  ( -1.000000000000000000, -0.000000000000000000, -0.000000000000000000 ) ) ;
#73037 = CARTESIAN_POINT ( 'NONE',  ( 0.000000000000000000, 74.18225833017888249, 34.94270380257665209 ) ) ;
#73038 = VECTOR ( 'NONE', #51925, 1000.000000000000114 ) ;
#73039 = CARTESIAN_POINT ( 'NONE',  ( 0.000000000000000000, 0.000000000000000000, 0.000000000000000000 ) ) ;
#73040 = EDGE_CURVE ( 'NONE', #70465, #59562, #57669, .T. ) ;
#73041 = DIRECTION ( 'NONE',  ( 0.000000000000000000, 0.000000000000000000, -1.000000000000000000 ) ) ;
#73042 = CYLINDRICAL_SURFACE ( 'NONE', #16706, 31.99999999999998579 ) ;
#73043 = CARTESIAN_POINT ( 'NONE',  ( -96.15314808468745866, -211.9973110713294489, 89.11364583420048291 ) ) ;
#73044 = EDGE_CURVE ( 'NONE', #53287, #59768, #46830, .T. ) ;
#73045 = CARTESIAN_POINT ( 'NONE',  ( -96.15314808468751551, 88.00268892867056536, 84.19239583420049655 ) ) ;
#73046 = EDGE_LOOP ( 'NONE', ( #23940, #9349, #19774, #45693 ) ) ;
#73048 = CARTESIAN_POINT ( 'NONE',  ( -93.84685191531254134, 91.99731107132950569, 89.43114583420047836 ) ) ;
#73047 = CARTESIAN_POINT ( 'NONE',  ( 92.69370383062498320, 90.00000000000002842, 88.37281250086715545 ) ) ;
#73049 = ORIENTED_EDGE ( 'NONE', *, *, #20653, .T. ) ;
#73050 = DIRECTION ( 'NONE',  ( -1.000000000000000000, -0.000000000000000000, -0.000000000000000000 ) ) ;
#73051 = DIRECTION ( 'NONE',  ( 0.000000000000000000, 0.000000000000000000, 1.000000000000000000 ) ) ;
#73052 = CARTESIAN_POINT ( 'NONE',  ( 10.00000000000000000, 41.91543099594818500, -2.663952781846293139 ) ) ;
#73053 = CARTESIAN_POINT ( 'NONE',  ( 15.00000000000000000, -0.9646360437375368635, -23.52805723605589705 ) ) ;
#73054 = CARTESIAN_POINT ( 'NONE',  ( -12.40464318976454727, 10.41032311384371845, -55.00000000000000000 ) ) ;
#73055 = FACE_OUTER_BOUND ( 'NONE', #18962, .T. ) ;
#73056 = ADVANCED_FACE ( 'NONE', ( #50897 ), #15943, .T. ) ;
#73057 = AXIS2_PLACEMENT_3D ( 'NONE', #25316, #53144, #23832 ) ;
#73058 = EDGE_CURVE ( 'NONE', #51144, #1695, #42047, .T. ) ;
#73059 = CARTESIAN_POINT ( 'NONE',  ( 0.000000000000000000, -17.80606268964516659, -33.00180498840066434 ) ) ;
#73060 = CARTESIAN_POINT ( 'NONE',  ( 97.64999999999999147, 90.00000000000002842, 89.68250000000000455 ) ) ;
#73061 = ORIENTED_EDGE ( 'NONE', *, *, #53786, .F. ) ;
#73062 = AXIS2_PLACEMENT_3D ( 'NONE', #19505, #59743, #47711 ) ;
#73063 = ORIENTED_EDGE ( 'NONE', *, *, #56479, .F. ) ;
#73064 = CIRCLE ( 'NONE', #32219, 82.00000000000000000 ) ;
#73065 = AXIS2_PLACEMENT_3D ( 'NONE', #22255, #47046, #24474 ) ;
#73066 = CARTESIAN_POINT ( 'NONE',  ( -97.65000000000001990, 88.47002178664754979, 80.52791666666665549 ) ) ;
#73067 = CARTESIAN_POINT ( 'NONE',  ( -97.64999999950686060, 89.99996796133669363, 83.73041644179562581 ) ) ;
#73068 = DIRECTION ( 'NONE',  ( -1.000000000000000000, 0.000000000000000000, -0.000000000000000000 ) ) ;
#73069 = CARTESIAN_POINT ( 'NONE',  ( 11.99999999999999822, 74.65491531819105830, 8.830959090343693418 ) ) ;
#73070 = DIRECTION ( 'NONE',  ( 1.000000000000000000, 0.000000000000000000, 0.000000000000000000 ) ) ;
#73071 = DIRECTION ( 'NONE',  ( 0.000000000000000000, -0.9781476007338040235, -0.2079116908177671419 ) ) ;
#73072 = CARTESIAN_POINT ( 'NONE',  ( 10.00000000000000000, 14.67089635893713684, 73.72996012237443608 ) ) ;
#73073 = PRESENTATION_LAYER_ASSIGNMENT (  '', '', ( #20266 ) ) ;
#73074 = EDGE_CURVE ( 'NONE', #15264, #10428, #31188, .T. ) ;
#73075 = ORIENTED_EDGE ( 'NONE', *, *, #47626, .T. ) ;
#73076 = CARTESIAN_POINT ( 'NONE',  ( -97.30629616937501680, 88.66845928578038638, 82.71072916753379900 ) ) ;
#73077 = CARTESIAN_POINT ( 'NONE',  ( -0.0004442498508594591917, 0.001194404164628348752, -65.00000000000000000 ) ) ;
#73078 = CARTESIAN_POINT ( 'NONE',  ( 10.00000000000000000, -71.27951684758046724, 30.41916302227088309 ) ) ;
#73079 = CARTESIAN_POINT ( 'NONE',  ( 0.000000000000000000, 31.46837873494978055, 68.27212725128286763 ) ) ;
#73080 = DIRECTION ( 'NONE',  ( -1.000000000000000000, -0.000000000000000000, 0.000000000000000000 ) ) ;
#73081 = DIRECTION ( 'NONE',  ( 0.000000000000000000, 0.000000000000000000, 1.000000000000000000 ) ) ;
#73082 = LINE ( 'NONE', #56182, #50253 ) ;
#73083 = CARTESIAN_POINT ( 'NONE',  ( -92.34999999999999432, -209.9999999999999716, 79.52249999999999375 ) ) ;
#73084 = AXIS2_PLACEMENT_3D ( 'NONE', #68913, #40334, #68165 ) ;
#73085 = EDGE_CURVE ( 'NONE', #6668, #67004, #69615, .T. ) ;
#73086 = EDGE_CURVE ( 'NONE', #10014, #39132, #50139, .T. ) ;
#73087 = AXIS2_PLACEMENT_3D ( 'NONE', #3180, #71184, #25348 ) ;
#73088 = EDGE_CURVE ( 'NONE', #43461, #26241, #34800, .T. ) ;
#73089 = CARTESIAN_POINT ( 'NONE',  ( 97.30629616937498838, 91.33154071421968467, 79.37697916753381833 ) ) ;
#73090 = AXIS2_PLACEMENT_3D ( 'NONE', #68514, #33914, #12459 ) ;
#73091 = VECTOR ( 'NONE', #58218, 1000.000000000000000 ) ;
#73092 = CARTESIAN_POINT ( 'NONE',  ( -94.99999999999997158, -207.3369185715606307, 83.92781250086716227 ) ) ;
#73093 = DIRECTION ( 'NONE',  ( 0.000000000000000000, 0.000000000000000000, 1.000000000000000000 ) ) ;
#73094 = EDGE_LOOP ( 'NONE', ( #72808, #2806, #145, #53357 ) ) ;
#73095 = CARTESIAN_POINT ( 'NONE',  ( -94.99999999999997158, -206.9400435732949575, 77.77624999999999034 ) ) ;
#73096 = CARTESIAN_POINT ( 'NONE',  ( 92.35000000000000853, -211.5299782133524218, 78.70229166840096013 ) ) ;
#73097 = VECTOR ( 'NONE', #31564, 1000.000000000000000 ) ;
#73098 = VECTOR ( 'NONE', #73371, 1000.000000000000000 ) ;
#73099 = CARTESIAN_POINT ( 'NONE',  ( -96.15314808468752972, 91.99731107132950569, 78.90072916753382515 ) ) ;
#73100 = CARTESIAN_POINT ( 'NONE',  ( 97.30629616937498838, -208.6684592857803011, 80.48822916753383083 ) ) ;
#73101 = ORIENTED_EDGE ( 'NONE', *, *, #54074, .T. ) ;
#73102 = DIRECTION ( 'NONE',  ( 0.000000000000000000, 0.000000000000000000, 1.000000000000000000 ) ) ;
#73103 = ORIENTED_EDGE ( 'NONE', *, *, #74296, .T. ) ;
#73104 = CARTESIAN_POINT ( 'NONE',  ( -97.64999999993850111, -209.9999881782113675, 76.10900611559516449 ) ) ;
#73105 = ORIENTED_EDGE ( 'NONE', *, *, #39888, .T. ) ;
#73106 = AXIS2_PLACEMENT_3D ( 'NONE', #22230, #61350, #55700 ) ;
#73107 = DIRECTION ( 'NONE',  ( -1.000000000000000000, 0.000000000000000000, 0.000000000000000000 ) ) ;
#73108 = VECTOR ( 'NONE', #18709, 1000.000000000000000 ) ;
#73109 = AXIS2_PLACEMENT_3D ( 'NONE', #57810, #63455, #45049 ) ;
#73110 = ORIENTED_EDGE ( 'NONE', *, *, #16476, .F. ) ;
#73111 = ORIENTED_EDGE ( 'NONE', *, *, #68671, .T. ) ;
#73112 = AXIS2_PLACEMENT_3D ( 'NONE', #29291, #18027, #24048 ) ;
#73113 = VERTEX_POINT ( 'NONE', #10308 ) ;
#73114 = AXIS2_PLACEMENT_3D ( 'NONE', #72536, #37247, #66908 ) ;
#73115 = CARTESIAN_POINT ( 'NONE',  ( 97.30629616937498838, -209.9999999999999716, 76.14906250086716000 ) ) ;
#73116 = ORIENTED_EDGE ( 'NONE', *, *, #41866, .F. ) ;
#73117 = CARTESIAN_POINT ( 'NONE',  ( 11.99999999999999822, -54.21277698773713638, 55.38113227695764351 ) ) ;
#73118 = ADVANCED_FACE ( 'NONE', ( #5432 ), #33223, .T. ) ;
#73119 = AXIS2_PLACEMENT_3D ( 'NONE', #8111, #14113, #31037 ) ;
#73120 = CARTESIAN_POINT ( 'NONE',  ( -96.10855813661771663, 87.63060383671344766, 74.97612907457774156 ) ) ;
#73121 = CARTESIAN_POINT ( 'NONE',  ( 96.15314808468748708, 88.00268892867053694, 86.20322916753382003 ) ) ;
#73122 = FACE_OUTER_BOUND ( 'NONE', #72000, .T. ) ;
#73123 = CARTESIAN_POINT ( 'NONE',  ( 92.35000000000002274, -211.5299782133524502, 79.25791666666665947 ) ) ;
#73124 = ORIENTED_EDGE ( 'NONE', *, *, #53208, .T. ) ;
#73125 = VERTEX_POINT ( 'NONE', #22334 ) ;
#73126 = VERTEX_POINT ( 'NONE', #68199 ) ;
#73127 = EDGE_LOOP ( 'NONE', ( #23422, #55909, #296, #6280 ) ) ;
#73128 = CARTESIAN_POINT ( 'NONE',  ( 96.32499999999998863, -207.7050326799711968, 89.15333333333333599 ) ) ;
#73129 = ADVANCED_FACE ( 'NONE', ( #45277 ), #28327, .T. ) ;
#73130 = CARTESIAN_POINT ( 'NONE',  ( -97.64999999999996305, -209.9999999999999716, 90.00000000000000000 ) ) ;
#73131 = FACE_OUTER_BOUND ( 'NONE', #41884, .T. ) ;
#73132 = CARTESIAN_POINT ( 'NONE',  ( 11.99999999999999822, 8.830959090342393125, 74.65491531819122883 ) ) ;
#73133 = EDGE_CURVE ( 'NONE', #33517, #56683, #73452, .T. ) ;
#73134 = CARTESIAN_POINT ( 'NONE',  ( 0.000000000000000000, 33.71516098798741012, 74.74816331893441657 ) ) ;
#73135 = DIRECTION ( 'NONE',  ( -0.000000000000000000, -0.000000000000000000, 1.000000000000000000 ) ) ;
#73136 = ORIENTED_EDGE ( 'NONE', *, *, #11953, .F. ) ;
#73137 = CARTESIAN_POINT ( 'NONE',  ( -97.64999999999996305, -209.9999999999999716, 81.82437500173429612 ) ) ;
#73138 = EDGE_LOOP ( 'NONE', ( #23854, #2047, #27261, #51331 ) ) ;
#73139 = FACE_OUTER_BOUND ( 'NONE', #11222, .T. ) ;
#73140 = EDGE_LOOP ( 'NONE', ( #63535, #60482, #67876, #46236, #55673 ) ) ;
#73142 = CARTESIAN_POINT ( 'NONE',  ( -92.35000000000005116, 88.47002178664754979, 83.35895833506762642 ) ) ;
#73141 = CARTESIAN_POINT ( 'NONE',  ( 92.34999999999999432, 90.00000000000002842, 81.18937500173430521 ) ) ;
#73143 =( BOUNDED_CURVE ( )  B_SPLINE_CURVE ( 2, ( #70637, #19150, #42099, #66057, #37483, #50213, #22029 ),
 .UNSPECIFIED., .F., .F. ) 
 B_SPLINE_CURVE_WITH_KNOTS ( ( 3, 2, 2, 3 ),
 ( 0.2328402629019979686, 0.2398960283900005153, 0.2469517939308828458, 0.2540073681283128160 ),
 .UNSPECIFIED. ) 
 CURVE ( )  GEOMETRIC_REPRESENTATION_ITEM ( )  RATIONAL_B_SPLINE_CURVE ( ( 1.000000000000000000, 0.8660254037844387076, 1.000000000000000000, 0.8660254037844387076, 1.000000000000000000, 0.8660290370063226106, 0.9999927337532890093 ) ) 
 REPRESENTATION_ITEM ( '' )  );
#73144 = EDGE_LOOP ( 'NONE', ( #5837, #7840, #18492, #41878 ) ) ;
#73145 = CARTESIAN_POINT ( 'NONE',  ( 93.84685191531248449, 91.99731107132950569, 83.98072916753382344 ) ) ;
#73146 = LINE ( 'NONE', #70458, #43396 ) ;
#73147 = VECTOR ( 'NONE', #21906, 1000.000000000000114 ) ;
#73148 = CARTESIAN_POINT ( 'NONE',  ( -14.25258209288423750, -138.6845900058201551, -2.500000000000000000 ) ) ;
#73149 = AXIS2_PLACEMENT_3D ( 'NONE', #66823, #3323, #37889 ) ;
#73150 = DIRECTION ( 'NONE',  ( 0.000000000000000000, 0.000000000000000000, 1.000000000000000000 ) ) ;
#73151 = FACE_OUTER_BOUND ( 'NONE', #38765, .T. ) ;
#73152 = EDGE_CURVE ( 'NONE', #16336, #44625, #16818, .T. ) ;
#73153 = AXIS2_PLACEMENT_3D ( 'NONE', #73154, #5134, #68277 ) ;
#73154 = CARTESIAN_POINT ( 'NONE',  ( 15.00000000000000000, -3.948201729842355068, -23.21447184625292692 ) ) ;
#73155 = ORIENTED_EDGE ( 'NONE', *, *, #13261, .F. ) ;
#73156 = CARTESIAN_POINT ( 'NONE',  ( 97.64999999999999147, -209.9999999999999716, 77.61749999999999261 ) ) ;
#73157 = CARTESIAN_POINT ( 'NONE',  ( 11.99999999999999822, 0.000000000000000000, 0.000000000000000000 ) ) ;
#73158 = DIRECTION ( 'NONE',  ( 0.000000000000000000, 0.000000000000000000, 1.000000000000000000 ) ) ;
#73159 = ORIENTED_EDGE ( 'NONE', *, *, #19664, .F. ) ;
#73160 = VERTEX_POINT ( 'NONE', #72694 ) ;
#73161 = CIRCLE ( 'NONE', #65934, 16.00000000000000000 ) ;
#73162 = DIRECTION ( 'NONE',  ( -1.000000000000000000, -0.000000000000000000, -0.000000000000000000 ) ) ;
#73163 = EDGE_CURVE ( 'NONE', #42446, #68977, #33607, .T. ) ;
#73164 = DIRECTION ( 'NONE',  ( 0.000000000000000000, 0.9876883405951381034, -0.1564344650402276216 ) ) ;
#73165 = DIRECTION ( 'NONE',  ( -0.5000000000000039968, 0.8660254037844363761, 0.000000000000000000 ) ) ;
#73166 = CARTESIAN_POINT ( 'NONE',  ( -97.30629616937495996, -209.9999999999999716, 79.64156250086715261 ) ) ;
#73167 = ORIENTED_EDGE ( 'NONE', *, *, #31825, .T. ) ;
#73168 = CARTESIAN_POINT ( 'NONE',  ( 95.00000000000000000, -213.0599564267049857, 81.26874999999999716 ) ) ;
#73169 = EDGE_CURVE ( 'NONE', #48451, #72658, #57285, .T. ) ;
#73170 = ORIENTED_EDGE ( 'NONE', *, *, #7564, .T. ) ;
#73171 = CIRCLE ( 'NONE', #35930, 31.99999999999998934 ) ;
#73172 = LINE ( 'NONE', #56269, #15041 ) ;
#73173 = ADVANCED_FACE ( 'NONE', ( #63306 ), #18531, .T. ) ;
#73174 = VECTOR ( 'NONE', #70550, 1000.000000000000000 ) ;
#73175 = LINE ( 'NONE', #56270, #7108 ) ;
#73176 = CARTESIAN_POINT ( 'NONE',  ( 95.00000000000000000, -206.9400435732949575, 82.93562500173430863 ) ) ;
#73177 = CARTESIAN_POINT ( 'NONE',  ( 94.99999999999998579, 92.66308142843932671, 77.41906250086714181 ) ) ;
#73178 = CARTESIAN_POINT ( 'NONE',  ( 10.00000000000000000, 41.76106447765580043, -62.50884508063379741 ) ) ;
#73179 = CARTESIAN_POINT ( 'NONE',  ( -89.99999999999998579, -204.9999999999999716, 90.00000000000000000 ) ) ;
#73180 = CARTESIAN_POINT ( 'NONE',  ( 6.000000000000000000, -81.34940948281344220, 10.30890764327355846 ) ) ;
#73181 = VECTOR ( 'NONE', #35861, 1000.000000000000000 ) ;
#73182 = DIRECTION ( 'NONE',  ( -1.000000000000000000, 0.000000000000000000, 0.000000000000000000 ) ) ;
#73183 = AXIS2_PLACEMENT_3D ( 'NONE', #45395, #68697, #5551 ) ;
#73184 = DIRECTION ( 'NONE',  ( -1.000000000000000000, 0.000000000000000000, -0.000000000000000000 ) ) ;
#73185 = CARTESIAN_POINT ( 'NONE',  ( 11.99999999999999822, -21.60688246758531150, -79.10210256391390260 ) ) ;
#73186 = EDGE_CURVE ( 'NONE', #66703, #70184, #38439, .T. ) ;
#73187 = CARTESIAN_POINT ( 'NONE',  ( 93.67500000000001137, -212.2949673200287179, 83.12083333333332291 ) ) ;
#73188 = EDGE_CURVE ( 'NONE', #46917, #17376, #40362, .T. ) ;
#73189 = DIRECTION ( 'NONE',  ( -1.000000000000000000, -0.000000000000000000, -0.000000000000000000 ) ) ;
#73190 = CARTESIAN_POINT ( 'NONE',  ( -92.35001786631356424, 88.47001147152658973, 78.27895762153875125 ) ) ;
#73191 = ORIENTED_EDGE ( 'NONE', *, *, #42382, .T. ) ;
#73192 = CARTESIAN_POINT ( 'NONE',  ( -97.30629616937501680, 91.33154071421968467, 83.87489583420047268 ) ) ;
#73193 = CARTESIAN_POINT ( 'NONE',  ( -7.500000000000015099, -73.00000000000001421, -255.0000000000000000 ) ) ;
#73194 = CARTESIAN_POINT ( 'NONE',  ( 10.00000000000000000, 59.46389618802034960, -49.70050353004825894 ) ) ;
#73195 = ORIENTED_EDGE ( 'NONE', *, *, #21306, .T. ) ;
#73197 = DIRECTION ( 'NONE',  ( 0.000000000000000000, 0.000000000000000000, 1.000000000000000000 ) ) ;
#73196 = AXIS2_PLACEMENT_3D ( 'NONE', #57182, #11664, #34604 ) ;
#73198 = CARTESIAN_POINT ( 'NONE',  ( 10.00000000000000000, -71.27951684758005513, -30.41916302227188851 ) ) ;
#73199 = CARTESIAN_POINT ( 'NONE',  ( 0.000000000000000000, 9.188173127307290855, 40.98264845739752360 ) ) ;
#73200 = VECTOR ( 'NONE', #3202, 1000.000000000000000 ) ;
#73201 = AXIS2_PLACEMENT_3D ( 'NONE', #48224, #42960, #60260 ) ;
#73202 = DIRECTION ( 'NONE',  ( 0.000000000000000000, 0.000000000000000000, 1.000000000000000000 ) ) ;
#73203 = CARTESIAN_POINT ( 'NONE',  ( 92.69370383062501162, -208.6684592857803011, 79.58864583420047722 ) ) ;
#73204 = ORIENTED_EDGE ( 'NONE', *, *, #63596, .F. ) ;
#73205 = ORIENTED_EDGE ( 'NONE', *, *, #4631, .F. ) ;
#73206 = CYLINDRICAL_SURFACE ( 'NONE', #41676, 77.49899999999999523 ) ;
#73207 = DIRECTION ( 'NONE',  ( -1.000000000000000000, -0.000000000000000000, -0.000000000000000000 ) ) ;
#73208 = LINE ( 'NONE', #61208, #5049 ) ;
#73209 = DIRECTION ( 'NONE',  ( 0.000000000000000000, 0.000000000000000000, 1.000000000000000000 ) ) ;
#73210 = CARTESIAN_POINT ( 'NONE',  ( 97.64999999999999147, -209.9999999999999716, 89.68250000000000455 ) ) ;
#73211 = AXIS2_PLACEMENT_3D ( 'NONE', #19805, #3299, #49497 ) ;
#73212 = ORIENTED_EDGE ( 'NONE', *, *, #65767, .F. ) ;
#73213 = EDGE_CURVE ( 'NONE', #62512, #54897, #68451, .T. ) ;
#73214 = FACE_OUTER_BOUND ( 'NONE', #21649, .T. ) ;
#73215 = EDGE_LOOP ( 'NONE', ( #36892, #61064, #58344, #15815 ) ) ;
#73216 = ORIENTED_EDGE ( 'NONE', *, *, #39498, .F. ) ;
#73217 = CARTESIAN_POINT ( 'NONE',  ( -5.565113727472255967, 10.17789316117534248, -44.99999999999998579 ) ) ;
#73218 = AXIS2_PLACEMENT_3D ( 'NONE', #68164, #49744, #26454 ) ;
#73219 = VECTOR ( 'NONE', #48300, 1000.000000000000000 ) ;
#73220 = EDGE_CURVE ( 'NONE', #64618, #41319, #19213, .T. ) ;
#73221 = CARTESIAN_POINT ( 'NONE',  ( 0.000000000000000000, 76.66974797899852945, -11.30684508768257679 ) ) ;
#73222 = CIRCLE ( 'NONE', #27622, 42.00000000000000000 ) ;
#73223 = VERTEX_POINT ( 'NONE', #6886 ) ;
#73224 = CARTESIAN_POINT ( 'NONE',  ( 10.00000000000000000, -17.28742895386139722, 75.54627589209937355 ) ) ;
#73225 = CARTESIAN_POINT ( 'NONE',  ( 95.00000000000000000, -206.9400435732949575, 78.49062500173430124 ) ) ;
#73226 = EDGE_CURVE ( 'NONE', #50178, #46694, #36022, .T. ) ;
#73227 = CARTESIAN_POINT ( 'NONE',  ( 97.64999999999999147, 90.00000000000002842, 82.69749999999999091 ) ) ;
#73228 = ORIENTED_EDGE ( 'NONE', *, *, #72887, .F. ) ;
#73229 = DIRECTION ( 'NONE',  ( 0.000000000000000000, 0.000000000000000000, 1.000000000000000000 ) ) ;
#73230 = ORIENTED_EDGE ( 'NONE', *, *, #67013, .T. ) ;
#73231 = CARTESIAN_POINT ( 'NONE',  ( 92.35004305005917047, 91.53000306831577859, 81.13645661577284329 ) ) ;
#73232 = EDGE_LOOP ( 'NONE', ( #39573, #57333, #40045, #23302 ) ) ;
#73233 = DIRECTION ( 'NONE',  ( 0.000000000000000000, -0.7431448254773954654, -0.6691306063588569053 ) ) ;
#73234 = EDGE_CURVE ( 'NONE', #6931, #33091, #64596, .T. ) ;
#73235 = CARTESIAN_POINT ( 'NONE',  ( -97.30629616937501680, 90.00000000000004263, 85.35656250086715602 ) ) ;
#73236 = CARTESIAN_POINT ( 'NONE',  ( 97.30629616937498838, 90.00000000000002842, 79.16531250086714522 ) ) ;
#73237 = ORIENTED_EDGE ( 'NONE', *, *, #56753, .F. ) ;
#73238 = DIRECTION ( 'NONE',  ( -1.000000000000000000, 0.000000000000000000, 0.000000000000000000 ) ) ;
#73239 = CYLINDRICAL_SURFACE ( 'NONE', #29276, 31.99999999999998579 ) ;
#73240 = CARTESIAN_POINT ( 'NONE',  ( 10.00000000000000000, 0.000000000000000000, 0.000000000000000000 ) ) ;
#73241 = CARTESIAN_POINT ( 'NONE',  ( -0.0004442498558709490585, 0.001194404164628348752, 127.4927882439603195 ) ) ;
#73242 = ORIENTED_EDGE ( 'NONE', *, *, #45434, .F. ) ;
#73243 = CARTESIAN_POINT ( 'NONE',  ( 92.69370383062501162, -209.9999999999999716, 89.80156250086714920 ) ) ;
#73244 = CARTESIAN_POINT ( 'NONE',  ( -96.15314808468745866, -211.9973110713294489, 81.49364583420047836 ) ) ;
#73245 = EDGE_LOOP ( 'NONE', ( #60910, #30888, #46438, #64297 ) ) ;
#73246 = VERTEX_POINT ( 'NONE', #35815 ) ;
#73247 = FACE_OUTER_BOUND ( 'NONE', #53951, .T. ) ;
#73248 = VERTEX_POINT ( 'NONE', #17790 ) ;
#73249 = DIRECTION ( 'NONE',  ( -0.000000000000000000, -0.000000000000000000, 1.000000000000000000 ) ) ;
#73250 = CARTESIAN_POINT ( 'NONE',  ( 93.67499999999998295, 92.29496732002878900, 88.06854166840095388 ) ) ;
#73251 = VERTEX_POINT ( 'NONE', #46377 ) ;
#73252 = CARTESIAN_POINT ( 'NONE',  ( -97.30629616937495996, -209.9999999999999716, 76.30781250086714351 ) ) ;
#73253 = ORIENTED_EDGE ( 'NONE', *, *, #63837, .T. ) ;
#73254 = LINE ( 'NONE', #22139, #24279 ) ;
#73255 = CARTESIAN_POINT ( 'NONE',  ( -99.99999999999998579, -124.0000000000000284, 39.99999999999996447 ) ) ;
#73256 = CARTESIAN_POINT ( 'NONE',  ( -25.50183398199384754, -112.6408924756582053, 5.500000000000000000 ) ) ;
#73257 = CARTESIAN_POINT ( 'NONE',  ( -30.50000000000000000, -120.0000000000000000, 2.500000000000000000 ) ) ;
#73258 = CIRCLE ( 'NONE', #50452, 77.49899999999999523 ) ;
#73259 = DIRECTION ( 'NONE',  ( 0.9918136447140104561, -0.1276937514489679681, 0.000000000000000000 ) ) ;
#73260 = VECTOR ( 'NONE', #23538, 1000.000000000000000 ) ;
#73261 = EDGE_CURVE ( 'NONE', #39405, #36301, #3630, .T. ) ;
#73262 = EDGE_CURVE ( 'NONE', #56886, #33390, #923, .T. ) ;
#73263 = DIRECTION ( 'NONE',  ( -1.000000000000000000, 0.000000000000000000, 0.000000000000000000 ) ) ;
#73265 = CARTESIAN_POINT ( 'NONE',  ( 93.84685191531248449, 88.00268892867053694, 89.11364583420048291 ) ) ;
#73264 = AXIS2_PLACEMENT_3D ( 'NONE', #37930, #26637, #48827 ) ;
#73266 = DIRECTION ( 'NONE',  ( -0.000000000000000000, -0.000000000000000000, -1.000000000000000000 ) ) ;
#73267 = CARTESIAN_POINT ( 'NONE',  ( 93.67499999999999716, 87.70503267997126784, 81.29520833506762756 ) ) ;
#73268 = LINE ( 'NONE', #43344, #52877 ) ;
#73269 = DIRECTION ( 'NONE',  ( 0.000000000000000000, -0.5877852522924801315, 0.8090169943749421222 ) ) ;
#73270 = DIRECTION ( 'NONE',  ( 0.000000000000000000, 0.000000000000000000, -1.000000000000000000 ) ) ;
#73271 = CARTESIAN_POINT ( 'NONE',  ( 15.00000000000000000, 0.000000000000000000, 0.000000000000000000 ) ) ;
#73272 = CARTESIAN_POINT ( 'NONE',  ( 92.34999999999999432, 90.00000000000002842, 77.29999999999999716 ) ) ;
#73273 = EDGE_CURVE ( 'NONE', #24045, #26445, #13203, .T. ) ;
#73274 = DIRECTION ( 'NONE',  ( -1.000000000000000000, -0.000000000000000000, -0.000000000000000000 ) ) ;
#73275 = DIRECTION ( 'NONE',  ( -1.000000000000000000, 0.000000000000000000, 0.000000000000000000 ) ) ;
#73276 = CIRCLE ( 'NONE', #1319, 31.99999999999999289 ) ;
#73277 = LINE ( 'NONE', #39085, #42174 ) ;
#73278 = DIRECTION ( 'NONE',  ( -0.000000000000000000, 0.8090169943749491166, 0.5877852522924709167 ) ) ;
#73279 = AXIS2_PLACEMENT_3D ( 'NONE', #67332, #71843, #55681 ) ;
#73280 = LINE ( 'NONE', #61647, #47881 ) ;
#73281 = CARTESIAN_POINT ( 'NONE',  ( -97.64999999999994884, -211.5299782133524502, 85.60791666666665378 ) ) ;
#73282 = AXIS2_PLACEMENT_3D ( 'NONE', #26042, #65544, #71900 ) ;
#73283 = CARTESIAN_POINT ( 'NONE',  ( 10.00000000000000000, 16.00000000000000000, -2.500000000000000000 ) ) ;
#73284 = DIRECTION ( 'NONE',  ( -1.000000000000000000, 0.000000000000000000, 0.000000000000000000 ) ) ;
#73285 = DIRECTION ( 'NONE',  ( 0.000000000000000000, 0.000000000000000000, 1.000000000000000000 ) ) ;
#73286 = CYLINDRICAL_SURFACE ( 'NONE', #51462, 42.00000000000000000 ) ;
#73287 = CARTESIAN_POINT ( 'NONE',  ( 92.34999999999999432, 90.00000000000002842, 81.74500000000000455 ) ) ;
#73288 = CARTESIAN_POINT ( 'NONE',  ( 97.30629616937498838, -209.9999999999999716, 74.72031250086713783 ) ) ;
#73289 = ORIENTED_EDGE ( 'NONE', *, *, #63826, .F. ) ;
#73290 = ORIENTED_EDGE ( 'NONE', *, *, #15029, .T. ) ;
#73291 = FACE_OUTER_BOUND ( 'NONE', #30651, .T. ) ;
#73292 = VERTEX_POINT ( 'NONE', #52374 ) ;
#73293 = CARTESIAN_POINT ( 'NONE',  ( 97.30629616937498838, -209.9999999999999716, 77.26031250086714408 ) ) ;
#73294 = ORIENTED_EDGE ( 'NONE', *, *, #64663, .F. ) ;
#73295 = CARTESIAN_POINT ( 'NONE',  ( 92.69370383062501162, -209.9999999999999716, 83.45156250086715488 ) ) ;
#73296 = AXIS2_PLACEMENT_3D ( 'NONE', #72070, #38615, #37137 ) ;
#73297 = ORIENTED_EDGE ( 'NONE', *, *, #4766, .F. ) ;
#73298 = EDGE_CURVE ( 'NONE', #21360, #19317, #43243, .T. ) ;
#73299 = CARTESIAN_POINT ( 'NONE',  ( -7.400000000000022560, 2.533442343334467755E-13, 23.49999999999998934 ) ) ;
#73300 = VERTEX_POINT ( 'NONE', #47485 ) ;
#73301 = AXIS2_PLACEMENT_3D ( 'NONE', #550, #24546, #64784 ) ;
#73302 = DIRECTION ( 'NONE',  ( -3.061616997868382648E-16, -1.000000000000000000, 0.000000000000000000 ) ) ;
#73303 = EDGE_CURVE ( 'NONE', #67626, #43336, #22834, .T. ) ;
#73304 = ORIENTED_EDGE ( 'NONE', *, *, #47985, .T. ) ;
#73305 = CARTESIAN_POINT ( 'NONE',  ( 0.000000000000000000, -120.0000000000000000, 40.00000000000000711 ) ) ;
#73306 = ORIENTED_EDGE ( 'NONE', *, *, #20456, .T. ) ;
#73307 = CARTESIAN_POINT ( 'NONE',  ( 10.00000000000000000, -27.05870788708213226, -26.08949754953053102 ) ) ;
#73308 = FACE_OUTER_BOUND ( 'NONE', #11625, .T. ) ;
#73309 = EDGE_CURVE ( 'NONE', #19670, #66145, #29073, .T. ) ;
#73310 = VERTEX_POINT ( 'NONE', #23810 ) ;
#73311 = CARTESIAN_POINT ( 'NONE',  ( 0.000000000000000000, 0.000000000000000000, 0.000000000000000000 ) ) ;
#73312 = VERTEX_POINT ( 'NONE', #18893 ) ;
#73313 = CARTESIAN_POINT ( 'NONE',  ( 0.000000000000000000, 31.47745569255140552, 68.26794271651274926 ) ) ;
#73314 = EDGE_CURVE ( 'NONE', #15341, #1614, #4819, .T. ) ;
#73315 = ORIENTED_EDGE ( 'NONE', *, *, #66046, .T. ) ;
#73316 = AXIS2_PLACEMENT_3D ( 'NONE', #72516, #54502, #20659 ) ;
#73317 = EDGE_CURVE ( 'NONE', #32442, #21322, #28828, .T. ) ;
#73318 = ORIENTED_EDGE ( 'NONE', *, *, #59661, .T. ) ;
#73319 = ORIENTED_EDGE ( 'NONE', *, *, #56951, .T. ) ;
#73320 = CARTESIAN_POINT ( 'NONE',  ( 95.00000000000000000, -207.3369185715606307, 76.78406250086712248 ) ) ;
#73321 = CIRCLE ( 'NONE', #6115, 16.00000000000000000 ) ;
#73322 = CARTESIAN_POINT ( 'NONE',  ( 6.782329983125270800, 10.49999999999999467, -145.0000000000000000 ) ) ;
#73323 = EDGE_LOOP ( 'NONE', ( #193, #55386, #17749, #62846 ) ) ;
#73324 = AXIS2_PLACEMENT_3D ( 'NONE', #16951, #56435, #68077 ) ;
#73325 = VERTEX_POINT ( 'NONE', #36933 ) ;
#73326 = ORIENTED_EDGE ( 'NONE', *, *, #50432, .F. ) ;
#73327 = FACE_BOUND ( 'NONE', #61824, .T. ) ;
#73328 = VECTOR ( 'NONE', #5260, 1000.000000000000000 ) ;
#73329 = DIRECTION ( 'NONE',  ( -1.000000000000000000, -0.000000000000000000, 0.000000000000000000 ) ) ;
#73330 = ADVANCED_FACE ( 'NONE', ( #65159 ), #71874, .T. ) ;
#73331 = CARTESIAN_POINT ( 'NONE',  ( -93.67500000000003979, 87.70503267997129626, 89.57666666666666799 ) ) ;
#73332 = ADVANCED_FACE ( 'NONE', ( #55983 ), #54602, .F. ) ;
#73333 = VERTEX_POINT ( 'NONE', #24915 ) ;
#73334 = CARTESIAN_POINT ( 'NONE',  ( 92.69370383062498320, 88.66845928578037217, 76.36072916753381890 ) ) ;
#73335 = ORIENTED_EDGE ( 'NONE', *, *, #35627, .F. ) ;
#73336 = DIRECTION ( 'NONE',  ( 1.000000000000000000, 0.000000000000000000, 0.000000000000000000 ) ) ;
#73337 = CARTESIAN_POINT ( 'NONE',  ( -93.84685191531247028, -211.9973110713294489, 88.58447916753381435 ) ) ;
#73338 = VERTEX_POINT ( 'NONE', #7995 ) ;
#73339 = CARTESIAN_POINT ( 'NONE',  ( 4.088737910769899564, -3.412868758467433317, -1.160540885688329249 ) ) ;
#73340 = CARTESIAN_POINT ( 'NONE',  ( 11.99999999999999822, -14.66109333815410487, -73.73191006444587003 ) ) ;
#73341 = DIRECTION ( 'NONE',  ( -1.000000000000000000, -0.000000000000000000, -0.000000000000000000 ) ) ;
#73342 = CARTESIAN_POINT ( 'NONE',  ( -97.30629616937497417, -211.3315407142195852, 78.26572916753380582 ) ) ;
#73343 = CARTESIAN_POINT ( 'NONE',  ( -97.64999999999996305, -209.9999999999999716, 83.65000000000000568 ) ) ;
#73344 = CARTESIAN_POINT ( 'NONE',  ( 10.00000000000000000, 0.000000000000000000, 0.000000000000000000 ) ) ;
#73345 = DIRECTION ( 'NONE',  ( 0.000000000000000000, 0.6691306063588563502, 0.7431448254773960205 ) ) ;
#73346 = ORIENTED_EDGE ( 'NONE', *, *, #28259, .T. ) ;
#73347 = ADVANCED_FACE ( 'NONE', ( #27401 ), #63628, .T. ) ;
#73348 = EDGE_CURVE ( 'NONE', #67308, #38997, #8393, .T. ) ;
#73349 = VERTEX_POINT ( 'NONE', #14377 ) ;
#73350 = CYLINDRICAL_SURFACE ( 'NONE', #25256, 2.649999999999985700 ) ;
#73351 = DIRECTION ( 'NONE',  ( -1.000000000000000000, 0.000000000000000000, 0.000000000000000000 ) ) ;
#73352 = CARTESIAN_POINT ( 'NONE',  ( 93.86969025972541658, -207.8557763824826168, 74.86230178910948041 ) ) ;
#73353 = CARTESIAN_POINT ( 'NONE',  ( -96.15314808468751551, 88.00268892867056536, 80.22364583420046813 ) ) ;
#73354 = CARTESIAN_POINT ( 'NONE',  ( 10.00000000000000000, -77.32052557432837148, -5.256550761633697277 ) ) ;
#73355 = LINE ( 'NONE', #9468, #14554 ) ;
#73356 = EDGE_LOOP ( 'NONE', ( #72837, #72746 ) ) ;
#73357 = DIRECTION ( 'NONE',  ( 1.000000000000000000, -0.000000000000000000, -0.000000000000000000 ) ) ;
#73358 = VECTOR ( 'NONE', #72704, 1000.000000000000000 ) ;
#73359 = AXIS2_PLACEMENT_3D ( 'NONE', #6952, #52830, #57735 ) ;
#73360 = CIRCLE ( 'NONE', #40970, 42.00000000000000000 ) ;
#73361 = LINE ( 'NONE', #27504, #62901 ) ;
#73362 = CARTESIAN_POINT ( 'NONE',  ( -2.499999999999965361, 90.00000000000000000, -310.0000000000000000 ) ) ;
#73363 = CARTESIAN_POINT ( 'NONE',  ( 0.000000000000000000, -37.48860685352290290, -0.8828120875904512665 ) ) ;
#73364 = CARTESIAN_POINT ( 'NONE',  ( -0.1714266706912549731, 5.674529457426383594, -1.878862934774786275 ) ) ;
#73365 = CARTESIAN_POINT ( 'NONE',  ( 97.64999999999997726, -210.0000085086476531, 88.49187470744953998 ) ) ;
#73366 = CARTESIAN_POINT ( 'NONE',  ( -97.30629616937497417, -211.3315407142195852, 79.05947916753382287 ) ) ;
#73367 = DIRECTION ( 'NONE',  ( -1.000000000000000000, -0.000000000000000000, 0.000000000000000000 ) ) ;
#73368 =( BOUNDED_CURVE ( )  B_SPLINE_CURVE ( 2, ( #46241, #62053, #73682, #45135, #16549, #34212, #21819 ),
 .UNSPECIFIED., .F., .F. ) 
 B_SPLINE_CURVE_WITH_KNOTS ( ( 3, 2, 2, 3 ),
 ( 0.2499999999999995837, 0.2569444444444442532, 0.2638888888888890061, 0.2708333333333337034 ),
 .UNSPECIFIED. ) 
 CURVE ( )  GEOMETRIC_REPRESENTATION_ITEM ( )  RATIONAL_B_SPLINE_CURVE ( ( 1.000000000000007994, 0.8660254037844307140, 1.000000000000000000, 0.8660254037844387076, 1.000000000000000000, 0.8660254037844311581, 1.000000000000007550 ) ) 
 REPRESENTATION_ITEM ( '' )  );
#73369 = VERTEX_POINT ( 'NONE', #53493 ) ;
#73370 = CARTESIAN_POINT ( 'NONE',  ( 0.000000000000000000, 0.000000000000000000, 52.00000000000002132 ) ) ;
#73371 = DIRECTION ( 'NONE',  ( -1.000000000000000000, 0.000000000000000000, 0.000000000000000000 ) ) ;
#73372 = DIRECTION ( 'NONE',  ( 0.000000000000000000, 0.000000000000000000, 1.000000000000000000 ) ) ;
#73373 = ORIENTED_EDGE ( 'NONE', *, *, #53370, .F. ) ;
#73374 = CARTESIAN_POINT ( 'NONE',  ( 1.560000000000000053, 0.8660254037844389297, 1.500000000000000000 ) ) ;
#73375 = CARTESIAN_POINT ( 'NONE',  ( 10.00000000000000000, -12.93880638057369659, 76.41127070299266677 ) ) ;
#73376 = AXIS2_PLACEMENT_3D ( 'NONE', #7254, #51249, #57275 ) ;
#73377 = CIRCLE ( 'NONE', #4990, 32.00000000000000000 ) ;
#73378 = AXIS2_PLACEMENT_3D ( 'NONE', #32128, #44171, #49791 ) ;
#73379 = CARTESIAN_POINT ( 'NONE',  ( -7.400000000000003908, -1.056673655988042765E-14, -5.892267102755452808E-15 ) ) ;
#73380 = ORIENTED_EDGE ( 'NONE', *, *, #53884, .T. ) ;
#73381 = EDGE_CURVE ( 'NONE', #63204, #37924, #17996, .T. ) ;
#73382 = CARTESIAN_POINT ( 'NONE',  ( 0.000000000000000000, -77.16300072079641836, -27.74655509720752278 ) ) ;
#73383 = CARTESIAN_POINT ( 'NONE',  ( 0.000000000000000000, -28.89263327155795480, 71.91182617369177876 ) ) ;
#73384 = VERTEX_POINT ( 'NONE', #47845 ) ;
#73385 = EDGE_CURVE ( 'NONE', #70635, #27457, #26019, .T. ) ;
#73386 = DIRECTION ( 'NONE',  ( 0.000000000000000000, -0.8660254037844437036, 0.4999999999999913403 ) ) ;
#73387 = CARTESIAN_POINT ( 'NONE',  ( 10.00000000000000000, -22.90783923731686045, 78.73519480814947258 ) ) ;
#73388 = ORIENTED_EDGE ( 'NONE', *, *, #4442, .T. ) ;
#73389 = EDGE_CURVE ( 'NONE', #18663, #68106, #37323, .T. ) ;
#73390 = CARTESIAN_POINT ( 'NONE',  ( -7.499999999999968914, 79.99999999999998579, -269.9999999999999432 ) ) ;
#73391 = VERTEX_POINT ( 'NONE', #59510 ) ;
#73392 = CARTESIAN_POINT ( 'NONE',  ( -92.35000000010064980, -209.9999769027738239, 83.41187580057901130 ) ) ;
#73393 = ORIENTED_EDGE ( 'NONE', *, *, #58664, .F. ) ;
#73394 = CARTESIAN_POINT ( 'NONE',  ( 96.32499999999998863, -212.2949673200287179, 81.95666666666666345 ) ) ;
#73395 = ORIENTED_EDGE ( 'NONE', *, *, #68842, .F. ) ;
#73396 = EDGE_CURVE ( 'NONE', #51872, #27944, #71135, .T. ) ;
#73397 = ORIENTED_EDGE ( 'NONE', *, *, #56882, .F. ) ;
#73398 = EDGE_LOOP ( 'NONE', ( #46546, #53947, #9405, #2111 ) ) ;
#73399 = DIRECTION ( 'NONE',  ( -7.632783294297813165E-16, -1.065814103640131188E-14, -1.000000000000000000 ) ) ;
#73400 = VERTEX_POINT ( 'NONE', #70770 ) ;
#73401 = PRODUCT ( 'Input Shaft', 'Input Shaft', '', ( #18495 ) ) ;
#73402 = ORIENTED_EDGE ( 'NONE', *, *, #30225, .F. ) ;
#73403 = CARTESIAN_POINT ( 'NONE',  ( 94.99999999999998579, 92.66308142843935514, 77.57781250086715374 ) ) ;
#73404 = CARTESIAN_POINT ( 'NONE',  ( 5.000000000000002665, 39.47590169984846398, 71.87247863392428826 ) ) ;
#73405 = EDGE_CURVE ( 'NONE', #50832, #1159, #37263, .T. ) ;
#73406 = DIRECTION ( 'NONE',  ( -7.943659481576819828E-16, -1.065814103640131188E-14, -1.000000000000000000 ) ) ;
#73407 = ORIENTED_EDGE ( 'NONE', *, *, #4457, .T. ) ;
#73408 = ORIENTED_EDGE ( 'NONE', *, *, #19660, .F. ) ;
#73409 = AXIS2_PLACEMENT_3D ( 'NONE', #71485, #14357, #37308 ) ;
#73410 = ORIENTED_EDGE ( 'NONE', *, *, #67815, .T. ) ;
#73411 = CARTESIAN_POINT ( 'NONE',  ( -92.35000000000003695, 90.00000000000004263, 89.68250000000000455 ) ) ;
#73412 = VECTOR ( 'NONE', #49512, 1000.000000000000000 ) ;
#73413 = ORIENTED_EDGE ( 'NONE', *, *, #68089, .T. ) ;
#73414 = CARTESIAN_POINT ( 'NONE',  ( 92.69370383062501162, -209.9999999999999716, 86.46781250086714010 ) ) ;
#73415 = SHAPE_DEFINITION_REPRESENTATION ( #5014, #31117 ) ;
#73416 = DIRECTION ( 'NONE',  ( -1.000000000000000000, -0.000000000000000000, -0.000000000000000000 ) ) ;
#73418 = DIRECTION ( 'NONE',  ( 0.000000000000000000, 0.000000000000000000, 1.000000000000000000 ) ) ;
#73417 = AXIS2_PLACEMENT_3D ( 'NONE', #63956, #832, #47029 ) ;
#73419 = PLANE ( 'NONE',  #70117 ) ;
#73420 = DIRECTION ( 'NONE',  ( -1.000000000000000000, 0.000000000000000000, 0.000000000000000000 ) ) ;
#73421 = FACE_OUTER_BOUND ( 'NONE', #53668, .T. ) ;
#73422 = CARTESIAN_POINT ( 'NONE',  ( 92.34999999999999432, 90.00000929204269084, 84.99937468035462018 ) ) ;
#73423 = CARTESIAN_POINT ( 'NONE',  ( -93.84685191531247028, -211.9973110713294489, 86.67947916753381321 ) ) ;
#73424 = EDGE_CURVE ( 'NONE', #8256, #63525, #73268, .T. ) ;
#73425 = CARTESIAN_POINT ( 'NONE',  ( -95.00000000000002842, 87.33691857156074434, 85.51531250086713953 ) ) ;
#73426 = VECTOR ( 'NONE', #36720, 1000.000000000000000 ) ;
#73427 = EDGE_CURVE ( 'NONE', #56348, #17276, #38498, .T. ) ;
#73428 = ORIENTED_EDGE ( 'NONE', *, *, #24022, .F. ) ;
#73430 = CARTESIAN_POINT ( 'NONE',  ( -97.30629616937501680, 88.66845928578038638, 85.88572916753382458 ) ) ;
#73429 = CARTESIAN_POINT ( 'NONE',  ( 92.69370383062498320, 88.66845928578037217, 89.06072916753379332 ) ) ;
#73431 = VERTEX_POINT ( 'NONE', #8373 ) ;
#73432 = FACE_OUTER_BOUND ( 'NONE', #66916, .T. ) ;
#73433 = DIRECTION ( 'NONE',  ( 0.000000000000000000, 0.000000000000000000, 1.000000000000000000 ) ) ;
#73434 = CARTESIAN_POINT ( 'NONE',  ( 10.00000000000000000, 37.16516213103277977, 4.992566952385115719 ) ) ;
#73435 = CARTESIAN_POINT ( 'NONE',  ( 10.00000000000000000, 0.000000000000000000, 0.000000000000000000 ) ) ;
#73436 = CARTESIAN_POINT ( 'NONE',  ( -96.15314808468745866, -211.9973110713294489, 88.47864583420047779 ) ) ;
#73437 = CARTESIAN_POINT ( 'NONE',  ( 96.32499999999998863, -207.7050326799711968, 82.16833333333332234 ) ) ;
#73438 = CARTESIAN_POINT ( 'NONE',  ( 26.00000000000000355, 3.334407072378456173E-16, -2.445500000000000007 ) ) ;
#73439 = DIRECTION ( 'NONE',  ( -1.000000000000000000, -0.000000000000000000, -0.000000000000000000 ) ) ;
#73440 = CARTESIAN_POINT ( 'NONE',  ( 0.000000000000000000, 0.000000000000000000, 0.000000000000000000 ) ) ;
#73441 = ORIENTED_EDGE ( 'NONE', *, *, #44071, .T. ) ;
#73442 = AXIS2_PLACEMENT_3D ( 'NONE', #34495, #69093, #10837 ) ;
#73443 = VERTEX_POINT ( 'NONE', #54243 ) ;
#73444 = TOROIDAL_SURFACE ( 'NONE', #54255, 18.00000000000000000, 3.300000000000000266 ) ;
#73445 = CARTESIAN_POINT ( 'NONE',  ( -93.67500000000003979, 87.70503267997129626, 80.68666666666665321 ) ) ;
#73446 = DIRECTION ( 'NONE',  ( 2.603472992746261562E-14, 2.546204323184492723E-14, -1.000000000000000000 ) ) ;
#73447 = CARTESIAN_POINT ( 'NONE',  ( 93.67500000000001137, -207.7050326799711968, 75.92416666666666458 ) ) ;
#73448 = CYLINDRICAL_SURFACE ( 'NONE', #60038, 16.00000000000000000 ) ;
#73449 = CARTESIAN_POINT ( 'NONE',  ( -94.99999999999997158, -213.0599564267049857, 76.90312500173429555 ) ) ;
#73450 = CYLINDRICAL_SURFACE ( 'NONE', #55566, 16.00000000000000000 ) ;
#73451 = CARTESIAN_POINT ( 'NONE',  ( 10.00000000000000000, -75.11725578898466438, -2.956366410621452001 ) ) ;
#73452 = LINE ( 'NONE', #74200, #66036 ) ;
#73453 = ORIENTED_EDGE ( 'NONE', *, *, #41370, .F. ) ;
#73454 = CARTESIAN_POINT ( 'NONE',  ( -96.15314808468751551, 88.00268892867056536, 80.22364583420046813 ) ) ;
#73455 = LINE ( 'NONE', #50900, #48753 ) ;
#73456 = CARTESIAN_POINT ( 'NONE',  ( 10.00000000000000000, 0.000000000000000000, 0.000000000000000000 ) ) ;
#73457 = CARTESIAN_POINT ( 'NONE',  ( 10.00000000000000000, 68.27212725128275395, 31.46837873495001503 ) ) ;
#73458 = CARTESIAN_POINT ( 'NONE',  ( -2.981742216678212820, 1.885622467846870828E-15, 15.39727592608509177 ) ) ;
#73459 = CARTESIAN_POINT ( 'NONE',  ( 2.500000000000043965, 65.00000000000000000, -290.0000000000000568 ) ) ;
#73460 = CARTESIAN_POINT ( 'NONE',  ( -97.30629616937497417, -211.3315407142195852, 87.94947916753382344 ) ) ;
#73461 = EDGE_CURVE ( 'NONE', #64387, #28018, #39685, .T. ) ;
#73462 = AXIS2_PLACEMENT_3D ( 'NONE', #68694, #39000, #63422 ) ;
#73463 = CARTESIAN_POINT ( 'NONE',  ( 92.69370383062498320, 88.66845928578035796, 80.32947916753381890 ) ) ;
#73464 = CARTESIAN_POINT ( 'NONE',  ( -93.84685191531248449, -208.0026889286704943, 80.06489583420048461 ) ) ;
#73465 = CARTESIAN_POINT ( 'NONE',  ( -92.35000000000003695, 89.99999988321006583, 84.68187499741277691 ) ) ;
#73466 = EDGE_LOOP ( 'NONE', ( #530, #54038, #68806, #55594 ) ) ;
#73467 =( GEOMETRIC_REPRESENTATION_CONTEXT ( 3 ) GLOBAL_UNCERTAINTY_ASSIGNED_CONTEXT ( ( #37435 ) ) GLOBAL_UNIT_ASSIGNED_CONTEXT ( ( #51404, #39024, #61961 ) ) REPRESENTATION_CONTEXT ( 'NONE', 'WORKASPACE' ) );
#73468 = CIRCLE ( 'NONE', #18256, 31.99999999999998579 ) ;
#73469 = CYLINDRICAL_SURFACE ( 'NONE', #47848, 32.00000000000000000 ) ;
#73470 = CARTESIAN_POINT ( 'NONE',  ( 92.34999999999999432, 91.52997821335252127, 85.58145833506763722 ) ) ;
#73471 = AXIS2_PLACEMENT_3D ( 'NONE', #4223, #33888, #67734 ) ;
#73472 = ADVANCED_FACE ( 'NONE', ( #66264 ), #10119, .T. ) ;
#73473 = CARTESIAN_POINT ( 'NONE',  ( -97.30629616937501680, 88.66845928578038638, 78.42447916753380355 ) ) ;
#73474 = CARTESIAN_POINT ( 'NONE',  ( 95.00000000000000000, -207.3369185715606307, 79.95906250086713385 ) ) ;
#73475 = VERTEX_POINT ( 'NONE', #71505 ) ;
#73476 = EDGE_CURVE ( 'NONE', #45237, #26049, #20002, .T. ) ;
#73477 = VECTOR ( 'NONE', #14446, 1000.000000000000000 ) ;
#73478 = FACE_OUTER_BOUND ( 'NONE', #34958, .T. ) ;
#73479 = VERTEX_POINT ( 'NONE', #30546 ) ;
#73480 = VECTOR ( 'NONE', #29489, 1000.000000000000000 ) ;
#73481 = CARTESIAN_POINT ( 'NONE',  ( -97.64999999999994884, -210.0000065184970026, 88.17437522718661569 ) ) ;
#73482 = VERTEX_POINT ( 'NONE', #11591 ) ;
#73483 = EDGE_CURVE ( 'NONE', #16194, #52621, #17253, .T. ) ;
#73484 = VECTOR ( 'NONE', #69796, 1000.000000000000000 ) ;
#73485 = CYLINDRICAL_SURFACE ( 'NONE', #8138, 82.00000000000000000 ) ;
#73486 = VECTOR ( 'NONE', #47839, 1000.000000000000114 ) ;
#73487 = ORIENTED_EDGE ( 'NONE', *, *, #32496, .T. ) ;
#73488 = EDGE_LOOP ( 'NONE', ( #35316, #23166, #56359, #8101 ) ) ;
#73489 = ORIENTED_EDGE ( 'NONE', *, *, #44136, .F. ) ;
#73490 = DIRECTION ( 'NONE',  ( -1.000000000000000000, 0.000000000000000000, 0.000000000000000000 ) ) ;
#73491 = ORIENTED_EDGE ( 'NONE', *, *, #9075, .F. ) ;
#73492 = CARTESIAN_POINT ( 'NONE',  ( 5.000000000000000000, 31.52238457039599595, 27.75498641678753842 ) ) ;
#73493 = CARTESIAN_POINT ( 'NONE',  ( 96.32499999999998863, -212.2949673200287179, 83.86166666666666458 ) ) ;
#73494 = CARTESIAN_POINT ( 'NONE',  ( 96.15314808468748708, 88.00268892867053694, 88.10822916753382117 ) ) ;
#73495 = ADVANCED_FACE ( 'NONE', ( #23269 ), #46201, .F. ) ;
#73496 = CARTESIAN_POINT ( 'NONE',  ( -11.99999999999999645, 0.000000000000000000, 0.000000000000000000 ) ) ;
#73497 = CARTESIAN_POINT ( 'NONE',  ( 92.35000000000002274, -208.4700217866474645, 77.88208333333332689 ) ) ;
#73498 = EDGE_LOOP ( 'NONE', ( #35961, #32884, #41777, #10155 ) ) ;
#73499 = EDGE_LOOP ( 'NONE', ( #58637, #72400, #27339, #47353 ) ) ;
#73500 = ORIENTED_EDGE ( 'NONE', *, *, #44492, .T. ) ;
#73501 = ORIENTED_EDGE ( 'NONE', *, *, #46456, .T. ) ;
#73502 = PLANE ( 'NONE',  #55009 ) ;
#73503 = LINE ( 'NONE', #27264, #17520 ) ;
#73504 = CARTESIAN_POINT ( 'NONE',  ( 10.00000000000000000, -10.74501242461308159, 35.92658777277507909 ) ) ;
#73505 = CARTESIAN_POINT ( 'NONE',  ( 0.000000000000000000, 0.000000000000000000, -1.466666666666671670 ) ) ;
#73506 = DIRECTION ( 'NONE',  ( -0.000000000000000000, -0.000000000000000000, 1.000000000000000000 ) ) ;
#73507 = CARTESIAN_POINT ( 'NONE',  ( 0.000000000000000000, 71.27951684758026829, 30.41916302227139113 ) ) ;
#73508 = VERTEX_POINT ( 'NONE', #11972 ) ;
#73509 = CARTESIAN_POINT ( 'NONE',  ( -92.34999999999999432, -208.4700217866474645, 83.46479166840096298 ) ) ;
#73511 = VERTEX_POINT ( 'NONE', #68765 ) ;
#73510 = EDGE_CURVE ( 'NONE', #70258, #70635, #15689, .T. ) ;
#73512 = CYLINDRICAL_SURFACE ( 'NONE', #24302, 42.00000000000000000 ) ;
#73513 = EDGE_CURVE ( 'NONE', #72289, #30548, #49264, .T. ) ;
#73514 = ORIENTED_EDGE ( 'NONE', *, *, #60095, .F. ) ;
#73516 = CARTESIAN_POINT ( 'NONE',  ( -93.67500000000003979, 92.29496732002878900, 83.51770833506763836 ) ) ;
#73515 = CARTESIAN_POINT ( 'NONE',  ( 92.34999999999999432, 88.47002178664753558, 82.51229166840094820 ) ) ;
#73518 = EDGE_CURVE ( 'NONE', #10549, #70108, #54064, .T. ) ;
#73517 = VERTEX_POINT ( 'NONE', #28517 ) ;
#73519 = CARTESIAN_POINT ( 'NONE',  ( 97.30629616937498838, 91.33154071421968467, 84.45697916753383083 ) ) ;
#73520 = CARTESIAN_POINT ( 'NONE',  ( -97.65000000000001990, 90.00000000000004263, 76.03000000000000114 ) ) ;
#73521 = DIRECTION ( 'NONE',  ( 0.000000000000000000, 0.000000000000000000, 1.000000000000000000 ) ) ;
#73522 = DIRECTION ( 'NONE',  ( 0.000000000000000000, 0.000000000000000000, 1.000000000000000000 ) ) ;
#73523 = DIRECTION ( 'NONE',  ( -1.000000000000000000, 0.000000000000000000, 0.000000000000000000 ) ) ;
#73524 = PLANE ( 'NONE',  #73153 ) ;
#73525 = ORIENTED_EDGE ( 'NONE', *, *, #37117, .T. ) ;
#73526 = CARTESIAN_POINT ( 'NONE',  ( 10.00000000000000000, -12.26510123303284594, 35.53030884539080603 ) ) ;
#73527 = DIRECTION ( 'NONE',  ( 0.000000000000000000, -0.9945218953682740670, -0.1045284632676459352 ) ) ;
#73528 = FACE_OUTER_BOUND ( 'NONE', #36798, .T. ) ;
#73529 = ORIENTED_EDGE ( 'NONE', *, *, #47750, .F. ) ;
#73530 = AXIS2_PLACEMENT_3D ( 'NONE', #29488, #35514, #22771 ) ;
#73531 = ORIENTED_EDGE ( 'NONE', *, *, #11857, .T. ) ;
#73532 = AXIS2_PLACEMENT_3D ( 'NONE', #34161, #46192, #11584 ) ;
#73533 = CARTESIAN_POINT ( 'NONE',  ( 11.99999999999999822, -8.830959090342926032, 74.65491531819115778 ) ) ;
#73534 = DIRECTION ( 'NONE',  ( 0.000000000000000000, 0.000000000000000000, 1.000000000000000000 ) ) ;
#73535 = CARTESIAN_POINT ( 'NONE',  ( -26.29030328629082902, -123.6496510949466341, -2.500000000000000000 ) ) ;
#73536 = VECTOR ( 'NONE', #17962, 1000.000000000000000 ) ;
#73537 = CARTESIAN_POINT ( 'NONE',  ( -93.84685191531248449, -208.0026889286704943, 81.96989583420048575 ) ) ;
#73538 = EDGE_LOOP ( 'NONE', ( #24361, #41685, #13412, #33823 ) ) ;
#73539 = DIRECTION ( 'NONE',  ( -1.000000000000000000, 0.000000000000000000, 0.000000000000000000 ) ) ;
#73540 = ORIENTED_EDGE ( 'NONE', *, *, #21266, .T. ) ;
#73541 = DIRECTION ( 'NONE',  ( -1.000000000000000000, -0.000000000000000000, -0.000000000000000000 ) ) ;
#73542 = VECTOR ( 'NONE', #59046, 1000.000000000000000 ) ;
#73543 = CIRCLE ( 'NONE', #62798, 16.00000000000000000 ) ;
#73544 = CARTESIAN_POINT ( 'NONE',  ( 0.000000000000000000, -2.946379043146863719, 75.11764819372146462 ) ) ;
#73545 = DIRECTION ( 'NONE',  ( 0.000000000000000000, 0.4539904997395413644, 0.8910065241883706744 ) ) ;
#73546 = DIRECTION ( 'NONE',  ( 0.9038112904824842087, -0.4279312458753000703, 0.000000000000000000 ) ) ;
#73547 = DIRECTION ( 'NONE',  ( -1.000000000000000000, 0.000000000000000000, -0.000000000000000000 ) ) ;
#73548 = DIRECTION ( 'NONE',  ( -1.000000000000000000, 0.000000000000000000, 0.000000000000000000 ) ) ;
#73549 = DIRECTION ( 'NONE',  ( -1.000000000000000000, 0.000000000000000000, 0.000000000000000000 ) ) ;
#73550 = DIRECTION ( 'NONE',  ( 1.000000000000000000, 0.000000000000000000, 0.000000000000000000 ) ) ;
#73551 = CARTESIAN_POINT ( 'NONE',  ( 10.00000000000000000, 71.91182617369230456, -28.89263327155667938 ) ) ;
#73552 = CARTESIAN_POINT ( 'NONE',  ( 10.00000000000000000, 0.000000000000000000, 0.000000000000000000 ) ) ;
#73553 = CARTESIAN_POINT ( 'NONE',  ( 92.35000000007822507, -209.9999869687480611, 79.28395951162927702 ) ) ;
#73554 = CARTESIAN_POINT ( 'NONE',  ( 15.00000000000000000, 22.07842321921492612, 8.187992925817123790 ) ) ;
#73555 = DIRECTION ( 'NONE',  ( -1.000000000000000000, 0.000000000000000000, 0.000000000000000000 ) ) ;
#73557 = EDGE_CURVE ( 'NONE', #23395, #35486, #119, .T. ) ;
#73556 = ORIENTED_EDGE ( 'NONE', *, *, #15969, .F. ) ;
#73558 = CARTESIAN_POINT ( 'NONE',  ( 0.000000000000000000, -59.75363087400114637, 56.15606465354937171 ) ) ;
#73559 = CARTESIAN_POINT ( 'NONE',  ( -93.84685191531254134, 91.99731107132950569, 79.27114583420046756 ) ) ;
#73560 = EDGE_CURVE ( 'NONE', #38392, #45747, #57710, .T. ) ;
#73561 = DIRECTION ( 'NONE',  ( -0.000000000000000000, -0.000000000000000000, 1.000000000000000000 ) ) ;
#73562 = ADVANCED_FACE ( 'NONE', ( #51453 ), #6353, .F. ) ;
#73563 = ORIENTED_EDGE ( 'NONE', *, *, #23283, .T. ) ;
#73564 = DIRECTION ( 'NONE',  ( -0.000000000000000000, -0.000000000000000000, 1.000000000000000000 ) ) ;
#73565 = FACE_OUTER_BOUND ( 'NONE', #35615, .T. ) ;
#73566 = CARTESIAN_POINT ( 'NONE',  ( 10.00000000000000000, 0.000000000000000000, 0.000000000000000000 ) ) ;
#73567 = EDGE_CURVE ( 'NONE', #50947, #35752, #55281, .T. ) ;
#73568 = CARTESIAN_POINT ( 'NONE',  ( 11.99999999999999822, -71.21200624218823805, 40.65526001592589722 ) ) ;
#73569 = CARTESIAN_POINT ( 'NONE',  ( 95.00000000000000000, -207.3369185715606307, 75.67281250086716682 ) ) ;
#73570 = AXIS2_PLACEMENT_3D ( 'NONE', #12554, #19669, #13295 ) ;
#73571 = ORIENTED_EDGE ( 'NONE', *, *, #34143, .T. ) ;
#73572 = VERTEX_POINT ( 'NONE', #34532 ) ;
#73573 = CARTESIAN_POINT ( 'NONE',  ( 11.99999999999999822, 0.000000000000000000, 0.000000000000000000 ) ) ;
#73574 = EDGE_CURVE ( 'NONE', #62322, #8415, #16880, .T. ) ;
#73575 = DIRECTION ( 'NONE',  ( 0.000000000000000000, -0.3090169943749350168, -0.9510565162951576390 ) ) ;
#73576 = AXIS2_PLACEMENT_3D ( 'NONE', #67768, #4255, #56496 ) ;
#73577 =( BOUNDED_CURVE ( )  B_SPLINE_CURVE ( 2, ( #4214, #21468, #39153, #56069, #44054, #44429, #9832 ),
 .UNSPECIFIED., .F., .F. ) 
 B_SPLINE_CURVE_WITH_KNOTS ( ( 3, 2, 2, 3 ),
 ( 0.3749999999999998335, 0.3819444444444441977, 0.3888888888888886730, 0.3958333333333330373 ),
 .UNSPECIFIED. ) 
 CURVE ( )  GEOMETRIC_REPRESENTATION_ITEM ( )  RATIONAL_B_SPLINE_CURVE ( ( 1.000000000000003109, 0.8660254037844354880, 1.000000000000000000, 0.8660254037844387076, 1.000000000000000000, 0.8660254037844440367, 0.9999999999999946709 ) ) 
 REPRESENTATION_ITEM ( '' )  );
#73578 = CARTESIAN_POINT ( 'NONE',  ( 11.99999999999999822, -76.66974797899844418, 11.30684508768314522 ) ) ;
#73579 = FACE_OUTER_BOUND ( 'NONE', #17230, .T. ) ;
#73580 = EDGE_CURVE ( 'NONE', #19963, #14426, #64902, .T. ) ;
#73581 = DIRECTION ( 'NONE',  ( -1.000000000000000000, -0.000000000000000000, 0.000000000000000000 ) ) ;
#73582 = EDGE_CURVE ( 'NONE', #65117, #35350, #46376, .T. ) ;
#73583 = CARTESIAN_POINT ( 'NONE',  ( 95.00000000000000000, -213.0599564267049857, 89.52375000000000682 ) ) ;
#73584 = ORIENTED_EDGE ( 'NONE', *, *, #55930, .T. ) ;
#73585 = DIRECTION ( 'NONE',  ( 0.000000000000000000, 0.000000000000000000, 1.000000000000000000 ) ) ;
#73586 = ORIENTED_EDGE ( 'NONE', *, *, #2017, .T. ) ;
#73587 = AXIS2_PLACEMENT_3D ( 'NONE', #42859, #32668, #25925 ) ;
#73588 = VERTEX_POINT ( 'NONE', #62010 ) ;
#73589 = CARTESIAN_POINT ( 'NONE',  ( 48.80839716909466830, -10.37454508288725208, 5.500000000000000000 ) ) ;
#73590 = CIRCLE ( 'NONE', #41199, 31.99999999999998579 ) ;
#73591 =( NAMED_UNIT ( * ) PLANE_ANGLE_UNIT ( ) SI_UNIT ( $, .RADIAN. ) );
#73592 = CARTESIAN_POINT ( 'NONE',  ( 2.499999999999988454, -65.00000000000000000, -290.0000000000000568 ) ) ;
#73593 = ORIENTED_EDGE ( 'NONE', *, *, #73317, .F. ) ;
#73594 = FACE_OUTER_BOUND ( 'NONE', #20241, .T. ) ;
#73595 = CARTESIAN_POINT ( 'NONE',  ( 97.64999999999997726, -211.5299782133524502, 80.18395833506764347 ) ) ;
#73596 = CARTESIAN_POINT ( 'NONE',  ( 93.67499999999999716, 87.70503267997126784, 81.21583333333333599 ) ) ;
#73597 = ORIENTED_EDGE ( 'NONE', *, *, #62701, .F. ) ;
#73598 = CARTESIAN_POINT ( 'NONE',  ( 0.000000000000000000, -4.992566952384716927, -37.16516213103282951 ) ) ;
#73599 = VERTEX_POINT ( 'NONE', #16506 ) ;
#73600 = ADVANCED_FACE ( 'NONE', ( #51832 ), #10489, .F. ) ;
#73601 = DIRECTION ( 'NONE',  ( -1.000000000000000000, 0.000000000000000000, -0.000000000000000000 ) ) ;
#73602 = EDGE_CURVE ( 'NONE', #55862, #70850, #70891, .T. ) ;
#73603 = ORIENTED_EDGE ( 'NONE', *, *, #68534, .F. ) ;
#73604 = FACE_OUTER_BOUND ( 'NONE', #6962, .T. ) ;
#73605 = CARTESIAN_POINT ( 'NONE',  ( -92.69370383062505425, 88.66845928578038638, 84.98614583420047097 ) ) ;
#73606 = CARTESIAN_POINT ( 'NONE',  ( 94.99999999999998579, 92.66308142843935514, 78.05406250086714692 ) ) ;
#73607 = ORIENTED_EDGE ( 'NONE', *, *, #5446, .T. ) ;
#73608 = FACE_OUTER_BOUND ( 'NONE', #28290, .T. ) ;
#73609 = CARTESIAN_POINT ( 'NONE',  ( 0.000000000000000000, -120.0000000000000000, 2.500000000000000000 ) ) ;
#73610 = DIRECTION ( 'NONE',  ( -1.000000000000000000, 0.000000000000000000, -0.000000000000000000 ) ) ;
#73611 = LINE ( 'NONE', #38674, #46836 ) ;
#73612 = ORIENTED_EDGE ( 'NONE', *, *, #52036, .F. ) ;
#73613 = DIRECTION ( 'NONE',  ( 1.000000000000000000, 0.000000000000000000, 0.000000000000000000 ) ) ;
#73614 = CARTESIAN_POINT ( 'NONE',  ( -92.69370383062498320, -208.6684592857803011, 76.04322916753380923 ) ) ;
#73615 = ORIENTED_EDGE ( 'NONE', *, *, #42703, .F. ) ;
#73616 = ORIENTED_EDGE ( 'NONE', *, *, #71036, .T. ) ;
#73617 = DIRECTION ( 'NONE',  ( 0.000000000000000000, 0.000000000000000000, 1.000000000000000000 ) ) ;
#73618 = ORIENTED_EDGE ( 'NONE', *, *, #66650, .T. ) ;
#73619 = DIRECTION ( 'NONE',  ( -1.000000000000000000, 0.000000000000000000, 0.000000000000000000 ) ) ;
#73620 = VECTOR ( 'NONE', #18717, 1000.000000000000000 ) ;
#73621 = LINE ( 'NONE', #45454, #14860 ) ;
#73622 = ORIENTED_EDGE ( 'NONE', *, *, #55991, .T. ) ;
#73623 = CARTESIAN_POINT ( 'NONE',  ( -96.15314808468747287, -208.0026889286704943, 74.93197916753379673 ) ) ;
#73624 = ORIENTED_EDGE ( 'NONE', *, *, #49206, .T. ) ;
#73625 = DIRECTION ( 'NONE',  ( -1.000000000000000000, 0.000000000000000000, 0.000000000000000000 ) ) ;
#73626 = DIRECTION ( 'NONE',  ( -1.000000000000000000, -0.000000000000000000, 0.000000000000000000 ) ) ;
#73627 = CARTESIAN_POINT ( 'NONE',  ( 15.00000000000000000, 22.07842321921480888, -8.187992925817425771 ) ) ;
#73628 = CARTESIAN_POINT ( 'NONE',  ( -94.99999999999997158, -206.9400435732949575, 89.28562500173430294 ) ) ;
#73629 = PRODUCT_DEFINITION_FORMATION_WITH_SPECIFIED_SOURCE ( 'ANY', '', #49976, .NOT_KNOWN. ) ;
#73630 = DIRECTION ( 'NONE',  ( 0.000000000000000000, 0.3090169943749450088, -0.9510565162951543083 ) ) ;
#73631 = CARTESIAN_POINT ( 'NONE',  ( -10.00000000000000000, 0.000000000000000000, 0.000000000000000000 ) ) ;
#73632 = CARTESIAN_POINT ( 'NONE',  ( 96.15314808468748708, 91.99731107132950569, 85.62114583420046188 ) ) ;
#73633 = LINE ( 'NONE', #16504, #65247 ) ;
#73634 = DIRECTION ( 'NONE',  ( -1.000000000000000000, 0.000000000000000000, -0.000000000000000000 ) ) ;
#73635 = CARTESIAN_POINT ( 'NONE',  ( 15.00000000000000000, -14.54903810567644484, 22.19967320028775504 ) ) ;
#73636 = CARTESIAN_POINT ( 'NONE',  ( 5.822613034544236399, -142.8165987265839760, 5.500000000000000000 ) ) ;
#73637 = LINE ( 'NONE', #3767, #65670 ) ;
#73638 = LINE ( 'NONE', #40935, #19116 ) ;
#73639 = CIRCLE ( 'NONE', #37644, 31.99999999999998934 ) ;
#73640 = FACE_OUTER_BOUND ( 'NONE', #47615, .T. ) ;
#73641 = AXIS2_PLACEMENT_3D ( 'NONE', #17908, #17537, #46481 ) ;
#73642 = CARTESIAN_POINT ( 'NONE',  ( 97.64999999999999147, 90.00000000000002842, 78.88750000000000284 ) ) ;
#73643 = EDGE_CURVE ( 'NONE', #855, #2154, #67305, .T. ) ;
#73644 = CARTESIAN_POINT ( 'NONE',  ( 11.99999999999999822, -20.40083707022829174, -72.35432306680507963 ) ) ;
#73645 = AXIS2_PLACEMENT_3D ( 'NONE', #25837, #26577, #13805 ) ;
#73646 = CARTESIAN_POINT ( 'NONE',  ( -92.69370383062505425, 88.66845928578038638, 88.63739583420047552 ) ) ;
#73647 = VECTOR ( 'NONE', #66542, 1000.000000000000000 ) ;
#73648 = VECTOR ( 'NONE', #26398, 1000.000000000000000 ) ;
#73649 = FACE_OUTER_BOUND ( 'NONE', #24905, .T. ) ;
#73650 = EDGE_CURVE ( 'NONE', #11562, #22041, #57114, .T. ) ;
#73651 = CARTESIAN_POINT ( 'NONE',  ( -96.32499999999996021, -212.2949673200287179, 85.66083333333332916 ) ) ;
#73652 = EDGE_CURVE ( 'NONE', #65113, #59483, #42094, .T. ) ;
#73653 = EDGE_CURVE ( 'NONE', #45691, #35608, #51643, .T. ) ;
#73654 = FACE_OUTER_BOUND ( 'NONE', #60116, .T. ) ;
#73655 = DIRECTION ( 'NONE',  ( 0.000000000000000000, 0.7604059656000322631, -0.6494480483301821039 ) ) ;
#73656 = LINE ( 'NONE', #16157, #4659 ) ;
#73657 = FACE_OUTER_BOUND ( 'NONE', #17596, .T. ) ;
#73658 = DIRECTION ( 'NONE',  ( -0.6862798483830534479, -0.7273375899149810975, 0.000000000000000000 ) ) ;
#73659 = ADVANCED_FACE ( 'NONE', ( #40932 ), #36751, .F. ) ;
#73660 = CARTESIAN_POINT ( 'NONE',  ( 97.30629616937498838, -211.3315407142195852, 85.62114583420047609 ) ) ;
#73661 = ORIENTED_EDGE ( 'NONE', *, *, #69027, .T. ) ;
#73662 = EDGE_LOOP ( 'NONE', ( #67430, #39340, #64214 ) ) ;
#73663 = PLANE ( 'NONE',  #30725 ) ;
#73664 = ORIENTED_EDGE ( 'NONE', *, *, #28272, .F. ) ;
#73665 = LINE ( 'NONE', #62041, #34176 ) ;
#73666 = CARTESIAN_POINT ( 'NONE',  ( 96.15314808468748708, -208.0026889286704943, 76.73114583420047552 ) ) ;
#73668 = VERTEX_POINT ( 'NONE', #6709 ) ;
#73667 = ADVANCED_FACE ( 'NONE', ( #52562 ), #59320, .T. ) ;
#73669 = ADVANCED_FACE ( 'NONE', ( #64232 ), #1483, .F. ) ;
#73670 = CARTESIAN_POINT ( 'NONE',  ( 95.00000000000000000, -212.6630814284392557, 81.70531250086715147 ) ) ;
#73671 = EDGE_CURVE ( 'NONE', #18572, #31821, #68611, .T. ) ;
#73672 = EDGE_LOOP ( 'NONE', ( #5844, #56245, #26768, #65407 ) ) ;
#73673 = CARTESIAN_POINT ( 'NONE',  ( 10.00000000000000000, 0.000000000000000000, 0.000000000000000000 ) ) ;
#73674 = ORIENTED_EDGE ( 'NONE', *, *, #72987, .T. ) ;
#73675 = EDGE_CURVE ( 'NONE', #62190, #13857, #36012, .T. ) ;
#73676 = EDGE_CURVE ( 'NONE', #14426, #8127, #2531, .T. ) ;
#73677 = VERTEX_POINT ( 'NONE', #2592 ) ;
#73678 = CYLINDRICAL_SURFACE ( 'NONE', #27366, 16.00000000000000000 ) ;
#73679 = AXIS2_PLACEMENT_3D ( 'NONE', #65648, #54002, #14499 ) ;
#73680 = DIRECTION ( 'NONE',  ( -0.000000000000000000, -0.000000000000000000, 1.000000000000000000 ) ) ;
#73681 = EDGE_LOOP ( 'NONE', ( #30486, #38910, #23207, #18116 ) ) ;
#73682 = CARTESIAN_POINT ( 'NONE',  ( 93.67499999999998295, 92.29496732002878900, 86.08416666666666117 ) ) ;
#73683 = CARTESIAN_POINT ( 'NONE',  ( 92.35000000000002274, -208.4700217866474645, 89.39145833506763950 ) ) ;
#73684 = ORIENTED_EDGE ( 'NONE', *, *, #65190, .T. ) ;
#73685 = CARTESIAN_POINT ( 'NONE',  ( 10.00000000000000000, 0.000000000000000000, 0.000000000000000000 ) ) ;
#73686 = EDGE_CURVE ( 'NONE', #72991, #30232, #29615, .T. ) ;
#73687 = ORIENTED_EDGE ( 'NONE', *, *, #1047, .T. ) ;
#73688 = DIRECTION ( 'NONE',  ( -0.5200609990132993854, -0.8541291221503275466, 0.000000000000000000 ) ) ;
#73689 = CIRCLE ( 'NONE', #20885, 23.50000000000489919 ) ;
#73690 = ORIENTED_EDGE ( 'NONE', *, *, #27846, .T. ) ;
#73691 = EDGE_CURVE ( 'NONE', #65118, #16263, #36374, .T. ) ;
#73692 = ORIENTED_EDGE ( 'NONE', *, *, #61396, .F. ) ;
#73693 = AXIS2_PLACEMENT_3D ( 'NONE', #68209, #9577, #50906 ) ;
#73694 = ORIENTED_EDGE ( 'NONE', *, *, #73040, .F. ) ;
#73695 = CARTESIAN_POINT ( 'NONE',  ( 97.30629616937498838, -208.6684592857803011, 76.04322916753380923 ) ) ;
#73696 = AXIS2_PLACEMENT_3D ( 'NONE', #60539, #38336, #61644 ) ;
#73697 = CONTEXT_DEPENDENT_SHAPE_REPRESENTATION ( #37879, #69864 ) ;
#73698 = CARTESIAN_POINT ( 'NONE',  ( -97.64999999999996305, -209.9999999999999716, 90.00000000000000000 ) ) ;
#73699 = ORIENTED_EDGE ( 'NONE', *, *, #60012, .F. ) ;
#73700 = ORIENTED_EDGE ( 'NONE', *, *, #71282, .F. ) ;
#73701 = VERTEX_POINT ( 'NONE', #7814 ) ;
#73702 = CARTESIAN_POINT ( 'NONE',  ( 96.32499999999998863, -212.2949673200287179, 76.24166666666666003 ) ) ;
#73703 = CARTESIAN_POINT ( 'NONE',  ( -97.65000000000004832, -208.4700217866474929, 88.67708333333332860 ) ) ;
#73704 = CARTESIAN_POINT ( 'NONE',  ( -93.84685191531254134, 91.99731107132950569, 76.88989583420048746 ) ) ;
#73705 = VERTEX_POINT ( 'NONE', #19458 ) ;
#73706 = CARTESIAN_POINT ( 'NONE',  ( 93.84685191531248449, 88.00268892867053694, 75.77864583420047495 ) ) ;
#73707 = VERTEX_POINT ( 'NONE', #24007 ) ;
#73708 = CARTESIAN_POINT ( 'NONE',  ( -92.69370383062498320, -208.6684592857803011, 84.93322916753379559 ) ) ;
#73709 = ORIENTED_EDGE ( 'NONE', *, *, #1426, .T. ) ;
#73710 = DIRECTION ( 'NONE',  ( 0.000000000000000000, -0.9510565162951499785, -0.3090169943749582204 ) ) ;
#73711 = CARTESIAN_POINT ( 'NONE',  ( -90.00000000000002842, 95.00000000000002842, 90.00000000000000000 ) ) ;
#73712 = DIRECTION ( 'NONE',  ( -1.000000000000000000, 0.000000000000000000, -0.000000000000000000 ) ) ;
#73713 = CARTESIAN_POINT ( 'NONE',  ( -92.69370383062498320, -211.3315407142195852, 79.11239583420046984 ) ) ;
#73714 = VECTOR ( 'NONE', #9538, 1000.000000000000000 ) ;
#73715 = DIRECTION ( 'NONE',  ( -1.000000000000000000, -0.000000000000000000, -0.000000000000000000 ) ) ;
#73716 = CARTESIAN_POINT ( 'NONE',  ( 11.99999999999999822, 62.50884508063427347, 41.76106447765511831 ) ) ;
#73717 = DIRECTION ( 'NONE',  ( 0.000000000000000000, 0.9510565162951544194, -0.3090169943749446757 ) ) ;
#73718 = ORIENTED_EDGE ( 'NONE', *, *, #68989, .T. ) ;
#73719 = DIRECTION ( 'NONE',  ( -1.000000000000000000, 0.000000000000000000, -0.000000000000000000 ) ) ;
#73720 = DIRECTION ( 'NONE',  ( -1.000000000000000000, 0.000000000000000000, 0.000000000000000000 ) ) ;
#73721 = CARTESIAN_POINT ( 'NONE',  ( 92.50303120605396145, -209.7556371990021944, 74.91343443312142369 ) ) ;
#73722 = CARTESIAN_POINT ( 'NONE',  ( -97.30629616937501680, 91.33154071421968467, 81.96989583420048575 ) ) ;
#73723 = CARTESIAN_POINT ( 'NONE',  ( 5.000000000000000000, -60.67117009219098378, -55.16347631943106933 ) ) ;
#73724 = CARTESIAN_POINT ( 'NONE',  ( 97.64999999999999147, 90.00000000000002842, 75.71250000000000568 ) ) ;
#73725 = ORIENTED_EDGE ( 'NONE', *, *, #46094, .F. ) ;
#73726 = DIRECTION ( 'NONE',  ( -1.000000000000000000, 0.000000000000000000, 0.000000000000000000 ) ) ;
#73727 = EDGE_CURVE ( 'NONE', #28568, #23400, #59327, .T. ) ;
#73728 = DIRECTION ( 'NONE',  ( 0.9781476007338069101, 0.000000000000000000, -0.2079116908177528755 ) ) ;
#73729 = CARTESIAN_POINT ( 'NONE',  ( 10.00000000000000000, 0.000000000000000000, 0.000000000000000000 ) ) ;
#73730 = CIRCLE ( 'NONE', #72497, 12.85999999999999943 ) ;
#73731 = FACE_OUTER_BOUND ( 'NONE', #51339, .T. ) ;
#73732 = EDGE_CURVE ( 'NONE', #32752, #34951, #13808, .T. ) ;
#73733 = CARTESIAN_POINT ( 'NONE',  ( 10.00000000000000000, 29.81001611431009479, 22.74946021919143391 ) ) ;
#73734 = CARTESIAN_POINT ( 'NONE',  ( -96.32500000000001705, 92.29496732002878900, 87.35416666666665719 ) ) ;
#73735 = CARTESIAN_POINT ( 'NONE',  ( -92.69370383062498320, -209.9999999999999716, 80.59406250086715318 ) ) ;
#73736 = EDGE_CURVE ( 'NONE', #16641, #5078, #73258, .T. ) ;
#73737 = EDGE_CURVE ( 'NONE', #1727, #25328, #25476, .T. ) ;
#73738 = DIRECTION ( 'NONE',  ( 0.000000000000000000, 0.000000000000000000, 1.000000000000000000 ) ) ;
#73739 = AXIS2_PLACEMENT_3D ( 'NONE', #24775, #59735, #25155 ) ;
#73740 = ORIENTED_EDGE ( 'NONE', *, *, #6715, .F. ) ;
#73741 = CIRCLE ( 'NONE', #38929, 16.00000000000000000 ) ;
#73742 = DIRECTION ( 'NONE',  ( 0.2867529058022011967, -0.9580045777625459946, 0.000000000000000000 ) ) ;
#73743 = CARTESIAN_POINT ( 'NONE',  ( -92.35000000000003695, 89.99999997928479445, 80.87187500099602744 ) ) ;
#73744 = DIRECTION ( 'NONE',  ( -0.000000000000000000, -0.000000000000000000, -1.000000000000000000 ) ) ;
#73745 = ORIENTED_EDGE ( 'NONE', *, *, #35499, .F. ) ;
#73746 = CYLINDRICAL_SURFACE ( 'NONE', #48523, 42.00000000000000000 ) ;
#73747 = DIRECTION ( 'NONE',  ( -1.000000000000000000, -0.000000000000000000, 0.000000000000000000 ) ) ;
#73748 = CIRCLE ( 'NONE', #62847, 32.00000000000000000 ) ;
#73749 = AXIS2_PLACEMENT_3D ( 'NONE', #6190, #56582, #39654 ) ;
#73750 = CIRCLE ( 'NONE', #63012, 31.99999999999998579 ) ;
#73751 = CARTESIAN_POINT ( 'NONE',  ( 11.99999999999999822, 77.49459641780886443, -0.8261519478433960728 ) ) ;
#73752 = ADVANCED_FACE ( 'NONE', ( #17987 ), #41649, .T. ) ;
#73753 = EDGE_LOOP ( 'NONE', ( #65844, #68457, #10770, #10084 ) ) ;
#73754 = DIRECTION ( 'NONE',  ( -1.000000000000000000, -0.000000000000000000, -0.000000000000000000 ) ) ;
#73755 = DIRECTION ( 'NONE',  ( 0.000000000000000000, 0.000000000000000000, -1.000000000000000000 ) ) ;
#73756 = ORIENTED_EDGE ( 'NONE', *, *, #47117, .T. ) ;
#73757 = VECTOR ( 'NONE', #8954, 1000.000000000000000 ) ;
#73758 = CARTESIAN_POINT ( 'NONE',  ( 96.15314808468750130, -211.9973110713294489, 87.94947916753380923 ) ) ;
#73759 = FACE_OUTER_BOUND ( 'NONE', #71721, .T. ) ;
#73760 = ORIENTED_EDGE ( 'NONE', *, *, #51442, .T. ) ;
#73761 = AXIS2_PLACEMENT_3D ( 'NONE', #8339, #19240, #7961 ) ;
#73762 = DIRECTION ( 'NONE',  ( -1.000000000000000000, 0.000000000000000000, -0.000000000000000000 ) ) ;
#73763 = VERTEX_POINT ( 'NONE', #14559 ) ;
#73764 = CARTESIAN_POINT ( 'NONE',  ( -92.34999999999999432, -210.0000001167898631, 84.68187499741277691 ) ) ;
#73765 = EDGE_LOOP ( 'NONE', ( #43929, #42357, #61813, #41496 ) ) ;
#73766 = EDGE_CURVE ( 'NONE', #8717, #57544, #19822, .T. ) ;
#73767 = EDGE_CURVE ( 'NONE', #63089, #41920, #26579, .T. ) ;
#73768 = CARTESIAN_POINT ( 'NONE',  ( 92.35000000000003695, -211.5299782133524218, 81.79791666666665151 ) ) ;
#73769 = VERTEX_POINT ( 'NONE', #43892 ) ;
#73770 = ORIENTED_EDGE ( 'NONE', *, *, #45483, .T. ) ;
#73771 = VERTEX_POINT ( 'NONE', #72435 ) ;
#73772 = DIRECTION ( 'NONE',  ( -1.000000000000000000, -0.000000000000000000, 0.000000000000000000 ) ) ;
#73773 = ORIENTED_EDGE ( 'NONE', *, *, #23006, .T. ) ;
#73774 = VERTEX_POINT ( 'NONE', #43534 ) ;
#73775 = CARTESIAN_POINT ( 'NONE',  ( 97.64999999999997726, 91.52997821335252127, 87.19541666666667368 ) ) ;
#73776 = CYLINDRICAL_SURFACE ( 'NONE', #4840, 2.649999999999985700 ) ;
#73777 = FACE_OUTER_BOUND ( 'NONE', #70018, .T. ) ;
#73778 = ORIENTED_EDGE ( 'NONE', *, *, #813, .F. ) ;
#73779 = ORIENTED_EDGE ( 'NONE', *, *, #39758, .F. ) ;
#73780 = VERTEX_POINT ( 'NONE', #72793 ) ;
#73781 = CARTESIAN_POINT ( 'NONE',  ( 96.15314808468748708, 88.00268892867053694, 89.21947916753380525 ) ) ;
#73782 = ORIENTED_EDGE ( 'NONE', *, *, #55183, .T. ) ;
#73783 = CARTESIAN_POINT ( 'NONE',  ( 93.84685191531251292, -211.9973110713294489, 85.93864583420048575 ) ) ;
#73784 = CIRCLE ( 'NONE', #25768, 16.00000000000000355 ) ;
#73785 = CARTESIAN_POINT ( 'NONE',  ( -94.99999999999877787, -210.0000000000012506, 102.7499999999999716 ) ) ;
#73786 = CARTESIAN_POINT ( 'NONE',  ( 0.000000000000000000, 0.000000000000000000, 0.000000000000000000 ) ) ;
#73787 = CARTESIAN_POINT ( 'NONE',  ( 10.00000000000000000, 0.000000000000000000, 0.000000000000000000 ) ) ;
#73788 = CARTESIAN_POINT ( 'NONE',  ( -93.67500000000003979, 92.29496732002878900, 77.80270833506763495 ) ) ;
#73789 = CARTESIAN_POINT ( 'NONE',  ( 0.000000000000000000, 0.000000000000000000, 0.000000000000000000 ) ) ;
#73790 = CYLINDRICAL_SURFACE ( 'NONE', #18012, 2.649999999999999467 ) ;
#73791 = CARTESIAN_POINT ( 'NONE',  ( 92.35000000002600018, 89.99999999999995737, -65.00000000000007105 ) ) ;
#73792 = CARTESIAN_POINT ( 'NONE',  ( -97.30629616937497417, -208.6684592857803011, 86.41489583420047893 ) ) ;
#73793 = CARTESIAN_POINT ( 'NONE',  ( -95.00000000000002842, 87.33691857156074434, 84.88031250086714863 ) ) ;
#73794 = EDGE_LOOP ( 'NONE', ( #29157, #43664, #60672, #35601 ) ) ;
#73796 = CARTESIAN_POINT ( 'NONE',  ( -97.30629616937501680, 90.00000000000004263, 85.83281250086714920 ) ) ;
#73795 = CARTESIAN_POINT ( 'NONE',  ( 94.99999999999998579, 92.66308142843935514, 83.13406250086714522 ) ) ;
#73797 = ORIENTED_EDGE ( 'NONE', *, *, #39337, .T. ) ;
#73798 = FACE_OUTER_BOUND ( 'NONE', #67146, .T. ) ;
#73799 = AXIS2_PLACEMENT_3D ( 'NONE', #34553, #45491, #39844 ) ;
#73800 = CARTESIAN_POINT ( 'NONE',  ( -93.67499999999998295, -212.2949673200287179, 80.76604166840097321 ) ) ;
#73801 = AXIS2_PLACEMENT_3D ( 'NONE', #11736, #34681, #35426 ) ;
#73802 = CARTESIAN_POINT ( 'NONE',  ( 10.00000000000000000, -36.88895765772637247, 6.736453364083436313 ) ) ;
#73803 = CARTESIAN_POINT ( 'NONE',  ( 10.00000000000000000, 0.000000000000000000, 0.000000000000000000 ) ) ;
#73804 = CARTESIAN_POINT ( 'NONE',  ( -93.84685191531248449, -208.0026889286704943, 88.79614583420047325 ) ) ;
#73805 = CARTESIAN_POINT ( 'NONE',  ( 4.999999999999999112, 38.55633173627034438, -16.65560815589369881 ) ) ;
#73806 = CARTESIAN_POINT ( 'NONE',  ( 0.000000000000000000, 40.65526001592713357, -71.21200624218752750 ) ) ;
#73807 = CYLINDRICAL_SURFACE ( 'NONE', #4298, 77.49899999999999523 ) ;
#73808 = AXIS2_PLACEMENT_3D ( 'NONE', #67754, #62503, #50453 ) ;
#73809 = DIRECTION ( 'NONE',  ( 1.000000000000000000, -0.000000000000000000, -0.000000000000000000 ) ) ;
#73810 = EDGE_LOOP ( 'NONE', ( #42305, #52595, #54540, #9874 ) ) ;
#73811 = ORIENTED_EDGE ( 'NONE', *, *, #6400, .T. ) ;
#73812 = CARTESIAN_POINT ( 'NONE',  ( -92.35000000000005116, 88.47002178664754979, 80.10458333333332348 ) ) ;
#73813 = CARTESIAN_POINT ( 'NONE',  ( 0.000000000000000000, 31.46837873495072913, -68.27212725128242710 ) ) ;
#73814 = DIRECTION ( 'NONE',  ( -7.381802025433090153E-16, -1.065814103640131188E-14, -1.000000000000000000 ) ) ;
#73815 = DIRECTION ( 'NONE',  ( 0.000000000000000000, 0.9135454576426010886, -0.4067366430757998752 ) ) ;
#73816 = DIRECTION ( 'NONE',  ( -1.000000000000000000, 0.000000000000000000, 0.000000000000000000 ) ) ;
#73817 = CIRCLE ( 'NONE', #54614, 2.650000000000540812 ) ;
#73818 = CARTESIAN_POINT ( 'NONE',  ( 97.64999999954044085, 90.00004935162768049, 87.22187670868791542 ) ) ;
#73819 = DIRECTION ( 'NONE',  ( -1.000000000000000000, -0.000000000000000000, 0.000000000000000000 ) ) ;
#73820 = DIRECTION ( 'NONE',  ( -1.000000000000000000, 0.000000000000000000, 0.000000000000000000 ) ) ;
#73821 =( BOUNDED_CURVE ( )  B_SPLINE_CURVE ( 2, ( #67177, #32946, #48767, #21677, #37871, #61547, #49140, #54783, #10026 ),
 .UNSPECIFIED., .F., .F. ) 
 B_SPLINE_CURVE_WITH_KNOTS ( ( 3, 2, 2, 2, 3 ),
 ( 0.8678591737257297378, 0.8749149270737099915, 0.8819706926146264614, 0.8890264581555429313, 0.8890265259402125864 ),
 .UNSPECIFIED. ) 
 CURVE ( )  GEOMETRIC_REPRESENTATION_ITEM ( )  RATIONAL_B_SPLINE_CURVE ( ( 1.000000000000000000, 0.8660254037844387076, 1.000000000000000000, 0.8660254037844387076, 1.000000000000000000, 0.8660254037844387076, 1.000000000000000000, 0.9999987129073806269, 0.9999974258394913607 ) ) 
 REPRESENTATION_ITEM ( '' )  );
#73822 = VERTEX_POINT ( 'NONE', #66812 ) ;
#73823 = CARTESIAN_POINT ( 'NONE',  ( -92.69370383062502583, 88.66845928578038638, 78.47739583420047893 ) ) ;
#73824 = AXIS2_PLACEMENT_3D ( 'NONE', #24622, #24264, #1735 ) ;
#73825 = EDGE_CURVE ( 'NONE', #42474, #18479, #15681, .T. ) ;
#73826 = CARTESIAN_POINT ( 'NONE',  ( 10.00000000000000000, 46.53671651293948486, 59.03961581697416250 ) ) ;
#73827 = DIRECTION ( 'NONE',  ( -0.000000000000000000, -0.000000000000000000, 1.000000000000000000 ) ) ;
#73828 = DIRECTION ( 'NONE',  ( 1.000000000000000000, 0.000000000000000000, 0.000000000000000000 ) ) ;
#73829 = EDGE_CURVE ( 'NONE', #45831, #33770, #33654, .T. ) ;
#73830 = DIRECTION ( 'NONE',  ( -1.000000000000000000, 0.000000000000000000, -0.000000000000000000 ) ) ;
#73831 = CARTESIAN_POINT ( 'NONE',  ( 11.99999999999999822, 2.946379043147425492, -75.11764819372145041 ) ) ;
#73832 = CARTESIAN_POINT ( 'NONE',  ( -93.84685191531248449, -208.0026889286704943, 89.58989583420049030 ) ) ;
#73833 = EDGE_CURVE ( 'NONE', #67617, #19812, #9723, .T. ) ;
#73834 = EDGE_CURVE ( 'NONE', #60600, #23124, #3734, .T. ) ;
#73835 = CARTESIAN_POINT ( 'NONE',  ( 92.69370383062498320, 90.00000000000002842, 78.37156250086715659 ) ) ;
#73836 = CARTESIAN_POINT ( 'NONE',  ( -94.99999999999997158, -212.6630814284392557, 81.07031250086716057 ) ) ;
#73837 = DIRECTION ( 'NONE',  ( 0.5687579148473744795, -0.8225049752423790883, 0.000000000000000000 ) ) ;
#73838 = VERTEX_POINT ( 'NONE', #20938 ) ;
#73839 = DIRECTION ( 'NONE',  ( -1.000000000000000000, 0.000000000000000000, -0.000000000000000000 ) ) ;
#73840 = CARTESIAN_POINT ( 'NONE',  ( -97.64999999999994884, -211.5299782133524502, 76.08291666666666231 ) ) ;
#73841 = DIRECTION ( 'NONE',  ( 0.000000000000000000, -0.8526401643540860720, -0.5224985647159589019 ) ) ;
#73842 = CIRCLE ( 'NONE', #23411, 77.49899999999998101 ) ;
#73843 = CARTESIAN_POINT ( 'NONE',  ( -93.84685191531254134, 91.99731107132950569, 79.42989583420049371 ) ) ;
#73845 = EDGE_CURVE ( 'NONE', #38841, #50744, #67359, .T. ) ;
#73844 = CARTESIAN_POINT ( 'NONE',  ( 96.15314808468750130, -211.9973110713294489, 79.05947916753380866 ) ) ;
#73846 = ORIENTED_EDGE ( 'NONE', *, *, #62993, .F. ) ;
#73847 = EDGE_CURVE ( 'NONE', #39991, #67442, #32586, .T. ) ;
#73848 = DIRECTION ( 'NONE',  ( -1.000000000000000000, -0.000000000000000000, -0.000000000000000000 ) ) ;
#73849 = ORIENTED_EDGE ( 'NONE', *, *, #14935, .T. ) ;
#73850 = AXIS2_PLACEMENT_3D ( 'NONE', #41223, #1043, #57782 ) ;
#73851 = DIRECTION ( 'NONE',  ( 2.603472992746261562E-14, 2.546204323184492723E-14, -1.000000000000000000 ) ) ;
#73852 = VECTOR ( 'NONE', #56248, 1000.000000000000000 ) ;
#73853 = ORIENTED_EDGE ( 'NONE', *, *, #29761, .T. ) ;
#73854 = DIRECTION ( 'NONE',  ( 1.000000000000000000, 0.000000000000000000, -0.000000000000000000 ) ) ;
#73855 = VECTOR ( 'NONE', #65723, 999.9999999999998863 ) ;
#73856 = EDGE_CURVE ( 'NONE', #68580, #45509, #49322, .T. ) ;
#73857 = ADVANCED_FACE ( 'NONE', ( #49873 ), #20193, .T. ) ;
#73858 = VERTEX_POINT ( 'NONE', #38235 ) ;
#73859 = ORIENTED_EDGE ( 'NONE', *, *, #9748, .T. ) ;
#73860 = VECTOR ( 'NONE', #29247, 1000.000000000000000 ) ;
#73861 = ORIENTED_EDGE ( 'NONE', *, *, #24676, .T. ) ;
#73862 = CARTESIAN_POINT ( 'NONE',  ( 93.84685191531249870, -208.0026889286704943, 75.09072916753380866 ) ) ;
#73863 = ORIENTED_EDGE ( 'NONE', *, *, #69999, .T. ) ;
#73864 =( REPRESENTATION_RELATIONSHIP ('NONE','NONE', #31117, #31559 ) REPRESENTATION_RELATIONSHIP_WITH_TRANSFORMATION ( #19236 )SHAPE_REPRESENTATION_RELATIONSHIP( ) );
#73865 = DIRECTION ( 'NONE',  ( -1.000000000000000000, -0.000000000000000000, 0.000000000000000000 ) ) ;
#73866 = CARTESIAN_POINT ( 'NONE',  ( 10.00000000000000000, -33.00180498840060039, 17.80606268964528027 ) ) ;
#73867 = CARTESIAN_POINT ( 'NONE',  ( 94.99999999999998579, 92.66308142843935514, 87.73781250086715033 ) ) ;
#73868 = DIRECTION ( 'NONE',  ( 1.000000000000000000, 0.000000000000000000, 0.000000000000000000 ) ) ;
#73869 = CARTESIAN_POINT ( 'NONE',  ( 97.64999999999999147, -209.9999999999999716, 79.52249999999999375 ) ) ;
#73870 = VECTOR ( 'NONE', #56157, 1000.000000000000114 ) ;
#73871 = ORIENTED_EDGE ( 'NONE', *, *, #44205, .F. ) ;
#73872 = ORIENTED_EDGE ( 'NONE', *, *, #8249, .T. ) ;
#73873 = EDGE_LOOP ( 'NONE', ( #15030, #14351, #49652, #40523 ) ) ;
#73874 = ORIENTED_EDGE ( 'NONE', *, *, #36655, .T. ) ;
#73875 = CARTESIAN_POINT ( 'NONE',  ( 5.000000000000000000, -79.10210256391353312, -21.60688246758668640 ) ) ;
#73876 = SURFACE_STYLE_FILL_AREA ( #19777 ) ;
#73877 = DIRECTION ( 'NONE',  ( -1.000000000000000000, -0.000000000000000000, -0.000000000000000000 ) ) ;
#73878 = AXIS2_PLACEMENT_3D ( 'NONE', #12157, #23091, #56567 ) ;
#73879 = CYLINDRICAL_SURFACE ( 'NONE', #65245, 2.649999999999985700 ) ;
#73880 = CARTESIAN_POINT ( 'NONE',  ( -6.112675177960399608, -145.7853679859090903, 2.500000000000000000 ) ) ;
#73881 = DIRECTION ( 'NONE',  ( 1.000000000000000000, 0.000000000000000000, 0.000000000000000000 ) ) ;
#73882 = CARTESIAN_POINT ( 'NONE',  ( 11.99999999999999822, 0.000000000000000000, 0.000000000000000000 ) ) ;
#73883 = ORIENTED_EDGE ( 'NONE', *, *, #47444, .F. ) ;
#73884 = CARTESIAN_POINT ( 'NONE',  ( -92.34999999999999432, -211.5299782133524502, 83.99395833506763154 ) ) ;
#73885 = ORIENTED_EDGE ( 'NONE', *, *, #36188, .F. ) ;
#73886 = CARTESIAN_POINT ( 'NONE',  ( -10.00000000000000000, 0.000000000000000000, 0.000000000000000000 ) ) ;
#73887 = ORIENTED_EDGE ( 'NONE', *, *, #11058, .T. ) ;
#73889 = CARTESIAN_POINT ( 'NONE',  ( -95.00000000000002842, 93.05995642670501411, 80.39562500173431658 ) ) ;
#73888 = CARTESIAN_POINT ( 'NONE',  ( 97.64999999999997726, 88.47002178664753558, 83.35895833506762642 ) ) ;
#73890 = ORIENTED_EDGE ( 'NONE', *, *, #15692, .F. ) ;
#73891 = CARTESIAN_POINT ( 'NONE',  ( 94.99999999999998579, 87.33691857156068750, 84.24531250086715772 ) ) ;
#73892 = FACE_OUTER_BOUND ( 'NONE', #36526, .T. ) ;
#73894 = EDGE_CURVE ( 'NONE', #26343, #69721, #6156, .T. ) ;
#73893 = CARTESIAN_POINT ( 'NONE',  ( 10.00000000000000000, -73.95703589263958122, -23.16143007188506431 ) ) ;
#73895 = CARTESIAN_POINT ( 'NONE',  ( -100.0000000000260059, -214.9999999999999716, -74.99999999999349143 ) ) ;
#73896 = CARTESIAN_POINT ( 'NONE',  ( 11.99999999999999822, 75.54627589209944460, 17.28742895386110945 ) ) ;
#73897 = CARTESIAN_POINT ( 'NONE',  ( 92.34999999999999432, 90.00000000000002842, 90.00000000000000000 ) ) ;
#73898 = EDGE_LOOP ( 'NONE', ( #11573, #42064, #34588, #20123 ) ) ;
#73899 = DIRECTION ( 'NONE',  ( 1.000000000000000000, 0.000000000000000000, 0.000000000000000000 ) ) ;
#73900 = CARTESIAN_POINT ( 'NONE',  ( 0.000000000000000000, -77.32052557432837148, -5.256550761633697277 ) ) ;
#73901 = CARTESIAN_POINT ( 'NONE',  ( -3.000000000000000000, -13.04903810567675038, 19.60159698893425428 ) ) ;
#73902 = AXIS2_PLACEMENT_3D ( 'NONE', #29490, #64467, #52425 ) ;
#73903 = ORIENTED_EDGE ( 'NONE', *, *, #70158, .T. ) ;
#73904 = EDGE_LOOP ( 'NONE', ( #24990, #1653, #69381, #48840 ) ) ;
#73905 = EDGE_CURVE ( 'NONE', #24035, #71821, #1350, .T. ) ;
#73906 = CARTESIAN_POINT ( 'NONE',  ( 100.0010000000000474, -65.00000000000002842, -290.0000000000000568 ) ) ;
#73907 = EDGE_CURVE ( 'NONE', #33472, #23343, #26204, .T. ) ;
#73908 = CARTESIAN_POINT ( 'NONE',  ( 10.00000000000000000, -30.00120703465222149, 22.64427369931158296 ) ) ;
#73909 = CARTESIAN_POINT ( 'NONE',  ( 11.41210121379328335, -99.40233154247455616, 5.500000000000000000 ) ) ;
#73910 = CYLINDRICAL_SURFACE ( 'NONE', #58125, 23.50000000000000355 ) ;
#73911 = CARTESIAN_POINT ( 'NONE',  ( -92.69370383062498320, -211.3315407142195852, 81.17614583420048291 ) ) ;
#73912 = EDGE_LOOP ( 'NONE', ( #38124, #12233, #69664, #859 ) ) ;
#73913 = CARTESIAN_POINT ( 'NONE',  ( -97.30629616937501680, 91.33154071421968467, 89.58989583420047609 ) ) ;
#73914 = ORIENTED_EDGE ( 'NONE', *, *, #16716, .F. ) ;
#73915 = EDGE_CURVE ( 'NONE', #72049, #59443, #19319, .T. ) ;
#73916 = DIRECTION ( 'NONE',  ( -0.000000000000000000, -0.000000000000000000, 1.000000000000000000 ) ) ;
#73917 = DIRECTION ( 'NONE',  ( -1.000000000000000000, -0.000000000000000000, 0.000000000000000000 ) ) ;
#73918 = CYLINDRICAL_SURFACE ( 'NONE', #6927, 31.99999999999998579 ) ;
#73919 = CARTESIAN_POINT ( 'NONE',  ( 7.400000000000003908, 2.639109708933072986E-13, 23.50000000000042277 ) ) ;
#73920 = DIRECTION ( 'NONE',  ( 0.000000000000000000, 0.7431448254773862505, -0.6691306063588671194 ) ) ;
#73921 = DIRECTION ( 'NONE',  ( -0.000000000000000000, -0.000000000000000000, -1.000000000000000000 ) ) ;
#73922 = CIRCLE ( 'NONE', #51114, 77.49899999999999523 ) ;
#73923 = DIRECTION ( 'NONE',  ( -0.000000000000000000, -0.000000000000000000, -1.000000000000000000 ) ) ;
#73924 = CARTESIAN_POINT ( 'NONE',  ( -99.99999999999998579, -116.0000000000000000, -40.00000000000002132 ) ) ;
#73925 = CARTESIAN_POINT ( 'NONE',  ( 10.00000000000000000, 0.000000000000000000, 0.000000000000000000 ) ) ;
#73926 = DIRECTION ( 'NONE',  ( -1.000000000000000000, 0.000000000000000000, 0.000000000000000000 ) ) ;
#73927 = AXIS2_PLACEMENT_3D ( 'NONE', #67070, #44145, #17063 ) ;
#73928 = VECTOR ( 'NONE', #34613, 1000.000000000000114 ) ;
#73929 = EDGE_CURVE ( 'NONE', #43091, #60565, #51750, .T. ) ;
#73930 = DIRECTION ( 'NONE',  ( 0.000000000000000000, 0.000000000000000000, 1.000000000000000000 ) ) ;
#73931 = CARTESIAN_POINT ( 'NONE',  ( 94.99999999999998579, 92.66308142843932671, 89.64281250086715147 ) ) ;
#73932 = CARTESIAN_POINT ( 'NONE',  ( -94.99999999999997158, -212.6630814284392557, 89.32531250086715602 ) ) ;
#73933 = DIRECTION ( 'NONE',  ( 0.9730327541852497042, -0.2306669878475622604, 0.000000000000000000 ) ) ;
#73934 = ORIENTED_EDGE ( 'NONE', *, *, #632, .F. ) ;
#73935 = CARTESIAN_POINT ( 'NONE',  ( 10.00000000000000000, 25.88420570971400991, 27.13269053701105449 ) ) ;
#73936 = CARTESIAN_POINT ( 'NONE',  ( -97.30629616937501680, 91.33154071421968467, 80.06489583420047040 ) ) ;
#73937 = CIRCLE ( 'NONE', #41526, 37.49900000000000944 ) ;
#73939 = EDGE_CURVE ( 'NONE', #7213, #10916, #71316, .T. ) ;
#73938 = DIRECTION ( 'NONE',  ( 0.000000000000000000, 0.000000000000000000, 1.000000000000000000 ) ) ;
#73940 = EDGE_CURVE ( 'NONE', #71349, #42442, #60082, .T. ) ;
#73941 = EDGE_LOOP ( 'NONE', ( #10098, #21566, #32426, #35116 ) ) ;
#73942 = DIRECTION ( 'NONE',  ( 0.9966891607226786576, 0.08130631524009862554, 0.000000000000000000 ) ) ;
#73943 = EDGE_CURVE ( 'NONE', #23737, #11727, #46108, .T. ) ;
#73944 = DIRECTION ( 'NONE',  ( 1.000000000000000000, 0.000000000000000000, 0.000000000000000000 ) ) ;
#73945 = CYLINDRICAL_SURFACE ( 'NONE', #49168, 32.00000000000000000 ) ;
#73946 = DIRECTION ( 'NONE',  ( -1.000000000000000000, 3.061616997868382648E-16, 0.000000000000000000 ) ) ;
#73947 = CARTESIAN_POINT ( 'NONE',  ( 96.15314808468748708, -208.0026889286704943, 74.98489583420048632 ) ) ;
#73948 = ORIENTED_EDGE ( 'NONE', *, *, #65470, .F. ) ;
#73949 = VERTEX_POINT ( 'NONE', #34442 ) ;
#73950 = CARTESIAN_POINT ( 'NONE',  ( 97.30629616937498838, -209.7238243954290056, 74.79348190356851944 ) ) ;
#73951 = DIRECTION ( 'NONE',  ( 1.000000000000000000, 0.000000000000000000, 0.000000000000000000 ) ) ;
#73952 = CARTESIAN_POINT ( 'NONE',  ( -4.749999999999999112, 0.000000000000000000, 0.000000000000000000 ) ) ;
#73953 = FACE_OUTER_BOUND ( 'NONE', #16192, .T. ) ;
#73954 = VECTOR ( 'NONE', #2755, 1000.000000000000000 ) ;
#73955 = DIRECTION ( 'NONE',  ( 0.000000000000000000, 0.000000000000000000, 1.000000000000000000 ) ) ;
#73956 = CARTESIAN_POINT ( 'NONE',  ( 95.00000000000000000, -213.0599564267049857, 88.25374999999999659 ) ) ;
#73957 = ORIENTED_EDGE ( 'NONE', *, *, #19463, .F. ) ;
#73958 = EDGE_LOOP ( 'NONE', ( #42353, #51565, #6346, #6611 ) ) ;
#73959 = DIRECTION ( 'NONE',  ( -4.476705744456277943E-17, 1.000000000000000000, -0.000000000000000000 ) ) ;
#73960 = ORIENTED_EDGE ( 'NONE', *, *, #40658, .F. ) ;
#73961 = ORIENTED_EDGE ( 'NONE', *, *, #26121, .T. ) ;
#73962 = FACE_OUTER_BOUND ( 'NONE', #57538, .T. ) ;
#73963 = AXIS2_PLACEMENT_3D ( 'NONE', #64253, #40956, #34 ) ;
#73964 = DIRECTION ( 'NONE',  ( 0.000000000000000000, 0.000000000000000000, 1.000000000000000000 ) ) ;
#73965 = AXIS2_PLACEMENT_3D ( 'NONE', #32117, #62192, #5067 ) ;
#73966 = ORIENTED_EDGE ( 'NONE', *, *, #42982, .F. ) ;
#73967 = DIRECTION ( 'NONE',  ( -0.000000000000000000, -0.7431448254773870277, -0.6691306063588662312 ) ) ;
#73968 = CARTESIAN_POINT ( 'NONE',  ( 95.00000000000000000, -213.0599564267049857, 77.53812500173428646 ) ) ;
#73969 = CARTESIAN_POINT ( 'NONE',  ( 94.99999999999998579, 86.94004357329500010, 80.63375000000000625 ) ) ;
#73970 = ORIENTED_EDGE ( 'NONE', *, *, #37130, .F. ) ;
#73971 = FACE_OUTER_BOUND ( 'NONE', #61913, .T. ) ;
#73972 = VERTEX_POINT ( 'NONE', #28810 ) ;
#73973 = CARTESIAN_POINT ( 'NONE',  ( 10.00000000000000000, 0.000000000000000000, 0.000000000000000000 ) ) ;
#73974 = VECTOR ( 'NONE', #53488, 1000.000000000000000 ) ;
#73975 = ORIENTED_EDGE ( 'NONE', *, *, #72948, .F. ) ;
#73976 = CIRCLE ( 'NONE', #41570, 16.00000000000000000 ) ;
#73977 = CARTESIAN_POINT ( 'NONE',  ( 96.32499999999998863, -212.2949673200287179, 88.38604166840097776 ) ) ;
#73978 = CARTESIAN_POINT ( 'NONE',  ( -95.00000000000002842, 87.33691857156074434, 80.43531250086715545 ) ) ;
#73979 = CARTESIAN_POINT ( 'NONE',  ( 97.30629616937498838, 90.00000000000002842, 77.26031250086714408 ) ) ;
#73980 = ORIENTED_EDGE ( 'NONE', *, *, #66629, .T. ) ;
#73981 = LINE ( 'NONE', #22496, #47793 ) ;
#73982 = CYLINDRICAL_SURFACE ( 'NONE', #61712, 77.49899999999999523 ) ;
#73983 = EDGE_CURVE ( 'NONE', #73431, #16620, #57385, .T. ) ;
#73984 = CARTESIAN_POINT ( 'NONE',  ( 10.00000000000000000, 0.000000000000000000, 0.000000000000000000 ) ) ;
#73985 = CARTESIAN_POINT ( 'NONE',  ( 11.99999999999999822, -34.44570377933549565, -69.42325613327476219 ) ) ;
#73986 = EDGE_LOOP ( 'NONE', ( #6037, #10023, #22760, #1507 ) ) ;
#73987 = CARTESIAN_POINT ( 'NONE',  ( -5.000000000000000000, -2.886751345948137981, -5.553418012614792509 ) ) ;
#73988 = CARTESIAN_POINT ( 'NONE',  ( -92.69370383062498320, -208.6684592857803011, 77.94822916753381037 ) ) ;
#73989 = VERTEX_POINT ( 'NONE', #5899 ) ;
#73990 = ORIENTED_EDGE ( 'NONE', *, *, #72375, .F. ) ;
#73991 = EDGE_CURVE ( 'NONE', #33698, #8597, #15738, .T. ) ;
#73992 = CARTESIAN_POINT ( 'NONE',  ( 0.000000000000000000, 0.000000000000000000, 0.000000000000000000 ) ) ;
#73993 = EDGE_CURVE ( 'NONE', #8951, #1496, #45763, .T. ) ;
#73994 = VERTEX_POINT ( 'NONE', #287 ) ;
#73995 = DIRECTION ( 'NONE',  ( 1.000000000000000000, -0.000000000000000000, 0.000000000000000000 ) ) ;
#73996 = CARTESIAN_POINT ( 'NONE',  ( 0.000000000000000000, -39.78640506895559525, -66.50666863322042843 ) ) ;
#73997 = ORIENTED_EDGE ( 'NONE', *, *, #52053, .F. ) ;
#73998 = CARTESIAN_POINT ( 'NONE',  ( -92.69370383062498320, -209.9999999999999716, 76.62531250086713897 ) ) ;
#73999 = ORIENTED_EDGE ( 'NONE', *, *, #21831, .T. ) ;
#74000 = DIRECTION ( 'NONE',  ( -1.000000000000000000, 0.000000000000000000, 0.000000000000000000 ) ) ;
#74001 = CARTESIAN_POINT ( 'NONE',  ( 0.000000000000000000, -77.16300072079681627, 27.74655509720641078 ) ) ;
#74002 = DIRECTION ( 'NONE',  ( 0.000000000000000000, -0.5000000000000011102, -0.8660254037844380415 ) ) ;
#74003 = DIRECTION ( 'NONE',  ( 0.000000000000000000, -0.9781476007338070211, 0.2079116908177532363 ) ) ;
#74004 = EDGE_CURVE ( 'NONE', #43826, #28647, #23182, .T. ) ;
#74005 = EDGE_CURVE ( 'NONE', #51313, #41146, #70944, .T. ) ;
#74006 = ADVANCED_BREP_SHAPE_REPRESENTATION ( '', ( #11785, #43395 ), #47140 ) ;
#74007 = CARTESIAN_POINT ( 'NONE',  ( -92.35000000000003695, 90.00000000000004263, 81.42749999999999488 ) ) ;
#74008 = SURFACE_STYLE_USAGE ( .BOTH. , #68009 ) ;
#74009 = CARTESIAN_POINT ( 'NONE',  ( 92.69370383062498320, 88.66845928578035796, 83.34572916753381833 ) ) ;
#74010 = DIRECTION ( 'NONE',  ( -1.000000000000000000, -0.000000000000000000, -0.000000000000000000 ) ) ;
#74011 = LINE ( 'NONE', #16887, #62610 ) ;
#74012 = DIRECTION ( 'NONE',  ( -1.000000000000000000, 0.000000000000000000, -0.000000000000000000 ) ) ;
#74013 = CARTESIAN_POINT ( 'NONE',  ( 0.000000000000000000, 10.74501242461333028, -35.92658777277499382 ) ) ;
#74014 = CARTESIAN_POINT ( 'NONE',  ( 10.00000000000000000, 0.6853352020790449695, 37.58145647212454321 ) ) ;
#74015 = CARTESIAN_POINT ( 'NONE',  ( 0.3476802294499899415, 5.572769417831398897, -1.687189089856316215 ) ) ;
#74016 = DIRECTION ( 'NONE',  ( 0.000000000000000000, -0.000000000000000000, 1.000000000000000000 ) ) ;
#74017 = LINE ( 'NONE', #33805, #9203 ) ;
#74018 = EDGE_CURVE ( 'NONE', #50553, #42920, #63404, .T. ) ;
#74019 = AXIS2_PLACEMENT_3D ( 'NONE', #37217, #30438, #2296 ) ;
#74020 = DIRECTION ( 'NONE',  ( 1.000000000000000000, 0.000000000000000000, 0.000000000000000000 ) ) ;
#74021 = LINE ( 'NONE', #40198, #73328 ) ;
#74022 = DIRECTION ( 'NONE',  ( -1.000000000000000000, -0.000000000000000000, 0.000000000000000000 ) ) ;
#74023 = DIRECTION ( 'NONE',  ( 1.000000000000000000, 1.427937372958405461E-15, 7.962523111839130290E-16 ) ) ;
#74024 = VECTOR ( 'NONE', #397, 1000.000000000000000 ) ;
#74025 = CARTESIAN_POINT ( 'NONE',  ( -97.64999999999994884, -211.5299782133524502, 84.33791666666667197 ) ) ;
#74026 = CIRCLE ( 'NONE', #49974, 16.00000000000000000 ) ;
#74027 = CARTESIAN_POINT ( 'NONE',  ( 96.32499999999998863, 87.70503267997126784, 85.76666666666665151 ) ) ;
#74028 = ADVANCED_FACE ( 'NONE', ( #5162 ), #11510, .F. ) ;
#74029 = EDGE_CURVE ( 'NONE', #49489, #14738, #34947, .T. ) ;
#74030 = CIRCLE ( 'NONE', #46459, 77.49899999999999523 ) ;
#74031 =( BOUNDED_CURVE ( )  B_SPLINE_CURVE ( 2, ( #73060, #68932, #23075, #44522, #74187, #56915, #22704 ),
 .UNSPECIFIED., .F., .F. ) 
 B_SPLINE_CURVE_WITH_KNOTS ( ( 3, 2, 2, 3 ),
 ( 0.02083333333333322115, 0.02777777777777762705, 0.03472222222222204335, 0.04166666666666644231 ),
 .UNSPECIFIED. ) 
 CURVE ( )  GEOMETRIC_REPRESENTATION_ITEM ( )  RATIONAL_B_SPLINE_CURVE ( ( 1.000000000000002220, 0.8660254037844365982, 1.000000000000000000, 0.8660254037844387076, 1.000000000000000000, 0.8660254037844430375, 0.9999999999999956701 ) ) 
 REPRESENTATION_ITEM ( '' )  );
#74032 = VERTEX_POINT ( 'NONE', #50245 ) ;
#74033 = CYLINDRICAL_SURFACE ( 'NONE', #57589, 16.00000000000000000 ) ;
#74034 = DIRECTION ( 'NONE',  ( 0.000000000000000000, -0.8090169943749530024, 0.5877852522924653655 ) ) ;
#74035 = DIRECTION ( 'NONE',  ( 0.000000000000000000, 0.9510565162951503115, 0.3090169943749573878 ) ) ;
#74036 = FACE_OUTER_BOUND ( 'NONE', #11132, .T. ) ;
#74037 = CARTESIAN_POINT ( 'NONE',  ( 93.84685191531251292, -211.9973110713294489, 86.09739583420049769 ) ) ;
#74038 = CIRCLE ( 'NONE', #65634, 77.49900000000000944 ) ;
#74039 = ORIENTED_EDGE ( 'NONE', *, *, #38096, .T. ) ;
#74040 = ORIENTED_EDGE ( 'NONE', *, *, #64429, .T. ) ;
#74041 = DIRECTION ( 'NONE',  ( -1.000000000000000000, -0.000000000000000000, 0.000000000000000000 ) ) ;
#74042 = VERTEX_POINT ( 'NONE', #17163 ) ;
#74043 = DIRECTION ( 'NONE',  ( 1.000000000000000000, 0.000000000000000000, 0.000000000000000000 ) ) ;
#74044 = CARTESIAN_POINT ( 'NONE',  ( 97.30629616937498838, -211.3315407142195852, 77.20739583420046870 ) ) ;
#74045 = ORIENTED_EDGE ( 'NONE', *, *, #71253, .T. ) ;
#74046 = CARTESIAN_POINT ( 'NONE',  ( 93.84685191531251292, -211.9973110713294489, 83.55739583420049144 ) ) ;
#74047 = ORIENTED_EDGE ( 'NONE', *, *, #29369, .F. ) ;
#74048 = CARTESIAN_POINT ( 'NONE',  ( 92.35000000009272014, 90.00001381026685010, 80.55392363656929433 ) ) ;
#74049 = EDGE_LOOP ( 'NONE', ( #62099, #15818, #45897, #6238 ) ) ;
#74050 = VERTEX_POINT ( 'NONE', #61923 ) ;
#74051 = CARTESIAN_POINT ( 'NONE',  ( -97.30629616937501680, 90.00000000000004263, 75.19656250086714522 ) ) ;
#74052 = AXIS2_PLACEMENT_3D ( 'NONE', #37926, #21346, #35244 ) ;
#74053 = DIRECTION ( 'NONE',  ( 0.000000000000000000, 0.8910065241883688980, -0.4539904997395445840 ) ) ;
#74054 = ORIENTED_EDGE ( 'NONE', *, *, #61010, .T. ) ;
#74055 = FACE_OUTER_BOUND ( 'NONE', #43269, .T. ) ;
#74056 = CARTESIAN_POINT ( 'NONE',  ( 97.64999999999997726, -208.4700217866474645, 88.54479166840097548 ) ) ;
#74057 = VERTEX_POINT ( 'NONE', #39357 ) ;
#74058 = CARTESIAN_POINT ( 'NONE',  ( -0.0004442498507136653329, 0.001194404164628348752, -70.59999999999999432 ) ) ;
#74059 = EDGE_CURVE ( 'NONE', #19568, #28732, #34825, .T. ) ;
#74060 = ORIENTED_EDGE ( 'NONE', *, *, #24447, .T. ) ;
#74061 = DIRECTION ( 'NONE',  ( 0.000000000000000000, 0.9969173337331282969, -0.07845909572784179331 ) ) ;
#74062 = VECTOR ( 'NONE', #69123, 1000.000000000000000 ) ;
#74063 = ORIENTED_EDGE ( 'NONE', *, *, #34023, .T. ) ;
#74064 = ADVANCED_FACE ( 'NONE', ( #10781 ), #57761, .T. ) ;
#74065 = VECTOR ( 'NONE', #63636, 1000.000000000000000 ) ;
#74066 = ORIENTED_EDGE ( 'NONE', *, *, #5820, .T. ) ;
#74067 = ORIENTED_EDGE ( 'NONE', *, *, #36475, .F. ) ;
#74068 = CARTESIAN_POINT ( 'NONE',  ( -11.63999999999999702, 0.000000000000000000, 0.000000000000000000 ) ) ;
#74069 = FACE_OUTER_BOUND ( 'NONE', #43545, .T. ) ;
#74071 = ADVANCED_FACE ( 'NONE', ( #67554 ), #27309, .F. ) ;
#74070 = ORIENTED_EDGE ( 'NONE', *, *, #71800, .T. ) ;
#74072 = ORIENTED_EDGE ( 'NONE', *, *, #30194, .F. ) ;
#74073 = AXIS2_PLACEMENT_3D ( 'NONE', #42207, #54585, #13250 ) ;
#74074 = ORIENTED_EDGE ( 'NONE', *, *, #33530, .F. ) ;
#74075 = AXIS2_PLACEMENT_3D ( 'NONE', #6588, #58829, #12213 ) ;
#74076 = CARTESIAN_POINT ( 'NONE',  ( 10.00000000000000000, 6.555932627142952995, -37.01155633439051940 ) ) ;
#74077 = EDGE_CURVE ( 'NONE', #12380, #73300, #27698, .T. ) ;
#74078 = DIRECTION ( 'NONE',  ( -1.000000000000000000, -0.000000000000000000, 0.000000000000000000 ) ) ;
#74079 = CARTESIAN_POINT ( 'NONE',  ( -92.69370383062502583, 88.66845928578038638, 75.46114583420049371 ) ) ;
#74080 = VERTEX_POINT ( 'NONE', #45002 ) ;
#74081 = VECTOR ( 'NONE', #30731, 1000.000000000000000 ) ;
#74082 = CARTESIAN_POINT ( 'NONE',  ( 92.69370383062498320, 90.00000000000002842, 75.67281250086713840 ) ) ;
#74083 = ORIENTED_EDGE ( 'NONE', *, *, #42860, .F. ) ;
#74084 = FACE_OUTER_BOUND ( 'NONE', #68187, .T. ) ;
#74085 = CARTESIAN_POINT ( 'NONE',  ( -93.84685191531248449, -208.0026889286704943, 86.89114583420047211 ) ) ;
#74086 = ORIENTED_EDGE ( 'NONE', *, *, #22413, .T. ) ;
#74087 = CYLINDRICAL_SURFACE ( 'NONE', #37436, 31.99999999999999289 ) ;
#74089 = AXIS2_PLACEMENT_3D ( 'NONE', #5267, #56388, #56763 ) ;
#74088 = DIRECTION ( 'NONE',  ( -1.000000000000000000, -0.000000000000000000, -0.000000000000000000 ) ) ;
#74090 = CARTESIAN_POINT ( 'NONE',  ( 50.00005079999999680, 1.530808498934191521E-15, -12.50000000000000000 ) ) ;
#74091 = CARTESIAN_POINT ( 'NONE',  ( -92.69370383062498320, -209.9999999999999716, 76.62531250086713897 ) ) ;
#74092 = EDGE_CURVE ( 'NONE', #9907, #70250, #13772, .T. ) ;
#74093 = DIRECTION ( 'NONE',  ( -1.000000000000000000, 0.000000000000000000, 0.000000000000000000 ) ) ;
#74094 = CARTESIAN_POINT ( 'NONE',  ( 0.000000000000000000, 0.000000000000000000, 20.00000000000000000 ) ) ;
#74095 = CIRCLE ( 'NONE', #8032, 31.99999999999999289 ) ;
#74096 = CARTESIAN_POINT ( 'NONE',  ( -95.00000000000002842, 86.94004357329504273, 85.15812500173429100 ) ) ;
#74097 = DIRECTION ( 'NONE',  ( 0.000000000000000000, 0.3826834323650907810, -0.9238795325112864054 ) ) ;
#74098 = AXIS2_PLACEMENT_3D ( 'NONE', #68517, #11712, #69614 ) ;
#74099 = CARTESIAN_POINT ( 'NONE',  ( 10.00000000000000000, -37.16516213103273714, -4.992566952385376844 ) ) ;
#74100 = CARTESIAN_POINT ( 'NONE',  ( -93.84685191531254134, 91.99731107132950569, 81.81114583420047381 ) ) ;
#74101 = LINE ( 'NONE', #22613, #61096 ) ;
#74102 = CYLINDRICAL_SURFACE ( 'NONE', #4979, 32.00000000000000000 ) ;
#74103 = EDGE_CURVE ( 'NONE', #5866, #40399, #62681, .T. ) ;
#74104 = B_SPLINE_CURVE_WITH_KNOTS ( 'NONE', 3,
 ( #34889, #63841, #63469, #36353, #69462, #11941 ),
 .UNSPECIFIED., .F., .F.,
 ( 4, 2, 4 ),
 ( 0.000000000000000000, 0.0008269033587273426789, 0.001653806717454685358 ),
 .UNSPECIFIED. ) ;
#74105 = EDGE_LOOP ( 'NONE', ( #61016, #17383, #34221, #22202 ) ) ;
#74106 = EDGE_CURVE ( 'NONE', #48711, #42829, #54116, .T. ) ;
#74107 = CYLINDRICAL_SURFACE ( 'NONE', #26790, 37.49900000000000233 ) ;
#74108 = EDGE_CURVE ( 'NONE', #38564, #973, #64883, .T. ) ;
#74109 = CARTESIAN_POINT ( 'NONE',  ( 10.00000000000000000, 37.22597642581158084, 10.79786254984347593 ) ) ;
#74110 = CARTESIAN_POINT ( 'NONE',  ( 0.000000000000000000, 81.90746397400387480, 3.894527615418180044 ) ) ;
#74111 = DIRECTION ( 'NONE',  ( -1.000000000000000000, 0.000000000000000000, 0.000000000000000000 ) ) ;
#74112 = CARTESIAN_POINT ( 'NONE',  ( 0.000000000000000000, 0.000000000000000000, 0.000000000000000000 ) ) ;
#74113 = CARTESIAN_POINT ( 'NONE',  ( -97.64996763243314604, 91.52999690077599837, 87.48645704240065868 ) ) ;
#74114 = CARTESIAN_POINT ( 'NONE',  ( -92.69370383062498320, -211.3315407142195852, 80.54114583420049200 ) ) ;
#74115 = CARTESIAN_POINT ( 'NONE',  ( 0.000000000000000000, 0.000000000000000000, 0.000000000000000000 ) ) ;
#74116 = EDGE_CURVE ( 'NONE', #74042, #30840, #72126, .T. ) ;
#74117 = ORIENTED_EDGE ( 'NONE', *, *, #50647, .F. ) ;
#74118 =( GEOMETRIC_REPRESENTATION_CONTEXT ( 3 ) GLOBAL_UNCERTAINTY_ASSIGNED_CONTEXT ( ( #54153 ) ) GLOBAL_UNIT_ASSIGNED_CONTEXT ( ( #10159, #33082, #17288 ) ) REPRESENTATION_CONTEXT ( 'NONE', 'WORKASPACE' ) );
#74119 = CARTESIAN_POINT ( 'NONE',  ( 24.95699195200416654, -110.9640411295978595, 5.500000000000000000 ) ) ;
#74120 = FACE_OUTER_BOUND ( 'NONE', #16086, .T. ) ;
#74121 = CARTESIAN_POINT ( 'NONE',  ( 5.000000000000002665, 81.90746397400387480, 3.894527615418187150 ) ) ;
#74122 = VECTOR ( 'NONE', #62827, 1000.000000000000000 ) ;
#74123 = ADVANCED_FACE ( 'NONE', ( #58870 ), #65255, .T. ) ;
#74124 = DIRECTION ( 'NONE',  ( 0.1736481776669309418, 0.9848077530122080203, -0.000000000000000000 ) ) ;
#74125 = DIRECTION ( 'NONE',  ( 0.000000000000000000, 0.000000000000000000, 1.000000000000000000 ) ) ;
#74126 = VECTOR ( 'NONE', #7890, 1000.000000000000000 ) ;
#74127 = CIRCLE ( 'NONE', #65719, 32.00000000000000000 ) ;
#74128 = DIRECTION ( 'NONE',  ( -1.000000000000000000, 0.000000000000000000, -0.000000000000000000 ) ) ;
#74129 = ORIENTED_EDGE ( 'NONE', *, *, #18099, .F. ) ;
#74130 = FACE_OUTER_BOUND ( 'NONE', #58235, .T. ) ;
#74131 = FACE_OUTER_BOUND ( 'NONE', #72493, .T. ) ;
#74132 = ORIENTED_EDGE ( 'NONE', *, *, #34309, .T. ) ;
#74133 = CARTESIAN_POINT ( 'NONE',  ( 96.15314808468750130, -211.9973110713294489, 89.21947916753380525 ) ) ;
#74134 = CARTESIAN_POINT ( 'NONE',  ( -97.64999999950680376, -210.0000320386661485, 83.73041644189096644 ) ) ;
#74135 = ORIENTED_EDGE ( 'NONE', *, *, #24228, .F. ) ;
#74136 = CARTESIAN_POINT ( 'NONE',  ( 0.000000000000000000, -35.53030884539094103, 12.26510123303246935 ) ) ;
#74137 = EDGE_LOOP ( 'NONE', ( #2808, #3096, #5669, #21257 ) ) ;
#74138 = PLANE ( 'NONE',  #27402 ) ;
#74139 = ORIENTED_EDGE ( 'NONE', *, *, #70797, .T. ) ;
#74140 = DIRECTION ( 'NONE',  ( -0.5000000000000042188, 1.060575238724903710E-16, -0.8660254037844361541 ) ) ;
#74141 = VECTOR ( 'NONE', #32238, 1000.000000000000000 ) ;
#74142 = VERTEX_POINT ( 'NONE', #41206 ) ;
#74143 = CARTESIAN_POINT ( 'NONE',  ( 10.00000000000000000, -17.67226234102801286, -33.17418723428327354 ) ) ;
#74144 = ORIENTED_EDGE ( 'NONE', *, *, #43294, .F. ) ;
#74145 = ORIENTED_EDGE ( 'NONE', *, *, #22924, .F. ) ;
#74146 = CARTESIAN_POINT ( 'NONE',  ( 7.103376864691351012E-17, -120.0000000000000000, -85.59999999999999432 ) ) ;
#74147 = AXIS2_PLACEMENT_3D ( 'NONE', #3904, #44861, #9524 ) ;
#74148 = EDGE_LOOP ( 'NONE', ( #30996, #27524, #22753, #18326 ) ) ;
#74149 = ORIENTED_EDGE ( 'NONE', *, *, #55222, .T. ) ;
#74150 = CARTESIAN_POINT ( 'NONE',  ( 92.34999999999999432, 88.47002178664753558, 89.41791666666667027 ) ) ;
#74151 = CARTESIAN_POINT ( 'NONE',  ( 92.34999999999999432, 90.00000000000002842, 77.93499999999998806 ) ) ;
#74152 = LINE ( 'NONE', #61407, #22541 ) ;
#74153 = EDGE_LOOP ( 'NONE', ( #72545, #5315 ) ) ;
#74154 = ORIENTED_EDGE ( 'NONE', *, *, #42132, .T. ) ;
#74155 = ADVANCED_FACE ( 'NONE', ( #12617 ), #53225, .F. ) ;
#74156 = ORIENTED_EDGE ( 'NONE', *, *, #1936, .T. ) ;
#74157 = CARTESIAN_POINT ( 'NONE',  ( 96.15314808468748708, 91.99731107132950569, 83.71614583420047495 ) ) ;
#74158 = ORIENTED_EDGE ( 'NONE', *, *, #39539, .F. ) ;
#74159 = CARTESIAN_POINT ( 'NONE',  ( 97.30629616937498838, -211.3315407142195852, 84.19239583420046813 ) ) ;
#74160 = DIRECTION ( 'NONE',  ( 1.000000000000000000, 0.000000000000000000, -5.551115123125782702E-17 ) ) ;
#74161 = CARTESIAN_POINT ( 'NONE',  ( 5.000000000000000000, -63.97538442413463855, 51.29473840253199768 ) ) ;
#74162 = ADVANCED_FACE ( 'NONE', ( #13361 ), #1759, .F. ) ;
#74163 = DIRECTION ( 'NONE',  ( -1.000000000000000000, 0.000000000000000000, -0.000000000000000000 ) ) ;
#74164 = CARTESIAN_POINT ( 'NONE',  ( -97.64999999996642543, 89.99999234487438571, 78.01464417100932280 ) ) ;
#74165 = FACE_OUTER_BOUND ( 'NONE', #4543, .T. ) ;
#74166 = DIRECTION ( 'NONE',  ( 0.000000000000000000, -1.000000000000000000, -1.047444401652940007E-14 ) ) ;
#74167 = EDGE_CURVE ( 'NONE', #64121, #48813, #23540, .T. ) ;
#74168 = DIRECTION ( 'NONE',  ( -1.000000000000000000, 0.000000000000000000, -0.000000000000000000 ) ) ;
#74169 = ADVANCED_FACE ( 'NONE', ( #35553 ), #58485, .T. ) ;
#74170 = CARTESIAN_POINT ( 'NONE',  ( -94.99999999999997158, -207.3369185715606307, 86.30906250086715659 ) ) ;
#74171 = CARTESIAN_POINT ( 'NONE',  ( -97.30629616937501680, 88.66845928578038638, 85.40947916753380298 ) ) ;
#74172 = ORIENTED_EDGE ( 'NONE', *, *, #8569, .F. ) ;
#74174 = CARTESIAN_POINT ( 'NONE',  ( -92.69370383062502583, 88.66845928578038638, 84.82739583420045903 ) ) ;
#74173 = CARTESIAN_POINT ( 'NONE',  ( 94.99999999999998579, 92.66308142843935514, 85.67406250086715147 ) ) ;
#74175 = ORIENTED_EDGE ( 'NONE', *, *, #43327, .T. ) ;
#74176 = DIRECTION ( 'NONE',  ( -1.000000000000000000, -0.000000000000000000, 0.000000000000000000 ) ) ;
#74177 = AXIS2_PLACEMENT_3D ( 'NONE', #1154, #11633, #69888 ) ;
#74178 = DIRECTION ( 'NONE',  ( -1.000000000000000000, -0.000000000000000000, -0.000000000000000000 ) ) ;
#74179 = DIRECTION ( 'NONE',  ( -2.603472992746261562E-14, -2.546204323184492723E-14, 1.000000000000000000 ) ) ;
#74180 = CARTESIAN_POINT ( 'NONE',  ( 5.999999999999999112, -77.16300072079641836, -27.74655509720751922 ) ) ;
#74181 = LINE ( 'NONE', #9554, #57878 ) ;
#74182 = AXIS2_PLACEMENT_3D ( 'NONE', #55896, #14180, #4410 ) ;
#74183 = AXIS2_PLACEMENT_3D ( 'NONE', #29533, #42323, #52473 ) ;
#74184 = CARTESIAN_POINT ( 'NONE',  ( 0.000000000000000000, -55.38113227695820484, 54.21277698773656084 ) ) ;
#74185 = DIRECTION ( 'NONE',  ( 1.000000000000000000, -0.000000000000000000, 0.000000000000000000 ) ) ;
#74186 = DIRECTION ( 'NONE',  ( 0.9918136447140100120, -0.1276937514489704939, 0.000000000000000000 ) ) ;
#74187 = CARTESIAN_POINT ( 'NONE',  ( 93.67499999999999716, 87.70503267997126784, 89.47083333333333144 ) ) ;
#74188 = ORIENTED_EDGE ( 'NONE', *, *, #20410, .T. ) ;
#74189 = VECTOR ( 'NONE', #52842, 1000.000000000000000 ) ;
#74190 = EDGE_CURVE ( 'NONE', #71438, #70238, #37326, .T. ) ;
#74191 = ORIENTED_EDGE ( 'NONE', *, *, #72738, .F. ) ;
#74192 = AXIS2_PLACEMENT_3D ( 'NONE', #68862, #30461, #53410 ) ;
#74193 = EDGE_CURVE ( 'NONE', #36080, #28680, #2128, .T. ) ;
#74194 = CARTESIAN_POINT ( 'NONE',  ( -97.65000000000001990, 91.52997821335253548, 79.15208333333332291 ) ) ;
#74195 = DIRECTION ( 'NONE',  ( -1.000000000000000000, -0.000000000000000000, 0.000000000000000000 ) ) ;
#74196 = LINE ( 'NONE', #64043, #62227 ) ;
#74197 = DIRECTION ( 'NONE',  ( 2.603472992746261562E-14, 2.546204323184492723E-14, -1.000000000000000000 ) ) ;
#74198 = CARTESIAN_POINT ( 'NONE',  ( -97.64999999999996305, -209.9999999999999716, 90.00000000000000000 ) ) ;
#74199 = DIRECTION ( 'NONE',  ( -0.000000000000000000, -0.000000000000000000, 1.000000000000000000 ) ) ;
#74200 = CARTESIAN_POINT ( 'NONE',  ( 5.000000000000002665, 15.33399622253481986, 80.55351364060595643 ) ) ;
#74201 = ORIENTED_EDGE ( 'NONE', *, *, #16571, .T. ) ;
#74202 = CARTESIAN_POINT ( 'NONE',  ( -96.15314808468751551, 88.00268892867056536, 77.68364583420047609 ) ) ;
#74203 = DIRECTION ( 'NONE',  ( -1.000000000000000000, -0.000000000000000000, -0.000000000000000000 ) ) ;
#74204 = EDGE_CURVE ( 'NONE', #9966, #44223, #14490, .T. ) ;
#74205 = EDGE_CURVE ( 'NONE', #59562, #71472, #24288, .T. ) ;
#74206 = CARTESIAN_POINT ( 'NONE',  ( 0.000000000000000000, -0.8299999999999999600, -1.199999999999999956 ) ) ;
#74207 = FACE_OUTER_BOUND ( 'NONE', #50286, .T. ) ;
#74208 = FACE_OUTER_BOUND ( 'NONE', #48339, .T. ) ;
#74209 = DIRECTION ( 'NONE',  ( 0.000000000000000000, 0.000000000000000000, 1.000000000000000000 ) ) ;
#74210 = LINE ( 'NONE', #10686, #43035 ) ;
#74211 = VECTOR ( 'NONE', #72286, 1000.000000000000000 ) ;
#74212 = CIRCLE ( 'NONE', #45405, 16.00000000000000000 ) ;
#74213 = CIRCLE ( 'NONE', #14150, 77.49899999999999523 ) ;
#74214 = CARTESIAN_POINT ( 'NONE',  ( 92.69370383062498320, 90.00000000000002842, 77.10156250086714635 ) ) ;
#74215 = CARTESIAN_POINT ( 'NONE',  ( -97.30629616937497417, -208.6684592857803295, 79.58864583420049144 ) ) ;
#74216 = DIRECTION ( 'NONE',  ( -1.000000000000000000, -0.000000000000000000, 0.000000000000000000 ) ) ;
#74217 = ORIENTED_EDGE ( 'NONE', *, *, #15958, .F. ) ;
#74218 = DIRECTION ( 'NONE',  ( 0.000000000000000000, 0.000000000000000000, 1.000000000000000000 ) ) ;
#74219 = CARTESIAN_POINT ( 'NONE',  ( -92.34999999999999432, -208.4700217866474645, 75.13041666666666174 ) ) ;
#74220 = CARTESIAN_POINT ( 'NONE',  ( 0.000000000000000000, 81.34940948281337114, 10.30890764327411979 ) ) ;
#74221 = CARTESIAN_POINT ( 'NONE',  ( -95.00000000000002842, 87.33691857156074434, 77.89531250086714920 ) ) ;
#74222 = CARTESIAN_POINT ( 'NONE',  ( 92.69370383062501162, -208.6684592857803011, 81.33489583420048064 ) ) ;
#74223 = ORIENTED_EDGE ( 'NONE', *, *, #69141, .T. ) ;
#74224 = CARTESIAN_POINT ( 'NONE',  ( -6.782329983125270800, 10.49999999999999467, -20.00000000000000000 ) ) ;
#74225 = EDGE_LOOP ( 'NONE', ( #67218, #38285, #2999 ) ) ;
#74226 = CIRCLE ( 'NONE', #41815, 42.00000000000000000 ) ;
#74227 = ORIENTED_EDGE ( 'NONE', *, *, #15604, .T. ) ;
#74228 = AXIS2_PLACEMENT_3D ( 'NONE', #35185, #1016, #69761 ) ;
#74229 = CIRCLE ( 'NONE', #41821, 32.00000000000000000 ) ;
#74230 = CARTESIAN_POINT ( 'NONE',  ( 10.00000000000000000, 30.84782396557248418, -21.32104025579081252 ) ) ;
#74231 = VECTOR ( 'NONE', #71133, 1000.000000000000114 ) ;
#74232 = ORIENTED_EDGE ( 'NONE', *, *, #31000, .T. ) ;
#74233 = EDGE_LOOP ( 'NONE', ( #52617, #33239, #38835, #31695 ) ) ;
#74234 = AXIS2_PLACEMENT_3D ( 'NONE', #4805, #37240, #42142 ) ;
#74235 = ORIENTED_EDGE ( 'NONE', *, *, #9435, .T. ) ;
#74236 = DIRECTION ( 'NONE',  ( 0.000000000000000000, -0.1564344650402380854, 0.9876883405951365491 ) ) ;
#74237 = VERTEX_POINT ( 'NONE', #30641 ) ;
#74238 = CARTESIAN_POINT ( 'NONE',  ( 10.00000000000000000, 2.946379043146343246, 75.11764819372150725 ) ) ;
#74239 = ORIENTED_EDGE ( 'NONE', *, *, #65095, .F. ) ;
#74240 = CARTESIAN_POINT ( 'NONE',  ( 93.84685191531248449, 88.00268892867053694, 82.92239583420048632 ) ) ;
#74241 = CARTESIAN_POINT ( 'NONE',  ( 97.64999999999999147, -209.9999999999999716, 77.61749999999999261 ) ) ;
#74242 = ORIENTED_EDGE ( 'NONE', *, *, #67817, .F. ) ;
#74244 = ORIENTED_EDGE ( 'NONE', *, *, #57322, .F. ) ;
#74243 = VECTOR ( 'NONE', #11423, 1000.000000000000000 ) ;
#74245 = ORIENTED_EDGE ( 'NONE', *, *, #50023, .F. ) ;
#74246 = VERTEX_POINT ( 'NONE', #47215 ) ;
#74247 = DIRECTION ( 'NONE',  ( 0.9580045777625456616, 0.2867529058022021404, 0.000000000000000000 ) ) ;
#74248 = CIRCLE ( 'NONE', #37018, 17.37152077436032371 ) ;
#74249 =( NAMED_UNIT ( * ) SI_UNIT ( $, .STERADIAN. ) SOLID_ANGLE_UNIT ( ) );
#74250 = LINE ( 'NONE', #4747, #49912 ) ;
#74251 = ADVANCED_FACE ( 'NONE', ( #648 ), #24647, .F. ) ;
#74252 = DIRECTION ( 'NONE',  ( -0.000000000000000000, -0.000000000000000000, 1.000000000000000000 ) ) ;
#74253 = FACE_OUTER_BOUND ( 'NONE', #71211, .T. ) ;
#74254 = CARTESIAN_POINT ( 'NONE',  ( 92.35000000049298308, -210.0000320324309939, 85.63541623677062375 ) ) ;
#74255 = DIRECTION ( 'NONE',  ( 0.000000000000000000, -1.000000000000000000, -1.040834085586084414E-14 ) ) ;
#74256 = AXIS2_PLACEMENT_3D ( 'NONE', #60203, #54185, #19945 ) ;
#74257 = CARTESIAN_POINT ( 'NONE',  ( -97.64999999950680376, -210.0000320386661485, 83.73041644189096644 ) ) ;
#74258 = VECTOR ( 'NONE', #13545, 999.9999999999998863 ) ;
#74260 = ORIENTED_EDGE ( 'NONE', *, *, #66949, .T. ) ;
#74259 = ADVANCED_FACE ( 'NONE', ( #52106 ), #69395, .F. ) ;
#74261 = CARTESIAN_POINT ( 'NONE',  ( -92.34999999999999432, -208.4700217866474645, 82.82979166840095786 ) ) ;
#74262 = ORIENTED_EDGE ( 'NONE', *, *, #23184, .F. ) ;
#74263 = CARTESIAN_POINT ( 'NONE',  ( 0.000000000000000000, -26.23277895567245821, -4.042438405570103477 ) ) ;
#74264 = ORIENTED_EDGE ( 'NONE', *, *, #73676, .F. ) ;
#74266 = CARTESIAN_POINT ( 'NONE',  ( -92.35000000000005116, 88.47002178664754979, 79.54895833506762415 ) ) ;
#74265 = CARTESIAN_POINT ( 'NONE',  ( 97.64999999999997726, 88.47002178664753558, 78.27895833506762813 ) ) ;
#74267 =( BOUNDED_CURVE ( )  B_SPLINE_CURVE ( 2, ( #31386, #55440, #49785, #54335, #37426, #49427, #2862 ),
 .UNSPECIFIED., .F., .F. ) 
 B_SPLINE_CURVE_WITH_KNOTS ( ( 3, 2, 2, 3 ),
 ( 0.5926843883797353607, 0.5997400709749997061, 0.6067958365158828693, 0.6138516023186938453 ),
 .UNSPECIFIED. ) 
 CURVE ( )  GEOMETRIC_REPRESENTATION_ITEM ( )  RATIONAL_B_SPLINE_CURVE ( ( 0.9999968501007930888, 0.8660269787525570750, 1.000000000000000000, 0.8660254037844387076, 1.000000000000000000, 0.8660254037844387076, 1.000000000000000000 ) ) 
 REPRESENTATION_ITEM ( '' )  );
#74268 = ADVANCED_FACE ( 'NONE', ( #6620 ), #47579, .F. ) ;
#74269 = ORIENTED_EDGE ( 'NONE', *, *, #26728, .F. ) ;
#74270 = CARTESIAN_POINT ( 'NONE',  ( 92.69370383062498320, 90.00000000000002842, 83.45156250086715488 ) ) ;
#74271 = CARTESIAN_POINT ( 'NONE',  ( -11.68233973192911535, 0.000000000000000000, -17.37152077436032371 ) ) ;
#74272 = DIRECTION ( 'NONE',  ( 0.9997280174009349762, -0.02332147558787671729, 0.000000000000000000 ) ) ;
#74273 = DIRECTION ( 'NONE',  ( -1.000000000000000000, 0.000000000000000000, 0.000000000000000000 ) ) ;
#74274 = DIRECTION ( 'NONE',  ( 0.000000000000000000, 0.000000000000000000, 1.000000000000000000 ) ) ;
#74275 = DIRECTION ( 'NONE',  ( 0.000000000000000000, 0.000000000000000000, 1.000000000000000000 ) ) ;
#74276 = VERTEX_POINT ( 'NONE', #46852 ) ;
#74277 = DIRECTION ( 'NONE',  ( 0.000000000000000000, 0.000000000000000000, 1.000000000000000000 ) ) ;
#74278 = CARTESIAN_POINT ( 'NONE',  ( 5.000000000000000000, 77.16300072079660310, 27.74655509720696855 ) ) ;
#74279 = DIRECTION ( 'NONE',  ( -1.000000000000000000, 0.000000000000000000, -0.000000000000000000 ) ) ;
#74280 = VERTEX_POINT ( 'NONE', #26497 ) ;
#74281 = ORIENTED_EDGE ( 'NONE', *, *, #3360, .T. ) ;
#74282 = EDGE_CURVE ( 'NONE', #4552, #73705, #9580, .T. ) ;
#74283 = AXIS2_PLACEMENT_3D ( 'NONE', #15894, #6116, #68890 ) ;
#74284 = EDGE_CURVE ( 'NONE', #45691, #24219, #42682, .T. ) ;
#74285 = CARTESIAN_POINT ( 'NONE',  ( -7.670864526094549163, -97.73662565058241114, 5.500000000000000000 ) ) ;
#74286 = CARTESIAN_POINT ( 'NONE',  ( -3.667169054266697259, -3.656261651251520917, -0.8603634151101461347 ) ) ;
#74287 = DIRECTION ( 'NONE',  ( -0.9918136447140104561, 0.1276937514489679681, 0.000000000000000000 ) ) ;
#74288 = CARTESIAN_POINT ( 'NONE',  ( -92.69370383062498320, -209.9999999999999716, 81.86406250086714920 ) ) ;
#74289 = ORIENTED_EDGE ( 'NONE', *, *, #52948, .T. ) ;
#74290 = VECTOR ( 'NONE', #25708, 1000.000000000000000 ) ;
#74291 = ORIENTED_EDGE ( 'NONE', *, *, #25229, .F. ) ;
#74292 = AXIS2_PLACEMENT_3D ( 'NONE', #59144, #52010, #23453 ) ;
#74293 = AXIS2_PLACEMENT_3D ( 'NONE', #63508, #68409, #24019 ) ;
#74294 = DIRECTION ( 'NONE',  ( 7.943659481576819828E-16, 1.065814103640131188E-14, 1.000000000000000000 ) ) ;
#74295 = EDGE_CURVE ( 'NONE', #53104, #58523, #55065, .T. ) ;
#74296 = EDGE_CURVE ( 'NONE', #22189, #16005, #56590, .T. ) ;
#74297 = DIRECTION ( 'NONE',  ( -1.000000000000000000, 0.000000000000000000, -0.000000000000000000 ) ) ;
#74298 = SURFACE_STYLE_FILL_AREA ( #5524 ) ;
#74299 = CARTESIAN_POINT ( 'NONE',  ( 92.69370383062498320, 90.00000000000002842, 75.67281250086713840 ) ) ;
#74300 = AXIS2_PLACEMENT_3D ( 'NONE', #58688, #59067, #57952 ) ;
#74301 = DIRECTION ( 'NONE',  ( -1.000000000000000000, 0.000000000000000000, 0.000000000000000000 ) ) ;
#74302 = LINE ( 'NONE', #68676, #30056 ) ;
#74303 = CARTESIAN_POINT ( 'NONE',  ( -97.65000000000003411, -208.4700217866475214, 79.15208333333333712 ) ) ;
#74304 = CARTESIAN_POINT ( 'NONE',  ( -92.34999999999999432, -209.9999999999999716, 90.00000000000000000 ) ) ;
#74305 = CARTESIAN_POINT ( 'NONE',  ( 12.75000000000259881, -119.9999999999951257, -64.99999999999967315 ) ) ;
#74306 = CARTESIAN_POINT ( 'NONE',  ( 97.30629616937498838, 88.66845928578035796, 86.25614583420048120 ) ) ;
#74307 = CIRCLE ( 'NONE', #62301, 31.99999999999998579 ) ;
#74308 = CARTESIAN_POINT ( 'NONE',  ( -94.99999999999997158, -212.6630814284392557, 88.69031250086716511 ) ) ;
#74309 = DIRECTION ( 'NONE',  ( -1.000000000000000000, 0.000000000000000000, -0.000000000000000000 ) ) ;
#74310 = AXIS2_PLACEMENT_3D ( 'NONE', #3878, #54262, #19656 ) ;
#74311 = VERTEX_POINT ( 'NONE', #43447 ) ;
#74312 = CARTESIAN_POINT ( 'NONE',  ( 10.00000000000000000, -17.80606268964516659, -33.00180498840066434 ) ) ;
#74313 = CARTESIAN_POINT ( 'NONE',  ( -97.30629616937501680, 90.00000000000004263, 79.48281250086714067 ) ) ;
#74314 = CIRCLE ( 'NONE', #62308, 15.99999999999999822 ) ;
#74315 = AXIS2_PLACEMENT_3D ( 'NONE', #16084, #26980, #4085 ) ;
#74316 = AXIS2_PLACEMENT_3D ( 'NONE', #43357, #33147, #3503 ) ;
#74317 = ORIENTED_EDGE ( 'NONE', *, *, #58055, .F. ) ;
#74318 = AXIS2_PLACEMENT_3D ( 'NONE', #10705, #28359, #12179 ) ;
#74319 = LINE ( 'NONE', #29181, #17463 ) ;
#74320 = CARTESIAN_POINT ( 'NONE',  ( 0.000000000000000000, -3.948201729842038432, -23.21447184625298021 ) ) ;
#74321 = DIRECTION ( 'NONE',  ( 0.000000000000000000, -0.8090169943749504489, 0.5877852522924689183 ) ) ;
#74322 = CARTESIAN_POINT ( 'NONE',  ( 10.00000000000000000, 0.000000000000000000, 0.000000000000000000 ) ) ;
#74323 = CARTESIAN_POINT ( 'NONE',  ( 93.84685191531251292, -211.9973110713294489, 75.30239583420048177 ) ) ;
#74324 = ORIENTED_EDGE ( 'NONE', *, *, #69075, .T. ) ;
#74325 = EDGE_CURVE ( 'NONE', #24805, #35621, #31387, .T. ) ;
#74326 = EDGE_LOOP ( 'NONE', ( #16025, #70795, #13148, #48551 ) ) ;
#74327 = EDGE_CURVE ( 'NONE', #20728, #60846, #72355, .T. ) ;
#74328 = AXIS2_PLACEMENT_3D ( 'NONE', #72219, #54574, #48562 ) ;
#74329 = CARTESIAN_POINT ( 'NONE',  ( 96.15314808468748708, -208.0026889286704943, 85.77989583420048803 ) ) ;
#74330 = FACE_OUTER_BOUND ( 'NONE', #18635, .T. ) ;
#74331 = CARTESIAN_POINT ( 'NONE',  ( 0.000000000000000000, -59.03342792756231461, -46.54456581323868392 ) ) ;
#74332 = EDGE_CURVE ( 'NONE', #38273, #37771, #13369, .T. ) ;
#74333 = DIRECTION ( 'NONE',  ( 0.000000000000000000, -0.5877852522924625900, -0.8090169943749551118 ) ) ;
#74334 = DIRECTION ( 'NONE',  ( 0.000000000000000000, 0.000000000000000000, -1.000000000000000000 ) ) ;
#74335 = AXIS2_PLACEMENT_3D ( 'NONE', #44418, #27474, #73336 ) ;
#74336 = CYLINDRICAL_SURFACE ( 'NONE', #58526, 16.00000000000000000 ) ;
#74337 = CARTESIAN_POINT ( 'NONE',  ( 96.32499999999998863, -212.2949673200287179, 88.94166666666666288 ) ) ;
#74338 = AXIS2_PLACEMENT_3D ( 'NONE', #25234, #48522, #54181 ) ;
#74339 = CIRCLE ( 'NONE', #22731, 31.99999999999999645 ) ;
#74340 = DIRECTION ( 'NONE',  ( -1.000000000000000000, -0.000000000000000000, -0.000000000000000000 ) ) ;
#74341 = NEXT_ASSEMBLY_USAGE_OCCURRENCE ( 'NAUO1', ' ', ' ', #40833, #6784, $ ) ;
#74342 = NEXT_ASSEMBLY_USAGE_OCCURRENCE ( 'NAUO2', ' ', ' ', #40833, #23745, $ ) ;
#74343 = NEXT_ASSEMBLY_USAGE_OCCURRENCE ( 'NAUO3', ' ', ' ', #40833, #29261, $ ) ;
#74344 = NEXT_ASSEMBLY_USAGE_OCCURRENCE ( 'NAUO4', ' ', ' ', #40833, #52691, $ ) ;
#74345 = NEXT_ASSEMBLY_USAGE_OCCURRENCE ( 'NAUO5', ' ', ' ', #40833, #3585, $ ) ;
#74346 = NEXT_ASSEMBLY_USAGE_OCCURRENCE ( 'NAUO6', ' ', ' ', #40833, #37077, $ ) ;
#74347 = NEXT_ASSEMBLY_USAGE_OCCURRENCE ( 'NAUO7', ' ', ' ', #40833, #11351, $ ) ;
#74348 = NEXT_ASSEMBLY_USAGE_OCCURRENCE ( 'NAUO8', ' ', ' ', #40833, #5869, $ ) ;
#74349 = NEXT_ASSEMBLY_USAGE_OCCURRENCE ( 'NAUO9', ' ', ' ', #40833, #8124, $ ) ;
#74350 = NEXT_ASSEMBLY_USAGE_OCCURRENCE ( 'NAUO10', ' ', ' ', #40833, #63750, $ ) ;
#74351 = NEXT_ASSEMBLY_USAGE_OCCURRENCE ( 'NAUO11', ' ', ' ', #40833, #33419, $ ) ;
#74352 = NEXT_ASSEMBLY_USAGE_OCCURRENCE ( 'NAUO12', ' ', ' ', #40833, #56863, $ ) ;
#74353 = NEXT_ASSEMBLY_USAGE_OCCURRENCE ( 'NAUO13', ' ', ' ', #40833, #56863, $ ) ;
#74354 = NEXT_ASSEMBLY_USAGE_OCCURRENCE ( 'NAUO14', ' ', ' ', #40833, #53621, $ ) ;
#74355 = NEXT_ASSEMBLY_USAGE_OCCURRENCE ( 'NAUO15', ' ', ' ', #40833, #53621, $ ) ;
#74356 = NEXT_ASSEMBLY_USAGE_OCCURRENCE ( 'NAUO16', ' ', ' ', #40833, #31551, $ ) ;
#74357 = NEXT_ASSEMBLY_USAGE_OCCURRENCE ( 'NAUO17', ' ', ' ', #40833, #53621, $ ) ;
#74358 = NEXT_ASSEMBLY_USAGE_OCCURRENCE ( 'NAUO18', ' ', ' ', #40833, #53621, $ ) ;
#74359 = NEXT_ASSEMBLY_USAGE_OCCURRENCE ( 'NAUO19', ' ', ' ', #40833, #56863, $ ) ;
#74360 = NEXT_ASSEMBLY_USAGE_OCCURRENCE ( 'NAUO20', ' ', ' ', #40833, #56863, $ ) ;
#74361 = NEXT_ASSEMBLY_USAGE_OCCURRENCE ( 'NAUO21', ' ', ' ', #40833, #40301, $ ) ;
#74362 = NEXT_ASSEMBLY_USAGE_OCCURRENCE ( 'NAUO22', ' ', ' ', #40833, #40301, $ ) ;
#74363 = NEXT_ASSEMBLY_USAGE_OCCURRENCE ( 'NAUO23', ' ', ' ', #40833, #14154, $ ) ;
#74364 = NEXT_ASSEMBLY_USAGE_OCCURRENCE ( 'NAUO24', ' ', ' ', #40833, #14154, $ ) ;
#74365 = NEXT_ASSEMBLY_USAGE_OCCURRENCE ( 'NAUO25', ' ', ' ', #40833, #14154, $ ) ;
#74366 = NEXT_ASSEMBLY_USAGE_OCCURRENCE ( 'NAUO26', ' ', ' ', #40833, #14154, $ ) ;
#74367 = NEXT_ASSEMBLY_USAGE_OCCURRENCE ( 'NAUO27', ' ', ' ', #40833, #37077, $ ) ;
#74368 = NEXT_ASSEMBLY_USAGE_OCCURRENCE ( 'NAUO28', ' ', ' ', #40833, #24681, $ ) ;
#74369 = NEXT_ASSEMBLY_USAGE_OCCURRENCE ( 'NAUO29', ' ', ' ', #40833, #66939, $ ) ;
#74370 = NEXT_ASSEMBLY_USAGE_OCCURRENCE ( 'NAUO30', ' ', ' ', #40833, #49042, $ ) ;
#74371 = NEXT_ASSEMBLY_USAGE_OCCURRENCE ( 'NAUO31', ' ', ' ', #40833, #49042, $ ) ;
#74372 = NEXT_ASSEMBLY_USAGE_OCCURRENCE ( 'NAUO32', ' ', ' ', #40833, #66939, $ ) ;
#74373 = NEXT_ASSEMBLY_USAGE_OCCURRENCE ( 'NAUO33', ' ', ' ', #40833, #66939, $ ) ;
#74374 = NEXT_ASSEMBLY_USAGE_OCCURRENCE ( 'NAUO34', ' ', ' ', #40833, #66939, $ ) ;
#74375 = NEXT_ASSEMBLY_USAGE_OCCURRENCE ( 'NAUO35', ' ', ' ', #40833, #49042, $ ) ;
#74376 = NEXT_ASSEMBLY_USAGE_OCCURRENCE ( 'NAUO36', ' ', ' ', #40833, #49042, $ ) ;
#74377 = NEXT_ASSEMBLY_USAGE_OCCURRENCE ( 'NAUO37', ' ', ' ', #40833, #30197, $ ) ;
#74378 = NEXT_ASSEMBLY_USAGE_OCCURRENCE ( 'NAUO38', ' ', ' ', #40833, #30197, $ ) ;
#74379 = NEXT_ASSEMBLY_USAGE_OCCURRENCE ( 'NAUO39', ' ', ' ', #40833, #30197, $ ) ;
#74380 = NEXT_ASSEMBLY_USAGE_OCCURRENCE ( 'NAUO40', ' ', ' ', #40833, #30197, $ ) ;
ENDSEC;
END-ISO-10303-21;
